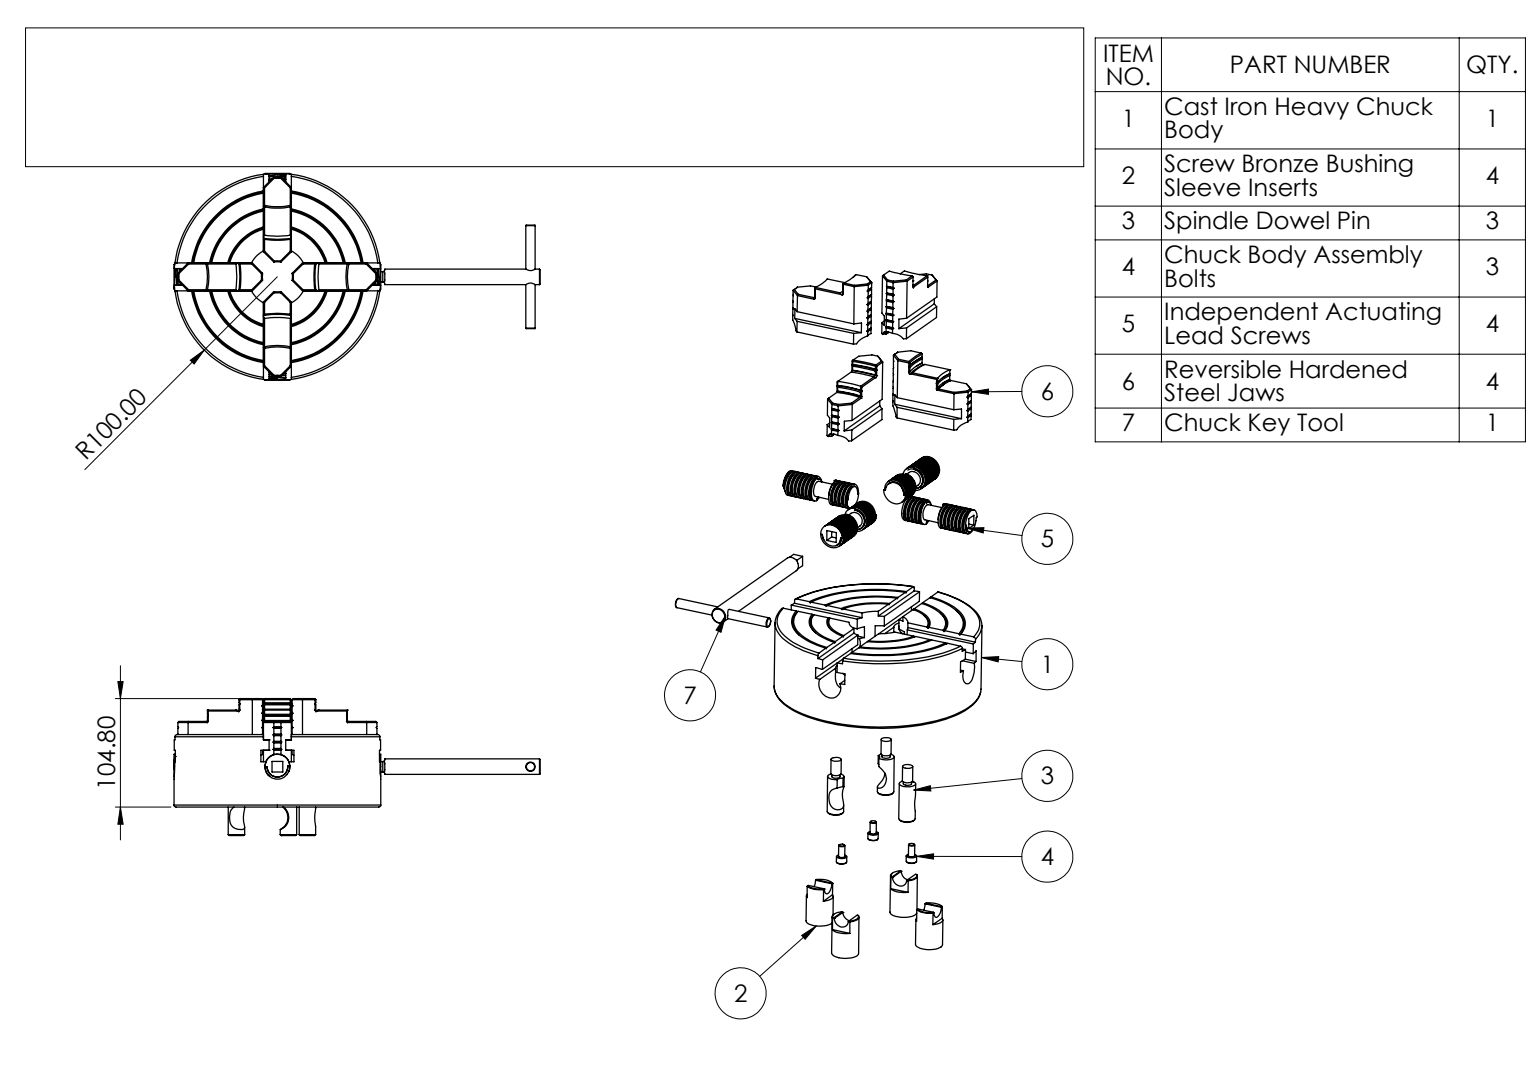
ISO-10303-21;
HEADER;
FILE_DESCRIPTION (('STEP AP214'),
    '1' );
FILE_NAME ('MAS-416',
    '2026-10-09T08:48:44',
    ( '' ),
    ( '' ),
    'SwSTEP 2.0',
    'SolidWorks 2026',
    '' );
FILE_SCHEMA (( 'AUTOMOTIVE_DESIGN' ));
ENDSEC;

DATA;
#1 =( BOUNDED_CURVE ( )  B_SPLINE_CURVE ( 2, ( #10533, #60209, #55118, #80827, #73261, #48394, #10118, #21906, #55527, #48810, #23141, #53876, #74509 ),
 .UNSPECIFIED., .F., .F. ) 
 B_SPLINE_CURVE_WITH_KNOTS ( ( 3, 2, 2, 2, 2, 2, 3 ),
 ( 0.7124999999999999112, 0.7166666666666665630, 0.7208333333333332149, 0.7249999999999998668, 0.7291666666666665186, 0.7333333333333331705, 0.7374999999999999334 ),
 .UNSPECIFIED. ) 
 CURVE ( )  GEOMETRIC_REPRESENTATION_ITEM ( )  RATIONAL_B_SPLINE_CURVE ( ( 1.000000000000000888, 0.9659258262890674240, 1.000000000000000000, 0.9659258262890683122, 1.000000000000000000, 0.9659258262890683122, 1.000000000000000000, 0.9659258262890683122, 1.000000000000000000, 0.9659258262890683122, 1.000000000000000000, 0.9659258262890692004, 0.9999999999999991118 ) ) 
 REPRESENTATION_ITEM ( '' )  );
#2 = CARTESIAN_POINT ( 'NONE',  ( 0.3392501089628018329, 0.1958661417322835607, -1.790682414698162805 ) ) ;
#3 = CARTESIAN_POINT ( 'NONE',  ( -1.404199475065615932, -0.3690944881889765550, -0.3153832671262227771 ) ) ;
#4 = CARTESIAN_POINT ( 'NONE',  ( 1.318897637795276356, 0.1660481256975883668, -0.3530559997133364547 ) ) ;
#5 = CARTESIAN_POINT ( 'NONE',  ( 1.194225721784777594, 0.05413385826771666132, 0.4176697321401328100 ) ) ;
#6 = CARTESIAN_POINT ( 'NONE',  ( 0.3018372703412079971, -0.004921259842519870586, -0.3153832671262229437 ) ) ;
#7 = CARTESIAN_POINT ( 'NONE',  ( 1.003937007874016185, 0.1660481256975883668, -0.3530559997133364547 ) ) ;
#8 = CARTESIAN_POINT ( 'NONE',  ( 0.4091458600556403535, 0.2362204724409449896, -1.625328083989501460 ) ) ;
#9 = CARTESIAN_POINT ( 'NONE',  ( 0.1377952755905518800, 0.07958543189024071263, -0.2665933059059888421 ) ) ;
#10 = CARTESIAN_POINT ( 'NONE',  ( 0.3149606299212603933, -0.1870078740157479769, 0.4822834645669291653 ) ) ;
#11 = CARTESIAN_POINT ( 'NONE',  ( 0.3949938075777409408, -0.1058382717557499186, -1.133202099737532720 ) ) ;
#12 = CARTESIAN_POINT ( 'NONE',  ( -1.043307086614172707, 0.1660481256975883668, -0.3530559997133364547 ) ) ;
#13 = CARTESIAN_POINT ( 'NONE',  ( 0.4330708661417329575, -0.5511811023622047445, 6.969142054262312111E-17 ) ) ;
#14 = PLANE ( 'NONE',  #11131 ) ;
#15 = CARTESIAN_POINT ( 'NONE',  ( -0.1902887139107604098, -0.6692913385826771977, 0.1292274648535927661 ) ) ;
#16 = CARTESIAN_POINT ( 'NONE',  ( -0.1574803149606292529, -0.1870078740157480601, -0.3641732283464567677 ) ) ;
#17 = CARTESIAN_POINT ( 'NONE',  ( 3.210901138312283187, 2.729659904327170317, 0.5314960629921260393 ) ) ;
#18 = CARTESIAN_POINT ( 'NONE',  ( -0.2493438320209966919, 0.05413385826771626580, -0.4176697321401330321 ) ) ;
#19 = CARTESIAN_POINT ( 'NONE',  ( 0.4002624671916016896, -0.2845877964562161244, -0.3641732283464567121 ) ) ;
#20 = CARTESIAN_POINT ( 'NONE',  ( 0.1070741851644053388, 0.3996062992125986035, -1.959973753280839892 ) ) ;
#21 = CARTESIAN_POINT ( 'NONE',  ( -0.03280839895013062252, 0.2952755905511810774, -0.1292274648535930714 ) ) ;
#22 = EDGE_CURVE ( 'NONE', #75161, #32355, #82357, .T. ) ;
#23 = CARTESIAN_POINT ( 'NONE',  ( -0.1958661417322834497, -0.3392501089628018884, -1.562972810202412521 ) ) ;
#24 = CARTESIAN_POINT ( 'NONE',  ( 1.135170603674541256, -0.5511811023622048555, -0.09757992244046775898 ) ) ;
#25 = CARTESIAN_POINT ( 'NONE',  ( 2.372150492836604986E-17, 0.000000000000000000, 0.1937007874015747588 ) ) ;
#26 = CARTESIAN_POINT ( 'NONE',  ( -0.8530183727034112984, -0.3690944881889765550, -0.3153832671262227771 ) ) ;
#27 = CARTESIAN_POINT ( 'NONE',  ( -0.8792650918635160906, -0.004921259842519870586, -0.3153832671262229437 ) ) ;
#28 = CARTESIAN_POINT ( 'NONE',  ( -0.8530183727034112984, 0.05413385826771666132, 0.4176697321401328100 ) ) ;
#29 = CARTESIAN_POINT ( 'NONE',  ( -0.3018372703412066094, 0.05413385826771666132, 0.4176697321401328100 ) ) ;
#30 = CARTESIAN_POINT ( 'NONE',  ( 0.5905511811023629321, 0.1771653543307087630, 0.000000000000000000 ) ) ;
#31 = CARTESIAN_POINT ( 'NONE',  ( -0.2597599741900292747, 0.1405915162213216552, 5.593567858643829993 ) ) ;
#32 = CARTESIAN_POINT ( 'NONE',  ( 1.351706036745407458, -0.3690944881889765550, -0.3153832671262227771 ) ) ;
#33 = CARTESIAN_POINT ( 'NONE',  ( 0.6758530183727039509, -0.6692913385826771977, 0.1292274648535927661 ) ) ;
#34 = CARTESIAN_POINT ( 'NONE',  ( 0.3996062992125986035, -0.1070741851644052972, -0.03083989501312336262 ) ) ;
#35 = CARTESIAN_POINT ( 'NONE',  ( -0.09186351706036689768, 0.05413385826771626580, -0.4176697321401330321 ) ) ;
#36 = CARTESIAN_POINT ( 'NONE',  ( 0.1958661417322836440, -0.3392501089628017219, -0.9639107611548557442 ) ) ;
#37 = CARTESIAN_POINT ( 'NONE',  ( 1.476377952755906220, 0.07958543189024071263, -0.2665933059059888421 ) ) ;
#38 = CARTESIAN_POINT ( 'NONE',  ( 0.7874015748031503170, -0.1870078740157480879, -0.4822834645669291653 ) ) ;
#39 = CARTESIAN_POINT ( 'NONE',  ( 8.195543980992789655E-16, -0.1870078740157480879, -0.4822834645669291653 ) ) ;
#40 = DIRECTION ( 'NONE',  ( 0.000000000000000000, 0.000000000000000000, 1.000000000000000000 ) ) ;
#41 = CARTESIAN_POINT ( 'NONE',  ( 0.1706036745406830368, -0.3690944881889765550, -0.3153832671262227771 ) ) ;
#42 = CARTESIAN_POINT ( 'NONE',  ( 1.141732283464567788, -0.6692913385826771977, 8.415575281601705876E-17 ) ) ;
#43 = CARTESIAN_POINT ( 'NONE',  ( -0.2952755905511804668, 0.07958543189024085140, 0.2665933059059887866 ) ) ;
#44 = CARTESIAN_POINT ( 'NONE',  ( -0.7152230971128602510, -0.3162353388693405765, 0.4822834645669290543 ) ) ;
#45 = CARTESIAN_POINT ( 'NONE',  ( 0.4091458600556404646, -0.2362204724409448231, -2.624671916010498762 ) ) ;
#46 = CARTESIAN_POINT ( 'NONE',  ( 0.3346456692913390985, 0.1660481256975885056, 0.3530559997133364547 ) ) ;
#47 = CARTESIAN_POINT ( 'NONE',  ( -0.6758530183727028406, 0.2952755905511811885, 0.1292274648535926551 ) ) ;
#48 = CARTESIAN_POINT ( 'NONE',  ( -0.7086614173228339419, -0.1870078740157480601, -0.3641732283464567677 ) ) ;
#49 = CARTESIAN_POINT ( 'NONE',  ( 0.1837270341207354329, 0.2306618581243848609, 0.2411417322834645549 ) ) ;
#50 = CARTESIAN_POINT ( 'NONE',  ( -1.135170603674539924, -0.6692913385826771977, 0.1292274648535927661 ) ) ;
#51 = CARTESIAN_POINT ( 'NONE',  ( -0.3412073490813641308, 0.2306618581243847221, -0.2411417322834647770 ) ) ;
#52 = CARTESIAN_POINT ( 'NONE',  ( 0.4724409448818898682, 2.892866454678787531E-17, -2.322834645669291209 ) ) ;
#54 = CARTESIAN_POINT ( 'NONE',  ( 1.161417322834646271, 0.1660481256975883668, -0.3530559997133364547 ) ) ;
#53 = CYLINDRICAL_SURFACE ( 'NONE', #64776, 0.3937007874015748254 ) ;
#55 = CARTESIAN_POINT ( 'NONE',  ( 1.135170603674541256, -0.6692913385826773087, -0.1292274648535924053 ) ) ;
#56 = CARTESIAN_POINT ( 'NONE',  ( 0.2867679344610366554, -0.2867679344610365444, -2.610236220472440749 ) ) ;
#57 = CARTESIAN_POINT ( 'NONE',  ( -1.489501312335957062, -0.05778040916215522460, 0.4822834645669289988 ) ) ;
#58 = CARTESIAN_POINT ( 'NONE',  ( -0.7217847769028863381, 0.05413385826771626580, -0.4176697321401330321 ) ) ;
#59 = CARTESIAN_POINT ( 'NONE',  ( 5.785732909357575061E-17, -0.4724409448818898682, -0.3937007874015748254 ) ) ;
#60 = CARTESIAN_POINT ( 'NONE',  ( -0.1070741851644051862, -0.3996062992125987146, -0.07217847769028871985 ) ) ;
#61 = ORIENTED_EDGE ( 'NONE', *, *, #30614, .T. ) ;
#62 = CARTESIAN_POINT ( 'NONE',  ( -0.08530183727034056085, -0.2845877964562159024, 0.3641732283464567677 ) ) ;
#63 = CARTESIAN_POINT ( 'NONE',  ( -0.1049643490035302024, -0.3917322834645671215, -1.796587926509185973 ) ) ;
#64 = EDGE_LOOP ( 'NONE', ( #43919, #18024, #48228, #40467 ) ) ;
#65 = CARTESIAN_POINT ( 'NONE',  ( 0.1837270341207354329, 0.2306618581243848609, 0.2411417322834645549 ) ) ;
#66 = CARTESIAN_POINT ( 'NONE',  ( -0.4724409448818898682, -8.678599364036362592E-17, -2.716535433070865757 ) ) ;
#67 = CYLINDRICAL_SURFACE ( 'NONE', #60105, 0.3937007874015748254 ) ;
#68 = CARTESIAN_POINT ( 'NONE',  ( -0.4265091863517051496, -0.5511811023622046335, 0.09757992244046803654 ) ) ;
#69 = CARTESIAN_POINT ( 'NONE',  ( 0.3346456692913390985, 0.1660481256975885056, 0.3530559997133364547 ) ) ;
#70 = CARTESIAN_POINT ( 'NONE',  ( 1.220472440944882608, 0.2952755905511811885, 0.000000000000000000 ) ) ;
#71 = CARTESIAN_POINT ( 'NONE',  ( 0.7283464566929140904, -0.4536011799217368745, -0.2665933059059886201 ) ) ;
#72 = AXIS2_PLACEMENT_3D ( 'NONE', #38595, #24309, #82401 ) ;
#73 = CARTESIAN_POINT ( 'NONE',  ( -0.04593175853018302557, 0.2952755905511811885, 0.1292274648535926551 ) ) ;
#74 = CARTESIAN_POINT ( 'NONE',  ( 4.797336870675655290E-17, -0.3917322834645669549, -0.9461749099399457963 ) ) ;
#75 = CARTESIAN_POINT ( 'NONE',  ( -0.7414698162729651543, -0.6692913385826771977, 0.1292274648535927661 ) ) ;
#76 = CARTESIAN_POINT ( 'NONE',  ( -1.351706036745406347, -0.004921259842519870586, -0.3153832671262229437 ) ) ;
#77 = CARTESIAN_POINT ( 'NONE',  ( -0.5839895013123351797, 0.2952755905511810774, -0.1292274648535930714 ) ) ;
#78 = FACE_OUTER_BOUND ( 'NONE', #30932, .T. ) ;
#79 = CARTESIAN_POINT ( 'NONE',  ( 1.515748031496063408, 0.07958543189024085140, 0.2665933059059887866 ) ) ;
#80 = VERTEX_POINT ( 'NONE', #70589 ) ;
#81 = CARTESIAN_POINT ( 'NONE',  ( 0.1049643490035304799, -0.3917322834645670104, -2.444245037566615597 ) ) ;
#82 = CARTESIAN_POINT ( 'NONE',  ( 0.2362204724409456558, -0.1870078740157479769, 0.4822834645669291653 ) ) ;
#83 = ORIENTED_EDGE ( 'NONE', *, *, #43269, .T. ) ;
#84 = CARTESIAN_POINT ( 'NONE',  ( -0.6561679790026240244, -0.6046776061558807314, 0.2411417322834647770 ) ) ;
#85 = CARTESIAN_POINT ( 'NONE',  ( 1.332020997375328974, -0.05778040916215560624, -0.4822834645669293319 ) ) ;
#86 = CARTESIAN_POINT ( 'NONE',  ( 1.213910761154856299, -0.6692913385826773087, -0.1292274648535924053 ) ) ;
#87 = CARTESIAN_POINT ( 'NONE',  ( 0.4724409448818904789, -0.1870078740157479769, 0.4822834645669291653 ) ) ;
#88 = CARTESIAN_POINT ( 'NONE',  ( 0.1574803149606306130, -0.1870078740157480879, -0.4822834645669291653 ) ) ;
#89 = CARTESIAN_POINT ( 'NONE',  ( -0.1049643490035302024, -0.3917322834645671215, -1.416666666666666519 ) ) ;
#90 = CARTESIAN_POINT ( 'NONE',  ( -0.9120734908136475250, 0.2952755905511811885, 0.1292274648535926551 ) ) ;
#91 = CARTESIAN_POINT ( 'NONE',  ( -0.1968503937007867743, 0.2952755905511811885, 0.000000000000000000 ) ) ;
#92 = CARTESIAN_POINT ( 'NONE',  ( -0.006561679790025524116, -0.08942795157528024563, -0.3641732283464568787 ) ) ;
#93 = CARTESIAN_POINT ( 'NONE',  ( -0.2945219335573386332, -0.02405856270293451477, 5.877884953661866696 ) ) ;
#94 = CARTESIAN_POINT ( 'NONE',  ( 0.07217847769028949700, -0.05778040916215560624, -0.4822834645669293319 ) ) ;
#95 = CARTESIAN_POINT ( 'NONE',  ( 2.362204724409448620, 1.724409448818897461, 8.247593713802677664E-15 ) ) ;
#96 = CARTESIAN_POINT ( 'NONE',  ( 1.253280839895013710, -0.3162353388693405765, 0.4822834645669290543 ) ) ;
#97 = CARTESIAN_POINT ( 'NONE',  ( 3.935554666754304876, 1.075197191891656523, -0.1080298857917176142 ) ) ;
#98 = EDGE_LOOP ( 'NONE', ( #67193, #53701, #56792, #76408 ) ) ;
#99 = ORIENTED_EDGE ( 'NONE', *, *, #69485, .F. ) ;
#100 = CARTESIAN_POINT ( 'NONE',  ( 0.3215223097112867578, -0.3162353388693409650, -0.4822834645669289433 ) ) ;
#101 = CARTESIAN_POINT ( 'NONE',  ( -0.3543307086614165824, -0.5511811023622047445, 6.969142054262312111E-17 ) ) ;
#103 = CARTESIAN_POINT ( 'NONE',  ( -0.06764250034433647030, -3.915482057279200494E-15, 0.3954985857520088577 ) ) ;
#102 = CARTESIAN_POINT ( 'NONE',  ( 1.377952755905512472, 0.1771653543307087630, 0.000000000000000000 ) ) ;
#104 = CARTESIAN_POINT ( 'NONE',  ( -0.3392501089628019995, 0.1958661417322832277, -1.213254593175852936 ) ) ;
#105 = CARTESIAN_POINT ( 'NONE',  ( -0.4091458600556405756, 0.2362204724409446288, -0.1030183727034120617 ) ) ;
#106 = CARTESIAN_POINT ( 'NONE',  ( 1.410761154855643795, -0.08942795157528024563, -0.3641732283464568787 ) ) ;
#107 = CARTESIAN_POINT ( 'NONE',  ( -1.423884514435694859, -0.05778040916215560624, -0.4822834645669293319 ) ) ;
#108 = CARTESIAN_POINT ( 'NONE',  ( 0.2891555358219910499, 0.2891555358219910499, 0.1003937007874015630 ) ) ;
#109 = CARTESIAN_POINT ( 'NONE',  ( -0.1377952755905504645, 0.1660481256975885056, 0.3530559997133364547 ) ) ;
#110 = CARTESIAN_POINT ( 'NONE',  ( -1.056430446194224881, -0.6692913385826771977, 0.1292274648535927661 ) ) ;
#111 = CARTESIAN_POINT ( 'NONE',  ( -0.9645669291338575535, -0.5400638737290844871, 0.3530559997133364547 ) ) ;
#112 = CARTESIAN_POINT ( 'NONE',  ( 0.1902887139107617975, 0.2952755905511811885, 0.1292274648535926551 ) ) ;
#113 = CARTESIAN_POINT ( 'NONE',  ( -0.3949938075777409963, -7.255918531996591613E-17, 0.04133858267716533641 ) ) ;
#114 = CARTESIAN_POINT ( 'NONE',  ( -1.653543307086613234, -0.1870078740157479769, 0.3641732283464567677 ) ) ;
#115 = CARTESIAN_POINT ( 'NONE',  ( 1.108923884514436242, -0.05778040916215522460, 0.4822834645669289988 ) ) ;
#116 = CARTESIAN_POINT ( 'NONE',  ( 0.7545931758530189937, 0.1771653543307087075, -0.09757992244046823083 ) ) ;
#117 = CARTESIAN_POINT ( 'NONE',  ( 0.3074112942705509166, 1.261823755618582510, 0.05913325304464405602 ) ) ;
#118 = CARTESIAN_POINT ( 'NONE',  ( 0.9055118110236227702, 0.1771653543307087630, 0.000000000000000000 ) ) ;
#119 = CARTESIAN_POINT ( 'NONE',  ( -1.200787401574802349, -0.5400638737290844871, 0.3530559997133364547 ) ) ;
#120 = CARTESIAN_POINT ( 'NONE',  ( -9.787531504996566615E-17, 0.3996062992125985480, -0.7066929133858268486 ) ) ;
#121 = CARTESIAN_POINT ( 'NONE',  ( 1.358267716535433323, 0.1660481256975885056, 0.3530559997133364547 ) ) ;
#122 = CARTESIAN_POINT ( 'NONE',  ( -0.3392501089628017219, -0.1958661417322836718, -0.6745406824146981117 ) ) ;
#124 = DIRECTION ( 'NONE',  ( 1.000000000000000000, 0.000000000000000000, -0.000000000000000000 ) ) ;
#123 = CARTESIAN_POINT ( 'NONE',  ( 0.6036745406824154392, 0.2306618581243847221, -0.2411417322834647770 ) ) ;
#125 = CARTESIAN_POINT ( 'NONE',  ( -1.653543307086613234, -0.1870078740157480601, -0.3641732283464567677 ) ) ;
#126 = CARTESIAN_POINT ( 'NONE',  ( 0.01968503937007957949, -0.5400638737290845981, -0.3530559997133363437 ) ) ;
#127 = CARTESIAN_POINT ( 'NONE',  ( 0.6102362204724416372, -0.4536011799217367080, 0.2665933059059888421 ) ) ;
#128 = CARTESIAN_POINT ( 'NONE',  ( 0.9776902887139113929, -0.6692913385826773087, -0.1292274648535924053 ) ) ;
#129 = CARTESIAN_POINT ( 'NONE',  ( 1.640419947506562393, -0.3690944881889763329, 0.3153832671262228327 ) ) ;
#130 = CARTESIAN_POINT ( 'NONE',  ( -0.6824146981627291497, -0.5023911411419708095, -0.1820866141732282451 ) ) ;
#131 = CARTESIAN_POINT ( 'NONE',  ( -0.6430446194225716283, -0.4281496062992124485, 0.4176697321401328655 ) ) ;
#132 = CARTESIAN_POINT ( 'NONE',  ( 1.574803149606299746, -0.1870078740157480879, -0.4822834645669291653 ) ) ;
#133 = CARTESIAN_POINT ( 'NONE',  ( -1.246719160104986512, 0.05413385826771666132, 0.4176697321401328100 ) ) ;
#134 = CONICAL_SURFACE ( 'NONE', #57903, 2.401574803149606918, 0.7125723459225955514 ) ;
#135 = CARTESIAN_POINT ( 'NONE',  ( 0.8923884514435703741, 0.2306618581243848609, 0.2411417322834645549 ) ) ;
#136 = CARTESIAN_POINT ( 'NONE',  ( -1.345144356955379816, -0.2845877964562159024, 0.3641732283464567677 ) ) ;
#137 = CARTESIAN_POINT ( 'NONE',  ( 1.067341128551216878, 1.212753000281105331, 0.3462674622822208836 ) ) ;
#138 = CARTESIAN_POINT ( 'NONE',  ( 0.8070866141732288002, 0.1660481256975885056, 0.3530559997133364547 ) ) ;
#139 = CARTESIAN_POINT ( 'NONE',  ( -0.2362204724409447953, -0.4091458600556404646, -2.347112860892388575 ) ) ;
#140 = CARTESIAN_POINT ( 'NONE',  ( -1.561679790026246017, 0.05413385826771666132, 0.4176697321401328100 ) ) ;
#141 = CARTESIAN_POINT ( 'NONE',  ( -1.555118110236219930, -0.4536011799217368745, -0.2665933059059886201 ) ) ;
#142 = CARTESIAN_POINT ( 'NONE',  ( -0.8792650918635160906, -0.004921259842519870586, -0.3153832671262229437 ) ) ;
#143 = B_SPLINE_CURVE_WITH_KNOTS ( 'NONE', 3,
 ( #64397, #13065, #45854, #433 ),
 .UNSPECIFIED., .F., .F.,
 ( 4, 4 ),
 ( 3.878959614448864246E-18, 0.001357026659661165861 ),
 .UNSPECIFIED. ) ;
#144 = CARTESIAN_POINT ( 'NONE',  ( 1.496062992125985147, -0.1870078740157479769, 0.3641732283464567677 ) ) ;
#145 = CARTESIAN_POINT ( 'NONE',  ( -0.3280839895013117347, 0.05413385826771626580, -0.4176697321401330321 ) ) ;
#146 = CARTESIAN_POINT ( 'NONE',  ( -0.2230971128608915943, -0.004921259842519576551, 0.3153832671262227771 ) ) ;
#147 = CARTESIAN_POINT ( 'NONE',  ( -1.660104986876639543, -0.08942795157528024563, -0.3641732283464568787 ) ) ;
#148 = CARTESIAN_POINT ( 'NONE',  ( 0.9711286089238851948, 0.1283753931104748280, 0.1820866141732283561 ) ) ;
#149 = CARTESIAN_POINT ( 'NONE',  ( 0.6299212598425204535, -0.1870078740157480879, -0.4822834645669291653 ) ) ;
#150 = CARTESIAN_POINT ( 'NONE',  ( 1.489501312335958172, -0.05778040916215560624, -0.4822834645669293319 ) ) ;
#151 = CARTESIAN_POINT ( 'NONE',  ( 0.4986876640419954376, -0.6046776061558809534, -0.2411417322834644161 ) ) ;
#152 = CIRCLE ( 'NONE', #29714, 0.3149606299212598381 ) ;
#153 = EDGE_CURVE ( 'NONE', #58154, #38787, #62911, .T. ) ;
#154 = CARTESIAN_POINT ( 'NONE',  ( 0.6889763779527563470, 0.07958543189024071263, -0.2665933059059888421 ) ) ;
#155 = CARTESIAN_POINT ( 'NONE',  ( -1.443569553805773564, 0.2306618581243847221, -0.2411417322834647770 ) ) ;
#156 = ADVANCED_FACE ( 'NONE', ( #41522 ), #80675, .F. ) ;
#157 = CARTESIAN_POINT ( 'NONE',  ( -1.351706036745406347, -0.4281496062992124485, 0.4176697321401328655 ) ) ;
#158 = CARTESIAN_POINT ( 'NONE',  ( -0.4724409448818890911, -0.1870078740157479769, 0.4822834645669291653 ) ) ;
#159 = CARTESIAN_POINT ( 'NONE',  ( 0.1070741851644053666, 0.3996062992125986035, -0.4658792650918635037 ) ) ;
#160 = CARTESIAN_POINT ( 'NONE',  ( -0.1070741851644051862, -0.3996062992125986590, -2.668635170603674833 ) ) ;
#161 = CARTESIAN_POINT ( 'NONE',  ( -0.04593175853018302557, -0.6692913385826773087, -0.1292274648535924053 ) ) ;
#162 = CARTESIAN_POINT ( 'NONE',  ( 1.187664041994751285, -0.2845877964562161244, -0.3641732283464567121 ) ) ;
#163 = CARTESIAN_POINT ( 'NONE',  ( -0.3608923884514428360, 0.2952755905511811885, 0.1292274648535926551 ) ) ;
#164 = CARTESIAN_POINT ( 'NONE',  ( 0.2952755905511816326, -0.5400638737290844871, 0.3530559997133364547 ) ) ;
#165 = CARTESIAN_POINT ( 'NONE',  ( 0.2925321140481932369, 0.2925321140481932369, -2.342519685039369914 ) ) ;
#166 = CARTESIAN_POINT ( 'NONE',  ( 0.3420746716998660508, -0.1974969037888703871, -1.994750656167979086 ) ) ;
#167 = CARTESIAN_POINT ( 'NONE',  ( -0.3917322834645671215, 0.1049643490035301469, -0.4973753280839895430 ) ) ;
#168 = CARTESIAN_POINT ( 'NONE',  ( -1.157146581871515012E-16, 0.4724409448818898682, -2.519685039370078705 ) ) ;
#169 = CARTESIAN_POINT ( 'NONE',  ( 0.1049643490035304799, -0.3917322834645669549, -0.8648293963254591876 ) ) ;
#170 = CARTESIAN_POINT ( 'NONE',  ( -0.8464566929133852113, -0.4536011799217368745, -0.2665933059059886201 ) ) ;
#171 = CARTESIAN_POINT ( 'NONE',  ( -1.272965879265091305, -0.4281496062992124485, 0.4176697321401328655 ) ) ;
#172 = CARTESIAN_POINT ( 'NONE',  ( -0.3420746716998662729, 0.1974969037888702206, -2.780183727034121866 ) ) ;
#173 = CARTESIAN_POINT ( 'NONE',  ( 0.3280839895013130669, -0.4281496062992127816, -0.4176697321401328100 ) ) ;
#174 = EDGE_CURVE ( 'NONE', #2979, #51820, #28890, .T. ) ;
#175 = CARTESIAN_POINT ( 'NONE',  ( 1.233595800524935227, -0.6046776061558807314, 0.2411417322834647770 ) ) ;
#176 = CARTESIAN_POINT ( 'NONE',  ( 0.8202099737532813073, 0.2952755905511811885, 0.1292274648535926551 ) ) ;
#177 = CARTESIAN_POINT ( 'NONE',  ( 0.2362204724409451007, -0.4091458600556402980, -2.769028871391076230 ) ) ;
#178 = CARTESIAN_POINT ( 'NONE',  ( 0.2925321140481932369, 0.2925321140481932369, -2.185039370078739829 ) ) ;
#179 = CARTESIAN_POINT ( 'NONE',  ( -0.3392501089628017219, -0.1958661417322836995, -0.8366334890101857491 ) ) ;
#180 = CARTESIAN_POINT ( 'NONE',  ( 1.541994750656168645, 0.2952755905511810774, -0.1292274648535930714 ) ) ;
#181 = CARTESIAN_POINT ( 'NONE',  ( 0.4330708661417329575, -0.6692913385826771977, 8.415575281601705876E-17 ) ) ;
#182 = CARTESIAN_POINT ( 'NONE',  ( 0.07217847769028949700, -0.05778040916215560624, -0.4822834645669293319 ) ) ;
#183 = CARTESIAN_POINT ( 'NONE',  ( 0.7480314960629927956, -0.5511811023622047445, 6.969142054262312111E-17 ) ) ;
#184 = CARTESIAN_POINT ( 'NONE',  ( 1.371391076115485941, 0.2952755905511811885, 0.1292274648535926551 ) ) ;
#185 = CARTESIAN_POINT ( 'NONE',  ( -0.2867679344610364334, -0.2867679344610367109, -0.1437007874015748810 ) ) ;
#186 = CARTESIAN_POINT ( 'NONE',  ( 0.5643044619422579178, -0.4281496062992127816, -0.4176697321401328100 ) ) ;
#187 = CARTESIAN_POINT ( 'NONE',  ( 0.9514435695538062676, -0.3162353388693409650, -0.4822834645669289433 ) ) ;
#188 = CARTESIAN_POINT ( 'NONE',  ( 0.2690288713910767848, 0.2952755905511811885, 0.1292274648535926551 ) ) ;
#189 = CARTESIAN_POINT ( 'NONE',  ( 1.233595800524935227, 0.1283753931104746893, -0.1820866141732285504 ) ) ;
#190 = CARTESIAN_POINT ( 'NONE',  ( -0.9448818897637790704, -0.1870078740157479769, 0.4822834645669291653 ) ) ;
#191 = CARTESIAN_POINT ( 'NONE',  ( -1.102362204724408601, -0.1870078740157479769, 0.4822834645669291653 ) ) ;
#192 = CIRCLE ( 'NONE', #6913, 0.3149606299212597826 ) ;
#193 = CARTESIAN_POINT ( 'NONE',  ( 1.089238845144357537, -0.4281496062992124485, 0.4176697321401328655 ) ) ;
#194 = CARTESIAN_POINT ( 'NONE',  ( -0.3917322834645670104, -7.196005306013484475E-17, -0.7539370078740157410 ) ) ;
#195 = CARTESIAN_POINT ( 'NONE',  ( 0.3917322834645669549, 0.1049643490035304660, -1.691601049868766360 ) ) ;
#196 = CARTESIAN_POINT ( 'NONE',  ( -0.3917322834645671215, 0.1049643490035301469, -2.859580052493438274 ) ) ;
#197 = ORIENTED_EDGE ( 'NONE', *, *, #73267, .T. ) ;
#198 = CARTESIAN_POINT ( 'NONE',  ( -0.2925321140481930704, -0.2925321140481933480, -0.2165354330708662012 ) ) ;
#199 = VERTEX_POINT ( 'NONE', #53305 ) ;
#200 = CARTESIAN_POINT ( 'NONE',  ( 1.509186351706037543, 0.05413385826771666132, 0.4176697321401328100 ) ) ;
#201 = CARTESIAN_POINT ( 'NONE',  ( 0.9317585301837276734, -0.3690944881889763329, 0.3153832671262228327 ) ) ;
#202 = CARTESIAN_POINT ( 'NONE',  ( -0.3996062992125986035, -0.1070741851644056997, -1.620734908136482799 ) ) ;
#203 = CARTESIAN_POINT ( 'NONE',  ( 1.213910761154856299, 0.1771653543307087630, 0.09757992244046791164 ) ) ;
#204 = CARTESIAN_POINT ( 'NONE',  ( -0.4724409448818899238, 0.1265901696524986964, -2.471784776902886893 ) ) ;
#205 = DIRECTION ( 'NONE',  ( 1.000000000000000000, 0.000000000000000000, -1.692413147294446216E-16 ) ) ;
#206 = CARTESIAN_POINT ( 'NONE',  ( -0.6175017169405814244, 0.000000000000000000, 0.3464511005275205946 ) ) ;
#207 = CARTESIAN_POINT ( 'NONE',  ( 0.3392501089628018884, -0.1958661417322834220, -0.6620734908136483021 ) ) ;
#208 = CARTESIAN_POINT ( 'NONE',  ( -0.9776902887139098386, 0.1771653543307087075, -0.09757992244046823083 ) ) ;
#209 = CARTESIAN_POINT ( 'NONE',  ( -1.640419947506561060, -0.3690944881889765550, -0.3153832671262227771 ) ) ;
#210 = CARTESIAN_POINT ( 'NONE',  ( -1.423884514435694859, -0.05778040916215560624, -0.4822834645669293319 ) ) ;
#211 = CARTESIAN_POINT ( 'NONE',  ( 5.463695987328526437E-16, -0.1870078740157479769, 0.4822834645669291653 ) ) ;
#212 = CARTESIAN_POINT ( 'NONE',  ( 1.312335958005249825, 0.2306618581243847221, -0.2411417322834647770 ) ) ;
#213 = ORIENTED_EDGE ( 'NONE', *, *, #72282, .F. ) ;
#214 = CARTESIAN_POINT ( 'NONE',  ( -1.122047244094487306, 0.1012011053420775880, -0.2882089793578256898 ) ) ;
#215 =( CONVERSION_BASED_UNIT ( 'INCH', #44794 ) LENGTH_UNIT ( ) NAMED_UNIT ( #76065 ) );
#216 = CARTESIAN_POINT ( 'NONE',  ( -0.2362204724409447953, -0.4091458600556404646, -2.112860892388451539 ) ) ;
#217 = DIRECTION ( 'NONE',  ( 1.000000000000000000, -0.000000000000000000, -0.000000000000000000 ) ) ;
#218 = LINE ( 'NONE', #70923, #26406 ) ;
#219 = CARTESIAN_POINT ( 'NONE',  ( -0.8727034120734901146, -0.2845877964562159024, 0.3641732283464567677 ) ) ;
#220 = CARTESIAN_POINT ( 'NONE',  ( -1.161417322834644716, 0.1660481256975885056, 0.3530559997133364547 ) ) ;
#221 = CARTESIAN_POINT ( 'NONE',  ( 0.7283464566929143125, 0.1660481256975885056, 0.3530559997133364547 ) ) ;
#222 = ORIENTED_EDGE ( 'NONE', *, *, #16494, .T. ) ;
#223 = ADVANCED_FACE ( 'NONE', ( #9541 ), #47687, .T. ) ;
#225 = DIRECTION ( 'NONE',  ( -0.000000000000000000, -1.000000000000000000, -0.000000000000000000 ) ) ;
#224 = CARTESIAN_POINT ( 'NONE',  ( 0.3458507752293908943, -0.3458507752293908943, -2.537401574803149984 ) ) ;
#226 = CARTESIAN_POINT ( 'NONE',  ( 1.161417322834646493, -0.5400638737290844871, 0.3530559997133364547 ) ) ;
#227 = CARTESIAN_POINT ( 'NONE',  ( -1.240157480314959759, 0.1660481256975885056, 0.3530559997133364547 ) ) ;
#228 = CARTESIAN_POINT ( 'NONE',  ( -0.3917322834645669549, -7.196005306013483243E-17, -0.7493245162391581893 ) ) ;
#229 = CARTESIAN_POINT ( 'NONE',  ( -0.5380577427821514602, -0.3690944881889765550, -0.3153832671262227771 ) ) ;
#230 = CARTESIAN_POINT ( 'NONE',  ( -1.253280839895012377, -0.2845877964562161244, -0.3641732283464567121 ) ) ;
#231 = CARTESIAN_POINT ( 'NONE',  ( 0.1958661417322836440, -0.3392501089628017219, -0.9639107611548557442 ) ) ;
#232 = CARTESIAN_POINT ( 'NONE',  ( -0.4855643044619415427, -0.004921259842519870586, -0.3153832671262229437 ) ) ;
#233 = CARTESIAN_POINT ( 'NONE',  ( -0.07217847769028813698, -0.2845877964562161244, -0.3641732283464567121 ) ) ;
#234 = CARTESIAN_POINT ( 'NONE',  ( 0.3215223097112867578, -0.05778040916215522460, 0.4822834645669289988 ) ) ;
#235 = CARTESIAN_POINT ( 'NONE',  ( -1.076115485564303809, -0.5023911411419708095, -0.1820866141732282451 ) ) ;
#236 = CARTESIAN_POINT ( 'NONE',  ( -0.3392501089628017219, -0.1958661417322836718, -2.879265091863516979 ) ) ;
#237 = CARTESIAN_POINT ( 'NONE',  ( 1.167979002624672580, 0.05413385826771626580, -0.4176697321401330321 ) ) ;
#238 = EDGE_CURVE ( 'NONE', #62570, #82725, #55742, .T. ) ;
#239 = CARTESIAN_POINT ( 'NONE',  ( -1.345144356955379816, -0.3162353388693405765, 0.4822834645669290543 ) ) ;
#240 = CARTESIAN_POINT ( 'NONE',  ( -1.157146581871515012E-16, 0.4724409448818898682, -1.021653543307086576 ) ) ;
#241 = CARTESIAN_POINT ( 'NONE',  ( -0.2952755905511804668, 0.1660481256975885056, 0.3530559997133364547 ) ) ;
#242 = CARTESIAN_POINT ( 'NONE',  ( -0.8923884514435688198, -0.6046776061558807314, 0.2411417322834647770 ) ) ;
#243 = CARTESIAN_POINT ( 'NONE',  ( 0.9251968503937015864, 0.07958543189024071263, -0.2665933059059888421 ) ) ;
#244 = CARTESIAN_POINT ( 'NONE',  ( -0.4986876640419942164, -0.5023911411419708095, 0.1820866141732285504 ) ) ;
#245 = CARTESIAN_POINT ( 'NONE',  ( -0.5052493438320203589, -0.6692913385826771977, 0.1292274648535927661 ) ) ;
#246 = CARTESIAN_POINT ( 'NONE',  ( -1.364829396325458521, -0.6046776061558807314, 0.2411417322834647770 ) ) ;
#247 = CARTESIAN_POINT ( 'NONE',  ( 0.000000000000000000, 0.000000000000000000, -0.01968503937007903132 ) ) ;
#248 = CARTESIAN_POINT ( 'NONE',  ( 1.089238845144357759, -0.004921259842519870586, -0.3153832671262229437 ) ) ;
#249 = CARTESIAN_POINT ( 'NONE',  ( -0.4330708661417315697, -0.6692913385826771977, 8.415575281601705876E-17 ) ) ;
#250 = CARTESIAN_POINT ( 'NONE',  ( -1.561679790026246017, 0.05413385826771666132, 0.4176697321401328100 ) ) ;
#251 = AXIS2_PLACEMENT_3D ( 'NONE', #31198, #57691, #45055 ) ;
#252 = ORIENTED_EDGE ( 'NONE', *, *, #19019, .F. ) ;
#253 = CARTESIAN_POINT ( 'NONE',  ( -0.3996062992125984925, -0.1070741851644056858, -2.484908136482939955 ) ) ;
#254 = CARTESIAN_POINT ( 'NONE',  ( -0.9776902887139098386, 0.1771653543307087075, -0.09757992244046823083 ) ) ;
#255 = CARTESIAN_POINT ( 'NONE',  ( 0.7349081364829402885, -0.6046776061558809534, -0.2411417322834644161 ) ) ;
#256 = CARTESIAN_POINT ( 'NONE',  ( -1.135170603674539924, -0.5511811023622046335, 0.09757992244046803654 ) ) ;
#257 = CARTESIAN_POINT ( 'NONE',  ( 0.1070741851644053388, 0.3996062992125986035, -1.330052493438320438 ) ) ;
#258 = CARTESIAN_POINT ( 'NONE',  ( -1.017060367454067249, -0.3162353388693409650, -0.4822834645669289433 ) ) ;
#259 = CARTESIAN_POINT ( 'NONE',  ( 0.7020997375328090762, -0.3162353388693405765, 0.4822834645669290543 ) ) ;
#260 = CARTESIAN_POINT ( 'NONE',  ( 0.6955380577427828781, -0.4281496062992124485, 0.4176697321401328655 ) ) ;
#261 = CARTESIAN_POINT ( 'NONE',  ( 1.463254593175853824, 0.2952755905511810774, -0.1292274648535930714 ) ) ;
#262 = CARTESIAN_POINT ( 'NONE',  ( -1.377952755905511140, 0.1771653543307087630, 0.000000000000000000 ) ) ;
#263 = CARTESIAN_POINT ( 'NONE',  ( -0.2925321140481930149, -0.2925321140481933480, -0.7657480314960628531 ) ) ;
#264 = CARTESIAN_POINT ( 'NONE',  ( 0.1998031496062994405, -0.3460692066303958092, -0.8792650918635170898 ) ) ;
#265 = CARTESIAN_POINT ( 'NONE',  ( 0.3420746716998659953, 0.1974969037888705536, -0.2887139107611549349 ) ) ;
#266 = LINE ( 'NONE', #58323, #72192 ) ;
#267 = CARTESIAN_POINT ( 'NONE',  ( 1.043307086614173818, 0.07958543189024085140, 0.2665933059059887866 ) ) ;
#268 = CARTESIAN_POINT ( 'NONE',  ( 0.3871391076115492380, -0.08942795157528024563, -0.3641732283464568787 ) ) ;
#269 = CARTESIAN_POINT ( 'NONE',  ( 0.1377952755905518800, -0.5400638737290844871, 0.3530559997133364547 ) ) ;
#270 = CARTESIAN_POINT ( 'NONE',  ( 1.161417322834646271, 0.1660481256975883668, -0.3530559997133364547 ) ) ;
#271 = CARTESIAN_POINT ( 'NONE',  ( -0.1974969037888704149, -0.3420746716998661063, -1.244750656167979086 ) ) ;
#272 = CARTESIAN_POINT ( 'NONE',  ( 0.2887139107611556010, 0.1283753931104746893, -0.1820866141732285504 ) ) ;
#273 = CARTESIAN_POINT ( 'NONE',  ( -0.6036745406824141069, -0.6046776061558809534, -0.2411417322834644161 ) ) ;
#274 = CARTESIAN_POINT ( 'NONE',  ( -1.246719160104985846, -0.4281496062992127816, -0.4176697321401328100 ) ) ;
#275 = CARTESIAN_POINT ( 'NONE',  ( 0.6627296587926517768, -0.6692913385826773087, -0.1292274648535924053 ) ) ;
#276 = CARTESIAN_POINT ( 'NONE',  ( -0.3458507752293906723, -0.3458507752293910609, -1.633858267716534973 ) ) ;
#277 = CARTESIAN_POINT ( 'NONE',  ( 4.893765752498283924E-17, -0.3996062992125986035, -2.598425196850393970 ) ) ;
#278 = EDGE_LOOP ( 'NONE', ( #70982, #45636, #76392, #46329 ) ) ;
#279 = ORIENTED_EDGE ( 'NONE', *, *, #37675, .F. ) ;
#280 = CARTESIAN_POINT ( 'NONE',  ( -1.391076115485563758, 0.2306618581243848609, 0.2411417322834645549 ) ) ;
#281 = CARTESIAN_POINT ( 'NONE',  ( -0.7742782152230962556, -0.4281496062992127816, -0.4176697321401328100 ) ) ;
#283 = CARTESIAN_POINT ( 'NONE',  ( -0.5971128608923877978, -0.6692913385826773087, -0.1292274648535924053 ) ) ;
#282 = CARTESIAN_POINT ( 'NONE',  ( -0.7020997375328074108, -0.08942795157527998196, 0.3641732283464567121 ) ) ;
#284 = CARTESIAN_POINT ( 'NONE',  ( -9.594673741351310580E-17, 0.3917322834645669549, -1.969796957184039909 ) ) ;
#285 = CARTESIAN_POINT ( 'NONE',  ( -9.787531504996566615E-17, 0.3996062992125985480, -2.753937007874015741 ) ) ;
#286 = CARTESIAN_POINT ( 'NONE',  ( -1.607611548556429737, 0.1771653543307087075, -0.09757992244046823083 ) ) ;
#287 = CARTESIAN_POINT ( 'NONE',  ( -1.069553805774277722, 0.2952755905511811885, 0.1292274648535926551 ) ) ;
#288 = CARTESIAN_POINT ( 'NONE',  ( 0.2952755905511816326, -0.5400638737290844871, 0.3530559997133364547 ) ) ;
#289 = CARTESIAN_POINT ( 'NONE',  ( -0.7349081364829387342, -0.6046776061558807314, 0.2411417322834647770 ) ) ;
#290 = CARTESIAN_POINT ( 'NONE',  ( -0.1958661417322834220, -0.3392501089628018884, -1.317585301837270295 ) ) ;
#291 = CARTESIAN_POINT ( 'NONE',  ( -0.8595800524934373854, -0.08942795157527998196, 0.3641732283464567121 ) ) ;
#292 = ORIENTED_EDGE ( 'NONE', *, *, #19718, .F. ) ;
#293 = CARTESIAN_POINT ( 'NONE',  ( 0.1974969037888704704, 0.3420746716998660508, -2.034120734908136718 ) ) ;
#294 = ORIENTED_EDGE ( 'NONE', *, *, #5614, .T. ) ;
#295 = CARTESIAN_POINT ( 'NONE',  ( -1.535433070866141225, 0.1771653543307087630, 0.000000000000000000 ) ) ;
#296 = CARTESIAN_POINT ( 'NONE',  ( -1.240157480314959759, 0.1660481256975885056, 0.3530559997133364547 ) ) ;
#297 = CARTESIAN_POINT ( 'NONE',  ( -0.7414698162729651543, -0.6692913385826771977, 0.1292274648535927661 ) ) ;
#298 = CARTESIAN_POINT ( 'NONE',  ( -0.1998031496062994683, 0.3460692066303958092, -0.3280839895013123453 ) ) ;
#299 = CARTESIAN_POINT ( 'NONE',  ( -0.9645669291338575535, -0.5400638737290844871, 0.3530559997133364547 ) ) ;
#300 = CARTESIAN_POINT ( 'NONE',  ( -1.410761154855642463, -0.05778040916215522460, 0.4822834645669289988 ) ) ;
#301 = CARTESIAN_POINT ( 'NONE',  ( 0.000000000000000000, 2.185039370078740273, -0.2736220472440938911 ) ) ;
#302 = EDGE_CURVE ( 'NONE', #13567, #50475, #28771, .T. ) ;
#303 = LINE ( 'NONE', #76901, #13349 ) ;
#304 = CARTESIAN_POINT ( 'NONE',  ( 0.5971128608923891301, 0.1771653543307087075, -0.09757992244046823083 ) ) ;
#305 = DIRECTION ( 'NONE',  ( -3.096699300667737957E-16, 1.000000000000000000, -0.000000000000000000 ) ) ;
#306 = CARTESIAN_POINT ( 'NONE',  ( 0.1049643490035303689, 0.3917322834645670104, -0.5505249343832020470 ) ) ;
#307 = CARTESIAN_POINT ( 'NONE',  ( -0.2034120734908131112, -0.5511811023622048555, -0.09757992244046775898 ) ) ;
#308 = CARTESIAN_POINT ( 'NONE',  ( -0.6036745406824141069, -0.6046776061558809534, -0.2411417322834644161 ) ) ;
#309 = ADVANCED_FACE ( 'NONE', ( #49336 ), #12419, .F. ) ;
#310 = CARTESIAN_POINT ( 'NONE',  ( 1.555118110236221041, -0.5400638737290844871, 0.3530559997133364547 ) ) ;
#311 = CARTESIAN_POINT ( 'NONE',  ( -0.6233595800524928121, -0.3162353388693409650, -0.4822834645669289433 ) ) ;
#312 = VERTEX_POINT ( 'NONE', #80938 ) ;
#313 = ORIENTED_EDGE ( 'NONE', *, *, #50172, .F. ) ;
#314 = CARTESIAN_POINT ( 'NONE',  ( 0.2925321140481932369, -0.2925321140481931814, -2.064960629921259283 ) ) ;
#316 = TOROIDAL_SURFACE ( 'NONE', #58028, 1.178877988035069047, 0.01968503937007873988 ) ;
#315 = CARTESIAN_POINT ( 'NONE',  ( -1.095800524934382292, -0.3162353388693409650, -0.4822834645669289433 ) ) ;
#317 = CARTESIAN_POINT ( 'NONE',  ( 1.404199475065617264, -0.4281496062992124485, 0.4176697321401328655 ) ) ;
#318 = CARTESIAN_POINT ( 'NONE',  ( -1.043307086614172707, 0.07958543189024071263, -0.2665933059059888421 ) ) ;
#319 = CARTESIAN_POINT ( 'NONE',  ( -1.443569553805773564, -0.6046776061558807314, 0.2411417322834647770 ) ) ;
#320 = CARTESIAN_POINT ( 'NONE',  ( -0.3458507752293906723, -0.3458507752293910609, -0.8464566929133857665 ) ) ;
#321 = CARTESIAN_POINT ( 'NONE',  ( 2.165589143934496530, 1.494558157769224405, 0.4725443725032424380 ) ) ;
#322 = CARTESIAN_POINT ( 'NONE',  ( -0.1049643490035302024, -0.3917322834645671215, -0.2217847769028870319 ) ) ;
#323 = CARTESIAN_POINT ( 'NONE',  ( 0.3808816823641231752, -0.09156050430092187165, -1.929133858267716661 ) ) ;
#324 = CARTESIAN_POINT ( 'NONE',  ( 0.01312335958005323398, -0.4281496062992127816, -0.4176697321401328100 ) ) ;
#325 = CARTESIAN_POINT ( 'NONE',  ( -1.135170603674539924, 0.1771653543307087075, -0.09757992244046823083 ) ) ;
#326 = CARTESIAN_POINT ( 'NONE',  ( -0.6299212598425188991, -0.1870078740157479769, 0.4822834645669291653 ) ) ;
#327 = CARTESIAN_POINT ( 'NONE',  ( 0.2362204724409451007, -0.4091458600556402980, -2.845800524934383624 ) ) ;
#328 = CARTESIAN_POINT ( 'NONE',  ( -1.384514435695537005, 0.2952755905511811885, 0.1292274648535926551 ) ) ;
#329 = CARTESIAN_POINT ( 'NONE',  ( -1.095800524934382292, -0.05778040916215522460, 0.4822834645669289988 ) ) ;
#330 = CARTESIAN_POINT ( 'NONE',  ( 0.2362204724409456558, -0.1870078740157480879, -0.4822834645669291653 ) ) ;
#331 = CARTESIAN_POINT ( 'NONE',  ( -0.1058382717557497660, -0.3949938075777411073, -2.668635170603674833 ) ) ;
#332 = CARTESIAN_POINT ( 'NONE',  ( 0.7349081364829402885, -0.5023911411419708095, -0.1820866141732282451 ) ) ;
#333 = CARTESIAN_POINT ( 'NONE',  ( -0.7742782152230965886, -0.004921259842519576551, 0.3153832671262227771 ) ) ;
#334 = CARTESIAN_POINT ( 'NONE',  ( -0.09693039542137318887, 1.072949718929360641, -1.590986883761158932 ) ) ;
#335 = CARTESIAN_POINT ( 'NONE',  ( 0.8267716535433078384, -0.5511811023622047445, 6.969142054262312111E-17 ) ) ;
#336 = CARTESIAN_POINT ( 'NONE',  ( 1.496062992125984703, -0.1870078740157480601, -0.3641732283464567677 ) ) ;
#337 = CARTESIAN_POINT ( 'NONE',  ( 1.299212598425197429, 0.2952755905511811885, 0.000000000000000000 ) ) ;
#338 = CARTESIAN_POINT ( 'NONE',  ( -0.05905511811023545637, 0.07958543189024085140, 0.2665933059059887866 ) ) ;
#339 = CARTESIAN_POINT ( 'NONE',  ( 0.2867679344610365999, -0.2867679344610365444, -1.350393700787401619 ) ) ;
#340 = CARTESIAN_POINT ( 'NONE',  ( -1.023622047244093558, -0.1870078740157479769, 0.4822834645669291653 ) ) ;
#341 = CARTESIAN_POINT ( 'NONE',  ( 1.049868766404200127, -0.6046776061558809534, -0.2411417322834644161 ) ) ;
#342 = CARTESIAN_POINT ( 'NONE',  ( -0.1265901696524993347, 0.4724409448818895907, 0.2316272965879264956 ) ) ;
#343 = CARTESIAN_POINT ( 'NONE',  ( -0.3215223097112853146, -0.08942795157528024563, -0.3641732283464568787 ) ) ;
#344 = CLOSED_SHELL ( 'NONE', ( #79052, #33768, #52211, #21587, #26399, #17656, #70205, #46060, #62381, #39288, #25788, #19324, #81414, #28723, #19290, #156, #10629, #6095, #46496, #61602, #656, #8490, #16295, #73331, #72597, #52522, #44952 ) ) ;
#345 = CARTESIAN_POINT ( 'NONE',  ( 0.3937007874015754361, -0.1870078740157479769, 0.4822834645669291653 ) ) ;
#346 = CARTESIAN_POINT ( 'NONE',  ( -1.024276469446319116, 1.664626768191372896, -0.4581463608586889835 ) ) ;
#347 = CARTESIAN_POINT ( 'NONE',  ( 0.8398950131233602345, 0.1283753931104746893, -0.1820866141732285504 ) ) ;
#348 = CARTESIAN_POINT ( 'NONE',  ( 0.02624671916010564918, 0.1283753931104748280, 0.1820866141732283561 ) ) ;
#349 = CARTESIAN_POINT ( 'NONE',  ( 0.1181102362204730916, 0.2952755905511811885, 0.000000000000000000 ) ) ;
#350 = CARTESIAN_POINT ( 'NONE',  ( -1.207349081364828880, 0.2306618581243847221, -0.2411417322834647770 ) ) ;
#351 = CARTESIAN_POINT ( 'NONE',  ( -0.4986876640419939388, 0.1283753931104746893, -0.1820866141732285504 ) ) ;
#352 = DIRECTION ( 'NONE',  ( 0.000000000000000000, 1.000000000000000000, 0.000000000000000000 ) ) ;
#353 = CARTESIAN_POINT ( 'NONE',  ( -0.9580052493438311334, 0.05413385826771626580, -0.4176697321401330321 ) ) ;
#354 = CARTESIAN_POINT ( 'NONE',  ( 0.3996062992125985480, 2.446882876249141654E-17, -0.9822834645669291653 ) ) ;
#355 = CARTESIAN_POINT ( 'NONE',  ( 0.1049643490035303689, 0.3917322834645670104, -2.597769028871390606 ) ) ;
#356 = CARTESIAN_POINT ( 'NONE',  ( 0.3608923884514443348, 0.1771653543307087075, -0.09757992244046823083 ) ) ;
#357 = CARTESIAN_POINT ( 'NONE',  ( -0.6692913385826764205, 0.2952755905511811885, 0.000000000000000000 ) ) ;
#358 = CARTESIAN_POINT ( 'NONE',  ( -1.227034120734907141, -0.6692913385826773087, -0.1292274648535924053 ) ) ;
#359 = CARTESIAN_POINT ( 'NONE',  ( -1.023622047244093558, -0.1870078740157479769, 0.3641732283464567677 ) ) ;
#360 = CARTESIAN_POINT ( 'NONE',  ( 1.548556430446194954, 0.2306618581243847221, -0.2411417322834647770 ) ) ;
#361 =( BOUNDED_SURFACE ( )  B_SPLINE_SURFACE ( 1, 2, ( 
 ( #63527, #18507, #32782, #810, #5858, #57610, #388, #44971, #24798, #82892, #31534, #44150, #60014, #57190, #26473, #37849, #12602, #7111, #44556, #25212, #19741, #21303, #64772, #58024, #6692, #14998, #13435, #70667, #78982, #53273, #58450, #50878, #46956, #26045, #64355, #32362, #76578, #6273, #18906, #63937, #31949, #50466, #72648, #38677, #83301, #25623, #40655, #51704, #51286, #76989, #77406, #19319, #66339, #69842, #8678, #34348, #76170, #12192, #71092, #13023, #39091, #16663, #53684, #36007, #28856, #73906, #54518, #67177, #42303, #79392, #49035, #68001, #22549, #15842, #17080, #21711, #47375, #73065, #16247, #54100, #10346, #68413, #9098, #9506, #10753, #22132, #35179, #29273, #60840, #74732, #22955, #34771, #41076, #47790, #15415, #3607, #66765, #41490, #60430, #2781, #28441, #61677, #4018, #29682, #42717, #73494, #54937, #55344, #79815, #3192, #81051, #23365, #80643, #48211, #2369, #48622, #41894, #80233, #67588, #9918, #36413, #61253, #28025, #35590, #74317, #24189, #49858, #11989, #70043, #37643, #82687, #38054, #12397, #63730, #6070, #51083, #75558, #5658, #31744, #4837, #62918, #57406, #83097, #63320, #82283, #62086, #31325, #18307, #55757, #30093, #68820, #76780, #56989, #44761, #81463, #75146, #17898, #43534, #25006, #25418, #50678, #76377, #19112, #43122, #11582, #18711, #24601, #4427, #36824, #17491, #23781, #12815, #11165, #70457, #62499, #69233, #44352, #81877, #30512, #49452, #56174, #37241, #5251, #43949, #30915, #56582, #50270, #75967, #69645, #65422, #70888, #7756, #1029, #7325, #32994, #45185, #603, #51494, #13238, #38887, #40148, #33422, #64990, #26259, #64566, #27095, #26682, #51920, #45609, #52337, #71302, #20790, #32159, #78465, #72139, #52757, #46446, #46025, #6903, #77625, #14074, #6489, #59083, #19958, #39303, #13650, #58664, #39727, #64156, #14495, #1438, #78044, #32574, #38472, #25835, #182, #77197, #20373, #58236, #57815, #19528, #71719, #55293, #42669, #10291, #35538, #10706, #61200, #28804, #11113, #54047, #81002, #16610, #15785, #47737, #48159, #3141, #23316, #54468, #48985, #55704, #73435, #3557, #29222, #81412, #75094, #80181, #22496, #62037, #54889, #35958, #74684, #23729, #17442, #35122, #17030, #49400, #68368, #68769, #36362, #36770, #62446, #43072, #4782, #60788, #48569, #61627, #41437, #67120, #9451, #4374, #73854, #30042, #79761, #80594, #74267, #16195, #3969, #22078, #41841, #67531, #9869, #22902, #42253, #67948, #29632, #69994, #11939, #70409, #37594, #5202, #70840, #30458, #57351, #76329, #75509, #24138, #24553, #62865, #31692, #30866, #12765, #56531, #82234, #83047, #64517, #37186, #38422, #49808, #12349, #19483, #25370, #63683, #77151, #6021, #13189, #38838, #63267, #5608, #24951, #44303, #51033, #56122, #64104, #131, #38005, #76732, #81828, #17848, #43482, #50219, #31276, #45136, #11529, #75915, #18254, #43896, #69593, #56941, #82638, #44712, #19064, #6439, #32111, #50624, #18659, #57769, #25786, #51447, #69178, #13601, #32948, #52291, #53123, #46397, #52707, #58614, #66197, #71672, #59039, #7708, #33786, #14024, #1802, #45559, #981, #59865, #8534, #27884, #39255, #7277, #14856, #33375, #72090, #27465, #34202, #53544, #71255, #78834, #2218, #21160, #21567, #46816, #47229, #15270, #79252, #72919, #64937, #1393, #14449, #26209, #51871, #77577, #40517, #26637, #59450, #72507, #65373, #27047, #77996, #40100, #40931, #6854, #19909, #20324, #556, #45977, #8121, #32524, #65788, #39681, #58186, #78418, #20747, #23629, #66611, #10195, #29126, #28294, #60287, #60696, #15690, #67857, #67029, #23218, #9361, #41348, #35864, #17347, #73342, #74589, #2637, #22813, #55604, #61529, #16518, #29940, #42162, #49300, #75001, #73764, #41744, #61109, #80497, #3875, #8947, #48888, #36267, #48470, #29534, #34623, #53955, #79668, #35032, #67438, #81316, #47647, #3046, #28711, #54375, #80085, #22405, #48062, #80904, #74171, #55197, #16933, #16099, #9772, #42573, #54794, #68275, #10610, #35443, #3461, #61936, #4279, #21985, #5511, #69080, #18964, #24450, #11845, #43790, #69897, #50118, #37907, #81731, #11431, #12661, #44207 ),
 ( #17751, #37086, #62772, #75405, #49710, #43380, #57247, #24856, #12251, #31592, #5106, #30773, #25269, #31174, #5918, #63584, #56434, #82136, #75815, #82951, #82538, #56840, #18158, #44612, #69496, #37498, #63173, #50935, #50524, #76633, #24040, #76230, #38322, #70308, #63996, #36669, #18564, #6337, #32010, #57670, #32, #25685, #51345, #77049, #42975, #68671, #11010, #62344, #4683, #30354, #56023, #8022, #34099, #65693, #59762, #27783, #21058, #72410, #451, #13922, #58938, #38739, #64416, #6751, #53020, #45456, #71993, #46298, #77893, #39578, #26106, #1296, #78735, #53446, #32423, #58085, #13086, #51768, #20645, #33685, #26946, #877, #59347, #26536, #77470, #2117, #19381, #14346, #65268, #19807, #71154, #13495, #39151, #40006, #64836, #1704, #7174, #32845, #27361, #45033, #58514, #46718, #52189, #52607, #8431, #14759, #78314, #66095, #40414, #70732, #20224, #45873, #71571, #7604, #33278, #16416, #4180, #35757, #34937, #15169, #34520, #72819, #3773, #55096, #29437, #68169, #41246, #22713, #80804, #21882, #79986, #48789, #23121, #80400, #16005, #79154, #48371, #35347, #40825, #47129, #2538, #10512, #54689, #61839, #66510, #8844, #66933, #9266, #29023, #74486, #74070, #42063, #16833, #60186, #28614, #67758, #41652, #21471, #53854, #28196, #79567, #29843, #47546, #42469, #73236, #60599, #61423, #15587, #2949, #10092, #36165, #54271, #22299, #61009, #47960, #73664, #67343, #9676, #3358, #64624, #55921, #37810, #31078, #11751, #37407, #30257, #36990, #36571, #81634, #23945, #7383, #6961, #69399, #62669, #75307, #51977, #56746, #5009, #24353, #5417, #50022, #45663, #74901, #20012, #13706, #77682, #71359, #18471, #49612, #30679, #69806, #23530, #32632, #82039, #43694, #75721, #56340, #12154, #49200, #39361, #58295, #18061, #68982, #65046, #17249, #42878, #68571, #63079, #17651, #660, #10913, #62249, #26316, #55507, #43283, #82444, #24761, #50429, #81215, #76129, #4586, #11330, #44114, #1085, #34308, #26737, #7811, #14553, #14131, #59139, #33477, #67132, #66720, #46917, #40205, #52813, #28399, #8637, #65888, #1908, #66298, #27569, #22088, #52391, #79772, #73447, #54057, #47748, #79353, #1497, #8223, #47333, #78100, #9056, #59553, #21262, #53228, #33887, #73023, #20431, #15797, #15373, #78944, #46500, #41447, #46084, #71777, #39784, #72610, #27149, #41034, #65479, #78523, #34729, #33051, #20847, #14958, #59969, #40615, #58722, #53645, #72200, #2329, #27985, #21672, #60389, #2739, #48580, #28815, #48169, #3151, #17453, #68780, #43083, #81839, #16621, #61211, #75520, #43494, #24150, #4385, #42680, #56134, #68378, #49820, #17859, #42263, #67960, #3979, #23326, #30054, #9461, #49413, #62458, #48996, #10717, #35135, #60797, #54479, #67544, #10302, #80191, #73864, #9879, #35548, #3566, #41852, #16205, #29233, #23740, #74695, #36374, #81425, #54897, #80603, #75106, #55304, #55715, #62048, #22912, #74277, #35968, #11124, #17040, #81013, #61638, #36781, #29643, #4793, #30470, #22508, #50635, #64116, #12360, #57363, #38018, #76340, #25798, #37197, #32534, #142, #6033, #82649, #566, #62878, #5213, #30877, #83059, #37606, #77161, #56544, #75926, #19493, #51882, #5621, #18670, #12776, #44315, #58198, #6451, #18266, #24564, #31287, #82245, #70421, #50230, #24964, #43907, #69605, #11951, #45147, #70850, #13201, #26219, #77587, #38848, #64528, #31705, #70005, #6865, #19921, #38433, #25381, #69190, #32121, #51044, #63280, #56952, #63694, #11541, #44723, #76745, #19075, #57779, #51458, #7717, #78843, #53553, #21169, #66206, #21576, #26646, #78428, #46825, #65797, #45570, #20334, #991, #64947, #79676, #78006, #47238, #58624, #33385, #27893, #65382, #52300, #40527, #40940, #2228, #72517, #27474, #34631, #34211, #8131, #15279, #72928, #79261, #45986, #66619, #14865, #1812, #53132, #71682, #27058, #14034, #39690, #59048, #71264, #8957, #59461, #52717, #1402, #60295, #8545, #20756, #14458, #59874, #40110, #2645, #7287, #28302, #53964, #13611, #39265, #32957, #46406, #72100, #33796, #73350, #55612, #23225, #15698, #61116, #41355, #60704, #67036, #29948, #81323, #23637, #11020 ) ),
 .UNSPECIFIED., .F., .F., .F. ) 
 B_SPLINE_SURFACE_WITH_KNOTS ( ( 2, 2 ),
 ( 3, 2, 2, 2, 2, 2, 2, 2, 2, 2, 2, 2, 2, 2, 2, 2, 2, 2, 2, 2, 2, 2, 2, 2, 2, 2, 2, 2, 2, 2, 2, 2, 2, 2, 2, 2, 2, 2, 2, 2, 2, 2, 2, 2, 2, 2, 2, 2, 2, 2, 2, 2, 2, 2, 2, 2, 2, 2, 2, 2, 2, 2, 2, 2, 2, 2, 2, 2, 2, 2, 2, 2, 2, 2, 2, 2, 2, 2, 2, 2, 2, 2, 2, 2, 2, 2, 2, 2, 2, 2, 2, 2, 2, 2, 2, 2, 2, 2, 2, 2, 2, 2, 2, 2, 2, 2, 2, 2, 2, 2, 2, 2, 2, 2, 2, 2, 2, 2, 2, 2, 2, 2, 2, 2, 2, 2, 2, 2, 2, 2, 2, 2, 2, 2, 2, 2, 2, 2, 2, 2, 2, 2, 2, 2, 2, 2, 2, 2, 2, 2, 2, 2, 2, 2, 2, 2, 2, 2, 2, 2, 2, 2, 2, 2, 2, 2, 2, 2, 2, 2, 2, 2, 2, 2, 2, 2, 2, 2, 2, 2, 2, 2, 2, 2, 2, 2, 2, 2, 2, 2, 2, 2, 2, 2, 2, 2, 2, 2, 2, 2, 2, 2, 2, 2, 2, 2, 2, 2, 2, 2, 2, 2, 2, 2, 2, 2, 2, 2, 2, 2, 2, 2, 2, 2, 2, 2, 2, 2, 2, 2, 2, 2, 2, 2, 2, 2, 2, 2, 2, 2, 2, 2, 2, 2, 2, 2, 2, 2, 2, 2, 2, 2, 2, 2, 2, 3 ),
 ( 0.000000000000000000, 1.000000000000000000 ),
 ( 0.000000000000000000, 0.003787878787878787984, 0.007575757575757575968, 0.01136363636363636395, 0.01515151515151515194, 0.01893939393939393992, 0.02272727272727272790, 0.02651515151515151589, 0.03030303030303030387, 0.03409090909090908839, 0.03787878787878787984, 0.04166666666666666435, 0.04545454545454545581, 0.04924242424242424032, 0.05303030303030303177, 0.05681818181818181629, 0.06060606060606060774, 0.06439393939393939226, 0.06818181818181817677, 0.07196969696969697516, 0.07575757575757575968, 0.07954545454545454419, 0.08333333333333332871, 0.08712121212121212710, 0.09090909090909091161, 0.09469696969696969613, 0.09848484848484848064, 0.1022727272727272790, 0.1060606060606060635, 0.1098484848484848481, 0.1136363636363636326, 0.1174242424242424310, 0.1212121212121212155, 0.1250000000000000000, 0.1287878787878787845, 0.1325757575757575690, 0.1363636363636363535, 0.1401515151515151381, 0.1439393939393939503, 0.1477272727272727348, 0.1515151515151515194, 0.1553030303030303039, 0.1590909090909090884, 0.1628787878787878729, 0.1666666666666666574, 0.1704545454545454419, 0.1742424242424242542, 0.1780303030303030387, 0.1818181818181818232, 0.1856060606060606077, 0.1893939393939393923, 0.1931818181818181768, 0.1969696969696969613, 0.2007575757575757458, 0.2045454545454545581, 0.2083333333333333426, 0.2121212121212121271, 0.2159090909090909116, 0.2196969696969696961, 0.2234848484848484806, 0.2272727272727272652, 0.2310606060606060497, 0.2348484848484848619, 0.2386363636363636465, 0.2424242424242424310, 0.2462121212121212155, 0.2500000000000000000, 0.2537878787878787845, 0.2575757575757575690, 0.2613636363636363535, 0.2651515151515151381, 0.2689393939393939226, 0.2727272727272727071, 0.2765151515151514916, 0.2803030303030302761, 0.2840909090909091161, 0.2878787878787879007, 0.2916666666666666852, 0.2954545454545454697, 0.2992424242424242542, 0.3030303030303030387, 0.3068181818181818232, 0.3106060606060606077, 0.3143939393939393923, 0.3181818181818181768, 0.3219696969696969613, 0.3257575757575757458, 0.3295454545454545303, 0.3333333333333333148, 0.3371212121212120993, 0.3409090909090908839, 0.3446969696969697239, 0.3484848484848485084, 0.3522727272727272929, 0.3560606060606060774, 0.3598484848484848619, 0.3636363636363636465, 0.3674242424242424310, 0.3712121212121212155, 0.3750000000000000000, 0.3787878787878787845, 0.3825757575757575690, 0.3863636363636363535, 0.3901515151515151381, 0.3939393939393939226, 0.3977272727272727071, 0.4015151515151514916, 0.4053030303030302761, 0.4090909090909091161, 0.4128787878787879007, 0.4166666666666666852, 0.4204545454545454697, 0.4242424242424242542, 0.4280303030303030387, 0.4318181818181818232, 0.4356060606060606077, 0.4393939393939393923, 0.4431818181818181768, 0.4469696969696969613, 0.4507575757575757458, 0.4545454545454545303, 0.4583333333333333148, 0.4621212121212120993, 0.4659090909090908839, 0.4696969696969697239, 0.4734848484848485084, 0.4772727272727272929, 0.4810606060606060774, 0.4848484848484848619, 0.4886363636363636465, 0.4924242424242424310, 0.4962121212121212155, 0.5000000000000000000, 0.5037878787878787845, 0.5075757575757575690, 0.5113636363636363535, 0.5151515151515151381, 0.5189393939393939226, 0.5227272727272727071, 0.5265151515151514916, 0.5303030303030302761, 0.5340909090909090606, 0.5378787878787878451, 0.5416666666666666297, 0.5454545454545454142, 0.5492424242424241987, 0.5530303030303029832, 0.5568181818181817677, 0.5606060606060605522, 0.5643939393939394478, 0.5681818181818182323, 0.5719696969696970168, 0.5757575757575758013, 0.5795454545454545858, 0.5833333333333333703, 0.5871212121212121549, 0.5909090909090909394, 0.5946969696969697239, 0.5984848484848485084, 0.6022727272727272929, 0.6060606060606060774, 0.6098484848484848619, 0.6136363636363636465, 0.6174242424242424310, 0.6212121212121212155, 0.6250000000000000000, 0.6287878787878787845, 0.6325757575757575690, 0.6363636363636363535, 0.6401515151515151381, 0.6439393939393939226, 0.6477272727272727071, 0.6515151515151514916, 0.6553030303030302761, 0.6590909090909090606, 0.6628787878787878451, 0.6666666666666666297, 0.6704545454545454142, 0.6742424242424241987, 0.6780303030303029832, 0.6818181818181817677, 0.6856060606060605522, 0.6893939393939394478, 0.6931818181818182323, 0.6969696969696970168, 0.7007575757575758013, 0.7045454545454545858, 0.7083333333333333703, 0.7121212121212121549, 0.7159090909090909394, 0.7196969696969697239, 0.7234848484848485084, 0.7272727272727272929, 0.7310606060606060774, 0.7348484848484848619, 0.7386363636363636465, 0.7424242424242424310, 0.7462121212121212155, 0.7500000000000000000, 0.7537878787878787845, 0.7575757575757575690, 0.7613636363636363535, 0.7651515151515151381, 0.7689393939393939226, 0.7727272727272727071, 0.7765151515151514916, 0.7803030303030302761, 0.7840909090909090606, 0.7878787878787878451, 0.7916666666666666297, 0.7954545454545454142, 0.7992424242424241987, 0.8030303030303029832, 0.8068181818181817677, 0.8106060606060605522, 0.8143939393939394478, 0.8181818181818182323, 0.8219696969696970168, 0.8257575757575758013, 0.8295454545454545858, 0.8333333333333333703, 0.8371212121212121549, 0.8409090909090909394, 0.8446969696969697239, 0.8484848484848485084, 0.8522727272727272929, 0.8560606060606060774, 0.8598484848484848619, 0.8636363636363636465, 0.8674242424242424310, 0.8712121212121212155, 0.8750000000000000000, 0.8787878787878787845, 0.8825757575757575690, 0.8863636363636363535, 0.8901515151515151381, 0.8939393939393939226, 0.8977272727272727071, 0.9015151515151514916, 0.9053030303030302761, 0.9090909090909090606, 0.9128787878787878451, 0.9166666666666666297, 0.9204545454545454142, 0.9242424242424241987, 0.9280303030303029832, 0.9318181818181817677, 0.9356060606060605522, 0.9393939393939394478, 0.9431818181818182323, 0.9469696969696970168, 0.9507575757575758013, 0.9545454545454545858, 0.9583333333333333703, 0.9621212121212121549, 0.9659090909090909394 ),
 .UNSPECIFIED. ) 
 GEOMETRIC_REPRESENTATION_ITEM ( )  RATIONAL_B_SPLINE_SURFACE ( (
 ( 1.000000000000000000, 0.9659258262890683122, 1.000000000000000000, 0.9659258262890683122, 1.000000000000000000, 0.9659258262890683122, 1.000000000000000000, 0.9659258262890683122, 1.000000000000000000, 0.9659258262890683122, 1.000000000000000000, 0.9659258262890683122, 1.000000000000000000, 0.9659258262890683122, 1.000000000000000000, 0.9659258262890683122, 1.000000000000000000, 0.9659258262890683122, 1.000000000000000000, 0.9659258262890683122, 1.000000000000000000, 0.9659258262890683122, 1.000000000000000000, 0.9659258262890683122, 1.000000000000000000, 0.9659258262890683122, 1.000000000000000000, 0.9659258262890683122, 1.000000000000000000, 0.9659258262890683122, 1.000000000000000000, 0.9659258262890683122, 1.000000000000000000, 0.9659258262890683122, 1.000000000000000000, 0.9659258262890683122, 1.000000000000000000, 0.9659258262890683122, 1.000000000000000000, 0.9659258262890683122, 1.000000000000000000, 0.9659258262890683122, 1.000000000000000000, 0.9659258262890683122, 1.000000000000000000, 0.9659258262890683122, 1.000000000000000000, 0.9659258262890683122, 1.000000000000000000, 0.9659258262890683122, 1.000000000000000000, 0.9659258262890683122, 1.000000000000000000, 0.9659258262890683122, 1.000000000000000000, 0.9659258262890683122, 1.000000000000000000, 0.9659258262890683122, 1.000000000000000000, 0.9659258262890683122, 1.000000000000000000, 0.9659258262890683122, 1.000000000000000000, 0.9659258262890683122, 1.000000000000000000, 0.9659258262890683122, 1.000000000000000000, 0.9659258262890683122, 1.000000000000000000, 0.9659258262890683122, 1.000000000000000000, 0.9659258262890683122, 1.000000000000000000, 0.9659258262890683122, 1.000000000000000000, 0.9659258262890683122, 1.000000000000000000, 0.9659258262890683122, 1.000000000000000000, 0.9659258262890683122, 1.000000000000000000, 0.9659258262890683122, 1.000000000000000000, 0.9659258262890683122, 1.000000000000000000, 0.9659258262890683122, 1.000000000000000000, 0.9659258262890683122, 1.000000000000000000, 0.9659258262890683122, 1.000000000000000000, 0.9659258262890683122, 1.000000000000000000, 0.9659258262890683122, 1.000000000000000000, 0.9659258262890683122, 1.000000000000000000, 0.9659258262890683122, 1.000000000000000000, 0.9659258262890683122, 1.000000000000000000, 0.9659258262890683122, 1.000000000000000000, 0.9659258262890683122, 1.000000000000000000, 0.9659258262890683122, 1.000000000000000000, 0.9659258262890683122, 1.000000000000000000, 0.9659258262890683122, 1.000000000000000000, 0.9659258262890683122, 1.000000000000000000, 0.9659258262890683122, 1.000000000000000000, 0.9659258262890683122, 1.000000000000000000, 0.9659258262890683122, 1.000000000000000000, 0.9659258262890683122, 1.000000000000000000, 0.9659258262890683122, 1.000000000000000000, 0.9659258262890683122, 1.000000000000000000, 0.9659258262890683122, 1.000000000000000000, 0.9659258262890683122, 1.000000000000000000, 0.9659258262890683122, 1.000000000000000000, 0.9659258262890683122, 1.000000000000000000, 0.9659258262890683122, 1.000000000000000000, 0.9659258262890683122, 1.000000000000000000, 0.9659258262890683122, 1.000000000000000000, 0.9659258262890683122, 1.000000000000000000, 0.9659258262890683122, 1.000000000000000000, 0.9659258262890683122, 1.000000000000000000, 0.9659258262890683122, 1.000000000000000000, 0.9659258262890683122, 1.000000000000000000, 0.9659258262890683122, 1.000000000000000000, 0.9659258262890683122, 1.000000000000000000, 0.9659258262890683122, 1.000000000000000000, 0.9659258262890683122, 1.000000000000000000, 0.9659258262890683122, 1.000000000000000000, 0.9659258262890683122, 1.000000000000000000, 0.9659258262890683122, 1.000000000000000000, 0.9659258262890683122, 1.000000000000000000, 0.9659258262890683122, 1.000000000000000000, 0.9659258262890683122, 1.000000000000000000, 0.9659258262890683122, 1.000000000000000000, 0.9659258262890683122, 1.000000000000000000, 0.9659258262890683122, 1.000000000000000000, 0.9659258262890683122, 1.000000000000000000, 0.9659258262890683122, 1.000000000000000000, 0.9659258262890683122, 1.000000000000000000, 0.9659258262890683122, 1.000000000000000000, 0.9659258262890683122, 1.000000000000000000, 0.9659258262890683122, 1.000000000000000000, 0.9659258262890683122, 1.000000000000000000, 0.9659258262890683122, 1.000000000000000000, 0.9659258262890683122, 1.000000000000000000, 0.9659258262890683122, 1.000000000000000000, 0.9659258262890683122, 1.000000000000000000, 0.9659258262890683122, 1.000000000000000000, 0.9659258262890683122, 1.000000000000000000, 0.9659258262890683122, 1.000000000000000000, 0.9659258262890683122, 1.000000000000000000, 0.9659258262890683122, 1.000000000000000000, 0.9659258262890683122, 1.000000000000000000, 0.9659258262890683122, 1.000000000000000000, 0.9659258262890683122, 1.000000000000000000, 0.9659258262890683122, 1.000000000000000000, 0.9659258262890683122, 1.000000000000000000, 0.9659258262890683122, 1.000000000000000000, 0.9659258262890683122, 1.000000000000000000, 0.9659258262890683122, 1.000000000000000000, 0.9659258262890683122, 1.000000000000000000, 0.9659258262890683122, 1.000000000000000000, 0.9659258262890683122, 1.000000000000000000, 0.9659258262890683122, 1.000000000000000000, 0.9659258262890683122, 1.000000000000000000, 0.9659258262890683122, 1.000000000000000000, 0.9659258262890683122, 1.000000000000000000, 0.9659258262890683122, 1.000000000000000000, 0.9659258262890683122, 1.000000000000000000, 0.9659258262890683122, 1.000000000000000000, 0.9659258262890683122, 1.000000000000000000, 0.9659258262890683122, 1.000000000000000000, 0.9659258262890683122, 1.000000000000000000, 0.9659258262890683122, 1.000000000000000000, 0.9659258262890683122, 1.000000000000000000, 0.9659258262890683122, 1.000000000000000000, 0.9659258262890683122, 1.000000000000000000, 0.9659258262890683122, 1.000000000000000000, 0.9659258262890683122, 1.000000000000000000, 0.9659258262890683122, 1.000000000000000000, 0.9659258262890683122, 1.000000000000000000, 0.9659258262890683122, 1.000000000000000000, 0.9659258262890683122, 1.000000000000000000, 0.9659258262890683122, 1.000000000000000000, 0.9659258262890683122, 1.000000000000000000, 0.9659258262890683122, 1.000000000000000000, 0.9659258262890683122, 1.000000000000000000, 0.9659258262890683122, 1.000000000000000000, 0.9659258262890683122, 1.000000000000000000, 0.9659258262890683122, 1.000000000000000000, 0.9659258262890683122, 1.000000000000000000, 0.9659258262890683122, 1.000000000000000000, 0.9659258262890683122, 1.000000000000000000, 0.9659258262890683122, 1.000000000000000000, 0.9659258262890683122, 1.000000000000000000, 0.9659258262890683122, 1.000000000000000000, 0.9659258262890683122, 1.000000000000000000, 0.9659258262890683122, 1.000000000000000000, 0.9659258262890683122, 1.000000000000000000, 0.9659258262890683122, 1.000000000000000000, 0.9659258262890683122, 1.000000000000000000, 0.9659258262890683122, 1.000000000000000000, 0.9659258262890683122, 1.000000000000000000, 0.9659258262890683122, 1.000000000000000000, 0.9659258262890683122, 1.000000000000000000, 0.9659258262890683122, 1.000000000000000000, 0.9659258262890683122, 1.000000000000000000, 0.9659258262890683122, 1.000000000000000000, 0.9659258262890683122, 1.000000000000000000, 0.9659258262890683122, 1.000000000000000000, 0.9659258262890683122, 1.000000000000000000, 0.9659258262890683122, 1.000000000000000000, 0.9659258262890683122, 1.000000000000000000, 0.9659258262890683122, 1.000000000000000000, 0.9659258262890683122, 1.000000000000000000, 0.9659258262890683122, 1.000000000000000000, 0.9659258262890683122, 1.000000000000000000, 0.9659258262890683122, 1.000000000000000000, 0.9659258262890683122, 1.000000000000000000, 0.9659258262890683122, 1.000000000000000000, 0.9659258262890683122, 1.000000000000000000, 0.9659258262890683122, 1.000000000000000000, 0.9659258262890683122, 1.000000000000000000, 0.9659258262890683122, 1.000000000000000000, 0.9659258262890683122, 1.000000000000000000, 0.9659258262890683122, 1.000000000000000000, 0.9659258262890683122, 1.000000000000000000, 0.9659258262890683122, 1.000000000000000000, 0.9659258262890683122, 1.000000000000000000, 0.9659258262890683122, 1.000000000000000000, 0.9659258262890683122, 1.000000000000000000, 0.9659258262890683122, 1.000000000000000000, 0.9659258262890683122, 1.000000000000000000, 0.9659258262890683122, 1.000000000000000000, 0.9659258262890683122, 1.000000000000000000, 0.9659258262890683122, 1.000000000000000000, 0.9659258262890683122, 1.000000000000000000, 0.9659258262890683122, 1.000000000000000000, 0.9659258262890683122, 1.000000000000000000, 0.9659258262890683122, 1.000000000000000000, 0.9659258262890683122, 1.000000000000000000, 0.9659258262890683122, 1.000000000000000000, 0.9659258262890683122, 1.000000000000000000, 0.9659258262890683122, 1.000000000000000000, 0.9659258262890683122, 1.000000000000000000, 0.9659258262890683122, 1.000000000000000000, 0.9659258262890683122, 1.000000000000000000, 0.9659258262890683122, 1.000000000000000000, 0.9659258262890683122, 1.000000000000000000, 0.9659258262890683122, 1.000000000000000000, 0.9659258262890683122, 1.000000000000000000, 0.9659258262890683122, 1.000000000000000000, 0.9659258262890683122, 1.000000000000000000, 0.9659258262890683122, 1.000000000000000000, 0.9659258262890683122, 1.000000000000000000, 0.9659258262890683122, 1.000000000000000000, 0.9659258262890683122, 1.000000000000000000, 0.9659258262890683122, 1.000000000000000000, 0.9659258262890683122, 1.000000000000000000, 0.9659258262890683122, 1.000000000000000000, 0.9659258262890683122, 1.000000000000000000, 0.9659258262890683122, 1.000000000000000000, 0.9659258262890683122, 1.000000000000000000, 0.9659258262890683122, 1.000000000000000000, 0.9659258262890683122, 1.000000000000000000, 0.9659258262890683122, 1.000000000000000000, 0.9659258262890683122, 1.000000000000000000, 0.9659258262890683122, 1.000000000000000000, 0.9659258262890683122, 1.000000000000000000, 0.9659258262890683122, 1.000000000000000000, 0.9659258262890683122, 1.000000000000000000, 0.9659258262890683122, 1.000000000000000000, 0.9659258262890683122, 1.000000000000000000, 0.9659258262890683122, 1.000000000000000000, 0.9659258262890683122, 1.000000000000000000, 0.9659258262890683122, 1.000000000000000000, 0.9659258262890683122, 1.000000000000000000, 0.9659258262890683122, 1.000000000000000000, 0.9659258262890683122, 1.000000000000000000, 0.9659258262890683122, 1.000000000000000000, 0.9659258262890683122, 1.000000000000000000, 0.9659258262890683122, 1.000000000000000000, 0.9659258262890683122, 1.000000000000000000, 0.9659258262890683122, 1.000000000000000000, 0.9659258262890683122, 1.000000000000000000, 0.9659258262890683122, 1.000000000000000000, 0.9659258262890683122, 1.000000000000000000, 0.9659258262890683122, 1.000000000000000000, 0.9659258262890683122, 1.000000000000000000, 0.9659258262890683122, 1.000000000000000000, 0.9659258262890683122, 1.000000000000000000, 0.9659258262890683122, 1.000000000000000000, 0.9659258262890683122, 1.000000000000000000, 0.9659258262890683122, 1.000000000000000000, 0.9659258262890683122, 1.000000000000000000, 0.9659258262890683122, 1.000000000000000000, 0.9659258262890683122, 1.000000000000000000, 0.9659258262890683122, 1.000000000000000000, 0.9659258262890683122, 1.000000000000000000, 0.9659258262890683122, 1.000000000000000000, 0.9659258262890683122, 1.000000000000000000, 0.9659258262890683122, 1.000000000000000000, 0.9659258262890683122, 1.000000000000000000, 0.9659258262890683122, 1.000000000000000000),
 ( 1.000000000000000000, 0.9659258262890683122, 1.000000000000000000, 0.9659258262890683122, 1.000000000000000000, 0.9659258262890683122, 1.000000000000000000, 0.9659258262890683122, 1.000000000000000000, 0.9659258262890683122, 1.000000000000000000, 0.9659258262890683122, 1.000000000000000000, 0.9659258262890683122, 1.000000000000000000, 0.9659258262890683122, 1.000000000000000000, 0.9659258262890683122, 1.000000000000000000, 0.9659258262890683122, 1.000000000000000000, 0.9659258262890683122, 1.000000000000000000, 0.9659258262890683122, 1.000000000000000000, 0.9659258262890683122, 1.000000000000000000, 0.9659258262890683122, 1.000000000000000000, 0.9659258262890683122, 1.000000000000000000, 0.9659258262890683122, 1.000000000000000000, 0.9659258262890683122, 1.000000000000000000, 0.9659258262890683122, 1.000000000000000000, 0.9659258262890683122, 1.000000000000000000, 0.9659258262890683122, 1.000000000000000000, 0.9659258262890683122, 1.000000000000000000, 0.9659258262890683122, 1.000000000000000000, 0.9659258262890683122, 1.000000000000000000, 0.9659258262890683122, 1.000000000000000000, 0.9659258262890683122, 1.000000000000000000, 0.9659258262890683122, 1.000000000000000000, 0.9659258262890683122, 1.000000000000000000, 0.9659258262890683122, 1.000000000000000000, 0.9659258262890683122, 1.000000000000000000, 0.9659258262890683122, 1.000000000000000000, 0.9659258262890683122, 1.000000000000000000, 0.9659258262890683122, 1.000000000000000000, 0.9659258262890683122, 1.000000000000000000, 0.9659258262890683122, 1.000000000000000000, 0.9659258262890683122, 1.000000000000000000, 0.9659258262890683122, 1.000000000000000000, 0.9659258262890683122, 1.000000000000000000, 0.9659258262890683122, 1.000000000000000000, 0.9659258262890683122, 1.000000000000000000, 0.9659258262890683122, 1.000000000000000000, 0.9659258262890683122, 1.000000000000000000, 0.9659258262890683122, 1.000000000000000000, 0.9659258262890683122, 1.000000000000000000, 0.9659258262890683122, 1.000000000000000000, 0.9659258262890683122, 1.000000000000000000, 0.9659258262890683122, 1.000000000000000000, 0.9659258262890683122, 1.000000000000000000, 0.9659258262890683122, 1.000000000000000000, 0.9659258262890683122, 1.000000000000000000, 0.9659258262890683122, 1.000000000000000000, 0.9659258262890683122, 1.000000000000000000, 0.9659258262890683122, 1.000000000000000000, 0.9659258262890683122, 1.000000000000000000, 0.9659258262890683122, 1.000000000000000000, 0.9659258262890683122, 1.000000000000000000, 0.9659258262890683122, 1.000000000000000000, 0.9659258262890683122, 1.000000000000000000, 0.9659258262890683122, 1.000000000000000000, 0.9659258262890683122, 1.000000000000000000, 0.9659258262890683122, 1.000000000000000000, 0.9659258262890683122, 1.000000000000000000, 0.9659258262890683122, 1.000000000000000000, 0.9659258262890683122, 1.000000000000000000, 0.9659258262890683122, 1.000000000000000000, 0.9659258262890683122, 1.000000000000000000, 0.9659258262890683122, 1.000000000000000000, 0.9659258262890683122, 1.000000000000000000, 0.9659258262890683122, 1.000000000000000000, 0.9659258262890683122, 1.000000000000000000, 0.9659258262890683122, 1.000000000000000000, 0.9659258262890683122, 1.000000000000000000, 0.9659258262890683122, 1.000000000000000000, 0.9659258262890683122, 1.000000000000000000, 0.9659258262890683122, 1.000000000000000000, 0.9659258262890683122, 1.000000000000000000, 0.9659258262890683122, 1.000000000000000000, 0.9659258262890683122, 1.000000000000000000, 0.9659258262890683122, 1.000000000000000000, 0.9659258262890683122, 1.000000000000000000, 0.9659258262890683122, 1.000000000000000000, 0.9659258262890683122, 1.000000000000000000, 0.9659258262890683122, 1.000000000000000000, 0.9659258262890683122, 1.000000000000000000, 0.9659258262890683122, 1.000000000000000000, 0.9659258262890683122, 1.000000000000000000, 0.9659258262890683122, 1.000000000000000000, 0.9659258262890683122, 1.000000000000000000, 0.9659258262890683122, 1.000000000000000000, 0.9659258262890683122, 1.000000000000000000, 0.9659258262890683122, 1.000000000000000000, 0.9659258262890683122, 1.000000000000000000, 0.9659258262890683122, 1.000000000000000000, 0.9659258262890683122, 1.000000000000000000, 0.9659258262890683122, 1.000000000000000000, 0.9659258262890683122, 1.000000000000000000, 0.9659258262890683122, 1.000000000000000000, 0.9659258262890683122, 1.000000000000000000, 0.9659258262890683122, 1.000000000000000000, 0.9659258262890683122, 1.000000000000000000, 0.9659258262890683122, 1.000000000000000000, 0.9659258262890683122, 1.000000000000000000, 0.9659258262890683122, 1.000000000000000000, 0.9659258262890683122, 1.000000000000000000, 0.9659258262890683122, 1.000000000000000000, 0.9659258262890683122, 1.000000000000000000, 0.9659258262890683122, 1.000000000000000000, 0.9659258262890683122, 1.000000000000000000, 0.9659258262890683122, 1.000000000000000000, 0.9659258262890683122, 1.000000000000000000, 0.9659258262890683122, 1.000000000000000000, 0.9659258262890683122, 1.000000000000000000, 0.9659258262890683122, 1.000000000000000000, 0.9659258262890683122, 1.000000000000000000, 0.9659258262890683122, 1.000000000000000000, 0.9659258262890683122, 1.000000000000000000, 0.9659258262890683122, 1.000000000000000000, 0.9659258262890683122, 1.000000000000000000, 0.9659258262890683122, 1.000000000000000000, 0.9659258262890683122, 1.000000000000000000, 0.9659258262890683122, 1.000000000000000000, 0.9659258262890683122, 1.000000000000000000, 0.9659258262890683122, 1.000000000000000000, 0.9659258262890683122, 1.000000000000000000, 0.9659258262890683122, 1.000000000000000000, 0.9659258262890683122, 1.000000000000000000, 0.9659258262890683122, 1.000000000000000000, 0.9659258262890683122, 1.000000000000000000, 0.9659258262890683122, 1.000000000000000000, 0.9659258262890683122, 1.000000000000000000, 0.9659258262890683122, 1.000000000000000000, 0.9659258262890683122, 1.000000000000000000, 0.9659258262890683122, 1.000000000000000000, 0.9659258262890683122, 1.000000000000000000, 0.9659258262890683122, 1.000000000000000000, 0.9659258262890683122, 1.000000000000000000, 0.9659258262890683122, 1.000000000000000000, 0.9659258262890683122, 1.000000000000000000, 0.9659258262890683122, 1.000000000000000000, 0.9659258262890683122, 1.000000000000000000, 0.9659258262890683122, 1.000000000000000000, 0.9659258262890683122, 1.000000000000000000, 0.9659258262890683122, 1.000000000000000000, 0.9659258262890683122, 1.000000000000000000, 0.9659258262890683122, 1.000000000000000000, 0.9659258262890683122, 1.000000000000000000, 0.9659258262890683122, 1.000000000000000000, 0.9659258262890683122, 1.000000000000000000, 0.9659258262890683122, 1.000000000000000000, 0.9659258262890683122, 1.000000000000000000, 0.9659258262890683122, 1.000000000000000000, 0.9659258262890683122, 1.000000000000000000, 0.9659258262890683122, 1.000000000000000000, 0.9659258262890683122, 1.000000000000000000, 0.9659258262890683122, 1.000000000000000000, 0.9659258262890683122, 1.000000000000000000, 0.9659258262890683122, 1.000000000000000000, 0.9659258262890683122, 1.000000000000000000, 0.9659258262890683122, 1.000000000000000000, 0.9659258262890683122, 1.000000000000000000, 0.9659258262890683122, 1.000000000000000000, 0.9659258262890683122, 1.000000000000000000, 0.9659258262890683122, 1.000000000000000000, 0.9659258262890683122, 1.000000000000000000, 0.9659258262890683122, 1.000000000000000000, 0.9659258262890683122, 1.000000000000000000, 0.9659258262890683122, 1.000000000000000000, 0.9659258262890683122, 1.000000000000000000, 0.9659258262890683122, 1.000000000000000000, 0.9659258262890683122, 1.000000000000000000, 0.9659258262890683122, 1.000000000000000000, 0.9659258262890683122, 1.000000000000000000, 0.9659258262890683122, 1.000000000000000000, 0.9659258262890683122, 1.000000000000000000, 0.9659258262890683122, 1.000000000000000000, 0.9659258262890683122, 1.000000000000000000, 0.9659258262890683122, 1.000000000000000000, 0.9659258262890683122, 1.000000000000000000, 0.9659258262890683122, 1.000000000000000000, 0.9659258262890683122, 1.000000000000000000, 0.9659258262890683122, 1.000000000000000000, 0.9659258262890683122, 1.000000000000000000, 0.9659258262890683122, 1.000000000000000000, 0.9659258262890683122, 1.000000000000000000, 0.9659258262890683122, 1.000000000000000000, 0.9659258262890683122, 1.000000000000000000, 0.9659258262890683122, 1.000000000000000000, 0.9659258262890683122, 1.000000000000000000, 0.9659258262890683122, 1.000000000000000000, 0.9659258262890683122, 1.000000000000000000, 0.9659258262890683122, 1.000000000000000000, 0.9659258262890683122, 1.000000000000000000, 0.9659258262890683122, 1.000000000000000000, 0.9659258262890683122, 1.000000000000000000, 0.9659258262890683122, 1.000000000000000000, 0.9659258262890683122, 1.000000000000000000, 0.9659258262890683122, 1.000000000000000000, 0.9659258262890683122, 1.000000000000000000, 0.9659258262890683122, 1.000000000000000000, 0.9659258262890683122, 1.000000000000000000, 0.9659258262890683122, 1.000000000000000000, 0.9659258262890683122, 1.000000000000000000, 0.9659258262890683122, 1.000000000000000000, 0.9659258262890683122, 1.000000000000000000, 0.9659258262890683122, 1.000000000000000000, 0.9659258262890683122, 1.000000000000000000, 0.9659258262890683122, 1.000000000000000000, 0.9659258262890683122, 1.000000000000000000, 0.9659258262890683122, 1.000000000000000000, 0.9659258262890683122, 1.000000000000000000, 0.9659258262890683122, 1.000000000000000000, 0.9659258262890683122, 1.000000000000000000, 0.9659258262890683122, 1.000000000000000000, 0.9659258262890683122, 1.000000000000000000, 0.9659258262890683122, 1.000000000000000000, 0.9659258262890683122, 1.000000000000000000, 0.9659258262890683122, 1.000000000000000000, 0.9659258262890683122, 1.000000000000000000, 0.9659258262890683122, 1.000000000000000000, 0.9659258262890683122, 1.000000000000000000, 0.9659258262890683122, 1.000000000000000000, 0.9659258262890683122, 1.000000000000000000, 0.9659258262890683122, 1.000000000000000000, 0.9659258262890683122, 1.000000000000000000, 0.9659258262890683122, 1.000000000000000000, 0.9659258262890683122, 1.000000000000000000, 0.9659258262890683122, 1.000000000000000000, 0.9659258262890683122, 1.000000000000000000, 0.9659258262890683122, 1.000000000000000000, 0.9659258262890683122, 1.000000000000000000, 0.9659258262890683122, 1.000000000000000000, 0.9659258262890683122, 1.000000000000000000, 0.9659258262890683122, 1.000000000000000000, 0.9659258262890683122, 1.000000000000000000, 0.9659258262890683122, 1.000000000000000000, 0.9659258262890683122, 1.000000000000000000, 0.9659258262890683122, 1.000000000000000000, 0.9659258262890683122, 1.000000000000000000, 0.9659258262890683122, 1.000000000000000000, 0.9659258262890683122, 1.000000000000000000, 0.9659258262890683122, 1.000000000000000000, 0.9659258262890683122, 1.000000000000000000, 0.9659258262890683122, 1.000000000000000000, 0.9659258262890683122, 1.000000000000000000, 0.9659258262890683122, 1.000000000000000000, 0.9659258262890683122, 1.000000000000000000, 0.9659258262890683122, 1.000000000000000000, 0.9659258262890683122, 1.000000000000000000, 0.9659258262890683122, 1.000000000000000000, 0.9659258262890683122, 1.000000000000000000, 0.9659258262890683122, 1.000000000000000000, 0.9659258262890683122, 1.000000000000000000, 0.9659258262890683122, 1.000000000000000000, 0.9659258262890683122, 1.000000000000000000, 0.9659258262890683122, 1.000000000000000000, 0.9659258262890683122, 1.000000000000000000) ) ) 
 REPRESENTATION_ITEM ( '' )  SURFACE ( )  );
#362 = CARTESIAN_POINT ( 'NONE',  ( -0.9580052493438311334, -0.004921259842519870586, -0.3153832671262229437 ) ) ;
#363 = CARTESIAN_POINT ( 'NONE',  ( -1.377952755905511140, 0.1771653543307087630, 0.000000000000000000 ) ) ;
#364 = CARTESIAN_POINT ( 'NONE',  ( 1.450131233595801428, 0.2952755905511811885, 0.1292274648535926551 ) ) ;
#365 = CARTESIAN_POINT ( 'NONE',  ( -0.3996062992125987146, 0.1070741851644051862, 0.1246719160104986790 ) ) ;
#366 = CIRCLE ( 'NONE', #79699, 0.2755905511811031494 ) ;
#367 = CARTESIAN_POINT ( 'NONE',  ( -0.3917322834645670659, -7.196005306013484475E-17, -1.925872334154542509 ) ) ;
#368 = ORIENTED_EDGE ( 'NONE', *, *, #43225, .F. ) ;
#369 = CARTESIAN_POINT ( 'NONE',  ( 0.3149606299212637239, 2.165354330708661568, -1.076935383196056417 ) ) ;
#370 = CARTESIAN_POINT ( 'NONE',  ( 1.410761154855643795, -0.2845877964562159024, 0.3641732283464567677 ) ) ;
#371 = CARTESIAN_POINT ( 'NONE',  ( -1.351706036745406347, 0.05413385826771626580, -0.4176697321401330321 ) ) ;
#372 = CARTESIAN_POINT ( 'NONE',  ( -1.594488188976377119, 0.1660481256975883668, -0.3530559997133364547 ) ) ;
#373 = CARTESIAN_POINT ( 'NONE',  ( 0.1049643490035303689, 0.3917322834645670104, -1.810367454068241511 ) ) ;
#374 = DIRECTION ( 'NONE',  ( 0.000000000000000000, -0.000000000000000000, 1.000000000000000000 ) ) ;
#375 = CARTESIAN_POINT ( 'NONE',  ( 0.5971128608923891301, 0.2952755905511810774, -0.1292274648535930714 ) ) ;
#376 = CARTESIAN_POINT ( 'NONE',  ( 0.1181102362204730916, 0.2952755905511811885, 0.000000000000000000 ) ) ;
#377 = CARTESIAN_POINT ( 'NONE',  ( 0.06179655389848991154, 1.065998012190817246, -3.936642156184892105 ) ) ;
#378 = CARTESIAN_POINT ( 'NONE',  ( -0.6430446194225712953, 0.05413385826771626580, -0.4176697321401330321 ) ) ;
#379 = CARTESIAN_POINT ( 'NONE',  ( 0.6758530183727039509, 0.1771653543307087075, -0.09757992244046823083 ) ) ;
#380 = CARTESIAN_POINT ( 'NONE',  ( 0.1998031496062992740, 0.3460692066303959757, -1.404199475065616820 ) ) ;
#381 = ORIENTED_EDGE ( 'NONE', *, *, #63426, .T. ) ;
#382 = CARTESIAN_POINT ( 'NONE',  ( 4.797336870675656522E-17, -0.3917322834645670659, 0.08200168159348891761 ) ) ;
#383 = EDGE_LOOP ( 'NONE', ( #46578, #71434, #76162, #29656 ) ) ;
#384 = CARTESIAN_POINT ( 'NONE',  ( -0.07874015748031421014, -0.1870078740157480879, -0.4822834645669291653 ) ) ;
#385 = CARTESIAN_POINT ( 'NONE',  ( -1.332020997375327642, -0.05778040916215522460, 0.4822834645669289988 ) ) ;
#386 = CARTESIAN_POINT ( 'NONE',  ( 0.5708661417322842269, 0.1660481256975885056, 0.3530559997133364547 ) ) ;
#387 = CARTESIAN_POINT ( 'NONE',  ( 1.030183727034121421, -0.05778040916215522460, 0.4822834645669289988 ) ) ;
#388 = CARTESIAN_POINT ( 'NONE',  ( 1.574803149606299746, -0.1870078740157479769, 0.4822834645669291653 ) ) ;
#389 = CARTESIAN_POINT ( 'NONE',  ( -0.3543307086614165824, 0.2952755905511811885, 0.000000000000000000 ) ) ;
#390 = CARTESIAN_POINT ( 'NONE',  ( -0.1640419947506555343, -0.3162353388693405765, 0.4822834645669290543 ) ) ;
#391 = CARTESIAN_POINT ( 'NONE',  ( 1.482939632545932307, 0.05413385826771626580, -0.4176697321401330321 ) ) ;
#392 = CARTESIAN_POINT ( 'NONE',  ( 1.443569553805774897, 0.2306618581243848609, 0.2411417322834645549 ) ) ;
#393 = CARTESIAN_POINT ( 'NONE',  ( 1.345144356955381593, -0.05778040916215522460, 0.4822834645669289988 ) ) ;
#394 = CARTESIAN_POINT ( 'NONE',  ( -0.3083989501312330295, -0.05778040916215522460, 0.4822834645669289988 ) ) ;
#395 = CARTESIAN_POINT ( 'NONE',  ( 0.2867679344610365999, -0.2867679344610365444, -0.2480314960629920740 ) ) ;
#396 = CARTESIAN_POINT ( 'NONE',  ( 0.2755905511811031494, 0.1771653543307087630, 0.000000000000000000 ) ) ;
#397 = ORIENTED_EDGE ( 'NONE', *, *, #78869, .T. ) ;
#398 = CARTESIAN_POINT ( 'NONE',  ( -0.3420746716998661618, 0.1974969037888702206, -0.6561679790026245795 ) ) ;
#399 = B_SPLINE_CURVE_WITH_KNOTS ( 'NONE', 3,
 ( #14331, #45441, #8006, #13068 ),
 .UNSPECIFIED., .F., .F.,
 ( 4, 4 ),
 ( 0.05904796282231847965, 0.06105363127456257810 ),
 .UNSPECIFIED. ) ;
#400 = VERTEX_POINT ( 'NONE', #34658 ) ;
#401 = CARTESIAN_POINT ( 'NONE',  ( -0.4593175853018366950, -0.004921259842519576551, 0.3153832671262227771 ) ) ;
#402 = CARTESIAN_POINT ( 'NONE',  ( 1.614173228346456712, 2.401574803149606474, 0.5309055118110233007 ) ) ;
#403 = CARTESIAN_POINT ( 'NONE',  ( 0.1706036745406830368, 0.05413385826771666132, 0.4176697321401328100 ) ) ;
#404 = CARTESIAN_POINT ( 'NONE',  ( -0.1771653543307080136, -0.5400638737290844871, 0.3530559997133364547 ) ) ;
#405 = EDGE_CURVE ( 'NONE', #79849, #33739, #16525, .T. ) ;
#406 = CARTESIAN_POINT ( 'NONE',  ( -0.9120734908136475250, 0.2952755905511811885, 0.1292274648535926551 ) ) ;
#407 = CARTESIAN_POINT ( 'NONE',  ( 0.3392501089628018884, -0.1958661417322833942, -1.519048187172915343 ) ) ;
#408 = CARTESIAN_POINT ( 'NONE',  ( -1.338582677165353729, -0.1870078740157479769, 0.4822834645669291653 ) ) ;
#409 = CARTESIAN_POINT ( 'NONE',  ( 0.01224130022169934474, 1.075705580628688152, 0.2362204724409448231 ) ) ;
#410 = CARTESIAN_POINT ( 'NONE',  ( 1.056430446194226436, -0.5511811023622048555, -0.09757992244046775898 ) ) ;
#411 = AXIS2_PLACEMENT_3D ( 'NONE', #247, #37306, #45669 ) ;
#412 = CARTESIAN_POINT ( 'NONE',  ( 0.4068241469816281097, 0.05413385826771666132, 0.4176697321401328100 ) ) ;
#413 = CARTESIAN_POINT ( 'NONE',  ( 0.8858267716535438430, 0.1660481256975885056, 0.3530559997133364547 ) ) ;
#414 = CARTESIAN_POINT ( 'NONE',  ( -0.1070741851644056997, 0.3996062992125986035, -1.266404199475065440 ) ) ;
#415 = CARTESIAN_POINT ( 'NONE',  ( -1.568241469816272105, -0.05778040916215522460, 0.4822834645669289988 ) ) ;
#416 = CARTESIAN_POINT ( 'NONE',  ( 0.1998031496062994128, -0.3460692066303957537, -0.6410761154855643129 ) ) ;
#417 = CARTESIAN_POINT ( 'NONE',  ( -0.3460692066303957537, -0.1998031496062994405, -0.2867454068241469534 ) ) ;
#418 = CARTESIAN_POINT ( 'NONE',  ( -0.01312335958005186876, -0.4281496062992124485, 0.4176697321401328655 ) ) ;
#419 = CARTESIAN_POINT ( 'NONE',  ( -0.3460692066303960868, 0.1998031496062990242, -2.860892388451443669 ) ) ;
#420 = CARTESIAN_POINT ( 'NONE',  ( 0.2867679344610365999, 0.2867679344610365999, -2.269685039370078705 ) ) ;
#421 = CARTESIAN_POINT ( 'NONE',  ( -1.371391076115484609, -0.5511811023622046335, 0.09757992244046803654 ) ) ;
#422 = CARTESIAN_POINT ( 'NONE',  ( 1.246719160104987623, -0.4281496062992124485, 0.4176697321401328655 ) ) ;
#423 = CARTESIAN_POINT ( 'NONE',  ( 1.174540682414699111, -0.3162353388693405765, 0.4822834645669290543 ) ) ;
#424 = CARTESIAN_POINT ( 'NONE',  ( 0.1049868766404206816, 0.1283753931104748280, 0.1820866141732283561 ) ) ;
#425 = CARTESIAN_POINT ( 'NONE',  ( 0.5708661417322841158, -0.5400638737290845981, -0.3530559997133363437 ) ) ;
#426 = CARTESIAN_POINT ( 'NONE',  ( -0.4724409448818898682, -8.678599364036362592E-17, -1.375984251968503713 ) ) ;
#427 = CARTESIAN_POINT ( 'NONE',  ( 0.5314960629921267055, -0.4536011799217367080, 0.2665933059059888421 ) ) ;
#428 = CARTESIAN_POINT ( 'NONE',  ( -0.1246719160104980823, 0.2952755905511811885, 0.1292274648535926551 ) ) ;
#429 = VECTOR ( 'NONE', #73458, 39.37007874015748143 ) ;
#430 = CARTESIAN_POINT ( 'NONE',  ( 0.1058382717557500852, -0.3949938075777408852, -1.264435695538058013 ) ) ;
#431 = CARTESIAN_POINT ( 'NONE',  ( -1.122047244094487306, -0.5400638737290844871, 0.3530559997133364547 ) ) ;
#432 = CARTESIAN_POINT ( 'NONE',  ( 0.5971128608923890191, -0.5511811023622046335, 0.09757992244046803654 ) ) ;
#433 = CARTESIAN_POINT ( 'NONE',  ( 0.4606732211678742361, 1.778019097314512686, 0.5309055118110234117 ) ) ;
#434 = CARTESIAN_POINT ( 'NONE',  ( -0.6299212598425188991, -0.1870078740157479769, 0.4822834645669291653 ) ) ;
#435 = CARTESIAN_POINT ( 'NONE',  ( -0.1640419947506553400, -0.08942795157528024563, -0.3641732283464568787 ) ) ;
#436 = DIRECTION ( 'NONE',  ( 0.000000000000000000, 1.000000000000000000, 0.000000000000000000 ) ) ;
#437 = CARTESIAN_POINT ( 'NONE',  ( -0.2952755905511804668, 0.1660481256975885056, 0.3530559997133364547 ) ) ;
#438 = CARTESIAN_POINT ( 'NONE',  ( -0.4002624671916004129, -0.3162353388693405765, 0.4822834645669290543 ) ) ;
#439 = CARTESIAN_POINT ( 'NONE',  ( 0.4593175853018379162, -0.3690944881889763329, 0.3153832671262228327 ) ) ;
#440 = CARTESIAN_POINT ( 'NONE',  ( 0.1070741851644053388, 0.3996062992125986035, -2.274934383202099397 ) ) ;
#441 = CARTESIAN_POINT ( 'NONE',  ( -0.1312335958005241554, -0.6046776061558809534, -0.2411417322834644161 ) ) ;
#442 = CARTESIAN_POINT ( 'NONE',  ( 0.2867679344610365999, 0.2867679344610365999, -1.477670972932071614 ) ) ;
#443 = CARTESIAN_POINT ( 'NONE',  ( 0.8661417322834653598, -0.1870078740157479769, 0.3641732283464567677 ) ) ;
#444 = CARTESIAN_POINT ( 'NONE',  ( 1.266404199475066328, -0.05778040916215522460, 0.4822834645669289988 ) ) ;
#445 = CARTESIAN_POINT ( 'NONE',  ( -0.9842519685039365918, -0.5511811023622047445, 6.969142054262312111E-17 ) ) ;
#446 = CARTESIAN_POINT ( 'NONE',  ( -0.7283464566929126471, 0.07958543189024071263, -0.2665933059059888421 ) ) ;
#447 = CARTESIAN_POINT ( 'NONE',  ( -0.8727034120734901146, -0.3162353388693405765, 0.4822834645669290543 ) ) ;
#448 = CARTESIAN_POINT ( 'NONE',  ( -0.2362204724409442680, -0.1870078740157480879, -0.4822834645669291653 ) ) ;
#449 = CARTESIAN_POINT ( 'NONE',  ( 0.3871391076115493490, -0.2845877964562159024, 0.3641732283464567677 ) ) ;
#450 = CARTESIAN_POINT ( 'NONE',  ( 0.1265901696524989184, 0.4724409448818898127, -2.355643044619422533 ) ) ;
#451 = CARTESIAN_POINT ( 'NONE',  ( 1.233595800524935227, -0.5023911411419708095, 0.1820866141732285504 ) ) ;
#452 = CARTESIAN_POINT ( 'NONE',  ( 0.5971128608923891301, 0.2952755905511810774, -0.1292274648535930714 ) ) ;
#453 = CARTESIAN_POINT ( 'NONE',  ( 0.2925321140481932369, -0.2925321140481931814, -0.01771653543307087630 ) ) ;
#454 = CARTESIAN_POINT ( 'NONE',  ( -0.2362204724409442680, -0.1870078740157480879, -0.4822834645669291653 ) ) ;
#455 = CARTESIAN_POINT ( 'NONE',  ( 0.1049643490035304938, -0.3917322834645669549, -1.272309711286089273 ) ) ;
#456 = CARTESIAN_POINT ( 'NONE',  ( 1.364829396325459854, -0.5023911411419708095, -0.1820866141732282451 ) ) ;
#457 = CARTESIAN_POINT ( 'NONE',  ( 0.4986876640419954376, -0.6046776061558809534, -0.2411417322834644161 ) ) ;
#458 = CARTESIAN_POINT ( 'NONE',  ( 0.1181102362204730916, 0.2952755905511811885, 0.000000000000000000 ) ) ;
#459 = CARTESIAN_POINT ( 'NONE',  ( 0.4359958488159310086, 1.724409448818897461, 3.912791665790203766 ) ) ;
#460 = CARTESIAN_POINT ( 'NONE',  ( 0.4986876640419954376, -0.5023911411419708095, -0.1820866141732282451 ) ) ;
#461 = CARTESIAN_POINT ( 'NONE',  ( 0.8858267716535438430, 0.1660481256975885056, 0.3530559997133364547 ) ) ;
#462 = CARTESIAN_POINT ( 'NONE',  ( -0.2427821522309703550, -0.08942795157528024563, -0.3641732283464568787 ) ) ;
#463 = CARTESIAN_POINT ( 'NONE',  ( -0.7217847769028863381, -0.4281496062992124485, 0.4176697321401328655 ) ) ;
#464 = CARTESIAN_POINT ( 'NONE',  ( -0.4724409448818898682, 5.785732909357575061E-17, -2.755905511811024056 ) ) ;
#465 = CARTESIAN_POINT ( 'NONE',  ( -0.2887139107611542133, 0.2306618581243848609, 0.2411417322834645549 ) ) ;
#466 = CARTESIAN_POINT ( 'NONE',  ( -1.200787401574802349, -0.5400638737290844871, 0.3530559997133364547 ) ) ;
#467 = CIRCLE ( 'NONE', #4492, 0.1181102362204724116 ) ;
#468 = CARTESIAN_POINT ( 'NONE',  ( -0.5052493438320203589, -0.5511811023622046335, 0.09757992244046803654 ) ) ;
#469 = CARTESIAN_POINT ( 'NONE',  ( 0.5643044619422579178, -0.4281496062992127816, -0.4176697321401328100 ) ) ;
#470 = CARTESIAN_POINT ( 'NONE',  ( -1.364829396325458521, 0.2306618581243847221, -0.2411417322834647770 ) ) ;
#471 = CARTESIAN_POINT ( 'NONE',  ( -0.5183727034120726440, 0.2952755905511811885, 0.1292274648535926551 ) ) ;
#472 = CARTESIAN_POINT ( 'NONE',  ( -0.6299212598425164567, 2.165354330708661568, -0.9285414500055735321 ) ) ;
#474 = CARTESIAN_POINT ( 'NONE',  ( 1.561679790026247350, -0.4281496062992124485, 0.4176697321401328655 ) ) ;
#473 = FACE_OUTER_BOUND ( 'NONE', #49663, .T. ) ;
#475 = CARTESIAN_POINT ( 'NONE',  ( 1.259842519685040019, -0.1870078740157480879, -0.4822834645669291653 ) ) ;
#476 = CARTESIAN_POINT ( 'NONE',  ( 0.1049643490035303689, 0.3917322834645670104, -2.505249343832020692 ) ) ;
#477 = CARTESIAN_POINT ( 'NONE',  ( -1.587926509186350810, 0.05413385826771626580, -0.4176697321401330321 ) ) ;
#478 = CARTESIAN_POINT ( 'NONE',  ( -1.351706036745406347, 0.05413385826771626580, -0.4176697321401330321 ) ) ;
#479 = CARTESIAN_POINT ( 'NONE',  ( -0.3458507752293909498, 0.3458507752293907833, -0.8070866141732284671 ) ) ;
#480 = CARTESIAN_POINT ( 'NONE',  ( -0.2925321140481930704, -0.2925321140481933480, 0.09842519685039367860 ) ) ;
#481 = ORIENTED_EDGE ( 'NONE', *, *, #70225, .T. ) ;
#482 = CARTESIAN_POINT ( 'NONE',  ( 0.1181102362204730916, 0.1771653543307087630, 0.000000000000000000 ) ) ;
#484 = CARTESIAN_POINT ( 'NONE',  ( -0.3917322834645671215, 0.1049643490035301469, -1.757217847769028340 ) ) ;
#483 = CIRCLE ( 'NONE', #78489, 0.3149606299212597271 ) ;
#485 = ORIENTED_EDGE ( 'NONE', *, *, #53883, .T. ) ;
#486 = CARTESIAN_POINT ( 'NONE',  ( 0.3674540682414705883, 0.2306618581243847221, -0.2411417322834647770 ) ) ;
#487 = CARTESIAN_POINT ( 'NONE',  ( 0.5577427821522314977, -0.3162353388693409650, -0.4822834645669289433 ) ) ;
#488 = CARTESIAN_POINT ( 'NONE',  ( -0.1265901696524986964, -0.4724409448818899238, -2.906824146981627610 ) ) ;
#489 = CARTESIAN_POINT ( 'NONE',  ( -1.595398199321657717, 0.4829664696085547715, 0.1559797534342468595 ) ) ;
#490 = CARTESIAN_POINT ( 'NONE',  ( -0.3215223097112853146, -0.08942795157528024563, -0.3641732283464568787 ) ) ;
#491 = DIRECTION ( 'NONE',  ( 0.000000000000000000, 0.000000000000000000, -1.000000000000000000 ) ) ;
#492 = CARTESIAN_POINT ( 'NONE',  ( 0.8333333333333340365, -0.6692913385826771977, 0.1292274648535927661 ) ) ;
#493 = CARTESIAN_POINT ( 'NONE',  ( 0.8858267716535438430, -0.4536011799217368745, -0.2665933059059886201 ) ) ;
#494 = CARTESIAN_POINT ( 'NONE',  ( -0.4002624671916004129, -0.3162353388693405765, 0.4822834645669290543 ) ) ;
#495 = CARTESIAN_POINT ( 'NONE',  ( -0.1958661417322834497, -0.3392501089628018884, -1.248012180281152794 ) ) ;
#496 = CARTESIAN_POINT ( 'NONE',  ( -0.9186351706036736120, -0.6046776061558809534, -0.2411417322834644161 ) ) ;
#497 = CARTESIAN_POINT ( 'NONE',  ( -1.135170603674539924, -0.5511811023622046335, 0.09757992244046803654 ) ) ;
#498 = ADVANCED_FACE ( 'NONE', ( #29570 ), #56283, .F. ) ;
#499 = CARTESIAN_POINT ( 'NONE',  ( -0.9055118110236215490, 0.2952755905511811885, 0.000000000000000000 ) ) ;
#500 =( BOUNDED_CURVE ( )  B_SPLINE_CURVE ( 3, ( #56843, #36672, #56026, #75410 ),
 .UNSPECIFIED., .F., .F. ) 
 B_SPLINE_CURVE_WITH_KNOTS ( ( 4, 4 ),
 ( 0.000000000000000000, 0.6251940424154354137 ),
 .UNSPECIFIED. ) 
 CURVE ( )  GEOMETRIC_REPRESENTATION_ITEM ( )  RATIONAL_B_SPLINE_CURVE ( ( 1.000000000000000000, 0.9676920770090842172, 0.9676920770090842172, 1.000000000000000000 ) ) 
 REPRESENTATION_ITEM ( '' )  );
#501 = CARTESIAN_POINT ( 'NONE',  ( 1.476377952755906442, -0.5400638737290844871, 0.3530559997133364547 ) ) ;
#502 = CARTESIAN_POINT ( 'NONE',  ( -0.4477342634306575864, 1.379855024864608204, -2.114057166015708589 ) ) ;
#503 = ORIENTED_EDGE ( 'NONE', *, *, #38239, .F. ) ;
#504 = CARTESIAN_POINT ( 'NONE',  ( 0.1958661417322834775, 0.3392501089628018884, -2.503300155676852157 ) ) ;
#505 = CARTESIAN_POINT ( 'NONE',  ( 0.03937007874015833325, -0.6692913385826771977, 8.415575281601705876E-17 ) ) ;
#506 = ORIENTED_EDGE ( 'NONE', *, *, #19297, .F. ) ;
#507 = CARTESIAN_POINT ( 'NONE',  ( -0.8136482939632537770, -0.6046776061558807314, 0.2411417322834647770 ) ) ;
#508 = CARTESIAN_POINT ( 'NONE',  ( 1.404199475065617264, -0.4281496062992124485, 0.4176697321401328655 ) ) ;
#509 = CARTESIAN_POINT ( 'NONE',  ( 1.069553805774278610, -0.6692913385826771977, 0.1292274648535927661 ) ) ;
#510 = CARTESIAN_POINT ( 'NONE',  ( 0.05905511811023681640, 0.1660481256975883668, -0.3530559997133364547 ) ) ;
#511 = EDGE_CURVE ( 'NONE', #3191, #62716, #18015, .T. ) ;
#512 = CARTESIAN_POINT ( 'NONE',  ( 0.05249343832021075018, -0.6046776061558807314, 0.2411417322834647770 ) ) ;
#513 = CARTESIAN_POINT ( 'NONE',  ( -0.1958661417322834220, -0.3392501089628018884, -1.725065616797900381 ) ) ;
#514 = CARTESIAN_POINT ( 'NONE',  ( -1.259842519685038686, -0.1870078740157479769, 0.4822834645669291653 ) ) ;
#515 = CARTESIAN_POINT ( 'NONE',  ( -0.1115485564304453947, -0.6692913385826771977, 0.1292274648535927661 ) ) ;
#516 = CARTESIAN_POINT ( 'NONE',  ( -0.2559055118110227234, -0.4536011799217367080, 0.2665933059059888421 ) ) ;
#517 = CARTESIAN_POINT ( 'NONE',  ( 1.660104986876641320, -0.05778040916215522460, 0.4822834645669289988 ) ) ;
#518 = CARTESIAN_POINT ( 'NONE',  ( 1.450131233595801428, -0.6692913385826773087, -0.1292274648535924053 ) ) ;
#519 = CARTESIAN_POINT ( 'NONE',  ( -0.6036745406824141069, 0.2306618581243848609, 0.2411417322834645549 ) ) ;
#520 = CARTESIAN_POINT ( 'NONE',  ( 0.2755905511811031494, 0.2066929133858268208, 0.000000000000000000 ) ) ;
#521 = CARTESIAN_POINT ( 'NONE',  ( 1.259842519685040019, -0.1870078740157479769, 0.4822834645669291653 ) ) ;
#522 = CARTESIAN_POINT ( 'NONE',  ( 0.5387615594602674918, 2.409604939980833412E-17, -0.3464511005275205946 ) ) ;
#523 = ORIENTED_EDGE ( 'NONE', *, *, #53975, .F. ) ;
#524 = ORIENTED_EDGE ( 'NONE', *, *, #54320, .F. ) ;
#525 = CARTESIAN_POINT ( 'NONE',  ( 0.1115485564304470323, 0.2952755905511811885, 0.1292274648535926551 ) ) ;
#526 = CARTESIAN_POINT ( 'NONE',  ( -0.3937007874015740483, -0.1870078740157480601, -0.3641732283464567677 ) ) ;
#528 = CARTESIAN_POINT ( 'NONE',  ( 0.000000000000000000, 0.000000000000000000, -0.3937007874015748254 ) ) ;
#527 = CARTESIAN_POINT ( 'NONE',  ( 1.417322834645670104, -0.1870078740157480601, -0.3641732283464567677 ) ) ;
#529 = CARTESIAN_POINT ( 'NONE',  ( 0.3458507752293908943, -0.3458507752293908943, -0.1751968503937007537 ) ) ;
#530 = CARTESIAN_POINT ( 'NONE',  ( 1.614173228346457378, -0.5511811023622047445, 6.969142054262312111E-17 ) ) ;
#531 = CARTESIAN_POINT ( 'NONE',  ( -1.443569553805773564, 0.2306618581243847221, -0.2411417322834647770 ) ) ;
#532 = CARTESIAN_POINT ( 'NONE',  ( 4.837279021331061486E-17, -0.3949938075777409963, -0.3129921259842520231 ) ) ;
#533 = CARTESIAN_POINT ( 'NONE',  ( -0.1181102362204717315, 0.2952755905511811885, 0.000000000000000000 ) ) ;
#534 = CARTESIAN_POINT ( 'NONE',  ( -1.555118110236219930, -0.5400638737290845981, -0.3530559997133363437 ) ) ;
#535 = AXIS2_PLACEMENT_3D ( 'NONE', #45483, #71180, #13522 ) ;
#536 = CARTESIAN_POINT ( 'NONE',  ( -1.371391076115484831, 0.2952755905511810774, -0.1292274648535930714 ) ) ;
#537 = CARTESIAN_POINT ( 'NONE',  ( 0.1837270341207354329, 0.2306618581243848609, 0.2411417322834645549 ) ) ;
#538 = CARTESIAN_POINT ( 'NONE',  ( 0.1058382717557500852, -0.3949938075777408852, -0.004593175853018378711 ) ) ;
#539 = CARTESIAN_POINT ( 'NONE',  ( -1.646981627296586703, -0.08942795157527998196, 0.3641732283464567121 ) ) ;
#540 = CARTESIAN_POINT ( 'NONE',  ( 0.3543307086614179147, 0.2952755905511811885, 0.000000000000000000 ) ) ;
#541 = CARTESIAN_POINT ( 'NONE',  ( 0.8923884514435703741, 0.1283753931104748280, 0.1820866141732283561 ) ) ;
#542 = CARTESIAN_POINT ( 'NONE',  ( -0.06561679790026180015, 0.05413385826771666132, 0.4176697321401328100 ) ) ;
#543 = CARTESIAN_POINT ( 'NONE',  ( 0.6889763779527566800, -0.4536011799217367080, 0.2665933059059888421 ) ) ;
#544 = CARTESIAN_POINT ( 'NONE',  ( -1.463254593175852492, 0.2952755905511811885, 0.1292274648535926551 ) ) ;
#545 = CARTESIAN_POINT ( 'NONE',  ( 4.893765752498283308E-17, -0.3996062992125985480, -0.7854330708661416693 ) ) ;
#546 = CARTESIAN_POINT ( 'NONE',  ( 1.194225721784777594, 0.05413385826771666132, 0.4176697321401328100 ) ) ;
#547 = CARTESIAN_POINT ( 'NONE',  ( -0.2867679344610365999, 0.2867679344610364889, -0.7992125984251968740 ) ) ;
#549 = CARTESIAN_POINT ( 'NONE',  ( 1.614173228346457378, 0.7794589730112001513, -0.1372047244094476148 ) ) ;
#548 = CARTESIAN_POINT ( 'NONE',  ( 0.9055118110236227702, 0.2952755905511811885, 0.000000000000000000 ) ) ;
#550 = LINE ( 'NONE', #1797, #42889 ) ;
#551 = CARTESIAN_POINT ( 'NONE',  ( 0.4002624671916016896, -0.2845877964562161244, -0.3641732283464567121 ) ) ;
#552 = AXIS2_PLACEMENT_3D ( 'NONE', #45585, #8559, #7302 ) ;
#553 = CARTESIAN_POINT ( 'NONE',  ( 0.5643044619422579178, 0.05413385826771666132, 0.4176697321401328100 ) ) ;
#554 = CARTESIAN_POINT ( 'NONE',  ( 0.7349081364829403995, 0.1539470093639523085, 0.1968503937007873850 ) ) ;
#555 = CARTESIAN_POINT ( 'NONE',  ( -0.9842519685039365918, -0.5511811023622047445, 6.969142054262312111E-17 ) ) ;
#556 = CARTESIAN_POINT ( 'NONE',  ( -1.174540682414697335, -0.3162353388693409650, -0.4822834645669289433 ) ) ;
#557 = CARTESIAN_POINT ( 'NONE',  ( 1.548556430446194954, 0.2306618581243847221, -0.2411417322834647770 ) ) ;
#558 = CARTESIAN_POINT ( 'NONE',  ( -1.220472440944881054, 0.2952755905511811885, 0.000000000000000000 ) ) ;
#559 = CARTESIAN_POINT ( 'NONE',  ( 0.7545931758530189937, 0.2952755905511810774, -0.1292274648535930714 ) ) ;
#560 = CARTESIAN_POINT ( 'NONE',  ( -1.305774278215222184, 0.1771653543307087630, 0.09757992244046791164 ) ) ;
#561 = LINE ( 'NONE', #45565, #71983 ) ;
#562 = CARTESIAN_POINT ( 'NONE',  ( 0.9317585301837276734, -0.4281496062992124485, 0.4176697321401328655 ) ) ;
#563 = CARTESIAN_POINT ( 'NONE',  ( 0.1265901696524989462, 0.4724409448818897572, -2.274934383202099397 ) ) ;
#564 = CARTESIAN_POINT ( 'NONE',  ( -0.08874907683609993547, 8.471767977567108961E-16, -0.4445507791589058955 ) ) ;
#565 = CARTESIAN_POINT ( 'NONE',  ( 1.207349081364829990, 0.2306618581243848609, 0.2411417322834645549 ) ) ;
#566 = CARTESIAN_POINT ( 'NONE',  ( -0.8989501312335946848, 0.1771653543307087075, -0.09757992244046823083 ) ) ;
#567 = CARTESIAN_POINT ( 'NONE',  ( 1.509186351706037543, -0.004921259842519576551, 0.3153832671262227771 ) ) ;
#568 = CARTESIAN_POINT ( 'NONE',  ( -1.430446194225720724, -0.004921259842519870586, -0.3153832671262229437 ) ) ;
#569 = CARTESIAN_POINT ( 'NONE',  ( -0.5118110236220466680, 0.1771653543307087630, 0.000000000000000000 ) ) ;
#570 = CARTESIAN_POINT ( 'NONE',  ( -1.601049868766403650, -0.5023911411419708095, 0.1820866141732285504 ) ) ;
#571 = CARTESIAN_POINT ( 'NONE',  ( 0.7611548556430451917, -0.5023911411419708095, 0.1820866141732285504 ) ) ;
#572 = CARTESIAN_POINT ( 'NONE',  ( 0.6955380577427828781, -0.4281496062992124485, 0.4176697321401328655 ) ) ;
#573 = CARTESIAN_POINT ( 'NONE',  ( 1.456692913385827515, 0.2952755905511811885, 0.000000000000000000 ) ) ;
#574 = CARTESIAN_POINT ( 'NONE',  ( 0.03280839895013198948, -0.6692913385826773087, -0.1292274648535924053 ) ) ;
#575 = CARTESIAN_POINT ( 'NONE',  ( 0.5971128608923890191, -0.5511811023622046335, 0.09757992244046803654 ) ) ;
#576 = CARTESIAN_POINT ( 'NONE',  ( 1.601049868766404982, 0.2306618581243848609, 0.2411417322834645549 ) ) ;
#577 = CARTESIAN_POINT ( 'NONE',  ( -1.364829396325458521, -0.6046776061558807314, 0.2411417322834647770 ) ) ;
#578 = CARTESIAN_POINT ( 'NONE',  ( -0.5971128608923877978, 0.2952755905511811885, 0.1292274648535926551 ) ) ;
#579 = CARTESIAN_POINT ( 'NONE',  ( 4.893765752498283924E-17, -0.3996062992125986035, -0.2362204724409449341 ) ) ;
#580 = CARTESIAN_POINT ( 'NONE',  ( -0.4724409448818898682, -8.678599364036362592E-17, -1.218503937007874072 ) ) ;
#581 = CARTESIAN_POINT ( 'NONE',  ( 0.1115485564304467270, -0.6692913385826773087, -0.1292274648535924053 ) ) ;
#582 = CARTESIAN_POINT ( 'NONE',  ( -0.2755905511811015396, -0.6692913385826771977, 8.415575281601705876E-17 ) ) ;
#583 = CARTESIAN_POINT ( 'NONE',  ( 0.1771653543307093182, 0.1660481256975885056, 0.3530559997133364547 ) ) ;
#584 = CARTESIAN_POINT ( 'NONE',  ( -0.1070741851644056997, 0.3996062992125986035, -2.526246719160104792 ) ) ;
#585 = CARTESIAN_POINT ( 'NONE',  ( -0.3949938075777409963, -7.255918531996591613E-17, -2.086614173228346303 ) ) ;
#586 = CARTESIAN_POINT ( 'NONE',  ( -9.594673741351313045E-17, 0.3917322834645670104, -0.6220472440944880832 ) ) ;
#587 = CARTESIAN_POINT ( 'NONE',  ( 0.2950900605411925781, -0.01202116872835604609, 5.525111687089955481 ) ) ;
#588 = VECTOR ( 'NONE', #6530, 39.37007874015748143 ) ;
#589 = CARTESIAN_POINT ( 'NONE',  ( -0.1958661417322834220, -0.3392501089628018884, -1.160104986876640210 ) ) ;
#590 = CARTESIAN_POINT ( 'NONE',  ( -0.8267716535433065062, -0.5511811023622047445, 6.969142054262312111E-17 ) ) ;
#591 = CARTESIAN_POINT ( 'NONE',  ( -0.1049643490035307020, 0.3917322834645669549, -1.258530183727033958 ) ) ;
#592 = CARTESIAN_POINT ( 'NONE',  ( -1.305774278215222184, -0.6692913385826773087, -0.1292274648535924053 ) ) ;
#593 = CARTESIAN_POINT ( 'NONE',  ( -0.3917322834645668994, -0.1049643490035306742, 0.03151537877396508314 ) ) ;
#594 = CARTESIAN_POINT ( 'NONE',  ( 0.5708661417322842269, 0.1660481256975885056, 0.3530559997133364547 ) ) ;
#595 = CARTESIAN_POINT ( 'NONE',  ( 0.03937007874015806264, 0.1771653543307087630, 0.000000000000000000 ) ) ;
#596 = CARTESIAN_POINT ( 'NONE',  ( 1.174540682414699111, -0.05778040916215560624, -0.4822834645669293319 ) ) ;
#597 = CARTESIAN_POINT ( 'NONE',  ( 0.5511811023622054106, -0.1870078740157480879, -0.4822834645669291653 ) ) ;
#598 = CARTESIAN_POINT ( 'NONE',  ( -0.4091458600556405756, 0.2362204724409446288, -2.860892388451443669 ) ) ;
#599 = CARTESIAN_POINT ( 'NONE',  ( 0.3460692066303959757, -0.1998031496062991907, -2.624671916010498762 ) ) ;
#600 = CARTESIAN_POINT ( 'NONE',  ( -0.3392501089628017219, -0.1958661417322836995, -1.151594118931445365 ) ) ;
#601 = CARTESIAN_POINT ( 'NONE',  ( 1.141732283464567788, -0.6692913385826771977, 8.415575281601705876E-17 ) ) ;
#602 = CARTESIAN_POINT ( 'NONE',  ( 0.5183727034120741983, 0.2952755905511810774, -0.1292274648535930714 ) ) ;
#603 = CARTESIAN_POINT ( 'NONE',  ( 0.3280839895013130669, 0.05413385826771666132, 0.4176697321401328100 ) ) ;
#604 = CARTESIAN_POINT ( 'NONE',  ( 0.9711286089238851948, 0.1283753931104748280, 0.1820866141732283561 ) ) ;
#605 = CARTESIAN_POINT ( 'NONE',  ( 1.115485564304462551, -0.4281496062992127816, -0.4176697321401328100 ) ) ;
#606 = CARTESIAN_POINT ( 'NONE',  ( 0.1049643490035303689, 0.3917322834645670104, -0.07808398950131241467 ) ) ;
#607 = CARTESIAN_POINT ( 'NONE',  ( 0.2296587926509192634, -0.05778040916215560624, -0.4822834645669293319 ) ) ;
#608 = CARTESIAN_POINT ( 'NONE',  ( 1.062992125984252745, 0.2952755905511811885, 0.000000000000000000 ) ) ;
#609 = CARTESIAN_POINT ( 'NONE',  ( 0.5446194225721792126, -0.3162353388693405765, 0.4822834645669290543 ) ) ;
#610 = CARTESIAN_POINT ( 'NONE',  ( 1.030183727034121421, -0.08942795157527998196, 0.3641732283464567121 ) ) ;
#611 = CARTESIAN_POINT ( 'NONE',  ( -1.017060367454067249, -0.3162353388693409650, -0.4822834645669289433 ) ) ;
#612 = CARTESIAN_POINT ( 'NONE',  ( -1.476377952755905110, -0.5400638737290845981, -0.3530559997133363437 ) ) ;
#613 = CARTESIAN_POINT ( 'NONE',  ( 1.082677165354331228, -0.5400638737290844871, 0.3530559997133364547 ) ) ;
#614 = CARTESIAN_POINT ( 'NONE',  ( -0.05870088567476314939, -0.3874523867754370854, -1.929133858267717549 ) ) ;
#615 = CARTESIAN_POINT ( 'NONE',  ( -0.1958661417322834220, -0.3392501089628018884, -1.790026246719160330 ) ) ;
#616 = CARTESIAN_POINT ( 'NONE',  ( 0.3392501089628018329, 0.1958661417322835607, -2.800524934383201714 ) ) ;
#617 = ORIENTED_EDGE ( 'NONE', *, *, #783, .T. ) ;
#618 = CARTESIAN_POINT ( 'NONE',  ( -0.3996062992125986035, -0.1070741851644056997, -0.2034120734908136385 ) ) ;
#619 = EDGE_LOOP ( 'NONE', ( #4517, #46542, #69561, #51297 ) ) ;
#620 = CARTESIAN_POINT ( 'NONE',  ( 1.404199475065617708, 0.05413385826771626580, -0.4176697321401330321 ) ) ;
#621 = CARTESIAN_POINT ( 'NONE',  ( 0.8333333333333340365, 0.1771653543307087075, -0.09757992244046823083 ) ) ;
#622 = CARTESIAN_POINT ( 'NONE',  ( 0.1265901696524989184, 0.4724409448818898127, -2.432414698162729483 ) ) ;
#623 = DIRECTION ( 'NONE',  ( 0.000000000000000000, 1.000000000000000000, 0.000000000000000000 ) ) ;
#624 = DIRECTION ( 'NONE',  ( -1.000000000000000000, -3.050063254464715781E-16, 0.000000000000000000 ) ) ;
#625 = CARTESIAN_POINT ( 'NONE',  ( 0.3392501089628018884, -0.1958661417322834220, -0.8195538057742782767 ) ) ;
#626 = CARTESIAN_POINT ( 'NONE',  ( -1.056430446194224881, -0.5511811023622046335, 0.09757992244046803654 ) ) ;
#627 = CARTESIAN_POINT ( 'NONE',  ( -1.686351706036744558, 0.1771653543307087075, -0.09757992244046823083 ) ) ;
#628 = CARTESIAN_POINT ( 'NONE',  ( -1.607611548556429737, 0.2952755905511810774, -0.1292274648535930714 ) ) ;
#629 = CARTESIAN_POINT ( 'NONE',  ( -0.1377952755905504645, 0.1660481256975885056, 0.3530559997133364547 ) ) ;
#630 = CARTESIAN_POINT ( 'NONE',  ( 1.496062992125984703, -0.1870078740157480879, -0.4822834645669291653 ) ) ;
#631 = ORIENTED_EDGE ( 'NONE', *, *, #1460, .F. ) ;
#632 = EDGE_CURVE ( 'NONE', #39221, #82812, #83215, .T. ) ;
#633 = DIRECTION ( 'NONE',  ( -1.000000000000000000, 1.445602896647338917E-16, -0.000000000000000000 ) ) ;
#634 =( LENGTH_UNIT ( ) NAMED_UNIT ( * ) SI_UNIT ( $, .METRE. ) );
#635 = CARTESIAN_POINT ( 'NONE',  ( 0.1273213304869930951, 0.1377952755905511861, -1.680969278250197707 ) ) ;
#636 = CARTESIAN_POINT ( 'NONE',  ( -0.3503937007874015630, -0.5120078740157480990, 0.000000000000000000 ) ) ;
#637 = CARTESIAN_POINT ( 'NONE',  ( -1.049868766404198794, -0.5023911411419708095, 0.1820866141732285504 ) ) ;
#638 = CARTESIAN_POINT ( 'NONE',  ( -1.443569553805773564, 0.2306618581243847221, -0.2411417322834647770 ) ) ;
#639 = CARTESIAN_POINT ( 'NONE',  ( 0.4724409448818904789, -0.1870078740157480879, -0.4822834645669291653 ) ) ;
#640 = ORIENTED_EDGE ( 'NONE', *, *, #71767, .F. ) ;
#642 = FACE_OUTER_BOUND ( 'NONE', #22838, .T. ) ;
#641 = CARTESIAN_POINT ( 'NONE',  ( 0.000000000000000000, 2.677165354330708791, 0.000000000000000000 ) ) ;
#643 = CARTESIAN_POINT ( 'NONE',  ( 1.305774278215223960, -0.6692913385826771977, 0.1292274648535927661 ) ) ;
#644 = CARTESIAN_POINT ( 'NONE',  ( -1.620734908136482577, -0.6692913385826773087, -0.1292274648535924053 ) ) ;
#645 = CARTESIAN_POINT ( 'NONE',  ( 0.1958661417322836162, -0.3392501089628018329, -0.8018179545593683288 ) ) ;
#646 = CARTESIAN_POINT ( 'NONE',  ( -0.4330708661417315697, 0.1771653543307087630, 0.000000000000000000 ) ) ;
#647 = CARTESIAN_POINT ( 'NONE',  ( -1.463254593175852492, 0.1771653543307087630, 0.09757992244046791164 ) ) ;
#648 = CARTESIAN_POINT ( 'NONE',  ( 0.4091458600556403535, 0.2362204724409449896, -0.7611548556430446366 ) ) ;
#649 =( GEOMETRIC_REPRESENTATION_CONTEXT ( 3 ) GLOBAL_UNCERTAINTY_ASSIGNED_CONTEXT ( ( #13385 ) ) GLOBAL_UNIT_ASSIGNED_CONTEXT ( ( #28477, #67211, #3642 ) ) REPRESENTATION_CONTEXT ( 'NONE', 'WORKASPACE' ) );
#650 = CARTESIAN_POINT ( 'NONE',  ( -0.3674540682414689785, 0.1283753931104748280, 0.1820866141732283561 ) ) ;
#651 = CARTESIAN_POINT ( 'NONE',  ( 0.1574803149606306130, -0.1870078740157479769, 0.3641732283464567677 ) ) ;
#652 = CARTESIAN_POINT ( 'NONE',  ( 0.2493438320209980519, -0.4281496062992127816, -0.4176697321401328100 ) ) ;
#653 = CARTESIAN_POINT ( 'NONE',  ( -1.194225721784776262, -0.3690944881889763329, 0.3153832671262228327 ) ) ;
#654 = CARTESIAN_POINT ( 'NONE',  ( 0.1049643490035303689, 0.3917322834645670104, -2.662729658792650778 ) ) ;
#655 = CARTESIAN_POINT ( 'NONE',  ( 0.6824146981627303710, 0.2306618581243847221, -0.2411417322834647770 ) ) ;
#656 = ADVANCED_FACE ( 'NONE', ( #5775 ), #70162, .T. ) ;
#657 = CARTESIAN_POINT ( 'NONE',  ( -1.286089238845143479, 0.2306618581243847221, -0.2411417322834647770 ) ) ;
#658 = CARTESIAN_POINT ( 'NONE',  ( -0.2362204724409447953, -0.4091458600556404646, -1.087270341207349000 ) ) ;
#659 = CARTESIAN_POINT ( 'NONE',  ( -0.3280839895013117347, -0.4281496062992124485, 0.4176697321401328655 ) ) ;
#660 = CARTESIAN_POINT ( 'NONE',  ( 0.1115485564304467270, -0.5511811023622048555, -0.09757992244046775898 ) ) ;
#661 = CARTESIAN_POINT ( 'NONE',  ( -0.9711286089238838626, 0.2306618581243847221, -0.2411417322834647770 ) ) ;
#662 = CARTESIAN_POINT ( 'NONE',  ( 0.8136482939632553313, -0.5023911411419708095, -0.1820866141732282451 ) ) ;
#663 = AXIS2_PLACEMENT_3D ( 'NONE', #18331, #57428, #5275 ) ;
#664 = CARTESIAN_POINT ( 'NONE',  ( -0.3412073490813641308, -0.5023911411419708095, 0.1820866141732285504 ) ) ;
#665 = CARTESIAN_POINT ( 'NONE',  ( -0.4790026246719154557, -0.3162353388693405765, 0.4822834645669290543 ) ) ;
#666 = CARTESIAN_POINT ( 'NONE',  ( -1.384514435695537005, -0.6692913385826773087, -0.1292274648535924053 ) ) ;
#667 = CARTESIAN_POINT ( 'NONE',  ( -0.4043999638110875594, 5.961526036605507449E-15, -0.4118484887281962381 ) ) ;
#668 = CARTESIAN_POINT ( 'NONE',  ( 1.305774278215223960, -0.5511811023622046335, 0.09757992244046803654 ) ) ;
#669 = CARTESIAN_POINT ( 'NONE',  ( -1.594488188976377119, 0.1660481256975883668, -0.3530559997133364547 ) ) ;
#670 = CARTESIAN_POINT ( 'NONE',  ( -1.417322834645668772, -0.1870078740157479769, 0.4822834645669291653 ) ) ;
#671 = ORIENTED_EDGE ( 'NONE', *, *, #74772, .T. ) ;
#672 = EDGE_CURVE ( 'NONE', #11621, #29401, #37361, .T. ) ;
#673 = CARTESIAN_POINT ( 'NONE',  ( -0.1998031496062991630, -0.3460692066303959202, -2.504593175853018661 ) ) ;
#674 = CARTESIAN_POINT ( 'NONE',  ( -0.7874015748031489847, -0.1870078740157480601, -0.3641732283464567677 ) ) ;
#675 = CARTESIAN_POINT ( 'NONE',  ( 0.6036745406824153282, -0.6046776061558807314, 0.2411417322834647770 ) ) ;
#676 = CARTESIAN_POINT ( 'NONE',  ( -0.9317585301837263412, -0.004921259842519576551, 0.3153832671262227771 ) ) ;
#677 = CARTESIAN_POINT ( 'NONE',  ( 0.3996062992125985480, 2.446882876249141654E-17, -1.769685039370078927 ) ) ;
#678 = CARTESIAN_POINT ( 'NONE',  ( -0.8530183727034112984, -0.4281496062992127816, -0.4176697321401328100 ) ) ;
#679 = CARTESIAN_POINT ( 'NONE',  ( 0.9842519685039378130, -0.6692913385826771977, 8.415575281601705876E-17 ) ) ;
#680 = CARTESIAN_POINT ( 'NONE',  ( 0.3937007874015754361, -0.1870078740157479769, 0.4822834645669291653 ) ) ;
#681 = CARTESIAN_POINT ( 'NONE',  ( -1.351706036745406347, -0.004921259842519870586, -0.3153832671262229437 ) ) ;
#682 = CARTESIAN_POINT ( 'NONE',  ( 0.3996062992125984925, 0.1070741851644054499, -1.146325459317585116 ) ) ;
#683 = CARTESIAN_POINT ( 'NONE',  ( -0.3460692066303958092, -0.1998031496062994683, -1.469816272965879245 ) ) ;
#684 = CARTESIAN_POINT ( 'NONE',  ( 0.3420746716998659953, 0.1974969037888705536, -0.6036745406824147731 ) ) ;
#685 = CARTESIAN_POINT ( 'NONE',  ( 0.4602852883866460076, 1.653403552777538366, 2.586150256253575197 ) ) ;
#686 = CARTESIAN_POINT ( 'NONE',  ( 0.8398950131233602345, -0.5023911411419708095, 0.1820866141732285504 ) ) ;
#687 = CARTESIAN_POINT ( 'NONE',  ( 0.4133858267716541968, -0.4536011799217368745, -0.2665933059059886201 ) ) ;
#688 = CARTESIAN_POINT ( 'NONE',  ( -0.04593175853018302557, -0.6692913385826773087, -0.1292274648535924053 ) ) ;
#689 = CARTESIAN_POINT ( 'NONE',  ( 1.482939632545932307, 0.05413385826771626580, -0.4176697321401330321 ) ) ;
#690 = CARTESIAN_POINT ( 'NONE',  ( -0.3949938075777411073, 0.1058382717557497660, -1.841863517060367661 ) ) ;
#691 = CARTESIAN_POINT ( 'NONE',  ( 0.5446194225721792126, -0.2845877964562159024, 0.3641732283464567677 ) ) ;
#692 = CARTESIAN_POINT ( 'NONE',  ( -0.9055118110236215490, -0.6692913385826771977, 8.415575281601705876E-17 ) ) ;
#693 = CARTESIAN_POINT ( 'NONE',  ( -1.043307086614172041, -0.5400638737290844871, 0.3530559997133364547 ) ) ;
#694 = CARTESIAN_POINT ( 'NONE',  ( 0.9908136482939640111, -0.6692913385826771977, 0.1292274648535927661 ) ) ;
#695 = CARTESIAN_POINT ( 'NONE',  ( 0.1265901696524989462, 0.4724409448818897572, -1.410761154855643129 ) ) ;
#696 = CARTESIAN_POINT ( 'NONE',  ( -0.7742782152230965886, 0.05413385826771666132, 0.4176697321401328100 ) ) ;
#697 = ORIENTED_EDGE ( 'NONE', *, *, #58155, .F. ) ;
#698 = ORIENTED_EDGE ( 'NONE', *, *, #49898, .F. ) ;
#699 = CARTESIAN_POINT ( 'NONE',  ( -1.095800524934382292, -0.05778040916215522460, 0.4822834645669289988 ) ) ;
#700 = CARTESIAN_POINT ( 'NONE',  ( -0.6692913385826764205, 0.2952755905511811885, 0.000000000000000000 ) ) ;
#702 = CARTESIAN_POINT ( 'NONE',  ( -0.9448818897637790704, -0.1870078740157480879, -0.4822834645669291653 ) ) ;
#701 = CARTESIAN_POINT ( 'NONE',  ( -0.8792650918635160906, -0.3690944881889763329, 0.3153832671262228327 ) ) ;
#703 = CARTESIAN_POINT ( 'NONE',  ( 0.2867679344610365999, -0.2867679344610365999, -2.068222154034434546 ) ) ;
#704 = CARTESIAN_POINT ( 'NONE',  ( 0.1323808228461570424, -0.2647380121165202049, 0.1574803149606299746 ) ) ;
#705 = CARTESIAN_POINT ( 'NONE',  ( 1.568241469816273659, -0.05778040916215560624, -0.4822834645669293319 ) ) ;
#706 = CARTESIAN_POINT ( 'NONE',  ( -1.128608923884513837, -0.6046776061558807314, 0.2411417322834647770 ) ) ;
#707 = CARTESIAN_POINT ( 'NONE',  ( 0.3412073490813655186, 0.2306618581243848609, 0.2411417322834645549 ) ) ;
#708 = CARTESIAN_POINT ( 'NONE',  ( -0.8398950131233585692, 0.2306618581243848609, 0.2411417322834645549 ) ) ;
#709 = CARTESIAN_POINT ( 'NONE',  ( 0.7939632545931766261, -0.05778040916215522460, 0.4822834645669289988 ) ) ;
#710 = CARTESIAN_POINT ( 'NONE',  ( 0.1958661417322836440, -0.3392501089628017219, -1.501312335958005173 ) ) ;
#711 = CARTESIAN_POINT ( 'NONE',  ( -0.8530183727034112984, -0.004921259842519576551, 0.3153832671262227771 ) ) ;
#712 = VERTEX_POINT ( 'NONE', #12515 ) ;
#713 = CARTESIAN_POINT ( 'NONE',  ( -0.3420746716998661618, 0.1974969037888702206, -1.758530183727034180 ) ) ;
#714 = ORIENTED_EDGE ( 'NONE', *, *, #48541, .F. ) ;
#715 = CARTESIAN_POINT ( 'NONE',  ( -1.640419947506561060, -0.3690944881889765550, -0.3153832671262227771 ) ) ;
#716 = CONICAL_SURFACE ( 'NONE', #24907, 0.1771653543307085410, 1.029744258676653645 ) ;
#717 = CARTESIAN_POINT ( 'NONE',  ( -1.036745406824146176, 0.05413385826771626580, -0.4176697321401330321 ) ) ;
#718 = CARTESIAN_POINT ( 'NONE',  ( -1.122047244094487306, 0.1660481256975883668, -0.3530559997133364547 ) ) ;
#719 = CARTESIAN_POINT ( 'NONE',  ( -0.3996062992125986035, -0.1070741851644056997, -0.3608923884514435576 ) ) ;
#720 = CARTESIAN_POINT ( 'NONE',  ( -1.286089238845143479, -0.6046776061558807314, 0.2411417322834647770 ) ) ;
#721 = CARTESIAN_POINT ( 'NONE',  ( -1.279527559055116948, -0.5400638737290844871, 0.3530559997133364547 ) ) ;
#722 = CARTESIAN_POINT ( 'NONE',  ( -1.594488188976377119, 0.1660481256975883668, -0.3530559997133364547 ) ) ;
#723 = CARTESIAN_POINT ( 'NONE',  ( 3.224202737261815166, 2.716535433070866645, 0.5314960629921260393 ) ) ;
#724 = CARTESIAN_POINT ( 'NONE',  ( -0.7426113562972000981, 2.362204724409448620, -0.5309055118110235227 ) ) ;
#725 = AXIS2_PLACEMENT_3D ( 'NONE', #34776, #73071, #41496 ) ;
#726 = CARTESIAN_POINT ( 'NONE',  ( 0.2952755905511819101, 0.07958543189024071263, -0.2665933059059888421 ) ) ;
#727 = CARTESIAN_POINT ( 'NONE',  ( -0.1938976377952756625, -0.1938976377952756625, 0.07874015748031495954 ) ) ;
#728 = CARTESIAN_POINT ( 'NONE',  ( -0.2867679344610364334, -0.2867679344610367109, -0.4586614173228347746 ) ) ;
#729 = CARTESIAN_POINT ( 'NONE',  ( -0.1574803149606292529, -0.1870078740157479769, 0.3641732283464567677 ) ) ;
#730 = CARTESIAN_POINT ( 'NONE',  ( -0.9776902887139098386, 0.2952755905511810774, -0.1292274648535930714 ) ) ;
#731 = CARTESIAN_POINT ( 'NONE',  ( 1.220472440944882386, -0.6692913385826771977, 8.415575281601705876E-17 ) ) ;
#732 = CARTESIAN_POINT ( 'NONE',  ( -0.3215223097112853146, -0.05778040916215560624, -0.4822834645669293319 ) ) ;
#733 = EDGE_CURVE ( 'NONE', #7205, #57884, #50385, .T. ) ;
#734 = EDGE_LOOP ( 'NONE', ( #77385, #67273, #78260, #71101 ) ) ;
#735 = EDGE_LOOP ( 'NONE', ( #48750, #68189, #51593, #70339 ) ) ;
#736 = CARTESIAN_POINT ( 'NONE',  ( -0.1070741851644051862, -0.3996062992125986590, -2.038713910761154491 ) ) ;
#737 = CARTESIAN_POINT ( 'NONE',  ( -0.7874015748031489847, -0.1870078740157480879, -0.4822834645669291653 ) ) ;
#738 = CARTESIAN_POINT ( 'NONE',  ( 1.246719160104987623, -0.4281496062992124485, 0.4176697321401328655 ) ) ;
#739 = FACE_BOUND ( 'NONE', #72764, .T. ) ;
#740 = CARTESIAN_POINT ( 'NONE',  ( -0.1265901696524993347, 0.4724409448818895907, -0.7939632545931758489 ) ) ;
#741 = CARTESIAN_POINT ( 'NONE',  ( -2.152447471807442891, 1.622068519643041551, 0.4668652553835654917 ) ) ;
#742 = CARTESIAN_POINT ( 'NONE',  ( -0.3392501089628019995, 0.1958661417322832277, -0.3333333333333333148 ) ) ;
#743 = DIRECTION ( 'NONE',  ( 0.000000000000000000, 0.000000000000000000, 1.000000000000000000 ) ) ;
#744 = CARTESIAN_POINT ( 'NONE',  ( -0.4461942257217840213, -0.6046776061558809534, -0.2411417322834644161 ) ) ;
#745 = CARTESIAN_POINT ( 'NONE',  ( -1.338582677165353729, -0.1870078740157479769, 0.3641732283464567677 ) ) ;
#746 = CARTESIAN_POINT ( 'NONE',  ( -0.7677165354330699465, 0.1660481256975885056, 0.3530559997133364547 ) ) ;
#747 = CARTESIAN_POINT ( 'NONE',  ( -0.1998031496062994405, 0.3460692066303957537, 0.2250656167979002420 ) ) ;
#749 = CARTESIAN_POINT ( 'NONE',  ( -0.3458507752293906723, -0.3458507752293910609, -1.080708661417322691 ) ) ;
#748 = CARTESIAN_POINT ( 'NONE',  ( -1.148293963254592542, -0.6692913385826773087, -0.1292274648535924053 ) ) ;
#750 = CARTESIAN_POINT ( 'NONE',  ( -1.049868766404198794, 0.2306618581243847221, -0.2411417322834647770 ) ) ;
#751 = CARTESIAN_POINT ( 'NONE',  ( -0.1968503937007867743, -0.6692913385826771977, 8.415575281601705876E-17 ) ) ;
#752 = CARTESIAN_POINT ( 'NONE',  ( -0.2891555358219909388, -0.2891555358219912164, -2.498031496062992574 ) ) ;
#753 = CARTESIAN_POINT ( 'NONE',  ( 0.9317585301837276734, -0.3690944881889763329, 0.3153832671262228327 ) ) ;
#754 = CARTESIAN_POINT ( 'NONE',  ( 1.141392835773559211, 1.299212598425196985, 0.9642274814428540841 ) ) ;
#755 = CARTESIAN_POINT ( 'NONE',  ( 0.6430446194225729606, -0.3690944881889765550, -0.3153832671262227771 ) ) ;
#756 = CARTESIAN_POINT ( 'NONE',  ( 1.397637795275591177, -0.4536011799217367080, 0.2665933059059888421 ) ) ;
#757 = CARTESIAN_POINT ( 'NONE',  ( 1.469816272965879911, 0.2306618581243847221, -0.2411417322834647770 ) ) ;
#758 = CARTESIAN_POINT ( 'NONE',  ( 0.2296587926509192634, -0.2845877964562159024, 0.3641732283464567677 ) ) ;
#759 = CARTESIAN_POINT ( 'NONE',  ( -0.2867679344610365999, 0.2867679344610364889, -1.586614173228346747 ) ) ;
#760 = CARTESIAN_POINT ( 'NONE',  ( -0.9908136482939626788, 0.2952755905511811885, 0.1292274648535926551 ) ) ;
#761 = CARTESIAN_POINT ( 'NONE',  ( 1.391076115485564868, -0.6046776061558807314, 0.2411417322834647770 ) ) ;
#762 = CARTESIAN_POINT ( 'NONE',  ( -0.4091458600556405756, 0.2362204724409446288, 0.2119422572178477626 ) ) ;
#763 = CARTESIAN_POINT ( 'NONE',  ( -0.5577427821522301654, -0.2845877964562159024, 0.3641732283464567677 ) ) ;
#764 = CARTESIAN_POINT ( 'NONE',  ( 1.614173228346456712, 2.401574803149606474, -0.1372047244094476703 ) ) ;
#765 = CARTESIAN_POINT ( 'NONE',  ( 0.4461942257217856311, 0.2306618581243847221, -0.2411417322834647770 ) ) ;
#766 = PLANE ( 'NONE',  #65364 ) ;
#767 = CARTESIAN_POINT ( 'NONE',  ( 1.082677165354331228, -0.4536011799217367080, 0.2665933059059888421 ) ) ;
#768 = CARTESIAN_POINT ( 'NONE',  ( -0.02624671916010428221, -0.5023911411419708095, 0.1820866141732285504 ) ) ;
#769 = CARTESIAN_POINT ( 'NONE',  ( -0.4461942257217840213, -0.6046776061558809534, -0.2411417322834644161 ) ) ;
#770 = CARTESIAN_POINT ( 'NONE',  ( -1.272965879265091305, -0.4281496062992124485, 0.4176697321401328655 ) ) ;
#771 = CARTESIAN_POINT ( 'NONE',  ( -0.7939632545931750718, -0.08942795157528024563, -0.3641732283464568787 ) ) ;
#772 = DIRECTION ( 'NONE',  ( 0.000000000000000000, 0.000000000000000000, 1.000000000000000000 ) ) ;
#773 = CARTESIAN_POINT ( 'NONE',  ( 0.7414698162729663755, 0.2952755905511811885, 0.1292274648535926551 ) ) ;
#774 = CARTESIAN_POINT ( 'NONE',  ( -0.7939632545931750718, -0.05778040916215560624, -0.4822834645669293319 ) ) ;
#775 = CARTESIAN_POINT ( 'NONE',  ( -0.1998031496062994405, 0.3460692066303957537, -1.034776902887139194 ) ) ;
#776 = CARTESIAN_POINT ( 'NONE',  ( 0.3917322834645670104, 2.398668435337828261E-17, -2.722440944881889369 ) ) ;
#777 = CARTESIAN_POINT ( 'NONE',  ( 0.3346456692913390985, 0.07958543189024085140, 0.2665933059059887866 ) ) ;
#778 = CARTESIAN_POINT ( 'NONE',  ( -0.8661417322834640276, -0.1870078740157479769, 0.4822834645669291653 ) ) ;
#779 = VECTOR ( 'NONE', #35095, 39.37007874015748143 ) ;
#780 = CARTESIAN_POINT ( 'NONE',  ( -1.272965879265091305, 0.05413385826771626580, -0.4176697321401330321 ) ) ;
#781 = CARTESIAN_POINT ( 'NONE',  ( -1.108923884514435132, -0.08942795157528024563, -0.3641732283464568787 ) ) ;
#782 = CARTESIAN_POINT ( 'NONE',  ( 1.646981627296588035, -0.3162353388693405765, 0.4822834645669290543 ) ) ;
#783 = EDGE_CURVE ( 'NONE', #80, #29401, #36528, .T. ) ;
#784 = CARTESIAN_POINT ( 'NONE',  ( -1.089238845144356427, -0.3690944881889765550, -0.3153832671262227771 ) ) ;
#785 = CARTESIAN_POINT ( 'NONE',  ( -1.541994750656167090, 0.1771653543307087630, 0.09757992244046791164 ) ) ;
#786 = CARTESIAN_POINT ( 'NONE',  ( 1.095800524934383846, -0.3162353388693405765, 0.4822834645669290543 ) ) ;
#787 = CARTESIAN_POINT ( 'NONE',  ( 0.01193304242178773455, 1.795490347638496118E-16, 0.3627985898453511826 ) ) ;
#788 = CARTESIAN_POINT ( 'NONE',  ( -0.1958661417322836995, 0.3392501089628017219, -2.372066559876327307 ) ) ;
#789 = ORIENTED_EDGE ( 'NONE', *, *, #46286, .F. ) ;
#790 = ADVANCED_FACE ( 'NONE', ( #76083 ), #69761, .F. ) ;
#791 = DIRECTION ( 'NONE',  ( 0.000000000000000000, 0.000000000000000000, -1.000000000000000000 ) ) ;
#792 = CARTESIAN_POINT ( 'NONE',  ( -1.620734908136482577, -0.6692913385826773087, -0.1292274648535924053 ) ) ;
#793 = CARTESIAN_POINT ( 'NONE',  ( -1.181102362204723644, -0.1870078740157480879, -0.4822834645669291653 ) ) ;
#794 = CARTESIAN_POINT ( 'NONE',  ( 1.181102362204724976, -0.1870078740157480879, -0.4822834645669291653 ) ) ;
#795 = CARTESIAN_POINT ( 'NONE',  ( -0.3392501089628019995, 0.1958661417322832277, -1.843175853018372834 ) ) ;
#796 = CARTESIAN_POINT ( 'NONE',  ( 1.692913385826772421, 0.1771653543307087630, 0.000000000000000000 ) ) ;
#797 = CARTESIAN_POINT ( 'NONE',  ( 0.4461942257217856311, 0.2306618581243847221, -0.2411417322834647770 ) ) ;
#798 = CARTESIAN_POINT ( 'NONE',  ( -0.04593175853018302557, 0.2952755905511811885, 0.1292274648535926551 ) ) ;
#799 = DIRECTION ( 'NONE',  ( -0.000000000000000000, -1.000000000000000000, -0.000000000000000000 ) ) ;
#800 = CARTESIAN_POINT ( 'NONE',  ( -0.3996062992125985480, -7.340648628747423112E-17, -2.635826771653543066 ) ) ;
#801 = CARTESIAN_POINT ( 'NONE',  ( 0.7874015748031503170, -0.1870078740157479769, 0.3641732283464567677 ) ) ;
#802 = CARTESIAN_POINT ( 'NONE',  ( -0.1070741851644056997, 0.3996062992125986035, -1.423884514435695525 ) ) ;
#803 = ORIENTED_EDGE ( 'NONE', *, *, #65634, .F. ) ;
#804 = CARTESIAN_POINT ( 'NONE',  ( 0.3917322834645670104, -0.1049643490035303411, -2.938320209973753538 ) ) ;
#805 = ORIENTED_EDGE ( 'NONE', *, *, #65450, .T. ) ;
#806 = CARTESIAN_POINT ( 'NONE',  ( 0.07217847769028949700, -0.05778040916215560624, -0.4822834645669293319 ) ) ;
#807 = CARTESIAN_POINT ( 'NONE',  ( 1.148293963254593653, 0.2952755905511810774, -0.1292274648535930714 ) ) ;
#808 = CARTESIAN_POINT ( 'NONE',  ( 0.6889763779527566800, -0.5400638737290844871, 0.3530559997133364547 ) ) ;
#809 = CARTESIAN_POINT ( 'NONE',  ( 1.082677165354331228, 0.1660481256975883668, -0.3530559997133364547 ) ) ;
#810 = CARTESIAN_POINT ( 'NONE',  ( 1.594488188976378673, 0.1660481256975885056, 0.3530559997133364547 ) ) ;
#811 = CARTESIAN_POINT ( 'NONE',  ( -0.6758530183727028406, 0.2952755905511811885, 0.1292274648535926551 ) ) ;
#812 = CARTESIAN_POINT ( 'NONE',  ( 0.08530183727034192087, -0.3162353388693409650, -0.4822834645669289433 ) ) ;
#813 = CARTESIAN_POINT ( 'NONE',  ( 1.574803149606299746, -0.1870078740157479769, 0.4822834645669291653 ) ) ;
#814 = CARTESIAN_POINT ( 'NONE',  ( 1.227034120734908917, -0.6692913385826771977, 0.1292274648535927661 ) ) ;
#815 = EDGE_CURVE ( 'NONE', #64851, #29791, #21395, .T. ) ;
#816 = CARTESIAN_POINT ( 'NONE',  ( 1.122047244094488860, -0.5400638737290845981, -0.3530559997133363437 ) ) ;
#817 = CARTESIAN_POINT ( 'NONE',  ( -0.1968503937007867743, -0.6692913385826771977, 8.415575281601705876E-17 ) ) ;
#818 = CARTESIAN_POINT ( 'NONE',  ( 0.1958661417322834775, 0.3392501089628018884, -0.2939632545931757934 ) ) ;
#819 = CARTESIAN_POINT ( 'NONE',  ( 0.6364829396325465405, -0.2845877964562161244, -0.3641732283464567121 ) ) ;
#820 = VERTEX_POINT ( 'NONE', #82802 ) ;
#821 = CARTESIAN_POINT ( 'NONE',  ( 0.2891555358219910499, 0.2891555358219910499, -0.7677165354330709457 ) ) ;
#822 = AXIS2_PLACEMENT_3D ( 'NONE', #34394, #67220, #78191 ) ;
#823 = ORIENTED_EDGE ( 'NONE', *, *, #81853, .F. ) ;
#824 = CARTESIAN_POINT ( 'NONE',  ( -0.4396325459317579898, 0.1771653543307087630, 0.09757992244046791164 ) ) ;
#825 = AXIS2_PLACEMENT_3D ( 'NONE', #7918, #52916, #78631 ) ;
#826 = VECTOR ( 'NONE', #11111, 39.37007874015748143 ) ;
#827 = CARTESIAN_POINT ( 'NONE',  ( 0.02624671916010564918, -0.6046776061558809534, -0.2411417322834644161 ) ) ;
#828 = CARTESIAN_POINT ( 'NONE',  ( 2.750540364621160361, 1.199841186584418518, -0.3336616047370271065 ) ) ;
#829 = CARTESIAN_POINT ( 'NONE',  ( -0.01968503937007793844, -0.5400638737290844871, 0.3530559997133364547 ) ) ;
#830 = CARTESIAN_POINT ( 'NONE',  ( -0.1181102362204717315, 0.2952755905511811885, 0.000000000000000000 ) ) ;
#831 = CARTESIAN_POINT ( 'NONE',  ( -0.8989501312335946848, 0.2952755905511810774, -0.1292274648535930714 ) ) ;
#832 = ADVANCED_FACE ( 'NONE', ( #63850 ), #17200, .F. ) ;
#833 = CARTESIAN_POINT ( 'NONE',  ( 1.194225721784777594, -0.004921259842519576551, 0.3153832671262227771 ) ) ;
#834 = CARTESIAN_POINT ( 'NONE',  ( -1.463254593175852492, 0.2952755905511811885, 0.1292274648535926551 ) ) ;
#835 = CARTESIAN_POINT ( 'NONE',  ( 1.948818897637795367, 0.000000000000000000, 5.701968306260621233 ) ) ;
#836 = CARTESIAN_POINT ( 'NONE',  ( 0.8858267716535438430, -0.4536011799217368745, -0.2665933059059886201 ) ) ;
#837 = CARTESIAN_POINT ( 'NONE',  ( 0.4921259842519691285, -0.5400638737290845981, -0.3530559997133363437 ) ) ;
#838 = CARTESIAN_POINT ( 'NONE',  ( 0.9317585301837276734, 0.05413385826771626580, -0.4176697321401330321 ) ) ;
#839 = CARTESIAN_POINT ( 'NONE',  ( 0.1998031496062994405, -0.3460692066303958092, -1.351706036745406792 ) ) ;
#840 = CARTESIAN_POINT ( 'NONE',  ( -1.587926509186350810, -0.4281496062992124485, 0.4176697321401328655 ) ) ;
#841 = CARTESIAN_POINT ( 'NONE',  ( 0.3996062992125986035, -0.1070741851644052972, -0.8182414698162727706 ) ) ;
#842 = CARTESIAN_POINT ( 'NONE',  ( -0.2925321140481930149, -0.2925321140481933480, 0.02165354330708658959 ) ) ;
#843 = CARTESIAN_POINT ( 'NONE',  ( 0.03280839895013198948, 0.2952755905511811885, 0.1292274648535926551 ) ) ;
#844 = CARTESIAN_POINT ( 'NONE',  ( 0.2925321140481932369, 0.2925321140481932369, -2.814960629921259727 ) ) ;
#845 = EDGE_CURVE ( 'NONE', #15186, #5577, #75262, .T. ) ;
#846 = CARTESIAN_POINT ( 'NONE',  ( -0.1958661417322836718, 0.3392501089628017219, -1.987532808398950079 ) ) ;
#847 = CARTESIAN_POINT ( 'NONE',  ( -1.122047244094487306, 0.07958543189024071263, -0.2665933059059888421 ) ) ;
#848 = CARTESIAN_POINT ( 'NONE',  ( 1.128608923884514947, 0.2306618581243848609, 0.2411417322834645549 ) ) ;
#849 = CARTESIAN_POINT ( 'NONE',  ( 1.240157480314961314, 0.1660481256975883668, -0.3530559997133364547 ) ) ;
#850 = CARTESIAN_POINT ( 'NONE',  ( -0.4265091863517051496, -0.5511811023622046335, 0.09757992244046803654 ) ) ;
#851 = CARTESIAN_POINT ( 'NONE',  ( 0.5905511811023629321, -0.6692913385826771977, 8.415575281601705876E-17 ) ) ;
#852 = CARTESIAN_POINT ( 'NONE',  ( 0.4724409448818898682, 2.892866454678787531E-17, -1.612204724409448842 ) ) ;
#853 = CARTESIAN_POINT ( 'NONE',  ( 0.2559055118110243332, 0.07958543189024085140, 0.2665933059059887866 ) ) ;
#854 = CARTESIAN_POINT ( 'NONE',  ( -0.1509186351706028884, -0.05778040916215522460, 0.4822834645669289988 ) ) ;
#855 = CARTESIAN_POINT ( 'NONE',  ( -0.2891555358219911054, 0.2891555358219909388, -1.513779527559055094 ) ) ;
#856 = CARTESIAN_POINT ( 'NONE',  ( -1.017060367454067249, -0.3162353388693409650, -0.4822834645669289433 ) ) ;
#857 = CARTESIAN_POINT ( 'NONE',  ( 0.5183727034120741983, 0.1771653543307087075, -0.09757992244046823083 ) ) ;
#858 = CARTESIAN_POINT ( 'NONE',  ( -0.5314960629921122726, 2.755905511811024056, -3.937007874015763687 ) ) ;
#859 = CARTESIAN_POINT ( 'NONE',  ( -0.8136482939632537770, -0.6046776061558807314, 0.2411417322834647770 ) ) ;
#860 = CARTESIAN_POINT ( 'NONE',  ( -0.3608923884514428360, 0.1771653543307087630, 0.09757992244046791164 ) ) ;
#861 = CARTESIAN_POINT ( 'NONE',  ( -1.363814626685861287, 0.1354692512615926214, 0.3875633260700430682 ) ) ;
#862 = CARTESIAN_POINT ( 'NONE',  ( -0.5774278215223089816, 0.2306618581243847221, -0.2411417322834647770 ) ) ;
#863 = CARTESIAN_POINT ( 'NONE',  ( -0.3149606299212590610, -0.1870078740157480879, -0.4822834645669291653 ) ) ;
#864 = CARTESIAN_POINT ( 'NONE',  ( 0.3674540682414705883, 0.1283753931104746893, -0.1820866141732285504 ) ) ;
#865 = CARTESIAN_POINT ( 'NONE',  ( 0.2925321140481932369, 0.2925321140481932369, -2.104330708661417582 ) ) ;
#866 = CARTESIAN_POINT ( 'NONE',  ( 0.08530183727034192087, -0.05778040916215522460, 0.4822834645669289988 ) ) ;
#867 = CARTESIAN_POINT ( 'NONE',  ( 0.1049643490035303689, 0.3917322834645668994, -1.963235277394014267 ) ) ;
#868 = CARTESIAN_POINT ( 'NONE',  ( -1.594488188976377563, -0.4536011799217367080, 0.2665933059059888421 ) ) ;
#869 = CARTESIAN_POINT ( 'NONE',  ( 0.6299212598425204535, -0.1870078740157480601, -0.3641732283464567677 ) ) ;
#870 = CARTESIAN_POINT ( 'NONE',  ( 1.568241469816273437, -0.3162353388693405765, 0.4822834645669290543 ) ) ;
#871 = CARTESIAN_POINT ( 'NONE',  ( -0.6233595800524928121, -0.08942795157527998196, 0.3641732283464567121 ) ) ;
#872 = CARTESIAN_POINT ( 'NONE',  ( -1.108923884514435132, -0.2845877964562159024, 0.3641732283464567677 ) ) ;
#873 = CARTESIAN_POINT ( 'NONE',  ( -0.5511811023622038563, -0.1870078740157479769, 0.4822834645669291653 ) ) ;
#874 = CARTESIAN_POINT ( 'NONE',  ( -0.2624671916010490880, 0.2306618581243847221, -0.2411417322834647770 ) ) ;
#875 = CARTESIAN_POINT ( 'NONE',  ( 0.5314960629921267055, -0.4536011799217367080, 0.2665933059059888421 ) ) ;
#876 = DIRECTION ( 'NONE',  ( -0.000000000000000000, -1.000000000000000000, 0.000000000000000000 ) ) ;
#877 = CARTESIAN_POINT ( 'NONE',  ( 1.082677165354331228, -0.4536011799217367080, 0.2665933059059888421 ) ) ;
#878 = CARTESIAN_POINT ( 'NONE',  ( 0.1246719160104994284, 0.2952755905511810774, -0.1292274648535930714 ) ) ;
#879 = CARTESIAN_POINT ( 'NONE',  ( 0.3460692066303959202, -0.1998031496062991630, -0.02427821522309711946 ) ) ;
#880 = CARTESIAN_POINT ( 'NONE',  ( -0.3805774278215216522, -0.4281496062992127816, -0.4176697321401328100 ) ) ;
#881 = AXIS2_PLACEMENT_3D ( 'NONE', #25875, #225, #37687 ) ;
#882 = CARTESIAN_POINT ( 'NONE',  ( -0.3392501089628017219, -0.1958661417322836718, -1.554461942257217899 ) ) ;
#883 = CARTESIAN_POINT ( 'NONE',  ( 1.358267716535433323, -0.4536011799217368745, -0.2665933059059886201 ) ) ;
#885 = CARTESIAN_POINT ( 'NONE',  ( 0.6299212598425204535, -0.1870078740157480879, -0.4822834645669291653 ) ) ;
#884 = AXIS2_PLACEMENT_3D ( 'NONE', #26992, #71617, #52655 ) ;
#886 = AXIS2_PLACEMENT_3D ( 'NONE', #7786, #38921, #40179 ) ;
#887 = CARTESIAN_POINT ( 'NONE',  ( 0.1640419947506569498, -0.3162353388693409650, -0.4822834645669289433 ) ) ;
#888 = CARTESIAN_POINT ( 'NONE',  ( 0.1377952755905518800, 0.07958543189024071263, -0.2665933059059888421 ) ) ;
#889 = CARTESIAN_POINT ( 'NONE',  ( 0.7086614173228353852, -0.1870078740157479769, 0.4822834645669291653 ) ) ;
#890 = EDGE_CURVE ( 'NONE', #78998, #7122, #78646, .T. ) ;
#891 = CARTESIAN_POINT ( 'NONE',  ( -0.4790026246719154557, -0.2845877964562159024, 0.3641732283464567677 ) ) ;
#892 = CARTESIAN_POINT ( 'NONE',  ( -0.6955380577427815458, 0.05413385826771666132, 0.4176697321401328100 ) ) ;
#893 = CARTESIAN_POINT ( 'NONE',  ( -0.4724409448818896462, -0.1265901696524993070, -2.565616797900262647 ) ) ;
#894 = CARTESIAN_POINT ( 'NONE',  ( -0.2099737532808391705, -0.6046776061558809534, -0.2411417322834644161 ) ) ;
#895 = VERTEX_POINT ( 'NONE', #75675 ) ;
#896 = CARTESIAN_POINT ( 'NONE',  ( -1.003937007874014853, 0.1660481256975885056, 0.3530559997133364547 ) ) ;
#897 = CARTESIAN_POINT ( 'NONE',  ( -0.5118110236220466680, -0.5511811023622047445, 6.969142054262312111E-17 ) ) ;
#898 = CARTESIAN_POINT ( 'NONE',  ( 0.09186351706036799403, -0.4281496062992127816, -0.4176697321401328100 ) ) ;
#899 = CARTESIAN_POINT ( 'NONE',  ( -1.102362204724408601, -0.1870078740157479769, 0.4822834645669291653 ) ) ;
#900 = CARTESIAN_POINT ( 'NONE',  ( -0.8267716535433065062, 0.2952755905511811885, 0.000000000000000000 ) ) ;
#901 = CARTESIAN_POINT ( 'NONE',  ( 0.4359958488159797474, 1.724409448818897905, -2.094141031014984833 ) ) ;
#903 = CARTESIAN_POINT ( 'NONE',  ( 1.056430446194226436, -0.6692913385826773087, -0.1292274648535924053 ) ) ;
#902 = CARTESIAN_POINT ( 'NONE',  ( 1.089238845144357759, 0.05413385826771626580, -0.4176697321401330321 ) ) ;
#904 = CARTESIAN_POINT ( 'NONE',  ( 1.325459317585302665, -0.4281496062992124485, 0.4176697321401328655 ) ) ;
#905 = CARTESIAN_POINT ( 'NONE',  ( 0.1049643490035303689, 0.3917322834645670104, -2.662729658792650778 ) ) ;
#907 = VECTOR ( 'NONE', #66466, 39.37007874015748143 ) ;
#906 = CARTESIAN_POINT ( 'NONE',  ( -1.555118110236219930, -0.5400638737290845981, -0.3530559997133363437 ) ) ;
#908 = CARTESIAN_POINT ( 'NONE',  ( -1.240157480314959759, 0.1660481256975885056, 0.3530559997133364547 ) ) ;
#909 = CARTESIAN_POINT ( 'NONE',  ( 0.3458507752293908943, -0.3458507752293908943, -0.5708661417322833387 ) ) ;
#910 = CARTESIAN_POINT ( 'NONE',  ( -0.1998031496062991907, -0.3460692066303959757, -0.06561679790026248016 ) ) ;
#911 = ORIENTED_EDGE ( 'NONE', *, *, #49585, .T. ) ;
#912 = CARTESIAN_POINT ( 'NONE',  ( 0.08530183727034192087, -0.08942795157527998196, 0.3641732283464567121 ) ) ;
#913 = CARTESIAN_POINT ( 'NONE',  ( -0.2867679344610364334, -0.2867679344610367109, -1.625984251968503491 ) ) ;
#914 = ORIENTED_EDGE ( 'NONE', *, *, #4017, .T. ) ;
#915 = CARTESIAN_POINT ( 'NONE',  ( 0.2427821522309716595, -0.3162353388693409650, -0.4822834645669289433 ) ) ;
#916 = CARTESIAN_POINT ( 'NONE',  ( 0.2755905511811031494, -0.6692913385826771977, 8.415575281601705876E-17 ) ) ;
#917 = CARTESIAN_POINT ( 'NONE',  ( -0.2362204724409447953, -0.4091458600556404646, -2.900262467191600635 ) ) ;
#918 = CARTESIAN_POINT ( 'NONE',  ( -0.5400834452262261998, -4.992347309556208597E-15, 0.3954985857520076920 ) ) ;
#919 = CARTESIAN_POINT ( 'NONE',  ( -0.9645669291338575535, 0.07958543189024071263, -0.2665933059059888421 ) ) ;
#920 = FACE_OUTER_BOUND ( 'NONE', #64636, .T. ) ;
#921 = CARTESIAN_POINT ( 'NONE',  ( 0.6561679790026253567, -0.6046776061558809534, -0.2411417322834644161 ) ) ;
#922 = CARTESIAN_POINT ( 'NONE',  ( 0.9645669291338588858, 0.07958543189024085140, 0.2665933059059887866 ) ) ;
#923 = CARTESIAN_POINT ( 'NONE',  ( -0.4068241469816264999, -0.4281496062992124485, 0.4176697321401328655 ) ) ;
#924 = CARTESIAN_POINT ( 'NONE',  ( 0.1049643490035303689, 0.3917322834645668994, -1.333314017551494368 ) ) ;
#925 = CARTESIAN_POINT ( 'NONE',  ( -0.9120734908136475250, -0.6692913385826773087, -0.1292274648535924053 ) ) ;
#926 = CARTESIAN_POINT ( 'NONE',  ( 1.968503937007874072, 0.000000000000000000, 5.701968306260621233 ) ) ;
#927 = CARTESIAN_POINT ( 'NONE',  ( 1.299212598425197429, -0.6692913385826771977, 8.415575281601705876E-17 ) ) ;
#928 = CARTESIAN_POINT ( 'NONE',  ( 1.594488188976378673, -0.4536011799217368745, -0.2665933059059886201 ) ) ;
#929 = ORIENTED_EDGE ( 'NONE', *, *, #10585, .T. ) ;
#930 = CARTESIAN_POINT ( 'NONE',  ( 0.1958661417322834775, 0.3392501089628018884, -2.345819840716222515 ) ) ;
#931 = CARTESIAN_POINT ( 'NONE',  ( 0.03280839895013198948, -0.6692913385826773087, -0.1292274648535924053 ) ) ;
#932 = EDGE_LOOP ( 'NONE', ( #23051, #15115, #31365, #8595 ) ) ;
#933 = CARTESIAN_POINT ( 'NONE',  ( -0.6955380577427815458, -0.4281496062992127816, -0.4176697321401328100 ) ) ;
#934 = CARTESIAN_POINT ( 'NONE',  ( 1.496062992125984703, -0.1870078740157480879, -0.4822834645669291653 ) ) ;
#935 = CARTESIAN_POINT ( 'NONE',  ( 1.423884514435696191, -0.05778040916215522460, 0.4822834645669289988 ) ) ;
#936 = CARTESIAN_POINT ( 'NONE',  ( 0.2755905511811031494, -0.6692913385826771977, 8.415575281601705876E-17 ) ) ;
#937 = CARTESIAN_POINT ( 'NONE',  ( -0.5774278215223089816, -0.6046776061558807314, 0.2411417322834647770 ) ) ;
#938 = CARTESIAN_POINT ( 'NONE',  ( 0.3917322834645670104, 2.398668435337828261E-17, -1.777559055118110409 ) ) ;
#939 = CARTESIAN_POINT ( 'NONE',  ( -1.062992125984250968, 0.2952755905511811885, 0.000000000000000000 ) ) ;
#940 = CARTESIAN_POINT ( 'NONE',  ( -0.1377952755905504645, -0.5400638737290845981, -0.3530559997133363437 ) ) ;
#941 = CARTESIAN_POINT ( 'NONE',  ( -0.2821522309711278487, -0.5511811023622048555, -0.09757992244046775898 ) ) ;
#942 = CARTESIAN_POINT ( 'NONE',  ( 1.568241469816273659, -0.05778040916215560624, -0.4822834645669293319 ) ) ;
#943 = CARTESIAN_POINT ( 'NONE',  ( 1.292650918635171564, -0.6692913385826773087, -0.1292274648535924053 ) ) ;
#944 = CARTESIAN_POINT ( 'NONE',  ( -0.4986876640419942164, -0.6046776061558807314, 0.2411417322834647770 ) ) ;
#945 = CARTESIAN_POINT ( 'NONE',  ( -0.5314960629921398061, 2.687614851728676424, 3.900966923095589234 ) ) ;
#946 = CONICAL_SURFACE ( 'NONE', #61424, 1.250000000000000000, 0.1221730476396033355 ) ;
#947 = CARTESIAN_POINT ( 'NONE',  ( 1.056430446194226436, -0.6692913385826773087, -0.1292274648535924053 ) ) ;
#948 = DIRECTION ( 'NONE',  ( -0.000000000000000000, -1.000000000000000000, -0.000000000000000000 ) ) ;
#949 = VERTEX_POINT ( 'NONE', #43649 ) ;
#950 = AXIS2_PLACEMENT_3D ( 'NONE', #7471, #12953, #25977 ) ;
#951 = CARTESIAN_POINT ( 'NONE',  ( 0.4855643044619430415, -0.4281496062992127816, -0.4176697321401328100 ) ) ;
#952 = CARTESIAN_POINT ( 'NONE',  ( -0.3346456692913377662, -0.4536011799217367080, 0.2665933059059888421 ) ) ;
#953 = VECTOR ( 'NONE', #10670, 39.37007874015748143 ) ;
#955 = CARTESIAN_POINT ( 'NONE',  ( -1.614173228346457378, 0.7794589730111965986, 0.1372047244094476981 ) ) ;
#954 = CARTESIAN_POINT ( 'NONE',  ( 1.338582677165355062, -0.1870078740157479769, 0.3641732283464567677 ) ) ;
#956 = CARTESIAN_POINT ( 'NONE',  ( -0.1265901696524986964, -0.4724409448818899238, -0.1489501312335958227 ) ) ;
#957 = CARTESIAN_POINT ( 'NONE',  ( 1.522309711286089939, 0.1283753931104748280, 0.1820866141732283561 ) ) ;
#958 = CARTESIAN_POINT ( 'NONE',  ( 1.108923884514436242, -0.05778040916215522460, 0.4822834645669289988 ) ) ;
#959 = CARTESIAN_POINT ( 'NONE',  ( -0.1058382717557497660, -0.3949938075777411073, 0.008530183727034110208 ) ) ;
#960 = PRODUCT_DEFINITION_SHAPE ( 'NONE', 'NONE',  #83329 ) ;
#961 = CARTESIAN_POINT ( 'NONE',  ( 0.1443569553805781891, -0.4281496062992124485, 0.4176697321401328655 ) ) ;
#962 = DIRECTION ( 'NONE',  ( 0.000000000000000000, 0.000000000000000000, -1.000000000000000000 ) ) ;
#963 = CARTESIAN_POINT ( 'NONE',  ( -1.502624671916009680, -0.05778040916215560624, -0.4822834645669293319 ) ) ;
#964 = CARTESIAN_POINT ( 'NONE',  ( -0.1640419947506555343, -0.3162353388693405765, 0.4822834645669290543 ) ) ;
#965 = CARTESIAN_POINT ( 'NONE',  ( 0.3420746716998660508, 0.1974969037888705814, -0.05052493438320211638 ) ) ;
#966 = CARTESIAN_POINT ( 'NONE',  ( -1.450131233595799651, 0.1771653543307087075, -0.09757992244046823083 ) ) ;
#967 = CARTESIAN_POINT ( 'NONE',  ( 0.6955380577427828781, 0.05413385826771626580, -0.4176697321401330321 ) ) ;
#968 = CARTESIAN_POINT ( 'NONE',  ( 0.8989501312335964611, 0.1771653543307087630, 0.09757992244046791164 ) ) ;
#969 = CARTESIAN_POINT ( 'NONE',  ( 0.1341536278048623965, 1.050682278017460725, 0.2827841492639507348 ) ) ;
#970 = CARTESIAN_POINT ( 'NONE',  ( 0.8727034120734913358, -0.08942795157527998196, 0.3641732283464567121 ) ) ;
#971 = CARTESIAN_POINT ( 'NONE',  ( -1.391076115485563314, -0.6046776061558809534, -0.2411417322834644161 ) ) ;
#972 = CARTESIAN_POINT ( 'NONE',  ( -0.3996062992125985480, -7.340648628747423112E-17, -1.061023622047243986 ) ) ;
#973 = CARTESIAN_POINT ( 'NONE',  ( 1.187664041994751285, -0.05778040916215522460, 0.4822834645669289988 ) ) ;
#974 = CARTESIAN_POINT ( 'NONE',  ( 0.1049643490035304938, -0.3917322834645669549, -0.7073490813648293241 ) ) ;
#976 = CARTESIAN_POINT ( 'NONE',  ( 0.8858267716535438430, 0.1660481256975885056, 0.3530559997133364547 ) ) ;
#975 = CARTESIAN_POINT ( 'NONE',  ( 0.7349081364829403995, 0.2306618581243848609, 0.2411417322834645549 ) ) ;
#977 = CARTESIAN_POINT ( 'NONE',  ( -0.3809280630633181675, 0.004960608223778821026, 0.3437734562760189072 ) ) ;
#978 = CARTESIAN_POINT ( 'NONE',  ( 0.4330708661417329575, -0.5511811023622047445, 6.969142054262312111E-17 ) ) ;
#979 = CARTESIAN_POINT ( 'NONE',  ( 0.4330708661417329575, 0.2952755905511811885, 0.000000000000000000 ) ) ;
#980 = CARTESIAN_POINT ( 'NONE',  ( -0.7939632545931754048, -0.2845877964562159024, 0.3641732283464567677 ) ) ;
#981 = CARTESIAN_POINT ( 'NONE',  ( -0.9120734908136475250, 0.2952755905511811885, 0.1292274648535926551 ) ) ;
#982 = CARTESIAN_POINT ( 'NONE',  ( -1.706036745406823485, 0.2306618581243848609, 0.2411417322834645549 ) ) ;
#983 = CARTESIAN_POINT ( 'NONE',  ( 0.8661417322834653598, -0.1870078740157479769, 0.4822834645669291653 ) ) ;
#984 = B_SPLINE_CURVE_WITH_KNOTS ( 'NONE', 3,
 ( #68449, #81500, #10385, #37680, #36449, #62954, #50304, #24225, #61714, #57026, #56618, #36863 ),
 .UNSPECIFIED., .F., .F.,
 ( 4, 2, 2, 2, 2, 4 ),
 ( 0.007992874908875213444, 0.009303755029337302043, 0.01061463514979939064, 0.01192551527026147924, 0.01258095533049252354, 0.01323639539072356784 ),
 .UNSPECIFIED. ) ;
#985 = CARTESIAN_POINT ( 'NONE',  ( -1.653543307086613234, -0.1870078740157479769, 0.3641732283464567677 ) ) ;
#986 = CARTESIAN_POINT ( 'NONE',  ( 1.019692277575655615, 1.459399361446979126, -0.4682193611689622892 ) ) ;
#987 = CARTESIAN_POINT ( 'NONE',  ( 1.108923884514436242, -0.05778040916215522460, 0.4822834645669289988 ) ) ;
#988 = CARTESIAN_POINT ( 'NONE',  ( -1.157146581871515012E-16, 0.4724409448818898682, -2.281496062992125928 ) ) ;
#989 = CARTESIAN_POINT ( 'NONE',  ( 0.4116877677584974138, 1.299622705822838453, 3.915462153828698888 ) ) ;
#990 = CARTESIAN_POINT ( 'NONE',  ( 1.502624671916010790, -0.05778040916215522460, 0.4822834645669289988 ) ) ;
#991 = CARTESIAN_POINT ( 'NONE',  ( -1.318897637795274802, -0.4536011799217368745, -0.2665933059059886201 ) ) ;
#992 = CARTESIAN_POINT ( 'NONE',  ( 1.122047244094488860, -0.4536011799217368745, -0.2665933059059886201 ) ) ;
#993 = CARTESIAN_POINT ( 'NONE',  ( -1.476377952755905110, 0.07958543189024085140, 0.2665933059059887866 ) ) ;
#994 = CARTESIAN_POINT ( 'NONE',  ( -0.5905511811023613777, -0.5511811023622047445, 6.969142054262312111E-17 ) ) ;
#995 = ADVANCED_FACE ( 'NONE', ( #71847 ), #78589, .F. ) ;
#996 = CARTESIAN_POINT ( 'NONE',  ( -1.686351706036744558, 0.1771653543307087075, -0.09757992244046823083 ) ) ;
#997 = CARTESIAN_POINT ( 'NONE',  ( 0.8595800524934390507, -0.08942795157528024563, -0.3641732283464568787 ) ) ;
#998 = CARTESIAN_POINT ( 'NONE',  ( 0.5118110236220480003, -0.6692913385826771977, 8.415575281601705876E-17 ) ) ;
#999 = CARTESIAN_POINT ( 'NONE',  ( 0.9973753280839902091, 0.2306618581243847221, -0.2411417322834647770 ) ) ;
#1000 = CARTESIAN_POINT ( 'NONE',  ( -0.07217847769028787330, -0.05778040916215522460, 0.4822834645669289988 ) ) ;
#1001 = CARTESIAN_POINT ( 'NONE',  ( 0.5052493438320215802, 0.1771653543307087630, 0.09757992244046791164 ) ) ;
#1002 = CARTESIAN_POINT ( 'NONE',  ( 1.076115485564305141, -0.6046776061558807314, 0.2411417322834647770 ) ) ;
#1003 = CARTESIAN_POINT ( 'NONE',  ( 0.4724409448818898682, 2.892866454678787531E-17, -0.4330708661417322913 ) ) ;
#1004 = CARTESIAN_POINT ( 'NONE',  ( -0.7152230971128602510, -0.05778040916215560624, -0.4822834645669293319 ) ) ;
#1005 = CIRCLE ( 'NONE', #37280, 0.2952755905511810774 ) ;
#1006 = CARTESIAN_POINT ( 'NONE',  ( 0.3996062992125986035, 2.446882876249141962E-17, -0.4330708661417322913 ) ) ;
#1007 = CARTESIAN_POINT ( 'NONE',  ( -0.2937696495028822574, 1.187747051217076910, 0.1083477314895111149 ) ) ;
#1008 = CARTESIAN_POINT ( 'NONE',  ( 0.2427821522309716595, -0.3162353388693409650, -0.4822834645669289433 ) ) ;
#1009 = CARTESIAN_POINT ( 'NONE',  ( -0.5380577427821514602, 0.05413385826771666132, 0.4176697321401328100 ) ) ;
#1010 = CARTESIAN_POINT ( 'NONE',  ( 0.09842519685039434474, -0.5400638737290845981, -0.3530559997133363437 ) ) ;
#1011 = CARTESIAN_POINT ( 'NONE',  ( -0.1070741851644051862, -0.3996062992125987146, -2.749343832020996636 ) ) ;
#1012 = CARTESIAN_POINT ( 'NONE',  ( -0.3420746716998659953, -0.1974969037888706647, -2.099737532808398921 ) ) ;
#1013 = CARTESIAN_POINT ( 'NONE',  ( -0.3392501089628017219, -0.1958661417322836718, -0.6745406824146981117 ) ) ;
#1014 = CARTESIAN_POINT ( 'NONE',  ( 0.2952755905511810774, 3.179810529374183920E-17, 5.879133660591329580 ) ) ;
#1015 = CARTESIAN_POINT ( 'NONE',  ( -0.1958661417322836718, 0.3392501089628017219, -0.9501312335958004285 ) ) ;
#1016 = CARTESIAN_POINT ( 'NONE',  ( -0.7939632545931754048, -0.2845877964562159024, 0.3641732283464567677 ) ) ;
#1017 = CARTESIAN_POINT ( 'NONE',  ( -0.1049643490035307020, 0.3917322834645669549, -1.101049868766403872 ) ) ;
#1018 = CARTESIAN_POINT ( 'NONE',  ( -1.351706036745406347, 0.05413385826771626580, -0.4176697321401330321 ) ) ;
#1019 = CARTESIAN_POINT ( 'NONE',  ( 4.797336870675655290E-17, -0.3917322834645669549, -0.001293020176166160412 ) ) ;
#1020 = CARTESIAN_POINT ( 'NONE',  ( 0.3018372703412079971, 0.05413385826771626580, -0.4176697321401330321 ) ) ;
#1021 = CARTESIAN_POINT ( 'NONE',  ( -0.4724409448818890911, -0.1870078740157479769, 0.3641732283464567677 ) ) ;
#1022 = CARTESIAN_POINT ( 'NONE',  ( 1.181102362204724976, -0.1870078740157480879, -0.4822834645669291653 ) ) ;
#1023 = CARTESIAN_POINT ( 'NONE',  ( 0.2165354330708668673, 0.1660481256975883668, -0.3530559997133364547 ) ) ;
#1024 = CARTESIAN_POINT ( 'NONE',  ( 4.821444151489972621E-16, 1.062992125984252745, 3.937007874015748143 ) ) ;
#1025 = CARTESIAN_POINT ( 'NONE',  ( -0.3996062992125986035, -0.1070741851644056997, -2.723097112860892288 ) ) ;
#1026 = CARTESIAN_POINT ( 'NONE',  ( 0.1958661417322834775, 0.3392501089628018884, -1.085977321031183163 ) ) ;
#1027 = CARTESIAN_POINT ( 'NONE',  ( 1.056430446194226658, 0.2952755905511811885, 0.1292274648535926551 ) ) ;
#1028 = CARTESIAN_POINT ( 'NONE',  ( 0.2952755905511816326, -0.5400638737290844871, 0.3530559997133364547 ) ) ;
#1029 = CARTESIAN_POINT ( 'NONE',  ( 0.3543307086614179147, 0.2952755905511811885, 0.000000000000000000 ) ) ;
#1030 = CARTESIAN_POINT ( 'NONE',  ( 1.351706036745407680, 0.05413385826771666132, 0.4176697321401328100 ) ) ;
#1031 = CARTESIAN_POINT ( 'NONE',  ( 0.3917322834645670104, -0.1049643490035303411, -0.5111548556430445256 ) ) ;
#1032 = CARTESIAN_POINT ( 'NONE',  ( -0.03937007874015669567, -0.6692913385826771977, 8.415575281601705876E-17 ) ) ;
#1033 = CARTESIAN_POINT ( 'NONE',  ( 1.102362204724410155, -0.1870078740157480879, -0.4822834645669291653 ) ) ;
#1034 = CARTESIAN_POINT ( 'NONE',  ( 0.2099737532808405305, -0.6046776061558807314, 0.2411417322834647770 ) ) ;
#1035 = CARTESIAN_POINT ( 'NONE',  ( 0.9776902887139113929, -0.5511811023622048555, -0.09757992244046775898 ) ) ;
#1036 = CARTESIAN_POINT ( 'NONE',  ( -1.102362204724408601, -0.1870078740157479769, 0.4822834645669291653 ) ) ;
#1037 = CARTESIAN_POINT ( 'NONE',  ( -1.443569553805773564, -0.6046776061558807314, 0.2411417322834647770 ) ) ;
#1038 = CARTESIAN_POINT ( 'NONE',  ( 0.7020997375328090762, -0.05778040916215560624, -0.4822834645669293319 ) ) ;
#1039 = CARTESIAN_POINT ( 'NONE',  ( -0.7402641841139964152, 2.388450810264987734, -0.4916013665244729491 ) ) ;
#1040 = CARTESIAN_POINT ( 'NONE',  ( -0.3917322834645669549, -0.1049643490035306603, -1.927821522309711044 ) ) ;
#1041 = ORIENTED_EDGE ( 'NONE', *, *, #25445, .F. ) ;
#1042 = CARTESIAN_POINT ( 'NONE',  ( 0.2925321140481932369, -0.2925321140481932369, -0.09842519685039373412 ) ) ;
#1043 = ORIENTED_EDGE ( 'NONE', *, *, #78852, .T. ) ;
#1044 = CARTESIAN_POINT ( 'NONE',  ( 1.384514435695538559, 0.2952755905511810774, -0.1292274648535930714 ) ) ;
#1045 = CARTESIAN_POINT ( 'NONE',  ( 1.128608923884514947, 0.1283753931104748280, 0.1820866141732283561 ) ) ;
#1046 = DIRECTION ( 'NONE',  ( 0.000000000000000000, -0.000000000000000000, 1.000000000000000000 ) ) ;
#1047 = DIRECTION ( 'NONE',  ( 1.492469013153037857E-17, -0.9925461516413219831, 0.1218693434051477398 ) ) ;
#1048 = FACE_OUTER_BOUND ( 'NONE', #12186, .T. ) ;
#1049 = CARTESIAN_POINT ( 'NONE',  ( 0.3917322834645670104, -0.1049643490035303411, -0.6686351706036747222 ) ) ;
#1050 = CARTESIAN_POINT ( 'NONE',  ( -1.312335958005248715, 0.1283753931104748280, 0.1820866141732283561 ) ) ;
#1051 = CARTESIAN_POINT ( 'NONE',  ( 1.561679790026247350, -0.4281496062992124485, 0.4176697321401328655 ) ) ;
#1052 = CARTESIAN_POINT ( 'NONE',  ( 0.4711392887345147162, 1.601500657493326152, -3.908721069869979026 ) ) ;
#1053 = CARTESIAN_POINT ( 'NONE',  ( -0.3674540682414692561, -0.6046776061558809534, -0.2411417322834644161 ) ) ;
#1054 = CARTESIAN_POINT ( 'NONE',  ( 1.056430446194226436, -0.6692913385826773087, -0.1292274648535924053 ) ) ;
#1055 = VERTEX_POINT ( 'NONE', #7876 ) ;
#1056 = CARTESIAN_POINT ( 'NONE',  ( -1.522309711286088607, 0.2306618581243847221, -0.2411417322834647770 ) ) ;
#1057 = CARTESIAN_POINT ( 'NONE',  ( -0.7190005367825885729, -1.283732188437465593E-15, -0.4281993546915544013 ) ) ;
#1058 = CARTESIAN_POINT ( 'NONE',  ( 3.523619145740909619, 3.916330350904249524, 9.906383945723261419 ) ) ;
#1059 = CARTESIAN_POINT ( 'NONE',  ( -0.3458507752293909498, 0.3458507752293908388, -2.696850393700787052 ) ) ;
#1060 = CYLINDRICAL_SURFACE ( 'NONE', #55948, 0.4724409448818898682 ) ;
#1061 = CARTESIAN_POINT ( 'NONE',  ( -0.8202099737532799750, 0.1771653543307087075, -0.09757992244046823083 ) ) ;
#1062 = CARTESIAN_POINT ( 'NONE',  ( -1.581364829396324945, -0.05778040916215560624, -0.4822834645669293319 ) ) ;
#1063 = CARTESIAN_POINT ( 'NONE',  ( 0.4133858267716541968, 0.1660481256975885056, 0.3530559997133364547 ) ) ;
#1064 = AXIS2_PLACEMENT_3D ( 'NONE', #67446, #9780, #68282 ) ;
#1065 = VERTEX_POINT ( 'NONE', #20078 ) ;
#1067 = CARTESIAN_POINT ( 'NONE',  ( -2.787279214012418738, 2.401574803149606474, 0.000000000000000000 ) ) ;
#1066 = CARTESIAN_POINT ( 'NONE',  ( -0.7461015469960392554, 2.206450217141186609, 0.5309055118110236338 ) ) ;
#1068 = CARTESIAN_POINT ( 'NONE',  ( 1.312335958005250269, -0.6046776061558807314, 0.2411417322834647770 ) ) ;
#1069 = CARTESIAN_POINT ( 'NONE',  ( -1.699475065616797398, 0.2952755905511811885, 0.1292274648535926551 ) ) ;
#1070 = CARTESIAN_POINT ( 'NONE',  ( 0.2867679344610365999, -0.2867679344610365999, -0.8083796343493945269 ) ) ;
#1071 = CARTESIAN_POINT ( 'NONE',  ( -0.9645669291338575535, -0.4536011799217367080, 0.2665933059059888421 ) ) ;
#1072 = CARTESIAN_POINT ( 'NONE',  ( -1.489501312335957062, -0.08942795157527998196, 0.3641732283464567121 ) ) ;
#1073 = CARTESIAN_POINT ( 'NONE',  ( -0.3676198365746922714, 0.1467283321115996353, -1.216801570222568740 ) ) ;
#1074 = CARTESIAN_POINT ( 'NONE',  ( 0.6036745406824153282, -0.6046776061558807314, 0.2411417322834647770 ) ) ;
#1075 = CARTESIAN_POINT ( 'NONE',  ( -0.8727034120734901146, -0.2845877964562159024, 0.3641732283464567677 ) ) ;
#1076 = CARTESIAN_POINT ( 'NONE',  ( 0.1115485564304467270, -0.5511811023622048555, -0.09757992244046775898 ) ) ;
#1077 = CARTESIAN_POINT ( 'NONE',  ( 0.2624671916010504757, -0.6046776061558809534, -0.2411417322834644161 ) ) ;
#1078 = CARTESIAN_POINT ( 'NONE',  ( -1.272965879265091305, -0.004921259842519870586, -0.3153832671262229437 ) ) ;
#1079 = CARTESIAN_POINT ( 'NONE',  ( -9.594673741351313045E-17, 0.3917322834645670659, -0.1542187908474559610 ) ) ;
#1080 = CARTESIAN_POINT ( 'NONE',  ( 0.7217847769028878924, -0.4281496062992127816, -0.4176697321401328100 ) ) ;
#1081 = ADVANCED_FACE ( 'NONE', ( #25538 ), #52041, .F. ) ;
#1082 = CARTESIAN_POINT ( 'NONE',  ( -1.456692913385826182, 0.2952755905511811885, 0.000000000000000000 ) ) ;
#1083 = CARTESIAN_POINT ( 'NONE',  ( 0.1265901696524989462, 0.4724409448818897572, -1.330052493438320216 ) ) ;
#1084 = CARTESIAN_POINT ( 'NONE',  ( -0.6167979002624665030, 0.05413385826771666132, 0.4176697321401328100 ) ) ;
#1085 = CARTESIAN_POINT ( 'NONE',  ( 0.01968503937007930540, 0.07958543189024085140, 0.2665933059059887866 ) ) ;
#1086 = CARTESIAN_POINT ( 'NONE',  ( -1.108923884514435132, -0.05778040916215560624, -0.4822834645669293319 ) ) ;
#1087 = CARTESIAN_POINT ( 'NONE',  ( 0.9055118110236227702, 0.1771653543307087630, 0.000000000000000000 ) ) ;
#1088 = CARTESIAN_POINT ( 'NONE',  ( -0.1771653543307080136, -0.4536011799217367080, 0.2665933059059888421 ) ) ;
#1089 = CARTESIAN_POINT ( 'NONE',  ( -0.6889763779527552368, -0.5400638737290845981, -0.3530559997133363437 ) ) ;
#1090 = CARTESIAN_POINT ( 'NONE',  ( -1.017060367454067249, -0.3162353388693409650, -0.4822834645669289433 ) ) ;
#1091 = CARTESIAN_POINT ( 'NONE',  ( 1.666666666666667185, 0.05413385826771666132, 0.4176697321401328100 ) ) ;
#1092 = FACE_OUTER_BOUND ( 'NONE', #21318, .T. ) ;
#1093 = CARTESIAN_POINT ( 'NONE',  ( 1.325459317585302665, -0.3690944881889763329, 0.3153832671262228327 ) ) ;
#1094 = CARTESIAN_POINT ( 'NONE',  ( 0.2427821522309719648, -0.05778040916215522460, 0.4822834645669289988 ) ) ;
#1095 = CARTESIAN_POINT ( 'NONE',  ( 0.000000000000000000, 2.755905511811024056, 0.000000000000000000 ) ) ;
#1096 = CARTESIAN_POINT ( 'NONE',  ( -1.673228346456691717, 0.1660481256975883668, -0.3530559997133364547 ) ) ;
#1097 = ORIENTED_EDGE ( 'NONE', *, *, #67975, .T. ) ;
#1098 = CARTESIAN_POINT ( 'NONE',  ( -0.3460692066303957537, -0.1998031496062994405, -2.333989501312335957 ) ) ;
#1099 = CARTESIAN_POINT ( 'NONE',  ( -0.9908136482939626788, 0.1771653543307087630, 0.09757992244046791164 ) ) ;
#1100 = CARTESIAN_POINT ( 'NONE',  ( 0.9055118110236227702, -0.6692913385826771977, 8.415575281601705876E-17 ) ) ;
#1101 = CARTESIAN_POINT ( 'NONE',  ( -1.154855643044618851, -0.5023911411419708095, -0.1820866141732282451 ) ) ;
#1102 = CARTESIAN_POINT ( 'NONE',  ( 0.2925321140481932369, 0.2925321140481932369, -1.631889763779527325 ) ) ;
#1103 = CARTESIAN_POINT ( 'NONE',  ( -0.9973753280839886548, -0.6046776061558809534, -0.2411417322834644161 ) ) ;
#1104 = CARTESIAN_POINT ( 'NONE',  ( 1.036745406824147731, 0.05413385826771666132, 0.4176697321401328100 ) ) ;
#1105 = CARTESIAN_POINT ( 'NONE',  ( 0.6167979002624679463, 0.05413385826771626580, -0.4176697321401330321 ) ) ;
#1106 = CARTESIAN_POINT ( 'NONE',  ( 1.240157480314961314, -0.5400638737290844871, 0.3530559997133364547 ) ) ;
#1107 = CARTESIAN_POINT ( 'NONE',  ( -1.496062992125983815, -0.1870078740157480601, -0.3641732283464567677 ) ) ;
#1108 = CARTESIAN_POINT ( 'NONE',  ( 0.3996062992125985480, 2.446882876249141654E-17, -1.139763779527559029 ) ) ;
#1109 = CARTESIAN_POINT ( 'NONE',  ( -0.3460692066303960868, 0.1998031496062990242, -1.443569553805774230 ) ) ;
#1110 = CARTESIAN_POINT ( 'NONE',  ( 0.1974969037888706369, -0.3420746716998659953, -0.7217847769028871152 ) ) ;
#1111 = DIRECTION ( 'NONE',  ( -1.000000000000000000, 1.445602896647338917E-16, -0.000000000000000000 ) ) ;
#1112 = CARTESIAN_POINT ( 'NONE',  ( 0.7939632545931766261, -0.2845877964562161244, -0.3641732283464567121 ) ) ;
#1113 = CARTESIAN_POINT ( 'NONE',  ( 0.3805774278215230400, -0.004921259842519870586, -0.3153832671262229437 ) ) ;
#1114 = CARTESIAN_POINT ( 'NONE',  ( 0.05905511811023681640, 0.1660481256975883668, -0.3530559997133364547 ) ) ;
#1115 = CARTESIAN_POINT ( 'NONE',  ( 1.108923884514436242, -0.05778040916215522460, 0.4822834645669289988 ) ) ;
#1116 = CARTESIAN_POINT ( 'NONE',  ( 0.3949938075777408852, 0.1058382717557500435, -1.933727034120735100 ) ) ;
#1117 = CARTESIAN_POINT ( 'NONE',  ( 0.2165354330708668673, -0.4536011799217367080, 0.2665933059059888421 ) ) ;
#1118 = CARTESIAN_POINT ( 'NONE',  ( -0.7742782152230962556, -0.4281496062992127816, -0.4176697321401328100 ) ) ;
#1119 = CARTESIAN_POINT ( 'NONE',  ( 1.443569553805774897, 0.2306618581243848609, 0.2411417322834645549 ) ) ;
#1120 = CARTESIAN_POINT ( 'NONE',  ( 1.010498687664042716, -0.4281496062992124485, 0.4176697321401328655 ) ) ;
#1121 = CARTESIAN_POINT ( 'NONE',  ( -0.4724409448818898682, -8.678599364036362592E-17, -1.929133858267716439 ) ) ;
#1122 = VECTOR ( 'NONE', #79900, 39.37007874015748143 ) ;
#1123 = CARTESIAN_POINT ( 'NONE',  ( 1.167979002624672580, 0.05413385826771626580, -0.4176697321401330321 ) ) ;
#1124 = ORIENTED_EDGE ( 'NONE', *, *, #39342, .F. ) ;
#1125 = EDGE_LOOP ( 'NONE', ( #30642, #47090, #57720, #8607 ) ) ;
#1126 = CARTESIAN_POINT ( 'NONE',  ( -1.456692913385826182, -0.6692913385826771977, 8.415575281601705876E-17 ) ) ;
#1128 = CARTESIAN_POINT ( 'NONE',  ( -0.6561679790026240244, 0.2306618581243847221, -0.2411417322834647770 ) ) ;
#1127 = CARTESIAN_POINT ( 'NONE',  ( -0.8267716535433065062, 0.1771653543307087630, 0.000000000000000000 ) ) ;
#1129 = CARTESIAN_POINT ( 'NONE',  ( 0.3917322834645669549, 2.398668435337827645E-17, -2.245387508365142892 ) ) ;
#1130 = DIRECTION ( 'NONE',  ( 0.000000000000000000, -0.6427876096865366984, -0.7660444431189802339 ) ) ;
#1131 = CARTESIAN_POINT ( 'NONE',  ( 1.509186351706037543, 0.05413385826771666132, 0.4176697321401328100 ) ) ;
#1132 = CARTESIAN_POINT ( 'NONE',  ( -1.167979002624671470, -0.4281496062992127816, -0.4176697321401328100 ) ) ;
#1133 = CARTESIAN_POINT ( 'NONE',  ( 0.3280839895013130669, 0.05413385826771666132, 0.4176697321401328100 ) ) ;
#1134 = CARTESIAN_POINT ( 'NONE',  ( -1.227034120734907141, -0.6692913385826773087, -0.1292274648535924053 ) ) ;
#1135 = CARTESIAN_POINT ( 'NONE',  ( 0.3917322834645670104, -0.1049643490035303411, 0.1187664041994749703 ) ) ;
#1136 = CARTESIAN_POINT ( 'NONE',  ( 0.7742782152230978099, -0.4281496062992124485, 0.4176697321401328655 ) ) ;
#1137 = CARTESIAN_POINT ( 'NONE',  ( -0.1049643490035307020, 0.3917322834645669549, -2.045931758530183497 ) ) ;
#1138 = CARTESIAN_POINT ( 'NONE',  ( -0.8464566929133852113, 0.07958543189024085140, 0.2665933059059887866 ) ) ;
#1139 = ORIENTED_EDGE ( 'NONE', *, *, #22849, .T. ) ;
#1140 = CARTESIAN_POINT ( 'NONE',  ( -0.1974969037888706647, 0.3420746716998658843, -1.902887139107611869 ) ) ;
#1141 = ORIENTED_EDGE ( 'NONE', *, *, #845, .F. ) ;
#1142 = CARTESIAN_POINT ( 'NONE',  ( -0.7426113562971995430, 2.793565526369265584, 0.5309055118110235227 ) ) ;
#1143 = CARTESIAN_POINT ( 'NONE',  ( -1.207349081364828880, 0.2306618581243847221, -0.2411417322834647770 ) ) ;
#1144 = CARTESIAN_POINT ( 'NONE',  ( -1.456692913385826182, 0.2952755905511811885, 0.000000000000000000 ) ) ;
#1145 = CARTESIAN_POINT ( 'NONE',  ( -9.787531504996567848E-17, 0.3996062992125986035, -0.6299212598425196763 ) ) ;
#1146 = CARTESIAN_POINT ( 'NONE',  ( -1.706036745406823485, 0.2306618581243848609, 0.2411417322834645549 ) ) ;
#1147 = CARTESIAN_POINT ( 'NONE',  ( -1.141732283464566011, -0.6692913385826771977, 8.415575281601705876E-17 ) ) ;
#1148 = CARTESIAN_POINT ( 'NONE',  ( -1.312335958005248715, 0.2306618581243848609, 0.2411417322834645549 ) ) ;
#1149 = CARTESIAN_POINT ( 'NONE',  ( -0.3836918680457887532, -2.191421614605370878E-15, 0.4445507791589071167 ) ) ;
#1150 = CARTESIAN_POINT ( 'NONE',  ( -0.8136482939632537770, 0.2306618581243847221, -0.2411417322834647770 ) ) ;
#1151 = CARTESIAN_POINT ( 'NONE',  ( 0.1312335958005257930, 0.1283753931104746893, -0.1820866141732285504 ) ) ;
#1152 = CARTESIAN_POINT ( 'NONE',  ( 3.591975847892823865E-17, 2.185039370078740273, 0.2736220472440938911 ) ) ;
#1153 = CARTESIAN_POINT ( 'NONE',  ( 0.2867679344610365999, -0.2867679344610365444, -0.3405511811023621549 ) ) ;
#1154 = CARTESIAN_POINT ( 'NONE',  ( -0.4855643044619415427, -0.3690944881889763329, 0.3153832671262228327 ) ) ;
#1155 = CARTESIAN_POINT ( 'NONE',  ( -0.6364829396325453192, -0.05778040916215560624, -0.4822834645669293319 ) ) ;
#1156 = CARTESIAN_POINT ( 'NONE',  ( 0.8727034120734912248, -0.3162353388693409650, -0.4822834645669289433 ) ) ;
#1157 = CARTESIAN_POINT ( 'NONE',  ( -0.3871391076115476282, -0.05778040916215522460, 0.4822834645669289988 ) ) ;
#1158 = ORIENTED_EDGE ( 'NONE', *, *, #12089, .T. ) ;
#1159 = ORIENTED_EDGE ( 'NONE', *, *, #69637, .F. ) ;
#1160 = CARTESIAN_POINT ( 'NONE',  ( 4.893765752498283308E-17, -0.3996062992125985480, -2.202755905511811108 ) ) ;
#1161 = CARTESIAN_POINT ( 'NONE',  ( -1.030183727034119867, -0.3162353388693405765, 0.4822834645669290543 ) ) ;
#1162 = CARTESIAN_POINT ( 'NONE',  ( 1.082677165354331228, -0.5400638737290844871, 0.3530559997133364547 ) ) ;
#1163 = CARTESIAN_POINT ( 'NONE',  ( -1.732283464566928277, -0.1870078740157479769, 0.3641732283464567677 ) ) ;
#1164 =( CONVERSION_BASED_UNIT ( 'INCH', #77760 ) LENGTH_UNIT ( ) NAMED_UNIT ( #11550 ) );
#1165 = CARTESIAN_POINT ( 'NONE',  ( -0.4724409448818898682, -8.678599364036362592E-17, -1.141732283464566899 ) ) ;
#1166 = LINE ( 'NONE', #52475, #66762 ) ;
#1167 = CARTESIAN_POINT ( 'NONE',  ( 0.3392501089628018329, 0.1958661417322835607, -0.1233595800524933811 ) ) ;
#1168 = CARTESIAN_POINT ( 'NONE',  ( -0.2867679344610366554, 0.2867679344610365444, -2.624015748031495843 ) ) ;
#1169 = CARTESIAN_POINT ( 'NONE',  ( -0.2624671916010490880, -0.6046776061558807314, 0.2411417322834647770 ) ) ;
#1170 = CARTESIAN_POINT ( 'NONE',  ( -1.469816272965878357, 0.1283753931104748280, 0.1820866141732283561 ) ) ;
#1171 = CARTESIAN_POINT ( 'NONE',  ( -0.8136482939632537770, -0.6046776061558807314, 0.2411417322834647770 ) ) ;
#1172 = CARTESIAN_POINT ( 'NONE',  ( -0.1070741851644051862, -0.3996062992125986590, -0.1489501312335958227 ) ) ;
#1174 = DIRECTION ( 'NONE',  ( -0.000000000000000000, 1.734723475976808327E-16, 1.000000000000000000 ) ) ;
#1173 = CARTESIAN_POINT ( 'NONE',  ( -1.259842519685038686, -0.1870078740157479769, 0.4822834645669291653 ) ) ;
#1175 = CARTESIAN_POINT ( 'NONE',  ( -0.8464566929133852113, -0.5400638737290845981, -0.3530559997133363437 ) ) ;
#1176 = CARTESIAN_POINT ( 'NONE',  ( -0.3543307086614165824, -0.6692913385826771977, 8.415575281601705876E-17 ) ) ;
#1177 = CARTESIAN_POINT ( 'NONE',  ( -0.2891555358219909388, -0.2891555358219912164, -2.812992125984251857 ) ) ;
#1178 = CARTESIAN_POINT ( 'NONE',  ( 0.7939632545931766261, -0.08942795157527998196, 0.3641732283464567121 ) ) ;
#1179 = CARTESIAN_POINT ( 'NONE',  ( 0.3917322834645670104, 2.398668435337828261E-17, -0.2027559055118111353 ) ) ;
#1180 = CARTESIAN_POINT ( 'NONE',  ( 0.1246719160104994284, 0.1771653543307087075, -0.09757992244046823083 ) ) ;
#1181 = CARTESIAN_POINT ( 'NONE',  ( 1.535433070866142335, -0.5511811023622047445, 6.969142054262312111E-17 ) ) ;
#1182 = CARTESIAN_POINT ( 'NONE',  ( 1.548556430446194954, -0.6046776061558807314, 0.2411417322834647770 ) ) ;
#1183 = CARTESIAN_POINT ( 'NONE',  ( 0.1574803149606306130, -0.1870078740157480601, -0.3641732283464567677 ) ) ;
#1184 = CARTESIAN_POINT ( 'NONE',  ( 0.3917322834645669549, 0.1049643490035304660, -1.849081364829396223 ) ) ;
#1185 = CARTESIAN_POINT ( 'NONE',  ( -1.345144356955379816, -0.3162353388693405765, 0.4822834645669290543 ) ) ;
#1186 = CARTESIAN_POINT ( 'NONE',  ( 1.213910761154856299, -0.6692913385826773087, -0.1292274648535924053 ) ) ;
#1187 = B_SPLINE_CURVE_WITH_KNOTS ( 'NONE', 3,
 ( #54995, #8742, #74380, #67239 ),
 .UNSPECIFIED., .F., .F.,
 ( 4, 4 ),
 ( 0.1688788475280605661, 0.1702663099542993941 ),
 .UNSPECIFIED. ) ;
#1188 = CARTESIAN_POINT ( 'NONE',  ( 0.2362204724409451007, -0.4091458600556402980, 0.1463254593175852825 ) ) ;
#1189 = CARTESIAN_POINT ( 'NONE',  ( -0.7020997375328074108, -0.08942795157527998196, 0.3641732283464567121 ) ) ;
#1190 = CARTESIAN_POINT ( 'NONE',  ( -0.4593175853018366950, 0.05413385826771666132, 0.4176697321401328100 ) ) ;
#1191 = CARTESIAN_POINT ( 'NONE',  ( 0.2887139107611556010, 0.2306618581243847221, -0.2411417322834647770 ) ) ;
#1192 = CARTESIAN_POINT ( 'NONE',  ( 0.4091458600556403535, 0.2362204724409449896, -0.6804461942257218343 ) ) ;
#1193 = CARTESIAN_POINT ( 'NONE',  ( 1.122047244094488860, 0.07958543189024085140, 0.2665933059059887866 ) ) ;
#1194 = CARTESIAN_POINT ( 'NONE',  ( 0.3477690288713918276, 0.1771653543307087630, 0.09757992244046791164 ) ) ;
#1195 = CARTESIAN_POINT ( 'NONE',  ( -0.1837270341207340729, 0.2306618581243847221, -0.2411417322834647770 ) ) ;
#1196 = CARTESIAN_POINT ( 'NONE',  ( 3.937007874015748143, 2.559055118110236560, 0.5314960629921260393 ) ) ;
#1197 = CARTESIAN_POINT ( 'NONE',  ( -0.8661417322834640276, -0.1870078740157479769, 0.3641732283464567677 ) ) ;
#1198 = CARTESIAN_POINT ( 'NONE',  ( 0.4606732211678799538, 2.793565526369266028, -0.5309055118110236338 ) ) ;
#1199 = CARTESIAN_POINT ( 'NONE',  ( 0.6496062992125991586, -0.5400638737290845981, -0.3530559997133363437 ) ) ;
#1200 = CARTESIAN_POINT ( 'NONE',  ( -1.062992125984250968, -0.6692913385826771977, 8.415575281601705876E-17 ) ) ;
#1201 = CARTESIAN_POINT ( 'NONE',  ( 0.3996062992125984925, 0.1070741851644054637, -0.9888451443569553634 ) ) ;
#1202 = CARTESIAN_POINT ( 'NONE',  ( -0.2867679344610365999, 0.2867679344610364889, -2.781496062992125040 ) ) ;
#1203 = CARTESIAN_POINT ( 'NONE',  ( 0.1115485564304467270, -0.5511811023622048555, -0.09757992244046775898 ) ) ;
#1204 = CARTESIAN_POINT ( 'NONE',  ( -0.8267716535433065062, 0.2952755905511811885, 0.000000000000000000 ) ) ;
#1205 = CARTESIAN_POINT ( 'NONE',  ( -1.207349081364828436, -0.6046776061558807314, 0.2411417322834647770 ) ) ;
#1206 = CARTESIAN_POINT ( 'NONE',  ( -1.148293963254592542, 0.1771653543307087630, 0.09757992244046791164 ) ) ;
#1207 = CARTESIAN_POINT ( 'NONE',  ( -3.937007874015748143, 1.537401574803149984, -2.901595197523589142E-16 ) ) ;
#1208 = CARTESIAN_POINT ( 'NONE',  ( -0.8398950131233585692, 0.1283753931104748280, 0.1820866141732283561 ) ) ;
#1209 = CARTESIAN_POINT ( 'NONE',  ( -1.595398199321655497, 1.860919225514068076, 0.1559797534342490799 ) ) ;
#1210 = CARTESIAN_POINT ( 'NONE',  ( 1.128608923884514947, 0.2306618581243848609, 0.2411417322834645549 ) ) ;
#1211 = CARTESIAN_POINT ( 'NONE',  ( -0.1998031496062994683, 0.3460692066303958092, -0.1706036745406823985 ) ) ;
#1212 = CARTESIAN_POINT ( 'NONE',  ( 0.3917322834645670104, 0.1049643490035304660, -2.483615116306773452 ) ) ;
#1213 = ORIENTED_EDGE ( 'NONE', *, *, #76419, .T. ) ;
#1214 = FACE_BOUND ( 'NONE', #26809, .T. ) ;
#1215 = EDGE_CURVE ( 'NONE', #15840, #72947, #65515, .T. ) ;
#1216 = CARTESIAN_POINT ( 'NONE',  ( -1.699475065616797398, 0.2952755905511811885, 0.1292274648535926551 ) ) ;
#1217 = CARTESIAN_POINT ( 'NONE',  ( -1.417322834645668772, -0.1870078740157479769, 0.4822834645669291653 ) ) ;
#1218 = CARTESIAN_POINT ( 'NONE',  ( 1.397637795275591177, -0.5400638737290844871, 0.3530559997133364547 ) ) ;
#1219 = CARTESIAN_POINT ( 'NONE',  ( 0.2867679344610365999, 0.2867679344610365999, -2.269685039370078705 ) ) ;
#1220 = FACE_OUTER_BOUND ( 'NONE', #57084, .T. ) ;
#1221 = EDGE_CURVE ( 'NONE', #16864, #33327, #33540, .T. ) ;
#1222 = CARTESIAN_POINT ( 'NONE',  ( 0.3543307086614181922, -0.6692913385826771977, 8.415575281601705876E-17 ) ) ;
#1223 = CARTESIAN_POINT ( 'NONE',  ( -0.4199475065616791736, -0.6046776061558807314, 0.2411417322834647770 ) ) ;
#1224 = CARTESIAN_POINT ( 'NONE',  ( 0.4622706148242299307, 1.429654486764701193, -3.909775711958814348 ) ) ;
#1225 = DIRECTION ( 'NONE',  ( -0.000000000000000000, -1.000000000000000000, -0.000000000000000000 ) ) ;
#1226 = CARTESIAN_POINT ( 'NONE',  ( 0.7217847769028878924, -0.3690944881889765550, -0.3153832671262227771 ) ) ;
#1227 = CARTESIAN_POINT ( 'NONE',  ( -0.3460692066303958092, -0.1998031496062994683, -1.469816272965879245 ) ) ;
#1228 = ORIENTED_EDGE ( 'NONE', *, *, #71870, .F. ) ;
#1229 = CARTESIAN_POINT ( 'NONE',  ( 0.1049643490035303967, 0.3917322834645670659, -0.1476571110574297074 ) ) ;
#1230 = VERTEX_POINT ( 'NONE', #26801 ) ;
#1231 = CARTESIAN_POINT ( 'NONE',  ( -0.1049868766404193215, 0.2306618581243847221, -0.2411417322834647770 ) ) ;
#1232 = CARTESIAN_POINT ( 'NONE',  ( 1.456692913385827515, 0.2952755905511811885, 0.000000000000000000 ) ) ;
#1233 = CARTESIAN_POINT ( 'NONE',  ( 0.4199475065616805614, 0.2306618581243848609, 0.2411417322834645549 ) ) ;
#1234 = CARTESIAN_POINT ( 'NONE',  ( 1.404199475065617708, 0.05413385826771626580, -0.4176697321401330321 ) ) ;
#1235 = CARTESIAN_POINT ( 'NONE',  ( -0.6364829396325453192, -0.05778040916215560624, -0.4822834645669293319 ) ) ;
#1236 = CARTESIAN_POINT ( 'NONE',  ( 5.463695987328526437E-16, -0.1870078740157479769, 0.4822834645669291653 ) ) ;
#1237 = CARTESIAN_POINT ( 'NONE',  ( 1.456692913385827515, 0.2952755905511811885, 0.000000000000000000 ) ) ;
#1238 = CARTESIAN_POINT ( 'NONE',  ( 1.233595800524935227, -0.6046776061558807314, 0.2411417322834647770 ) ) ;
#1239 = CARTESIAN_POINT ( 'NONE',  ( 1.351706036745407680, 0.05413385826771666132, 0.4176697321401328100 ) ) ;
#1240 = EDGE_CURVE ( 'NONE', #12200, #44534, #303, .T. ) ;
#1241 = CARTESIAN_POINT ( 'NONE',  ( 4.797336870675656522E-17, -0.3917322834645670104, -0.2283464566929133410 ) ) ;
#1242 = CARTESIAN_POINT ( 'NONE',  ( 0.2296587926509192634, -0.2845877964562159024, 0.3641732283464567677 ) ) ;
#1243 = VERTEX_POINT ( 'NONE', #14615 ) ;
#1244 = CARTESIAN_POINT ( 'NONE',  ( 0.3420746716998659953, 0.1974969037888705536, -0.6036745406824147731 ) ) ;
#1245 = ORIENTED_EDGE ( 'NONE', *, *, #82772, .T. ) ;
#1246 = CARTESIAN_POINT ( 'NONE',  ( -0.5314960629921254842, -0.4536011799217368745, -0.2665933059059886201 ) ) ;
#1247 = CARTESIAN_POINT ( 'NONE',  ( 0.09186351706036827158, 0.05413385826771666132, 0.4176697321401328100 ) ) ;
#1248 = CARTESIAN_POINT ( 'NONE',  ( 2.759994995438110443, 1.188885443925058238, 0.3231744412229853869 ) ) ;
#1249 = CARTESIAN_POINT ( 'NONE',  ( 0.2559055118110243332, -0.5400638737290845981, -0.3530559997133363437 ) ) ;
#1250 = CARTESIAN_POINT ( 'NONE',  ( 0.1771653543307093182, 0.1660481256975885056, 0.3530559997133364547 ) ) ;
#1251 = EDGE_CURVE ( 'NONE', #57928, #4124, #72516, .T. ) ;
#1252 = CARTESIAN_POINT ( 'NONE',  ( -0.7020997375328074108, -0.05778040916215522460, 0.4822834645669289988 ) ) ;
#1253 = CARTESIAN_POINT ( 'NONE',  ( -0.8005249343832013809, -0.4281496062992124485, 0.4176697321401328655 ) ) ;
#1254 = CARTESIAN_POINT ( 'NONE',  ( 1.200787401574803681, 0.07958543189024085140, 0.2665933059059887866 ) ) ;
#1255 = CARTESIAN_POINT ( 'NONE',  ( 1.604771003085129433, 0.4514378173630680946, 0.1466069496707752551 ) ) ;
#1256 = DIRECTION ( 'NONE',  ( 1.000000000000000000, 0.000000000000000000, 0.000000000000000000 ) ) ;
#1257 = CARTESIAN_POINT ( 'NONE',  ( 1.030183727034121421, -0.2845877964562161244, -0.3641732283464567121 ) ) ;
#1258 = CARTESIAN_POINT ( 'NONE',  ( 0.5905511811023629321, 0.2952755905511811885, 0.000000000000000000 ) ) ;
#1259 = CARTESIAN_POINT ( 'NONE',  ( 0.9251968503937015864, 0.1660481256975883668, -0.3530559997133364547 ) ) ;
#1260 = CARTESIAN_POINT ( 'NONE',  ( 0.1070741851644053527, 0.3996062992125986590, -1.410761154855643129 ) ) ;
#1261 = CARTESIAN_POINT ( 'NONE',  ( -1.594488188976377563, -0.5400638737290844871, 0.3530559997133364547 ) ) ;
#1262 = CARTESIAN_POINT ( 'NONE',  ( -0.1070741851644056997, 0.3996062992125984925, -0.7132545931758530466 ) ) ;
#1263 = CARTESIAN_POINT ( 'NONE',  ( -0.3460692066303960313, 0.1998031496062989965, -0.1030183727034120894 ) ) ;
#1264 = CARTESIAN_POINT ( 'NONE',  ( -0.4790026246719154557, -0.3162353388693405765, 0.4822834645669290543 ) ) ;
#1265 = CARTESIAN_POINT ( 'NONE',  ( 0.3460692066303959202, 0.1998031496062993295, -2.650918635170603554 ) ) ;
#1266 = CARTESIAN_POINT ( 'NONE',  ( 0.3392501089628018329, 0.1958661417322835607, -1.948162729658792891 ) ) ;
#1267 = CARTESIAN_POINT ( 'NONE',  ( -1.246719160104985846, -0.3690944881889765550, -0.3153832671262227771 ) ) ;
#1268 = CARTESIAN_POINT ( 'NONE',  ( 1.213910761154856299, -0.6692913385826773087, -0.1292274648535924053 ) ) ;
#1269 = CARTESIAN_POINT ( 'NONE',  ( 1.115485564304462551, -0.4281496062992127816, -0.4176697321401328100 ) ) ;
#1270 = CARTESIAN_POINT ( 'NONE',  ( -0.3018372703412066094, -0.3690944881889765550, -0.3153832671262227771 ) ) ;
#1271 = CARTESIAN_POINT ( 'NONE',  ( 0.2821522309711292364, -0.6692913385826771977, 0.1292274648535927661 ) ) ;
#1272 = CARTESIAN_POINT ( 'NONE',  ( 0.1265901696524989462, 0.4724409448818897572, -1.330052493438320216 ) ) ;
#1273 = CARTESIAN_POINT ( 'NONE',  ( 0.3674540682414705883, -0.5023911411419708095, 0.1820866141732285504 ) ) ;
#1274 = CARTESIAN_POINT ( 'NONE',  ( -0.09842519685039295696, 0.1660481256975883668, -0.3530559997133364547 ) ) ;
#1275 = CARTESIAN_POINT ( 'NONE',  ( 0.3420746716998660508, -0.1974969037888704149, -1.284120734908136718 ) ) ;
#1276 = CARTESIAN_POINT ( 'NONE',  ( -1.259842519685038686, -0.1870078740157479769, 0.4822834645669291653 ) ) ;
#1277 = CARTESIAN_POINT ( 'NONE',  ( 0.6430446194225728496, -0.004921259842519576551, 0.3153832671262227771 ) ) ;
#1278 = CARTESIAN_POINT ( 'NONE',  ( 0.3805774278215230400, 0.009842519685039144428, -0.3409548833797004797 ) ) ;
#1279 = CARTESIAN_POINT ( 'NONE',  ( -0.8923884514435688198, 0.2306618581243847221, -0.2411417322834647770 ) ) ;
#1280 = CARTESIAN_POINT ( 'NONE',  ( -0.1443569553805765515, -0.3690944881889765550, -0.3153832671262227771 ) ) ;
#1281 = FACE_OUTER_BOUND ( 'NONE', #60724, .T. ) ;
#1282 = CARTESIAN_POINT ( 'NONE',  ( -0.8267716535433065062, -0.6692913385826771977, 8.415575281601705876E-17 ) ) ;
#1283 = CARTESIAN_POINT ( 'NONE',  ( -0.7020997375328074108, -0.05778040916215522460, 0.4822834645669289988 ) ) ;
#1284 = CARTESIAN_POINT ( 'NONE',  ( 0.1049868766404206816, 0.2306618581243848609, 0.2411417322834645549 ) ) ;
#1285 = CARTESIAN_POINT ( 'NONE',  ( -0.1070741851644051862, -0.3996062992125986590, -2.353674540682414662 ) ) ;
#1286 = CARTESIAN_POINT ( 'NONE',  ( 0.2867679344610365999, -0.2867679344610365999, -1.910741839073804016 ) ) ;
#1287 = DIRECTION ( 'NONE',  ( -1.000000000000000000, -0.000000000000000000, -0.000000000000000000 ) ) ;
#1288 = CARTESIAN_POINT ( 'NONE',  ( 0.8923884514435703741, 0.1283753931104748280, 0.1820866141732283561 ) ) ;
#1289 = CARTESIAN_POINT ( 'NONE',  ( 1.450131233595801428, 0.2952755905511811885, 0.1292274648535926551 ) ) ;
#1290 = CARTESIAN_POINT ( 'NONE',  ( -0.9055118110236215490, 0.1771653543307087630, 0.000000000000000000 ) ) ;
#1291 = CARTESIAN_POINT ( 'NONE',  ( -1.003937007874015297, -0.4536011799217368745, -0.2665933059059886201 ) ) ;
#1292 = CARTESIAN_POINT ( 'NONE',  ( -0.7086614173228339419, -0.1870078740157479769, 0.4822834645669291653 ) ) ;
#1293 = CARTESIAN_POINT ( 'NONE',  ( -0.2493438320209966919, 0.05413385826771626580, -0.4176697321401330321 ) ) ;
#1294 = CARTESIAN_POINT ( 'NONE',  ( 0.7086614173228353852, -0.1870078740157479769, 0.3641732283464567677 ) ) ;
#1295 = CARTESIAN_POINT ( 'NONE',  ( -0.2635443281053753695, 0.1334515064332122414, 5.819037890265706281 ) ) ;
#1296 = CARTESIAN_POINT ( 'NONE',  ( 1.148293963254593653, 0.1771653543307087075, -0.09757992244046823083 ) ) ;
#1297 = ADVANCED_FACE ( 'NONE', ( #26383 ), #52458, .F. ) ;
#1298 = CARTESIAN_POINT ( 'NONE',  ( 0.3083989501312343062, -0.05778040916215560624, -0.4822834645669293319 ) ) ;
#1299 = CARTESIAN_POINT ( 'NONE',  ( -0.3996062992125985480, -7.340648628747423112E-17, 0.04133858267716534335 ) ) ;
#1300 = CARTESIAN_POINT ( 'NONE',  ( -0.5511811023622041894, -0.1870078740157480879, -0.4822834645669291653 ) ) ;
#1301 = CARTESIAN_POINT ( 'NONE',  ( 0.1049643490035304938, -0.3917322834645669549, -1.587270341207349222 ) ) ;
#1302 = CARTESIAN_POINT ( 'NONE',  ( 1.266404199475066328, -0.08942795157527998196, 0.3641732283464567121 ) ) ;
#1303 = CARTESIAN_POINT ( 'NONE',  ( 0.3083989501312343062, -0.05778040916215560624, -0.4822834645669293319 ) ) ;
#1304 = CARTESIAN_POINT ( 'NONE',  ( 0.01312335958005323398, -0.4281496062992127816, -0.4176697321401328100 ) ) ;
#1305 = CARTESIAN_POINT ( 'NONE',  ( 0.1706036745406830368, -0.3690944881889765550, -0.3153832671262227771 ) ) ;
#1306 = DIRECTION ( 'NONE',  ( 0.000000000000000000, 0.000000000000000000, -1.000000000000000000 ) ) ;
#1307 = CARTESIAN_POINT ( 'NONE',  ( -0.03280839895013062252, 0.1771653543307087075, -0.09757992244046823083 ) ) ;
#1308 = CARTESIAN_POINT ( 'NONE',  ( 0.8595800524934390507, -0.3162353388693405765, 0.4822834645669290543 ) ) ;
#1309 = CARTESIAN_POINT ( 'NONE',  ( -0.7611548556430438595, 0.1283753931104748280, 0.1820866141732283561 ) ) ;
#1310 = CARTESIAN_POINT ( 'NONE',  ( -0.6692913385826764205, 0.2952755905511811885, 0.000000000000000000 ) ) ;
#1311 = CARTESIAN_POINT ( 'NONE',  ( -0.8537221893815262197, -2.294479370626195693E-15, 0.3464511005275217603 ) ) ;
#1312 = EDGE_LOOP ( 'NONE', ( #54492, #20805, #16795, #50693 ) ) ;
#1313 = CARTESIAN_POINT ( 'NONE',  ( -1.279527559055116948, 0.1660481256975883668, -0.3530559997133364547 ) ) ;
#1314 = CARTESIAN_POINT ( 'NONE',  ( -1.299212598425196097, -0.5511811023622047445, 6.969142054262312111E-17 ) ) ;
#1315 = CARTESIAN_POINT ( 'NONE',  ( -0.03937007874015669567, -0.6692913385826771977, 8.415575281601705876E-17 ) ) ;
#1316 = CARTESIAN_POINT ( 'NONE',  ( -1.489501312335957062, -0.3162353388693409650, -0.4822834645669289433 ) ) ;
#1317 = CARTESIAN_POINT ( 'NONE',  ( -0.9317585301837263412, -0.4281496062992127816, -0.4176697321401328100 ) ) ;
#1318 = CARTESIAN_POINT ( 'NONE',  ( 0.5314960629921156032, 0.000000000000000000, 0.9881811337016697117 ) ) ;
#1320 = CARTESIAN_POINT ( 'NONE',  ( 1.069553805774278610, -0.6692913385826771977, 0.1292274648535927661 ) ) ;
#1319 = CARTESIAN_POINT ( 'NONE',  ( 1.069553805774278832, 0.2952755905511810219, -0.1292274648535930437 ) ) ;
#1321 = CARTESIAN_POINT ( 'NONE',  ( 1.410761154855643795, -0.05778040916215560624, -0.4822834645669293319 ) ) ;
#1322 = CARTESIAN_POINT ( 'NONE',  ( 0.2867679344610366554, 0.2867679344610366554, -2.334645669291338432 ) ) ;
#1323 = CARTESIAN_POINT ( 'NONE',  ( 1.348312163386739426, 1.062992125984252079, 0.7386866130305692613 ) ) ;
#1324 = CARTESIAN_POINT ( 'NONE',  ( -1.187664041994750175, -0.05778040916215560624, -0.4822834645669293319 ) ) ;
#1325 = CARTESIAN_POINT ( 'NONE',  ( 0.4724409448818897572, -0.1265901696524988906, -0.7414698162729659314 ) ) ;
#1326 = CARTESIAN_POINT ( 'NONE',  ( 0.1070741851644053527, 0.3996062992125986590, 0.006561679790026227546 ) ) ;
#1327 = ORIENTED_EDGE ( 'NONE', *, *, #22709, .T. ) ;
#1328 = CARTESIAN_POINT ( 'NONE',  ( -0.2624671916010490880, -0.5023911411419708095, 0.1820866141732285504 ) ) ;
#1329 = CARTESIAN_POINT ( 'NONE',  ( 4.797336870675656522E-17, -0.3917322834645670104, -1.803149606299212726 ) ) ;
#1330 = ORIENTED_EDGE ( 'NONE', *, *, #56817, .F. ) ;
#1331 = CARTESIAN_POINT ( 'NONE',  ( 0.1246719160104994284, -0.6692913385826771977, 0.1292274648535927661 ) ) ;
#1332 = CARTESIAN_POINT ( 'NONE',  ( 0.1181102362204730916, -0.6692913385826771977, 8.415575281601705876E-17 ) ) ;
#1333 = CARTESIAN_POINT ( 'NONE',  ( -0.6561679790026240244, 0.2306618581243847221, -0.2411417322834647770 ) ) ;
#1334 = DIRECTION ( 'NONE',  ( 0.5773502691896310601, -0.5773502691896310601, -0.5773502691896149619 ) ) ;
#1335 = CARTESIAN_POINT ( 'NONE',  ( -0.9514435695538050464, -0.08942795157528024563, -0.3641732283464568787 ) ) ;
#1336 = CARTESIAN_POINT ( 'NONE',  ( 0.8070866141732289112, -0.5400638737290845981, -0.3530559997133363437 ) ) ;
#1337 = CARTESIAN_POINT ( 'NONE',  ( 0.7152230971128614723, -0.2845877964562161244, -0.3641732283464567121 ) ) ;
#1338 = CARTESIAN_POINT ( 'NONE',  ( -0.3346456692913377662, 0.1660481256975883668, -0.3530559997133364547 ) ) ;
#1339 = CARTESIAN_POINT ( 'NONE',  ( 4.797336870675655290E-17, -0.3917322834645669549, -1.103655224900575993 ) ) ;
#1340 = CARTESIAN_POINT ( 'NONE',  ( -0.6561679790026240244, 0.2306618581243847221, -0.2411417322834647770 ) ) ;
#1341 = CARTESIAN_POINT ( 'NONE',  ( -1.627296587926508442, -0.5023911411419708095, -0.1820866141732282451 ) ) ;
#1342 = EDGE_CURVE ( 'NONE', #17299, #25966, #65115, .T. ) ;
#1343 = CARTESIAN_POINT ( 'NONE',  ( 1.141732283464567788, -0.6692913385826771977, 8.415575281601705876E-17 ) ) ;
#1344 = CARTESIAN_POINT ( 'NONE',  ( 1.509186351706037543, -0.004921259842519576551, 0.3153832671262227771 ) ) ;
#1345 = EDGE_LOOP ( 'NONE', ( #66456, #45202, #47720, #72344 ) ) ;
#1346 = CARTESIAN_POINT ( 'NONE',  ( 0.2867679344610366554, 0.2867679344610366554, -2.654218790847456155 ) ) ;
#1347 = CARTESIAN_POINT ( 'NONE',  ( -0.1771653543307080136, 0.1660481256975883668, -0.3530559997133364547 ) ) ;
#1348 = ORIENTED_EDGE ( 'NONE', *, *, #13593, .T. ) ;
#1349 = CARTESIAN_POINT ( 'NONE',  ( -0.8923884514435688198, 0.2306618581243847221, -0.2411417322834647770 ) ) ;
#1350 = CARTESIAN_POINT ( 'NONE',  ( 1.299212598425197429, 0.2952755905511811885, 0.000000000000000000 ) ) ;
#1351 = CARTESIAN_POINT ( 'NONE',  ( 1.469816272965879911, 0.2306618581243847221, -0.2411417322834647770 ) ) ;
#1352 = CARTESIAN_POINT ( 'NONE',  ( 0.08530183727034192087, -0.3162353388693409650, -0.4822834645669289433 ) ) ;
#1353 = CARTESIAN_POINT ( 'NONE',  ( -0.2034120734908128059, 0.2952755905511811885, 0.1292274648535926551 ) ) ;
#1354 = CARTESIAN_POINT ( 'NONE',  ( 0.1049643490035303689, 0.3917322834645670104, -1.810367454068241511 ) ) ;
#1355 = CARTESIAN_POINT ( 'NONE',  ( -1.049868766404198794, 0.2306618581243847221, -0.2411417322834647770 ) ) ;
#1356 = CARTESIAN_POINT ( 'NONE',  ( -0.4199475065616791736, -0.6046776061558807314, 0.2411417322834647770 ) ) ;
#1357 = CARTESIAN_POINT ( 'NONE',  ( -0.1246719160104980823, -0.5511811023622048555, -0.09757992244046775898 ) ) ;
#1358 = CARTESIAN_POINT ( 'NONE',  ( 1.535433070866142558, 0.2952755905511811885, 0.000000000000000000 ) ) ;
#1359 = CARTESIAN_POINT ( 'NONE',  ( -0.6627296587926503335, -0.6692913385826771977, 0.1292274648535927661 ) ) ;
#1360 = CARTESIAN_POINT ( 'NONE',  ( -1.213910761154854967, 0.2952755905511810219, -0.1292274648535930437 ) ) ;
#1361 = CARTESIAN_POINT ( 'NONE',  ( 0.8005249343832027131, 0.05413385826771666132, 0.4176697321401328100 ) ) ;
#1362 = CARTESIAN_POINT ( 'NONE',  ( 3.915483736577200613, 1.300266479744685899, -0.4111838468780947276 ) ) ;
#1363 = ORIENTED_EDGE ( 'NONE', *, *, #54694, .F. ) ;
#1364 = CARTESIAN_POINT ( 'NONE',  ( -0.03937007874015669567, 0.2952755905511811885, 0.000000000000000000 ) ) ;
#1365 = CARTESIAN_POINT ( 'NONE',  ( -0.2296587926509179312, -0.2845877964562161244, -0.3641732283464567121 ) ) ;
#1367 = CARTESIAN_POINT ( 'NONE',  ( 0.6299212598425235621, 0.000000000000000000, -0.9285414500055687581 ) ) ;
#1366 = CARTESIAN_POINT ( 'NONE',  ( 1.220472440944882608, 0.1771653543307087630, 0.000000000000000000 ) ) ;
#1368 = CARTESIAN_POINT ( 'NONE',  ( -0.3458507752293906723, -0.3458507752293910609, -0.4507874015748031815 ) ) ;
#1369 = CARTESIAN_POINT ( 'NONE',  ( 1.646981627296588035, -0.2845877964562159024, 0.3641732283464567677 ) ) ;
#1370 = EDGE_CURVE ( 'NONE', #22431, #62933, #19231, .T. ) ;
#1371 = CARTESIAN_POINT ( 'NONE',  ( 1.167979002624672580, 0.05413385826771626580, -0.4176697321401330321 ) ) ;
#1372 = CARTESIAN_POINT ( 'NONE',  ( -0.3420746716998660508, -0.1974969037888706924, -0.1292650918635170898 ) ) ;
#1373 = CARTESIAN_POINT ( 'NONE',  ( 0.2230971128608929543, 0.05413385826771626580, -0.4176697321401330321 ) ) ;
#1374 = CARTESIAN_POINT ( 'NONE',  ( -1.489501312335957062, -0.3162353388693409650, -0.4822834645669289433 ) ) ;
#1375 = CARTESIAN_POINT ( 'NONE',  ( -0.2690288713910754526, 0.2952755905511810774, -0.1292274648535930714 ) ) ;
#1376 = EDGE_CURVE ( 'NONE', #53683, #11079, #1562, .T. ) ;
#1377 = CARTESIAN_POINT ( 'NONE',  ( 0.2891555358219910499, -0.2891555358219909944, 0.1397637795275590844 ) ) ;
#1378 = CARTESIAN_POINT ( 'NONE',  ( -1.633858267716534529, 0.07958543189024085140, 0.2665933059059887866 ) ) ;
#1379 = CARTESIAN_POINT ( 'NONE',  ( 0.5249343832021003964, 0.2306618581243847221, -0.2411417322834647770 ) ) ;
#1380 = CARTESIAN_POINT ( 'NONE',  ( 0.8858267716535438430, 0.07958543189024085140, 0.2665933059059887866 ) ) ;
#1381 = CARTESIAN_POINT ( 'NONE',  ( 0.2099737532808405305, -0.5023911411419708095, 0.1820866141732285504 ) ) ;
#1382 = CARTESIAN_POINT ( 'NONE',  ( -1.318897637795274802, 0.1660481256975885056, 0.3530559997133364547 ) ) ;
#1383 = CARTESIAN_POINT ( 'NONE',  ( -0.1998031496062994405, 0.3460692066303957537, -0.8772965879265091083 ) ) ;
#1384 = CARTESIAN_POINT ( 'NONE',  ( 1.286089238845145033, -0.6046776061558809534, -0.2411417322834644161 ) ) ;
#1385 = CARTESIAN_POINT ( 'NONE',  ( 0.1049643490035304938, -0.3917322834645669549, -0.8648293963254591876 ) ) ;
#1387 = CARTESIAN_POINT ( 'NONE',  ( 0.8792650918635177559, 0.05413385826771666132, 0.4176697321401328100 ) ) ;
#1386 = CARTESIAN_POINT ( 'NONE',  ( 0.8070866141732289112, -0.5400638737290845981, -0.3530559997133363437 ) ) ;
#1388 = CARTESIAN_POINT ( 'NONE',  ( 0.5314960629921070545, 2.755905511811024056, 1.813482582612299110 ) ) ;
#1389 = CARTESIAN_POINT ( 'NONE',  ( 0.4265091863517067039, -0.5511811023622048555, -0.09757992244046775898 ) ) ;
#1390 = CARTESIAN_POINT ( 'NONE',  ( 0.5577427821522316087, -0.05778040916215522460, 0.4822834645669289988 ) ) ;
#1391 = CARTESIAN_POINT ( 'NONE',  ( 1.627296587926509996, -0.5023911411419708095, 0.1820866141732285504 ) ) ;
#1392 = CARTESIAN_POINT ( 'NONE',  ( -0.8595800524934373854, -0.2845877964562161244, -0.3641732283464567121 ) ) ;
#1393 = CARTESIAN_POINT ( 'NONE',  ( -1.062992125984250968, 0.2952755905511811885, 0.000000000000000000 ) ) ;
#1394 = CARTESIAN_POINT ( 'NONE',  ( -1.528871391076114250, 0.2952755905511810774, -0.1292274648535930714 ) ) ;
#1395 = CARTESIAN_POINT ( 'NONE',  ( 0.8464566929133866546, -0.5400638737290844871, 0.3530559997133364547 ) ) ;
#1396 = CARTESIAN_POINT ( 'NONE',  ( -1.561679790026246017, -0.3690944881889765550, -0.3153832671262227771 ) ) ;
#1397 = CARTESIAN_POINT ( 'NONE',  ( -0.3951562584566667424, -0.01150853369506067876, -1.220472440945443493 ) ) ;
#1398 = CARTESIAN_POINT ( 'NONE',  ( 0.6561679790026253567, 0.2306618581243848609, 0.2411417322834645549 ) ) ;
#1399 = CARTESIAN_POINT ( 'NONE',  ( 0.4091458600556404646, -0.2362204724409448231, -2.858923884514435798 ) ) ;
#1400 = DIRECTION ( 'NONE',  ( 1.000000000000000000, -0.000000000000000000, -0.000000000000000000 ) ) ;
#1401 = CARTESIAN_POINT ( 'NONE',  ( 1.476377952755906442, -0.5400638737290844871, 0.3530559997133364547 ) ) ;
#1402 = CARTESIAN_POINT ( 'NONE',  ( -1.548556430446193399, 0.1283753931104748280, 0.1820866141732283561 ) ) ;
#1403 = CARTESIAN_POINT ( 'NONE',  ( 1.351706036745407680, -0.004921259842519576551, 0.3153832671262227771 ) ) ;
#1404 = CARTESIAN_POINT ( 'NONE',  ( -1.154855643044618851, 0.1283753931104748280, 0.1820866141732283561 ) ) ;
#1405 = CARTESIAN_POINT ( 'NONE',  ( -0.5380577427821514602, -0.004921259842519576551, 0.3153832671262227771 ) ) ;
#1406 = CARTESIAN_POINT ( 'NONE',  ( 0.1265901696524989184, 0.4724409448818898127, -2.040682414698162361 ) ) ;
#1407 = CARTESIAN_POINT ( 'NONE',  ( 0.9580052493438326877, -0.004921259842519576551, 0.3153832671262227771 ) ) ;
#1408 = CARTESIAN_POINT ( 'NONE',  ( 0.4396325459317593221, 0.2952755905511810774, -0.1292274648535930714 ) ) ;
#1409 = CARTESIAN_POINT ( 'NONE',  ( 1.181102362204724976, -0.1870078740157480879, -0.4822834645669291653 ) ) ;
#1410 = CIRCLE ( 'NONE', #37669, 0.1574803149606300579 ) ;
#1411 = CARTESIAN_POINT ( 'NONE',  ( 0.2034120734908144990, -0.6692913385826771977, 0.1292274648535927661 ) ) ;
#1412 = CARTESIAN_POINT ( 'NONE',  ( 0.4133858267716541968, -0.4536011799217368745, -0.2665933059059886201 ) ) ;
#1413 = CARTESIAN_POINT ( 'NONE',  ( 1.115485564304462551, 0.05413385826771666132, 0.4176697321401328100 ) ) ;
#1414 = PLANE ( 'NONE',  #32563 ) ;
#1415 = CARTESIAN_POINT ( 'NONE',  ( -0.5183727034120726440, -0.6692913385826773087, -0.1292274648535924053 ) ) ;
#1416 = CARTESIAN_POINT ( 'NONE',  ( -0.1070741851644057135, 0.3996062992125985480, -0.9514435695538056015 ) ) ;
#1417 = CARTESIAN_POINT ( 'NONE',  ( -0.3126853129631109174, 1.368901411070787777, 0.01600703956764241986 ) ) ;
#1418 = CARTESIAN_POINT ( 'NONE',  ( -0.01312335958005186876, -0.4281496062992124485, 0.4176697321401328655 ) ) ;
#1419 = CARTESIAN_POINT ( 'NONE',  ( -0.6299212598425188991, -0.1870078740157480879, -0.4822834645669291653 ) ) ;
#1420 = CARTESIAN_POINT ( 'NONE',  ( -0.2296587926509179312, -0.3162353388693409650, -0.4822834645669289433 ) ) ;
#1421 = CARTESIAN_POINT ( 'NONE',  ( 0.1998031496062994405, -0.3460692066303958092, -2.611548556430446144 ) ) ;
#1422 = CARTESIAN_POINT ( 'NONE',  ( 0.1974969037888706369, -0.3420746716998659953, -1.824146981627296382 ) ) ;
#1423 = CARTESIAN_POINT ( 'NONE',  ( 0.1049643490035304938, -0.3917322834645669549, -0.7073490813648293241 ) ) ;
#1424 = CARTESIAN_POINT ( 'NONE',  ( 0.3917322834645669549, 0.1049643490035304660, -1.061679790026246684 ) ) ;
#1425 = CARTESIAN_POINT ( 'NONE',  ( -0.9580052493438311334, -0.3690944881889763329, 0.3153832671262228327 ) ) ;
#1426 = CARTESIAN_POINT ( 'NONE',  ( -0.3917322834645671215, 0.1049643490035301469, -1.284776902887139194 ) ) ;
#1427 = CARTESIAN_POINT ( 'NONE',  ( -1.049868766404198794, 0.2306618581243847221, -0.2411417322834647770 ) ) ;
#1428 = CARTESIAN_POINT ( 'NONE',  ( 0.2867679344610365999, -0.2867679344610365999, 0.1365022554143850153 ) ) ;
#1429 = CARTESIAN_POINT ( 'NONE',  ( 0.4133858267716541968, 0.1660481256975885056, 0.3530559997133364547 ) ) ;
#1430 = CARTESIAN_POINT ( 'NONE',  ( -0.4199475065616791736, 0.1283753931104746893, -0.1820866141732285504 ) ) ;
#1431 = CARTESIAN_POINT ( 'NONE',  ( 1.437007874015748810, 0.1660481256975885056, 0.3530559997133364547 ) ) ;
#1432 = CARTESIAN_POINT ( 'NONE',  ( 0.1968503937007881344, 0.2952755905511811885, 0.000000000000000000 ) ) ;
#1433 = CARTESIAN_POINT ( 'NONE',  ( -0.4724922890202599146, 1.580837543196282446, -2.165463280039293892 ) ) ;
#1434 = CARTESIAN_POINT ( 'NONE',  ( 0.1070741851644054915, -0.3996062992125986035, -2.762467191601049255 ) ) ;
#1435 = CARTESIAN_POINT ( 'NONE',  ( 0.3917322834645670659, 2.398668435337828261E-17, -1.059730601871078148 ) ) ;
#1436 = CARTESIAN_POINT ( 'NONE',  ( 1.213910761154856299, 0.2952755905511811885, 0.1292274648535926551 ) ) ;
#1437 = CARTESIAN_POINT ( 'NONE',  ( 0.6430446194225728496, 0.05413385826771666132, 0.4176697321401328100 ) ) ;
#1438 = CARTESIAN_POINT ( 'NONE',  ( 0.1049868766404206816, -0.6046776061558809534, -0.2411417322834644161 ) ) ;
#1439 = CARTESIAN_POINT ( 'NONE',  ( 1.607611548556431069, 0.2952755905511811885, 0.1292274648535926551 ) ) ;
#1440 = CARTESIAN_POINT ( 'NONE',  ( 0.9251968503937015864, 0.1660481256975883668, -0.3530559997133364547 ) ) ;
#1441 = CARTESIAN_POINT ( 'NONE',  ( -0.1958661417322834220, -0.3392501089628018884, -0.6227034120734910028 ) ) ;
#1442 = CARTESIAN_POINT ( 'NONE',  ( 0.09186351706036799403, -0.4281496062992127816, -0.4176697321401328100 ) ) ;
#1443 = CARTESIAN_POINT ( 'NONE',  ( 1.108923884514436686, -0.3162353388693409650, -0.4822834645669289433 ) ) ;
#1444 = CARTESIAN_POINT ( 'NONE',  ( 0.3280839895013130669, -0.4281496062992127816, -0.4176697321401328100 ) ) ;
#1445 = CARTESIAN_POINT ( 'NONE',  ( 1.240157480314961314, 0.07958543189024071263, -0.2665933059059888421 ) ) ;
#1446 = CARTESIAN_POINT ( 'NONE',  ( -1.489501312335957062, -0.3162353388693409650, -0.4822834645669289433 ) ) ;
#1447 = CARTESIAN_POINT ( 'NONE',  ( -1.246719160104986512, 0.05413385826771666132, 0.4176697321401328100 ) ) ;
#1448 = CARTESIAN_POINT ( 'NONE',  ( 0.5774278215223103139, -0.6046776061558809534, -0.2411417322834644161 ) ) ;
#1449 = CARTESIAN_POINT ( 'NONE',  ( 0.4724409448818892576, 0.1265901696524997788, -0.5164041994750656617 ) ) ;
#1450 = CARTESIAN_POINT ( 'NONE',  ( -0.1049643490035302024, -0.3917322834645671215, -1.796587926509185973 ) ) ;
#1451 = EDGE_LOOP ( 'NONE', ( #12170, #38807, #56909, #39319 ) ) ;
#1452 = CARTESIAN_POINT ( 'NONE',  ( 0.3460692066303959202, 0.1998031496062993295, -0.2887139107611548794 ) ) ;
#1453 = VERTEX_POINT ( 'NONE', #31866 ) ;
#1454 = CARTESIAN_POINT ( 'NONE',  ( 1.627296587926509996, -0.6046776061558807314, 0.2411417322834647770 ) ) ;
#1455 = CARTESIAN_POINT ( 'NONE',  ( 1.003937007874016185, 0.07958543189024071263, -0.2665933059059888421 ) ) ;
#1456 = DIRECTION ( 'NONE',  ( -1.687538997430237941E-14, 0.000000000000000000, -1.000000000000000000 ) ) ;
#1457 = CARTESIAN_POINT ( 'NONE',  ( -0.008542603271839102619, 1.062992125984252301, 2.874015748031496731 ) ) ;
#1458 = DIRECTION ( 'NONE',  ( -3.096699300667737957E-16, 1.000000000000000000, -0.000000000000000000 ) ) ;
#1459 = CARTESIAN_POINT ( 'NONE',  ( 0.3392501089628018329, 0.1958661417322835607, -1.003280839895013266 ) ) ;
#1460 = EDGE_CURVE ( 'NONE', #74234, #57436, #76219, .T. ) ;
#1461 = CARTESIAN_POINT ( 'NONE',  ( 1.364829396325459854, -0.6046776061558809534, -0.2411417322834644161 ) ) ;
#1462 = CARTESIAN_POINT ( 'NONE',  ( -0.3726288332202236653, -0.1208384647423932784, -1.929133858267952473 ) ) ;
#1463 = CARTESIAN_POINT ( 'NONE',  ( -0.4855643044619415427, -0.4281496062992124485, 0.4176697321401328655 ) ) ;
#1464 = CARTESIAN_POINT ( 'NONE',  ( 1.076115485564305141, -0.6046776061558807314, 0.2411417322834647770 ) ) ;
#1465 = ORIENTED_EDGE ( 'NONE', *, *, #46764, .T. ) ;
#1466 = VECTOR ( 'NONE', #20081, 39.37007874015748143 ) ;
#1467 = CARTESIAN_POINT ( 'NONE',  ( -1.502624671916009680, -0.05778040916215560624, -0.4822834645669293319 ) ) ;
#1468 = CARTESIAN_POINT ( 'NONE',  ( -1.074107865122115868, 1.191152302059476087, -0.3246720348184669591 ) ) ;
#1469 = CARTESIAN_POINT ( 'NONE',  ( 3.523619145740964242, 3.916330350904249524, 2.040242213439797059 ) ) ;
#1470 = B_SPLINE_CURVE_WITH_KNOTS ( 'NONE', 3,
 ( #22018, #9392, #8152, #74203 ),
 .UNSPECIFIED., .F., .F.,
 ( 4, 4 ),
 ( 0.03364299943132197795, 0.03394594375427735511 ),
 .UNSPECIFIED. ) ;
#1471 = CARTESIAN_POINT ( 'NONE',  ( 1.679790026246720025, 0.1283753931104748280, 0.1820866141732283561 ) ) ;
#1472 = DIRECTION ( 'NONE',  ( -3.096699300667737957E-16, 1.000000000000000000, -0.000000000000000000 ) ) ;
#1473 = CARTESIAN_POINT ( 'NONE',  ( -0.8530183727034112984, -0.004921259842519576551, 0.3153832671262227771 ) ) ;
#1474 = CARTESIAN_POINT ( 'NONE',  ( 0.8858267716535437319, 0.1012011053420777407, 0.2882089793578256898 ) ) ;
#1475 = CARTESIAN_POINT ( 'NONE',  ( 0.7874015748031503170, -0.1870078740157480879, -0.4822834645669291653 ) ) ;
#1476 = ORIENTED_EDGE ( 'NONE', *, *, #70755, .T. ) ;
#1478 = DIRECTION ( 'NONE',  ( -0.000000000000000000, 1.000000000000000000, -0.000000000000000000 ) ) ;
#1477 = CARTESIAN_POINT ( 'NONE',  ( -0.5314960629921193780, 2.755905511811024056, -1.895394334970793793 ) ) ;
#1479 = CARTESIAN_POINT ( 'NONE',  ( 0.8727034120734913358, -0.05778040916215522460, 0.4822834645669289988 ) ) ;
#1480 = CARTESIAN_POINT ( 'NONE',  ( 1.502624671916010790, -0.2845877964562161244, -0.3641732283464567121 ) ) ;
#1481 = CARTESIAN_POINT ( 'NONE',  ( 0.3917322834645668994, -0.1049643490035303134, -0.9789833088900768976 ) ) ;
#1482 = CARTESIAN_POINT ( 'NONE',  ( -0.5971128608923877978, 0.1771653543307087630, 0.09757992244046791164 ) ) ;
#1483 = CARTESIAN_POINT ( 'NONE',  ( 1.646981627296588035, -0.3162353388693405765, 0.4822834645669290543 ) ) ;
#1484 = CARTESIAN_POINT ( 'NONE',  ( -0.1049643490035307020, 0.3917322834645669549, -1.193569553805774230 ) ) ;
#1485 = CARTESIAN_POINT ( 'NONE',  ( 0.5118110236220478892, 0.2952755905511811885, 0.000000000000000000 ) ) ;
#1486 = CARTESIAN_POINT ( 'NONE',  ( -1.095800524934382292, -0.2845877964562161244, -0.3641732283464567121 ) ) ;
#1487 = CARTESIAN_POINT ( 'NONE',  ( 0.1312335958005255154, -0.5023911411419708095, 0.1820866141732285504 ) ) ;
#1488 = AXIS2_PLACEMENT_3D ( 'NONE', #72842, #78337, #8046 ) ;
#1489 = CARTESIAN_POINT ( 'NONE',  ( -0.4002624671916004129, -0.05778040916215560624, -0.4822834645669293319 ) ) ;
#1490 = CARTESIAN_POINT ( 'NONE',  ( -1.207349081364828436, -0.5023911411419708095, 0.1820866141732285504 ) ) ;
#1491 = CARTESIAN_POINT ( 'NONE',  ( 0.2867679344610366554, -0.2867679344610365999, -0.09516367273721974829 ) ) ;
#1492 = CARTESIAN_POINT ( 'NONE',  ( 0.9120734908136489683, -0.6692913385826771977, 0.1292274648535927661 ) ) ;
#1493 =( BOUNDED_CURVE ( )  B_SPLINE_CURVE ( 2, ( #10605, #74166, #55192, #80899, #29935, #73759, #2632, #61524, #42568, #35027, #41739, #68269, #28288 ),
 .UNSPECIFIED., .F., .F. ) 
 B_SPLINE_CURVE_WITH_KNOTS ( ( 3, 2, 2, 2, 2, 2, 3 ),
 ( 0.4460583673620736045, 0.4469696969696969613, 0.4507575757575757458, 0.4545454545454545303, 0.4583333333333333148, 0.4621212121212120993, 0.4630325417288355672 ),
 .UNSPECIFIED. ) 
 CURVE ( )  GEOMETRIC_REPRESENTATION_ITEM ( )  RATIONAL_B_SPLINE_CURVE ( ( 0.9875488213027530104, 0.9918020599134685922, 1.000000000000000000, 0.9659258262890683122, 1.000000000000000000, 0.9659258262890683122, 1.000000000000000000, 0.9659258262890683122, 1.000000000000000000, 0.9659258262890683122, 1.000000000000000000, 0.9918020599134675930, 0.9875488213027519002 ) ) 
 REPRESENTATION_ITEM ( '' )  );
#1494 = FACE_OUTER_BOUND ( 'NONE', #73999, .T. ) ;
#1495 = CARTESIAN_POINT ( 'NONE',  ( 0.4724409448818897572, -0.1265901696524988906, -1.448162729658792669 ) ) ;
#1496 = CARTESIAN_POINT ( 'NONE',  ( -0.7808398950131225646, -0.05778040916215522460, 0.4822834645669289988 ) ) ;
#1497 = CARTESIAN_POINT ( 'NONE',  ( -0.1509186351706028884, -0.08942795157527998196, 0.3641732283464567121 ) ) ;
#1498 = CARTESIAN_POINT ( 'NONE',  ( -1.246719160104985846, -0.4281496062992127816, -0.4176697321401328100 ) ) ;
#1499 = CARTESIAN_POINT ( 'NONE',  ( 0.8595800524934390507, -0.2845877964562159024, 0.3641732283464567677 ) ) ;
#1500 = CARTESIAN_POINT ( 'NONE',  ( -0.7480314960629914633, 0.1771653543307087630, 0.000000000000000000 ) ) ;
#1501 = CARTESIAN_POINT ( 'NONE',  ( -1.056430446194224881, 0.2952755905511810774, -0.1292274648535930714 ) ) ;
#1502 = CARTESIAN_POINT ( 'NONE',  ( -0.9776902887139098386, -0.6692913385826771977, 0.1292274648535927661 ) ) ;
#1503 = CARTESIAN_POINT ( 'NONE',  ( -1.620734908136482577, 0.2952755905511811885, 0.1292274648535926551 ) ) ;
#1504 = CARTESIAN_POINT ( 'NONE',  ( 0.1265901696524989184, 0.4724409448818898127, -2.117454068241469756 ) ) ;
#1505 = CARTESIAN_POINT ( 'NONE',  ( 0.8989501312335964611, 0.1771653543307087630, 0.09757992244046791164 ) ) ;
#1506 = CARTESIAN_POINT ( 'NONE',  ( 0.3477690288713918276, -0.6692913385826773087, -0.1292274648535924053 ) ) ;
#1507 = CARTESIAN_POINT ( 'NONE',  ( -1.482939632545930975, 0.05413385826771666132, 0.4176697321401328100 ) ) ;
#1508 = CARTESIAN_POINT ( 'NONE',  ( -1.666666666666665853, 0.05413385826771626580, -0.4176697321401330321 ) ) ;
#1509 = ORIENTED_EDGE ( 'NONE', *, *, #33244, .T. ) ;
#1510 = CARTESIAN_POINT ( 'NONE',  ( 0.1070741851644054776, -0.3996062992125984925, -2.681758530183727895 ) ) ;
#1511 = CARTESIAN_POINT ( 'NONE',  ( -1.437007874015747477, 0.07958543189024071263, -0.2665933059059888421 ) ) ;
#1512 = CARTESIAN_POINT ( 'NONE',  ( -0.4330708661417315697, -0.6692913385826771977, 8.415575281601705876E-17 ) ) ;
#1513 = CARTESIAN_POINT ( 'NONE',  ( 0.7742782152230978099, -0.4281496062992124485, 0.4176697321401328655 ) ) ;
#1514 = CARTESIAN_POINT ( 'NONE',  ( -1.443569553805773564, -0.5023911411419708095, 0.1820866141732285504 ) ) ;
#1515 = CARTESIAN_POINT ( 'NONE',  ( -0.2925321140481932369, 0.2925321140481931259, -1.986220472440945128 ) ) ;
#1516 = CARTESIAN_POINT ( 'NONE',  ( -1.299212598425196097, -0.6692913385826771977, 8.415575281601705876E-17 ) ) ;
#1517 = CARTESIAN_POINT ( 'NONE',  ( 1.010498687664042716, -0.4281496062992124485, 0.4176697321401328655 ) ) ;
#1518 = CARTESIAN_POINT ( 'NONE',  ( 0.6299212598425204535, -0.1870078740157480879, -0.4822834645669291653 ) ) ;
#1519 = CARTESIAN_POINT ( 'NONE',  ( 1.076115485564305141, -0.6046776061558807314, 0.2411417322834647770 ) ) ;
#1520 = CARTESIAN_POINT ( 'NONE',  ( 0.3460692066303959202, -0.1998031496062991630, -0.9691601049868766582 ) ) ;
#1521 = CARTESIAN_POINT ( 'NONE',  ( -9.787531504996567848E-17, 0.3996062992125986035, -1.417322834645669216 ) ) ;
#1522 = CARTESIAN_POINT ( 'NONE',  ( 0.1058382717557499880, 0.3949938075777411073, -0.4658792650918635592 ) ) ;
#1523 = CARTESIAN_POINT ( 'NONE',  ( 0.2491324880211018833, 1.133662664435919787, -1.613879522126778543 ) ) ;
#1524 = CARTESIAN_POINT ( 'NONE',  ( 0.4265091863517067039, -0.5511811023622048555, -0.09757992244046775898 ) ) ;
#1525 = CARTESIAN_POINT ( 'NONE',  ( 0.1968503937007881344, 0.2952755905511811885, 0.000000000000000000 ) ) ;
#1526 = CARTESIAN_POINT ( 'NONE',  ( 1.299212598425197429, 0.2952755905511811885, 0.000000000000000000 ) ) ;
#1527 = CARTESIAN_POINT ( 'NONE',  ( -9.674558042662122972E-17, 0.3949938075777409963, -1.809055118110236560 ) ) ;
#1528 = CARTESIAN_POINT ( 'NONE',  ( 0.1771653543307093182, -0.4536011799217368745, -0.2665933059059886201 ) ) ;
#1529 = CARTESIAN_POINT ( 'NONE',  ( -0.7874015748031489847, -0.1870078740157480879, -0.4822834645669291653 ) ) ;
#1530 = CARTESIAN_POINT ( 'NONE',  ( 1.568241469816273437, -0.3162353388693405765, 0.4822834645669290543 ) ) ;
#1531 = CARTESIAN_POINT ( 'NONE',  ( 0.3477690288713918276, -0.6692913385826773087, -0.1292274648535924053 ) ) ;
#1532 = CARTESIAN_POINT ( 'NONE',  ( 0.1265901696524990294, -0.4724409448818896462, -1.975065616797900381 ) ) ;
#1533 = CARTESIAN_POINT ( 'NONE',  ( -0.7137454485294953965, 2.244094488188976388, -0.4917280318828581298 ) ) ;
#1534 = EDGE_LOOP ( 'NONE', ( #3579, #29369, #48090, #58856 ) ) ;
#1535 = ORIENTED_EDGE ( 'NONE', *, *, #67469, .T. ) ;
#1536 = CARTESIAN_POINT ( 'NONE',  ( 1.555118110236221041, -0.4536011799217367080, 0.2665933059059888421 ) ) ;
#1538 = CARTESIAN_POINT ( 'NONE',  ( -1.167979002624671470, 0.05413385826771666132, 0.4176697321401328100 ) ) ;
#1537 = CARTESIAN_POINT ( 'NONE',  ( -1.154855643044618851, 0.1283753931104748280, 0.1820866141732283561 ) ) ;
#1539 = CARTESIAN_POINT ( 'NONE',  ( 0.3392501089628018329, 0.1958661417322835052, -2.573471497866454794 ) ) ;
#1540 = CARTESIAN_POINT ( 'NONE',  ( -0.3996062992125984925, -0.1070741851644056858, -2.799868766404198794 ) ) ;
#1541 = CARTESIAN_POINT ( 'NONE',  ( -1.541994750656167090, -0.5511811023622048555, -0.09757992244046775898 ) ) ;
#1542 = CIRCLE ( 'NONE', #5549, 0.2165354330708660069 ) ;
#1543 = CARTESIAN_POINT ( 'NONE',  ( -1.233595800524933894, 0.2306618581243848609, 0.2411417322834645549 ) ) ;
#1544 = CARTESIAN_POINT ( 'NONE',  ( 0.2624671916010504757, -0.6046776061558809534, -0.2411417322834644161 ) ) ;
#1545 = CARTESIAN_POINT ( 'NONE',  ( -1.469816272965878357, 0.2306618581243848609, 0.2411417322834645549 ) ) ;
#1546 = CARTESIAN_POINT ( 'NONE',  ( -0.2867679344610366554, 0.2867679344610365444, -2.776883571357268821 ) ) ;
#1547 = ADVANCED_FACE ( 'NONE', ( #6606 ), #64907, .T. ) ;
#1548 = CARTESIAN_POINT ( 'NONE',  ( 0.8070866141732288002, 0.1660481256975885056, 0.3530559997133364547 ) ) ;
#1549 = CARTESIAN_POINT ( 'NONE',  ( 0.3917322834645670104, 2.398668435337828261E-17, -2.000000000000000000 ) ) ;
#1550 = CARTESIAN_POINT ( 'NONE',  ( -1.371391076115484609, -0.5511811023622046335, 0.09757992244046803654 ) ) ;
#1551 = ORIENTED_EDGE ( 'NONE', *, *, #64100, .T. ) ;
#1552 = CARTESIAN_POINT ( 'NONE',  ( 0.3420746716998660508, -0.1974969037888703871, -2.309711286089239035 ) ) ;
#1553 = ORIENTED_EDGE ( 'NONE', *, *, #33853, .T. ) ;
#1554 = CARTESIAN_POINT ( 'NONE',  ( -1.587926509186350810, -0.3690944881889763329, 0.3153832671262228327 ) ) ;
#1555 = CARTESIAN_POINT ( 'NONE',  ( -1.089238845144356427, 0.05413385826771666132, 0.4176697321401328100 ) ) ;
#1556 = CARTESIAN_POINT ( 'NONE',  ( -1.384514435695537005, -0.6692913385826773087, -0.1292274648535924053 ) ) ;
#1557 = CARTESIAN_POINT ( 'NONE',  ( -0.3996062992125986035, -7.340648628747425578E-17, -0.5118110236220472231 ) ) ;
#1558 = CARTESIAN_POINT ( 'NONE',  ( -1.476377952755905110, -0.5400638737290845981, -0.3530559997133363437 ) ) ;
#1559 = CARTESIAN_POINT ( 'NONE',  ( 1.019861537960135234, 1.617630162216313172, -0.4678516549211681474 ) ) ;
#1560 = CARTESIAN_POINT ( 'NONE',  ( -1.423884514435694859, -0.05778040916215560624, -0.4822834645669293319 ) ) ;
#1561 = CARTESIAN_POINT ( 'NONE',  ( -0.5411721830064186722, -2.191421614605370878E-15, 0.4445507791589071167 ) ) ;
#1562 = LINE ( 'NONE', #70580, #68456 ) ;
#1563 = EDGE_CURVE ( 'NONE', #58566, #38771, #73019, .T. ) ;
#1564 = CARTESIAN_POINT ( 'NONE',  ( 0.2427821522309719648, -0.08942795157527998196, 0.3641732283464567121 ) ) ;
#1565 = CARTESIAN_POINT ( 'NONE',  ( 0.4706608522957150820, 1.597527518877488450, 2.161121219943100691 ) ) ;
#1566 = CARTESIAN_POINT ( 'NONE',  ( 0.3917322834645670104, -0.1049643490035303411, -0.5111548556430445256 ) ) ;
#1567 = CARTESIAN_POINT ( 'NONE',  ( -0.5314960629921254842, -0.4536011799217368745, -0.2665933059059886201 ) ) ;
#1568 = CARTESIAN_POINT ( 'NONE',  ( -0.6496062992125976043, 0.1660481256975883668, -0.3530559997133364547 ) ) ;
#1569 = CARTESIAN_POINT ( 'NONE',  ( 1.082677165354331228, -0.5400638737290844871, 0.3530559997133364547 ) ) ;
#1570 = CARTESIAN_POINT ( 'NONE',  ( -0.8989501312335946848, -0.6692913385826771977, 0.1292274648535927661 ) ) ;
#1571 = VERTEX_POINT ( 'NONE', #58153 ) ;
#1572 = ORIENTED_EDGE ( 'NONE', *, *, #19166, .F. ) ;
#1573 = CARTESIAN_POINT ( 'NONE',  ( -1.023622047244093558, -0.1870078740157479769, 0.4822834645669291653 ) ) ;
#1574 = CARTESIAN_POINT ( 'NONE',  ( 0.6889763779527563470, 0.1660481256975883668, -0.3530559997133364547 ) ) ;
#1575 = CARTESIAN_POINT ( 'NONE',  ( -1.581364829396324945, -0.2845877964562159024, 0.3641732283464567677 ) ) ;
#1576 = CARTESIAN_POINT ( 'NONE',  ( -1.607611548556429737, -0.6692913385826771977, 0.1292274648535927661 ) ) ;
#1577 = CARTESIAN_POINT ( 'NONE',  ( 0.4091458600556403535, 0.2362204724409449896, -1.076115485564304475 ) ) ;
#1578 = CARTESIAN_POINT ( 'NONE',  ( -2.094141031015012366, 1.724409448818897905, 0.4359958488159718093 ) ) ;
#1579 = CARTESIAN_POINT ( 'NONE',  ( 4.797336870675656522E-17, -0.3917322834645670104, -0.3858267716535432879 ) ) ;
#1580 = CARTESIAN_POINT ( 'NONE',  ( -0.1958661417322836718, 0.3392501089628017219, -2.459973753280839670 ) ) ;
#1581 = CARTESIAN_POINT ( 'NONE',  ( -0.3871391076115476282, -0.05778040916215522460, 0.4822834645669289988 ) ) ;
#1582 = CARTESIAN_POINT ( 'NONE',  ( -1.384514435695537005, -0.5511811023622048555, -0.09757992244046775898 ) ) ;
#1583 = CARTESIAN_POINT ( 'NONE',  ( 0.2925321140481932369, -0.2925321140481931814, 0.1397637795275590289 ) ) ;
#1585 = CARTESIAN_POINT ( 'NONE',  ( 1.141392835773559211, 1.299212598425196985, 1.318558190104271333 ) ) ;
#1584 = CARTESIAN_POINT ( 'NONE',  ( -1.489501312335957062, -0.3162353388693409650, -0.4822834645669289433 ) ) ;
#1586 = CARTESIAN_POINT ( 'NONE',  ( -1.594488188976377563, -0.5400638737290844871, 0.3530559997133364547 ) ) ;
#1587 = CARTESIAN_POINT ( 'NONE',  ( -0.5118110236220466680, -0.6692913385826771977, 8.415575281601705876E-17 ) ) ;
#1588 = CARTESIAN_POINT ( 'NONE',  ( 0.1058382717557499880, 0.3949938075777409408, -2.589895013123359124 ) ) ;
#1589 = CARTESIAN_POINT ( 'NONE',  ( 0.5380577427821529035, -0.004921259842519870586, -0.3153832671262229437 ) ) ;
#1590 = LINE ( 'NONE', #65978, #22329 ) ;
#1591 = CARTESIAN_POINT ( 'NONE',  ( 0.1640419947506569498, -0.2845877964562161244, -0.3641732283464567121 ) ) ;
#1592 = CARTESIAN_POINT ( 'NONE',  ( 1.161417322834646271, 0.07958543189024071263, -0.2665933059059888421 ) ) ;
#1593 = CARTESIAN_POINT ( 'NONE',  ( 0.8661417322834652488, -0.1870078740157480879, -0.4822834645669291653 ) ) ;
#1594 = CARTESIAN_POINT ( 'NONE',  ( 0.1443569553805781891, -0.004921259842519870586, -0.3153832671262229437 ) ) ;
#1595 = CARTESIAN_POINT ( 'NONE',  ( 0.1049643490035303689, 0.3917322834645670104, -1.875328083989501460 ) ) ;
#1596 = CARTESIAN_POINT ( 'NONE',  ( -1.279527559055116948, 0.1660481256975883668, -0.3530559997133364547 ) ) ;
#1597 = CARTESIAN_POINT ( 'NONE',  ( -0.2230971128608915943, -0.3690944881889765550, -0.3153832671262227771 ) ) ;
#1598 = CARTESIAN_POINT ( 'NONE',  ( -1.157146581871515012E-16, 0.4724409448818898682, -0.3917322834645669549 ) ) ;
#1599 = CARTESIAN_POINT ( 'NONE',  ( -0.3477690288713902178, 0.1771653543307087075, -0.09757992244046823083 ) ) ;
#1600 = CARTESIAN_POINT ( 'NONE',  ( 0.01968503937007957949, -0.5400638737290845981, -0.3530559997133363437 ) ) ;
#1601 = CARTESIAN_POINT ( 'NONE',  ( 0.000000000000000000, 0.03937007874015747977, 0.000000000000000000 ) ) ;
#1602 = CARTESIAN_POINT ( 'NONE',  ( 1.049868766404200127, -0.5023911411419708095, -0.1820866141732282451 ) ) ;
#1603 = CARTESIAN_POINT ( 'NONE',  ( -0.3083989501312330295, -0.08942795157527998196, 0.3641732283464567121 ) ) ;
#1604 = CARTESIAN_POINT ( 'NONE',  ( -0.1115485564304453947, -0.6692913385826771977, 0.1292274648535927661 ) ) ;
#1605 = FACE_OUTER_BOUND ( 'NONE', #33008, .T. ) ;
#1606 = CARTESIAN_POINT ( 'NONE',  ( -1.305774278215222184, 0.1771653543307087630, 0.09757992244046791164 ) ) ;
#1607 = DIRECTION ( 'NONE',  ( 0.000000000000000000, -1.000000000000000000, 0.000000000000000000 ) ) ;
#1608 = CARTESIAN_POINT ( 'NONE',  ( 0.6955380577427828781, -0.4281496062992124485, 0.4176697321401328655 ) ) ;
#1609 = CARTESIAN_POINT ( 'NONE',  ( -0.7808398950131222316, -0.3162353388693409650, -0.4822834645669289433 ) ) ;
#1610 = CARTESIAN_POINT ( 'NONE',  ( -0.2925321140481932369, 0.2925321140481931259, -1.198818897637795367 ) ) ;
#1611 = CARTESIAN_POINT ( 'NONE',  ( -0.1049643490035302024, -0.3917322834645671215, -2.519028871391075786 ) ) ;
#1612 = CARTESIAN_POINT ( 'NONE',  ( 0.3215223097112867578, -0.08942795157527998196, 0.3641732283464567121 ) ) ;
#1613 = CARTESIAN_POINT ( 'NONE',  ( -0.9908136482939626788, 0.2952755905511811885, 0.1292274648535926551 ) ) ;
#1614 = CARTESIAN_POINT ( 'NONE',  ( -1.161417322834644716, 0.1660481256975885056, 0.3530559997133364547 ) ) ;
#1615 = CARTESIAN_POINT ( 'NONE',  ( -1.135170603674539924, 0.1771653543307087075, -0.09757992244046823083 ) ) ;
#1616 = CARTESIAN_POINT ( 'NONE',  ( 1.594488188976378673, -0.5400638737290845981, -0.3530559997133363437 ) ) ;
#1617 = CARTESIAN_POINT ( 'NONE',  ( -0.8005249343832011588, -0.004921259842519870586, -0.3153832671262229437 ) ) ;
#1618 = CARTESIAN_POINT ( 'NONE',  ( 0.5314960629920926216, 2.755905511811024056, 3.184294706754636106 ) ) ;
#1619 = CARTESIAN_POINT ( 'NONE',  ( 0.6758530183727039509, 0.2952755905511810774, -0.1292274648535930714 ) ) ;
#1620 = CARTESIAN_POINT ( 'NONE',  ( 0.2925321140481932369, -0.2925321140481932369, -0.2559055118110235560 ) ) ;
#1621 = CARTESIAN_POINT ( 'NONE',  ( -0.2867679344610367109, 0.2867679344610365444, -2.693588869587613566 ) ) ;
#1622 = CARTESIAN_POINT ( 'NONE',  ( 0.2952755905511810774, 3.616083068348483797E-17, 6.062992125984251857 ) ) ;
#1623 = CARTESIAN_POINT ( 'NONE',  ( -1.594488188976377563, -0.5400638737290844871, 0.3530559997133364547 ) ) ;
#1624 = CARTESIAN_POINT ( 'NONE',  ( -1.286089238845143479, -0.6046776061558807314, 0.2411417322834647770 ) ) ;
#1625 = CARTESIAN_POINT ( 'NONE',  ( 1.043307086614173818, -0.5400638737290845981, -0.3530559997133363437 ) ) ;
#1626 = CARTESIAN_POINT ( 'NONE',  ( 4.797336870675656522E-17, -0.3917322834645670104, -2.525590551181102317 ) ) ;
#1627 = CARTESIAN_POINT ( 'NONE',  ( 0.1181102362204724532, 0.09842519685039372024, 0.000000000000000000 ) ) ;
#1628 = CARTESIAN_POINT ( 'NONE',  ( 0.4068241469816281097, 0.05413385826771666132, 0.4176697321401328100 ) ) ;
#1629 = CARTESIAN_POINT ( 'NONE',  ( -0.5446194225721777693, -0.05778040916215522460, 0.4822834645669289988 ) ) ;
#1630 = CARTESIAN_POINT ( 'NONE',  ( 0.3567317632078913503, 1.224270319509463301, -3.920825516433590785 ) ) ;
#1631 = CARTESIAN_POINT ( 'NONE',  ( 4.893765752498283924E-17, -0.3996062992125986035, -1.968503937007873850 ) ) ;
#1632 = CARTESIAN_POINT ( 'NONE',  ( 0.6036745406824153282, -0.5023911411419708095, 0.1820866141732285504 ) ) ;
#1633 = CARTESIAN_POINT ( 'NONE',  ( -0.3996062992125986035, -7.340648628747425578E-17, -1.771653543307086576 ) ) ;
#1634 = ORIENTED_EDGE ( 'NONE', *, *, #46015, .T. ) ;
#1635 = CARTESIAN_POINT ( 'NONE',  ( 0.1049643490035304799, -0.3917322834645670104, -0.5544812580390570123 ) ) ;
#1636 = ORIENTED_EDGE ( 'NONE', *, *, #46095, .T. ) ;
#1637 = CARTESIAN_POINT ( 'NONE',  ( -0.05249343832020938322, -0.6046776061558809534, -0.2411417322834644161 ) ) ;
#1638 = PRODUCT_DEFINITION_SHAPE ( 'NONE', 'NONE',  #83319 ) ;
#1639 = CARTESIAN_POINT ( 'NONE',  ( 1.286089238845145033, 0.2306618581243848609, 0.2411417322834645549 ) ) ;
#1640 = CARTESIAN_POINT ( 'NONE',  ( 0.3608923884514443348, -0.6692913385826771977, 0.1292274648535927661 ) ) ;
#1641 = CARTESIAN_POINT ( 'NONE',  ( -0.2427821522309703550, -0.2845877964562159024, 0.3641732283464567677 ) ) ;
#1642 = CARTESIAN_POINT ( 'NONE',  ( 1.128608923884515169, -0.6046776061558809534, -0.2411417322834644161 ) ) ;
#1643 = CARTESIAN_POINT ( 'NONE',  ( -0.4986876640419939388, 0.2306618581243847221, -0.2411417322834647770 ) ) ;
#1644 = CARTESIAN_POINT ( 'NONE',  ( -0.1443569553805768291, 0.05413385826771666132, 0.4176697321401328100 ) ) ;
#1645 = CARTESIAN_POINT ( 'NONE',  ( -1.646981627296586703, -0.05778040916215522460, 0.4822834645669289988 ) ) ;
#1646 = CONICAL_SURFACE ( 'NONE', #8374, 1.220472440944881942, 0.7853981633974621568 ) ;
#1647 = CARTESIAN_POINT ( 'NONE',  ( 0.7152230971128614723, -0.3162353388693409650, -0.4822834645669289433 ) ) ;
#1648 = CARTESIAN_POINT ( 'NONE',  ( 1.286089238845145033, -0.6046776061558809534, -0.2411417322834644161 ) ) ;
#1649 = CARTESIAN_POINT ( 'NONE',  ( -0.1958661417322836718, 0.3392501089628017219, -0.6351706036745405903 ) ) ;
#1650 = CARTESIAN_POINT ( 'NONE',  ( 0.4986876640419954376, -0.5023911411419708095, -0.1820866141732282451 ) ) ;
#1651 = VERTEX_POINT ( 'NONE', #1773 ) ;
#1652 = CARTESIAN_POINT ( 'NONE',  ( 0.3420746716998660508, -0.1974969037888703871, -0.4199475065616798952 ) ) ;
#1653 = ORIENTED_EDGE ( 'NONE', *, *, #51709, .F. ) ;
#1654 = CARTESIAN_POINT ( 'NONE',  ( -0.6233595800524928121, -0.08942795157527998196, 0.3641732283464567121 ) ) ;
#1655 = CARTESIAN_POINT ( 'NONE',  ( -0.2493438320209966919, -0.4281496062992124485, 0.4176697321401328655 ) ) ;
#1656 = FACE_OUTER_BOUND ( 'NONE', #7657, .T. ) ;
#1657 = CARTESIAN_POINT ( 'NONE',  ( -0.2887139107611542133, 0.2306618581243848609, 0.2411417322834645549 ) ) ;
#1658 = CARTESIAN_POINT ( 'NONE',  ( -0.07874015748031421014, -0.1870078740157480879, -0.4822834645669291653 ) ) ;
#1659 = CARTESIAN_POINT ( 'NONE',  ( -0.9711286089238838626, 0.2306618581243847221, -0.2411417322834647770 ) ) ;
#1660 = CARTESIAN_POINT ( 'NONE',  ( -1.108923884514435132, -0.3162353388693405765, 0.4822834645669290543 ) ) ;
#1661 = CARTESIAN_POINT ( 'NONE',  ( 1.286089238845145033, -0.5023911411419708095, -0.1820866141732282451 ) ) ;
#1662 = FACE_OUTER_BOUND ( 'NONE', #12098, .T. ) ;
#1663 = CARTESIAN_POINT ( 'NONE',  ( -0.1450607720586916394, 0.000000000000000000, 0.3464511005275205946 ) ) ;
#1664 = CARTESIAN_POINT ( 'NONE',  ( 0.8464566929133865436, 0.07958543189024071263, -0.2665933059059888421 ) ) ;
#1665 = CARTESIAN_POINT ( 'NONE',  ( 0.2952755905511819101, 0.1660481256975883668, -0.3530559997133364547 ) ) ;
#1666 = CARTESIAN_POINT ( 'NONE',  ( 0.2559055118110243332, 0.1660481256975885056, 0.3530559997133364547 ) ) ;
#1667 = CARTESIAN_POINT ( 'NONE',  ( -0.1070741851644051862, -0.3996062992125987146, -1.174540682414698001 ) ) ;
#1668 = CARTESIAN_POINT ( 'NONE',  ( 0.6492324815748310440, 2.230753248847788139, 0.2292861212309488528 ) ) ;
#1669 = CARTESIAN_POINT ( 'NONE',  ( -0.3460692066303960313, 0.1998031496062989965, -0.5754593175853018883 ) ) ;
#1670 = CARTESIAN_POINT ( 'NONE',  ( -0.2925321140481930149, -0.2925321140481933480, -0.6082677165354329896 ) ) ;
#1671 = CARTESIAN_POINT ( 'NONE',  ( -0.7283464566929126471, 0.1660481256975883668, -0.3530559997133364547 ) ) ;
#1672 = CARTESIAN_POINT ( 'NONE',  ( 0.3458507752293908943, -0.3458507752293908943, 0.05905511811023620578 ) ) ;
#1673 = CARTESIAN_POINT ( 'NONE',  ( 0.1049643490035304938, -0.3917322834645669549, -1.902230971128608727 ) ) ;
#1674 = CARTESIAN_POINT ( 'NONE',  ( -1.266404199475064773, -0.08942795157528024563, -0.3641732283464568787 ) ) ;
#1675 = CARTESIAN_POINT ( 'NONE',  ( 0.9580052493438326877, 0.05413385826771666132, 0.4176697321401328100 ) ) ;
#1676 = CARTESIAN_POINT ( 'NONE',  ( 0.9383202099737538715, -0.05778040916215560624, -0.4822834645669293319 ) ) ;
#1677 = CARTESIAN_POINT ( 'NONE',  ( -0.1443569553805765515, -0.3690944881889765550, -0.3153832671262227771 ) ) ;
#1678 = CARTESIAN_POINT ( 'NONE',  ( 0.3871391076115492380, -0.05778040916215560624, -0.4822834645669293319 ) ) ;
#1679 = CARTESIAN_POINT ( 'NONE',  ( -1.157146581871515012E-16, 0.4724409448818898682, -1.809055118110236560 ) ) ;
#1680 = CARTESIAN_POINT ( 'NONE',  ( -0.03280839895013062252, 0.1771653543307087075, -0.09757992244046823083 ) ) ;
#1681 = CARTESIAN_POINT ( 'NONE',  ( 0.1115485564304467270, -0.6692913385826773087, -0.1292274648535924053 ) ) ;
#1682 = CARTESIAN_POINT ( 'NONE',  ( 4.837279021331061486E-17, -0.3949938075777409963, -1.572834645669291875 ) ) ;
#1683 = CARTESIAN_POINT ( 'NONE',  ( -1.646981627296586703, -0.3162353388693409650, -0.4822834645669289433 ) ) ;
#1684 = CARTESIAN_POINT ( 'NONE',  ( 0.4002624671916016896, -0.2845877964562161244, -0.3641732283464567121 ) ) ;
#1685 = CARTESIAN_POINT ( 'NONE',  ( 1.535433070866142558, 0.1771653543307087630, 0.000000000000000000 ) ) ;
#1687 = EDGE_CURVE ( 'NONE', #58735, #20676, #8090, .T. ) ;
#1686 = CARTESIAN_POINT ( 'NONE',  ( -0.9055118110236215490, 0.2952755905511811885, 0.000000000000000000 ) ) ;
#1688 = CARTESIAN_POINT ( 'NONE',  ( -0.1706036745406816491, -0.004921259842519870586, -0.3153832671262229437 ) ) ;
#1689 = DIRECTION ( 'NONE',  ( -3.491481338843132961E-15, -0.000000000000000000, 1.000000000000000000 ) ) ;
#1690 = CARTESIAN_POINT ( 'NONE',  ( -0.6692913385826764205, -0.6692913385826771977, 8.415575281601705876E-17 ) ) ;
#1691 = CARTESIAN_POINT ( 'NONE',  ( -0.5314960629921250401, 0.1660481256975885056, 0.3530559997133364547 ) ) ;
#1692 = CARTESIAN_POINT ( 'NONE',  ( -0.04593175853018302557, 0.2952755905511811885, 0.1292274648535926551 ) ) ;
#1693 = CARTESIAN_POINT ( 'NONE',  ( 0.3996062992125986035, -0.1070741851644052972, -2.708005249343832688 ) ) ;
#1694 = CARTESIAN_POINT ( 'NONE',  ( -0.1049643490035301746, -0.3917322834645670659, -1.884495119913699002 ) ) ;
#1695 = CARTESIAN_POINT ( 'NONE',  ( -1.541994750656167090, 0.1771653543307087630, 0.09757992244046791164 ) ) ;
#1696 = CARTESIAN_POINT ( 'NONE',  ( 0.9120734908136490793, 0.1771653543307087075, -0.09757992244046823083 ) ) ;
#1697 = CARTESIAN_POINT ( 'NONE',  ( 1.338582677165355062, -0.1870078740157480879, -0.4822834645669291653 ) ) ;
#1698 = CARTESIAN_POINT ( 'NONE',  ( -0.6167979002624665030, -0.004921259842519576551, 0.3153832671262227771 ) ) ;
#1699 = CARTESIAN_POINT ( 'NONE',  ( -1.240157480314959759, 0.07958543189024085140, 0.2665933059059887866 ) ) ;
#1700 = CIRCLE ( 'NONE', #48719, 3.937007874015748143 ) ;
#1701 = CARTESIAN_POINT ( 'NONE',  ( -0.6824146981627291497, -0.6046776061558809534, -0.2411417322834644161 ) ) ;
#1702 = CARTESIAN_POINT ( 'NONE',  ( 0.4396325459317593221, 0.1771653543307087075, -0.09757992244046823083 ) ) ;
#1703 = CARTESIAN_POINT ( 'NONE',  ( -0.2407525580057141290, 0.1709688663325618363, 5.655154502652836257 ) ) ;
#1704 = CARTESIAN_POINT ( 'NONE',  ( 0.9908136482939640111, 0.1771653543307087075, -0.09757992244046823083 ) ) ;
#1705 = ADVANCED_FACE ( 'NONE', ( #45099, #71223 ), #51837, .T. ) ;
#1706 = CARTESIAN_POINT ( 'NONE',  ( 0.5314960629921267055, -0.5400638737290844871, 0.3530559997133364547 ) ) ;
#1707 = EDGE_CURVE ( 'NONE', #26586, #5038, #58582, .T. ) ;
#1708 = CARTESIAN_POINT ( 'NONE',  ( 0.1070741851644054776, -0.3996062992125984925, -0.004593175853018378711 ) ) ;
#1709 = CARTESIAN_POINT ( 'NONE',  ( -0.4790026246719154557, -0.3162353388693405765, 0.4822834645669290543 ) ) ;
#1710 = CARTESIAN_POINT ( 'NONE',  ( 0.3392501089628018329, 0.1958661417322835607, -1.475721784776902856 ) ) ;
#1711 = CARTESIAN_POINT ( 'NONE',  ( 1.345144356955381593, -0.2845877964562161244, -0.3641732283464567121 ) ) ;
#1712 = CARTESIAN_POINT ( 'NONE',  ( 0.6496062992125991586, -0.5400638737290845981, -0.3530559997133363437 ) ) ;
#1713 = CARTESIAN_POINT ( 'NONE',  ( 0.1837270341207357105, -0.6046776061558809534, -0.2411417322834644161 ) ) ;
#1714 = CARTESIAN_POINT ( 'NONE',  ( -0.05249343832020911260, 0.1283753931104748280, 0.1820866141732283561 ) ) ;
#1715 = CARTESIAN_POINT ( 'NONE',  ( 1.113858370737683456, -1.206088964116209378E-16, 0.3791475997938230647 ) ) ;
#1716 = CARTESIAN_POINT ( 'NONE',  ( -0.1968503937007867743, 0.1771653543307087630, 0.000000000000000000 ) ) ;
#1717 = CARTESIAN_POINT ( 'NONE',  ( 0.8136482939632553313, -0.6046776061558809534, -0.2411417322834644161 ) ) ;
#1718 = CARTESIAN_POINT ( 'NONE',  ( -0.7939632545931754048, -0.2845877964562159024, 0.3641732283464567677 ) ) ;
#1719 = CARTESIAN_POINT ( 'NONE',  ( -1.095800524934382292, -0.3162353388693409650, -0.4822834645669289433 ) ) ;
#1720 = FACE_OUTER_BOUND ( 'NONE', #59119, .T. ) ;
#1721 = ORIENTED_EDGE ( 'NONE', *, *, #46438, .T. ) ;
#1722 = CARTESIAN_POINT ( 'NONE',  ( -1.345144356955379816, -0.3162353388693405765, 0.4822834645669290543 ) ) ;
#1723 = CARTESIAN_POINT ( 'NONE',  ( -1.076115485564303809, 0.1283753931104748280, 0.1820866141732283561 ) ) ;
#1724 = CARTESIAN_POINT ( 'NONE',  ( -0.1377952755905504645, 0.1660481256975885056, 0.3530559997133364547 ) ) ;
#1725 = CARTESIAN_POINT ( 'NONE',  ( -1.732283464566928277, -0.1870078740157479769, 0.4822834645669291653 ) ) ;
#1726 = CARTESIAN_POINT ( 'NONE',  ( -0.7545931758530176614, -0.6692913385826773087, -0.1292274648535924053 ) ) ;
#1727 =( BOUNDED_CURVE ( )  B_SPLINE_CURVE ( 2, ( #36399, #4412, #2768, #79802, #48608, #22118, #42290, #3177, #61664, #67987, #10332, #4005, #73479 ),
 .UNSPECIFIED., .F., .F. ) 
 B_SPLINE_CURVE_WITH_KNOTS ( ( 3, 2, 2, 2, 2, 2, 3 ),
 ( 0.2375000000000000167, 0.2416666666666666963, 0.2458333333333333204, 0.2500000000000000000, 0.2541666666666666519, 0.2583333333333333037, 0.2624999999999999556 ),
 .UNSPECIFIED. ) 
 CURVE ( )  GEOMETRIC_REPRESENTATION_ITEM ( )  RATIONAL_B_SPLINE_CURVE ( ( 0.9999999999999997780, 0.9659258262890685343, 1.000000000000000000, 0.9659258262890683122, 1.000000000000000000, 0.9659258262890683122, 1.000000000000000000, 0.9659258262890683122, 1.000000000000000000, 0.9659258262890683122, 1.000000000000000000, 0.9659258262890687563, 0.9999999999999995559 ) ) 
 REPRESENTATION_ITEM ( '' )  );
#1728 = FACE_OUTER_BOUND ( 'NONE', #20258, .T. ) ;
#1730 = CARTESIAN_POINT ( 'NONE',  ( 0.9317585301837276734, -0.4281496062992124485, 0.4176697321401328655 ) ) ;
#1729 = CARTESIAN_POINT ( 'NONE',  ( 1.679790026246720025, 0.2306618581243848609, 0.2411417322834645549 ) ) ;
#1731 = CARTESIAN_POINT ( 'NONE',  ( 0.9842519685039378130, -0.6692913385826771977, 8.415575281601705876E-17 ) ) ;
#1732 = CARTESIAN_POINT ( 'NONE',  ( 0.1958661417322834775, 0.3392501089628018884, -2.341207349081364963 ) ) ;
#1733 = FACE_OUTER_BOUND ( 'NONE', #53462, .T. ) ;
#1734 = CARTESIAN_POINT ( 'NONE',  ( -1.364829396325458521, 0.2306618581243847221, -0.2411417322834647770 ) ) ;
#1735 = CARTESIAN_POINT ( 'NONE',  ( 0.1998031496062994405, -0.3460692066303958092, -0.09186351706036746667 ) ) ;
#1736 = ORIENTED_EDGE ( 'NONE', *, *, #32413, .F. ) ;
#1737 = CARTESIAN_POINT ( 'NONE',  ( -0.5380577427821514602, -0.004921259842519576551, 0.3153832671262227771 ) ) ;
#1738 = CARTESIAN_POINT ( 'NONE',  ( 0.2867679344610365999, 0.2867679344610365999, -1.862204724409449064 ) ) ;
#1739 = ORIENTED_EDGE ( 'NONE', *, *, #20141, .T. ) ;
#1740 = CARTESIAN_POINT ( 'NONE',  ( 0.4133858267716541968, -0.5400638737290845981, -0.3530559997133363437 ) ) ;
#1741 = CARTESIAN_POINT ( 'NONE',  ( -0.03937007874015669567, -0.6692913385826771977, 8.415575281601705876E-17 ) ) ;
#1742 = CARTESIAN_POINT ( 'NONE',  ( -0.7414698162729651543, -0.6692913385826771977, 0.1292274648535927661 ) ) ;
#1743 = CARTESIAN_POINT ( 'NONE',  ( 1.437007874015748810, -0.5400638737290845981, -0.3530559997133363437 ) ) ;
#1744 = CARTESIAN_POINT ( 'NONE',  ( -1.023622047244093558, -0.1870078740157479769, 0.3641732283464567677 ) ) ;
#1745 = CARTESIAN_POINT ( 'NONE',  ( -0.4562819726585397584, 1.668167360224330098, -2.594269413088675424 ) ) ;
#1746 = CARTESIAN_POINT ( 'NONE',  ( 0.8136482939632553313, -0.6046776061558809534, -0.2411417322834644161 ) ) ;
#1747 = CARTESIAN_POINT ( 'NONE',  ( 0.5314960629921264834, 0.07958543189024071263, -0.2665933059059888421 ) ) ;
#1748 = CARTESIAN_POINT ( 'NONE',  ( -0.3280839895013117347, 0.05413385826771626580, -0.4176697321401330321 ) ) ;
#1749 = CARTESIAN_POINT ( 'NONE',  ( -9.594673741351310580E-17, 0.3917322834645669549, -1.182395382380890592 ) ) ;
#1750 = CARTESIAN_POINT ( 'NONE',  ( -0.6364829396325453192, -0.05778040916215560624, -0.4822834645669293319 ) ) ;
#1751 = CARTESIAN_POINT ( 'NONE',  ( -1.640419947506561060, -0.3690944881889765550, -0.3153832671262227771 ) ) ;
#1752 = CARTESIAN_POINT ( 'NONE',  ( 1.555118110236221041, 0.1660481256975883668, -0.3530559997133364547 ) ) ;
#1753 = CYLINDRICAL_SURFACE ( 'NONE', #53035, 0.1771653543307088186 ) ;
#1754 = VERTEX_POINT ( 'NONE', #46787 ) ;
#1755 = CARTESIAN_POINT ( 'NONE',  ( 0.2867679344610366554, 0.2867679344610366554, -2.496738475886826070 ) ) ;
#1756 = CARTESIAN_POINT ( 'NONE',  ( 0.02624671916010564918, -0.6046776061558809534, -0.2411417322834644161 ) ) ;
#1757 = VERTEX_POINT ( 'NONE', #65338 ) ;
#1758 = CARTESIAN_POINT ( 'NONE',  ( -1.377952755905511140, 0.2952755905511811885, 0.000000000000000000 ) ) ;
#1759 = CARTESIAN_POINT ( 'NONE',  ( 1.030183727034121421, -0.3162353388693409650, -0.4822834645669289433 ) ) ;
#1760 = CARTESIAN_POINT ( 'NONE',  ( 1.463254593175853824, 0.2952755905511810774, -0.1292274648535930714 ) ) ;
#1761 = CARTESIAN_POINT ( 'NONE',  ( 0.3937007874015754361, -0.1870078740157480879, -0.4822834645669291653 ) ) ;
#1762 = CARTESIAN_POINT ( 'NONE',  ( -0.4724409448818890911, -0.1870078740157480879, -0.4822834645669291653 ) ) ;
#1763 = CARTESIAN_POINT ( 'NONE',  ( -0.2867679344610365999, 0.2867679344610364889, -1.994094488188976610 ) ) ;
#1764 = CARTESIAN_POINT ( 'NONE',  ( -1.233595800524933894, 0.2306618581243848609, 0.2411417322834645549 ) ) ;
#1765 = CARTESIAN_POINT ( 'NONE',  ( -0.4855643044619415427, 0.05413385826771626580, -0.4176697321401330321 ) ) ;
#1766 = CARTESIAN_POINT ( 'NONE',  ( -0.5183727034120726440, 0.1771653543307087630, 0.09757992244046791164 ) ) ;
#1767 = CYLINDRICAL_SURFACE ( 'NONE', #31510, 0.4724409448818898682 ) ;
#1768 = CARTESIAN_POINT ( 'NONE',  ( -0.6889763779527552368, -0.5400638737290845981, -0.3530559997133363437 ) ) ;
#1769 = CARTESIAN_POINT ( 'NONE',  ( -0.5314960629921394730, 2.739927440807262915, 3.869764100875847213 ) ) ;
#1770 = ADVANCED_FACE ( 'NONE', ( #38806 ), #5298, .F. ) ;
#1771 = CARTESIAN_POINT ( 'NONE',  ( 0.5774278215223103139, -0.6046776061558809534, -0.2411417322834644161 ) ) ;
#1772 = CARTESIAN_POINT ( 'NONE',  ( 0.3996062992125986590, -0.1070741851644053111, -2.001312335958005395 ) ) ;
#1773 = CARTESIAN_POINT ( 'NONE',  ( -0.8761506516392493227, -2.567464376874931580E-15, -0.4445507791589072832 ) ) ;
#1774 = CARTESIAN_POINT ( 'NONE',  ( 0.05905511811023709395, -0.5400638737290844871, 0.3530559997133364547 ) ) ;
#1776 = CARTESIAN_POINT ( 'NONE',  ( -2.362204724409448620, 1.724409448818897905, -2.474278114140802984E-14 ) ) ;
#1775 = CARTESIAN_POINT ( 'NONE',  ( 0.8398950131233602345, -0.5023911411419708095, 0.1820866141732285504 ) ) ;
#1777 = CARTESIAN_POINT ( 'NONE',  ( 0.4724409448818898682, 2.892866454678787531E-17, -0.6673228346456693272 ) ) ;
#1778 = CARTESIAN_POINT ( 'NONE',  ( 1.194225721784777594, -0.004921259842519576551, 0.3153832671262227771 ) ) ;
#1779 = CARTESIAN_POINT ( 'NONE',  ( 1.384514435695538337, -0.6692913385826771977, 0.1292274648535927661 ) ) ;
#1780 = CARTESIAN_POINT ( 'NONE',  ( 0.1974969037888706092, -0.3420746716998660508, -0.01115485564304462274 ) ) ;
#1781 = CARTESIAN_POINT ( 'NONE',  ( 0.1246719160104994284, -0.6692913385826771977, 0.1292274648535927661 ) ) ;
#1782 = DIRECTION ( 'NONE',  ( -0.000000000000000000, 1.000000000000000000, 0.000000000000000000 ) ) ;
#1783 = CARTESIAN_POINT ( 'NONE',  ( -1.377952755905511140, 0.2952755905511811885, 0.000000000000000000 ) ) ;
#1784 = CARTESIAN_POINT ( 'NONE',  ( -0.03280839895013062252, -0.6692913385826771977, 0.1292274648535927661 ) ) ;
#1785 = CARTESIAN_POINT ( 'NONE',  ( -0.1058382717557497660, -0.3949938075777411073, -0.4639107611548556331 ) ) ;
#1786 = CARTESIAN_POINT ( 'NONE',  ( 1.213910761154856299, 0.2952755905511811885, 0.1292274648535926551 ) ) ;
#1787 = CARTESIAN_POINT ( 'NONE',  ( 0.4068241469816279987, -0.4281496062992127816, -0.4176697321401328100 ) ) ;
#1788 = CARTESIAN_POINT ( 'NONE',  ( 0.9514435695538062676, -0.2845877964562161244, -0.3641732283464567121 ) ) ;
#1789 = FACE_OUTER_BOUND ( 'NONE', #58870, .T. ) ;
#1790 = CARTESIAN_POINT ( 'NONE',  ( 0.3215223097112867578, -0.2845877964562161244, -0.3641732283464567121 ) ) ;
#1791 = CARTESIAN_POINT ( 'NONE',  ( -1.437007874015747477, 0.1660481256975883668, -0.3530559997133364547 ) ) ;
#1792 = CARTESIAN_POINT ( 'NONE',  ( 0.2925321140481932369, -0.2925321140481931814, -0.9625984251968502381 ) ) ;
#1793 = CARTESIAN_POINT ( 'NONE',  ( 1.154855643044620184, -0.6046776061558807314, 0.2411417322834647770 ) ) ;
#1794 = CARTESIAN_POINT ( 'NONE',  ( -0.1958661417322834220, -0.3392501089628018884, -0.6876640419947506189 ) ) ;
#1796 = CARTESIAN_POINT ( 'NONE',  ( 0.9186351706036752773, 0.2306618581243847221, -0.2411417322834647770 ) ) ;
#1795 = CARTESIAN_POINT ( 'NONE',  ( 0.4986876640419954376, -0.6046776061558809534, -0.2411417322834644161 ) ) ;
#1797 = CARTESIAN_POINT ( 'NONE',  ( -0.5120078740157480990, 6.270288040516270789E-17, -1.512162153811850596 ) ) ;
#1798 = CARTESIAN_POINT ( 'NONE',  ( 0.3280839895013130669, -0.004921259842519576551, 0.3153832671262227771 ) ) ;
#1799 = CARTESIAN_POINT ( 'NONE',  ( 0.3871391076115493490, -0.3162353388693405765, 0.4822834645669290543 ) ) ;
#1800 = CARTESIAN_POINT ( 'NONE',  ( 0.7749820319012125092, 2.784432375088962958E-17, -0.3464511005275205946 ) ) ;
#1801 = CARTESIAN_POINT ( 'NONE',  ( -1.003937007874015297, -0.4536011799217368745, -0.2665933059059886201 ) ) ;
#1802 = CARTESIAN_POINT ( 'NONE',  ( -0.8989501312335946848, 0.2952755905511810774, -0.1292274648535930714 ) ) ;
#1803 = AXIS2_PLACEMENT_3D ( 'NONE', #45032, #46717, #40005 ) ;
#1804 = CARTESIAN_POINT ( 'NONE',  ( -1.391076115485563758, 0.2306618581243848609, 0.2411417322834645549 ) ) ;
#1805 = CARTESIAN_POINT ( 'NONE',  ( 0.4527559055118117182, 0.1660481256975883668, -0.3530559997133364547 ) ) ;
#1806 = CARTESIAN_POINT ( 'NONE',  ( 1.587926509186352586, -0.4281496062992127816, -0.4176697321401328100 ) ) ;
#1807 = CARTESIAN_POINT ( 'NONE',  ( 1.087314056648182925, 1.152187173028865974, -0.2773278579668389532 ) ) ;
#1808 = CARTESIAN_POINT ( 'NONE',  ( 0.6036745406824153282, -0.6046776061558807314, 0.2411417322834647770 ) ) ;
#1809 = CARTESIAN_POINT ( 'NONE',  ( 0.3996062992125985480, 2.446882876249141654E-17, 0.1200787401574802959 ) ) ;
#1810 = FACE_OUTER_BOUND ( 'NONE', #51817, .T. ) ;
#1811 = CARTESIAN_POINT ( 'NONE',  ( 1.555118110236221041, 0.1660481256975883668, -0.3530559997133364547 ) ) ;
#1812 = CARTESIAN_POINT ( 'NONE',  ( -1.476377952755905110, -0.4536011799217368745, -0.2665933059059886201 ) ) ;
#1813 = CARTESIAN_POINT ( 'NONE',  ( 1.010498687664042716, -0.3690944881889763329, 0.3153832671262228327 ) ) ;
#1814 = CARTESIAN_POINT ( 'NONE',  ( -1.305774278215222184, 0.1771653543307087630, 0.09757992244046791164 ) ) ;
#1815 = CARTESIAN_POINT ( 'NONE',  ( -0.6955380577427815458, -0.004921259842519576551, 0.3153832671262227771 ) ) ;
#1816 = CARTESIAN_POINT ( 'NONE',  ( -0.4724409448818898682, -8.678599364036362592E-17, -2.086614173228346303 ) ) ;
#1817 = CARTESIAN_POINT ( 'NONE',  ( 0.5249343832021003964, 0.1283753931104746893, -0.1820866141732285504 ) ) ;
#1818 = CIRCLE ( 'NONE', #70341, 0.3149606299212598381 ) ;
#1819 = CARTESIAN_POINT ( 'NONE',  ( 0.4068241469816281097, 0.05413385826771666132, 0.4176697321401328100 ) ) ;
#1820 = CARTESIAN_POINT ( 'NONE',  ( 1.220472440944882386, -0.6692913385826771977, 8.415575281601705876E-17 ) ) ;
#1821 = ADVANCED_FACE ( 'NONE', ( #64482 ), #46366, .F. ) ;
#1822 = CARTESIAN_POINT ( 'NONE',  ( 0.1377952755905518800, 0.1660481256975883668, -0.3530559997133364547 ) ) ;
#1823 = CARTESIAN_POINT ( 'NONE',  ( 0.03937007874015806264, 0.1771653543307087630, 0.000000000000000000 ) ) ;
#1824 = CARTESIAN_POINT ( 'NONE',  ( 1.272965879265092637, 0.05413385826771666132, 0.4176697321401328100 ) ) ;
#1825 = CARTESIAN_POINT ( 'NONE',  ( -0.1702530392988850783, 0.004960608223778509643, -0.3437734562760191848 ) ) ;
#1826 = CARTESIAN_POINT ( 'NONE',  ( -0.9251968503937002541, 0.1660481256975885056, 0.3530559997133364547 ) ) ;
#1827 = CARTESIAN_POINT ( 'NONE',  ( 0.1070741851644053666, 0.3996062992125986035, -0.6233595800524933672 ) ) ;
#1828 = CARTESIAN_POINT ( 'NONE',  ( 2.795275590551181466, 1.968503937007874960, 0.000000000000000000 ) ) ;
#1829 = CARTESIAN_POINT ( 'NONE',  ( -0.006561679790025524116, -0.3162353388693405765, 0.4822834645669290543 ) ) ;
#1830 = CARTESIAN_POINT ( 'NONE',  ( -0.9908136482939626788, 0.2952755905511811885, 0.1292274648535926551 ) ) ;
#1831 = CARTESIAN_POINT ( 'NONE',  ( 0.03937007874015806264, 0.2952755905511811885, 0.000000000000000000 ) ) ;
#1832 = EDGE_CURVE ( 'NONE', #2851, #40183, #25750, .T. ) ;
#1833 = CARTESIAN_POINT ( 'NONE',  ( -0.3460692066303958092, -0.1998031496062994683, -2.414698162729658648 ) ) ;
#1834 = CARTESIAN_POINT ( 'NONE',  ( -0.3420746716998661618, 0.1974969037888702206, -1.758530183727034180 ) ) ;
#1835 = CARTESIAN_POINT ( 'NONE',  ( 0.3917322834645669549, 0.1049643490035304660, -0.7467191601049868455 ) ) ;
#1836 = DIRECTION ( 'NONE',  ( -0.000000000000000000, -1.000000000000000000, -0.000000000000000000 ) ) ;
#1837 = ADVANCED_FACE ( 'NONE', ( #71639 ), #72478, .F. ) ;
#1838 = CARTESIAN_POINT ( 'NONE',  ( -1.377952755905511140, 0.1771653543307087630, 0.000000000000000000 ) ) ;
#1839 = CARTESIAN_POINT ( 'NONE',  ( 4.797336870675656522E-17, -0.3917322834645670104, -1.015748031496062964 ) ) ;
#1840 = CARTESIAN_POINT ( 'NONE',  ( -1.646981627296586703, -0.3162353388693409650, -0.4822834645669289433 ) ) ;
#1841 = CARTESIAN_POINT ( 'NONE',  ( 0.1049643490035303689, 0.3917322834645668994, -0.07347149786645487679 ) ) ;
#1842 = CARTESIAN_POINT ( 'NONE',  ( 0.4396325459317593221, 0.2952755905511810774, -0.1292274648535930714 ) ) ;
#1843 = CARTESIAN_POINT ( 'NONE',  ( -0.5643044619422565855, -0.004921259842519870586, -0.3153832671262229437 ) ) ;
#1844 = CARTESIAN_POINT ( 'NONE',  ( 0.8464566929133865436, 0.1660481256975883668, -0.3530559997133364547 ) ) ;
#1845 = CARTESIAN_POINT ( 'NONE',  ( 0.2230971128608929543, 0.05413385826771626580, -0.4176697321401330321 ) ) ;
#1846 = CARTESIAN_POINT ( 'NONE',  ( -0.4724409448818898682, -8.678599364036362592E-17, -0.1161417322834645827 ) ) ;
#1847 = CARTESIAN_POINT ( 'NONE',  ( 0.1998031496062994405, -0.3460692066303958092, -2.611548556430446144 ) ) ;
#1848 = CARTESIAN_POINT ( 'NONE',  ( -0.1958661417322833942, -0.3392501089628018884, -1.322197793472127625 ) ) ;
#1849 = CARTESIAN_POINT ( 'NONE',  ( 1.371391076115485941, 0.2952755905511811885, 0.1292274648535926551 ) ) ;
#1850 = CARTESIAN_POINT ( 'NONE',  ( -0.1246719160104980823, 0.2952755905511811885, 0.1292274648535926551 ) ) ;
#1851 = CARTESIAN_POINT ( 'NONE',  ( -1.555118110236219930, -0.5400638737290845981, -0.3530559997133363437 ) ) ;
#1852 = CARTESIAN_POINT ( 'NONE',  ( 0.8595800524934390507, -0.3162353388693405765, 0.4822834645669290543 ) ) ;
#1853 = CARTESIAN_POINT ( 'NONE',  ( -0.3917322834645670104, -7.196005306013484475E-17, -0.4389763779527560139 ) ) ;
#1854 = CARTESIAN_POINT ( 'NONE',  ( 0.2690288713910767848, -0.6692913385826773087, -0.1292274648535924053 ) ) ;
#1855 = CARTESIAN_POINT ( 'NONE',  ( 0.8464566929133866546, -0.5400638737290844871, 0.3530559997133364547 ) ) ;
#1856 = CARTESIAN_POINT ( 'NONE',  ( -0.2230971128608915943, 0.05413385826771666132, 0.4176697321401328100 ) ) ;
#1857 = CARTESIAN_POINT ( 'NONE',  ( 0.6627296587926517768, -0.5511811023622048555, -0.09757992244046775898 ) ) ;
#1858 = CARTESIAN_POINT ( 'NONE',  ( -1.167979002624671470, -0.4281496062992127816, -0.4176697321401328100 ) ) ;
#1859 = CARTESIAN_POINT ( 'NONE',  ( -1.279527559055116948, -0.5400638737290844871, 0.3530559997133364547 ) ) ;
#1860 = CARTESIAN_POINT ( 'NONE',  ( 0.7545931758530188826, -0.6692913385826771977, 0.1292274648535927661 ) ) ;
#1861 = LINE ( 'NONE', #14911, #80277 ) ;
#1862 = EDGE_CURVE ( 'NONE', #53393, #21631, #12276, .T. ) ;
#1863 = CARTESIAN_POINT ( 'NONE',  ( -0.1958661417322836718, 0.3392501089628017219, -1.895013123359580165 ) ) ;
#1864 = ORIENTED_EDGE ( 'NONE', *, *, #35126, .T. ) ;
#1865 = CARTESIAN_POINT ( 'NONE',  ( -0.1070741851644051862, -0.3996062992125987146, -0.3871391076115485719 ) ) ;
#1866 = ORIENTED_EDGE ( 'NONE', *, *, #27189, .T. ) ;
#1867 = CARTESIAN_POINT ( 'NONE',  ( 1.246719160104987623, 0.05413385826771626580, -0.4176697321401330321 ) ) ;
#1868 = CARTESIAN_POINT ( 'NONE',  ( 1.023622047244095112, -0.1870078740157480601, -0.3641732283464567677 ) ) ;
#1869 = LINE ( 'NONE', #27531, #11538 ) ;
#1870 = CARTESIAN_POINT ( 'NONE',  ( -0.03178304480585582292, 0.3983403474834776858, -2.755905511811024500 ) ) ;
#1871 = DIRECTION ( 'NONE',  ( -0.000000000000000000, -1.000000000000000000, -0.000000000000000000 ) ) ;
#1872 = CARTESIAN_POINT ( 'NONE',  ( -0.3917322834645670104, -7.196005306013484475E-17, -1.383858267716535417 ) ) ;
#1873 = EDGE_CURVE ( 'NONE', #60349, #22261, #70553, .T. ) ;
#1874 = VECTOR ( 'NONE', #6880, 39.37007874015748143 ) ;
#1875 = CARTESIAN_POINT ( 'NONE',  ( 1.502624671916010790, -0.3162353388693409650, -0.4822834645669289433 ) ) ;
#1876 = CARTESIAN_POINT ( 'NONE',  ( 0.4615285972131335512, 1.648351240186696431, -3.909863522152617232 ) ) ;
#1877 = CARTESIAN_POINT ( 'NONE',  ( -0.5183727034120726440, -0.6692913385826773087, -0.1292274648535924053 ) ) ;
#1878 = CARTESIAN_POINT ( 'NONE',  ( 0.9645669291338588858, 0.1660481256975885056, 0.3530559997133364547 ) ) ;
#1879 = VERTEX_POINT ( 'NONE', #17206 ) ;
#1880 = CARTESIAN_POINT ( 'NONE',  ( -1.535433070866141225, 0.2952755905511811885, 0.000000000000000000 ) ) ;
#1881 = CARTESIAN_POINT ( 'NONE',  ( 0.5027385518326215053, 1.496062992125283708, 0.5309055118110234117 ) ) ;
#1882 = DIRECTION ( 'NONE',  ( 1.047444401652940007E-14, 0.000000000000000000, -1.000000000000000000 ) ) ;
#1883 = CARTESIAN_POINT ( 'NONE',  ( 1.502624671916010790, -0.08942795157527998196, 0.3641732283464567121 ) ) ;
#1884 = CARTESIAN_POINT ( 'NONE',  ( -1.603475055217291612, 1.881749232079046097, -0.04573490813648262154 ) ) ;
#1885 = CARTESIAN_POINT ( 'NONE',  ( -0.7677165354330699465, -0.4536011799217368745, -0.2665933059059886201 ) ) ;
#1886 = CARTESIAN_POINT ( 'NONE',  ( -1.594488188976377119, 0.1660481256975883668, -0.3530559997133364547 ) ) ;
#1887 = CARTESIAN_POINT ( 'NONE',  ( 0.4396325459317593221, 0.2952755905511810774, -0.1292274648535930714 ) ) ;
#1888 = ORIENTED_EDGE ( 'NONE', *, *, #11147, .T. ) ;
#1890 = CARTESIAN_POINT ( 'NONE',  ( -1.854472803289052507, 2.716535433070866645, 0.5314960629921260393 ) ) ;
#1889 = CARTESIAN_POINT ( 'NONE',  ( 1.502624671916010790, -0.05778040916215522460, 0.4822834645669289988 ) ) ;
#1891 = CARTESIAN_POINT ( 'NONE',  ( -0.7677165354330699465, 0.07958543189024085140, 0.2665933059059887866 ) ) ;
#1892 = CARTESIAN_POINT ( 'NONE',  ( 0.9186351706036752773, 0.2306618581243847221, -0.2411417322834647770 ) ) ;
#1893 = CARTESIAN_POINT ( 'NONE',  ( -1.660104986876639543, -0.05778040916215560624, -0.4822834645669293319 ) ) ;
#1894 = CARTESIAN_POINT ( 'NONE',  ( 0.3392501089628018329, -0.1958661417322834497, -1.129901944060680563 ) ) ;
#1895 = CARTESIAN_POINT ( 'NONE',  ( -0.7677165354330699465, 0.07958543189024085140, 0.2665933059059887866 ) ) ;
#1896 = CARTESIAN_POINT ( 'NONE',  ( 1.640419947506562393, -0.4281496062992124485, 0.4176697321401328655 ) ) ;
#1897 = CARTESIAN_POINT ( 'NONE',  ( 0.1265901696524989184, 0.4724409448818898127, -0.7808398950131233418 ) ) ;
#1898 = CARTESIAN_POINT ( 'NONE',  ( 0.5380577427821529035, 0.05413385826771626580, -0.4176697321401330321 ) ) ;
#1899 = CARTESIAN_POINT ( 'NONE',  ( -0.9186351706036736120, -0.5023911411419708095, -0.1820866141732282451 ) ) ;
#1900 = CARTESIAN_POINT ( 'NONE',  ( -0.4921259842519677963, -0.4536011799217367080, 0.2665933059059888421 ) ) ;
#1901 = CARTESIAN_POINT ( 'NONE',  ( -0.2427821522309703550, -0.05778040916215560624, -0.4822834645669293319 ) ) ;
#1902 = CARTESIAN_POINT ( 'NONE',  ( -1.220472440944881054, -0.5511811023622047445, 6.969142054262312111E-17 ) ) ;
#1903 = CARTESIAN_POINT ( 'NONE',  ( -0.3917322834645671770, 0.1049643490035302024, -0.1870271897975872011 ) ) ;
#1904 = CARTESIAN_POINT ( 'NONE',  ( 0.6299212598425204535, -0.1870078740157479769, 0.4822834645669291653 ) ) ;
#1905 = CARTESIAN_POINT ( 'NONE',  ( 0.8772393894194432384, 4.512065407040659715E-16, 0.3954985857520057491 ) ) ;
#1906 = CARTESIAN_POINT ( 'NONE',  ( -0.1265901696524993347, 0.4724409448818895907, -1.815616797900262425 ) ) ;
#1907 = CARTESIAN_POINT ( 'NONE',  ( -0.8595800524934373854, -0.3162353388693409650, -0.4822834645669289433 ) ) ;
#1908 = CARTESIAN_POINT ( 'NONE',  ( -0.08530183727034056085, -0.08942795157528024563, -0.3641732283464568787 ) ) ;
#1909 = CARTESIAN_POINT ( 'NONE',  ( -1.364829396325458521, -0.6046776061558807314, 0.2411417322834647770 ) ) ;
#1910 = CARTESIAN_POINT ( 'NONE',  ( 1.030183727034121421, -0.08942795157527998196, 0.3641732283464567121 ) ) ;
#1911 = CARTESIAN_POINT ( 'NONE',  ( -0.6036745406824141069, 0.1283753931104748280, 0.1820866141732283561 ) ) ;
#1912 = CARTESIAN_POINT ( 'NONE',  ( -1.115485564304461219, -0.4281496062992124485, 0.4176697321401328655 ) ) ;
#1913 = CARTESIAN_POINT ( 'NONE',  ( -1.502624671916009680, -0.05778040916215560624, -0.4822834645669293319 ) ) ;
#1914 = CARTESIAN_POINT ( 'NONE',  ( -1.587926509186350810, 0.05413385826771626580, -0.4176697321401330321 ) ) ;
#1915 = FACE_OUTER_BOUND ( 'NONE', #60545, .T. ) ;
#1916 = CARTESIAN_POINT ( 'NONE',  ( 0.8923884514435703741, 0.1283753931104748280, 0.1820866141732283561 ) ) ;
#1917 = VECTOR ( 'NONE', #49053, 39.37007874015748854 ) ;
#1918 = CARTESIAN_POINT ( 'NONE',  ( 0.5643044619422579178, 0.05413385826771666132, 0.4176697321401328100 ) ) ;
#1919 = CARTESIAN_POINT ( 'NONE',  ( -1.568241469816272105, -0.3162353388693409650, -0.4822834645669289433 ) ) ;
#1920 = CARTESIAN_POINT ( 'NONE',  ( 1.299212598425197429, 0.1771653543307087630, 0.000000000000000000 ) ) ;
#1921 = ORIENTED_EDGE ( 'NONE', *, *, #43859, .F. ) ;
#1922 = CARTESIAN_POINT ( 'NONE',  ( -0.3949938075777409963, -7.255918531996591613E-17, 0.1988188976377952832 ) ) ;
#1923 = CARTESIAN_POINT ( 'NONE',  ( -1.318897637795274802, 0.07958543189024085140, 0.2665933059059887866 ) ) ;
#1924 = CARTESIAN_POINT ( 'NONE',  ( -0.5905511811023613777, -0.6692913385826771977, 8.415575281601705876E-17 ) ) ;
#1925 = CARTESIAN_POINT ( 'NONE',  ( 0.3805774278215230400, 0.05413385826771626580, -0.4176697321401330321 ) ) ;
#1926 = CARTESIAN_POINT ( 'NONE',  ( -1.555118110236219930, 0.07958543189024085140, 0.2665933059059887866 ) ) ;
#1927 = CARTESIAN_POINT ( 'NONE',  ( 0.3460692066303959202, -0.1998031496062991630, -1.914041994750656395 ) ) ;
#1928 = CARTESIAN_POINT ( 'NONE',  ( -1.364829396325458521, 0.2306618581243847221, -0.2411417322834647770 ) ) ;
#1929 = CARTESIAN_POINT ( 'NONE',  ( 0.4986876640419954376, -0.6046776061558809534, -0.2411417322834644161 ) ) ;
#1930 = CARTESIAN_POINT ( 'NONE',  ( -0.05905511811023545637, 0.1660481256975885056, 0.3530559997133364547 ) ) ;
#1931 = CARTESIAN_POINT ( 'NONE',  ( 1.292650918635171564, 0.2952755905511811885, 0.1292274648535926551 ) ) ;
#1933 = EDGE_CURVE ( 'NONE', #33346, #9070, #6605, .T. ) ;
#1932 = CARTESIAN_POINT ( 'NONE',  ( -0.3996062992125986035, 0.1070741851644051584, -1.211942257217847541 ) ) ;
#1934 = CARTESIAN_POINT ( 'NONE',  ( 0.3996062992125986035, 2.446882876249141962E-17, -1.535433070866141669 ) ) ;
#1935 = AXIS2_PLACEMENT_3D ( 'NONE', #68198, #57178, #10937 ) ;
#1936 = CARTESIAN_POINT ( 'NONE',  ( -0.1058382717557503211, 0.3949938075777409408, -0.7939632545931760710 ) ) ;
#1937 = CARTESIAN_POINT ( 'NONE',  ( 0.2565672512708053188, 1.138339430604204061, -1.632951123234252400 ) ) ;
#1938 = CARTESIAN_POINT ( 'NONE',  ( 0.4068241469816279987, -0.3690944881889765550, -0.3153832671262227771 ) ) ;
#1939 = CARTESIAN_POINT ( 'NONE',  ( -0.3215223097112853146, -0.3162353388693405765, 0.4822834645669290543 ) ) ;
#1940 = CARTESIAN_POINT ( 'NONE',  ( 1.305774278215223960, 0.2952755905511810774, -0.1292274648535930714 ) ) ;
#1941 = CARTESIAN_POINT ( 'NONE',  ( 0.1974969037888706092, -0.3420746716998660508, -1.900918635170603554 ) ) ;
#1942 = CARTESIAN_POINT ( 'NONE',  ( 0.07217847769028949700, -0.2845877964562159024, 0.3641732283464567677 ) ) ;
#1943 = CARTESIAN_POINT ( 'NONE',  ( -0.9711286089238838626, 0.2306618581243847221, -0.2411417322834647770 ) ) ;
#1944 = CARTESIAN_POINT ( 'NONE',  ( 1.509186351706037543, -0.4281496062992127816, -0.4176697321401328100 ) ) ;
#1945 = CARTESIAN_POINT ( 'NONE',  ( -0.1265901696524986964, -0.4724409448818899238, -2.119422572178477626 ) ) ;
#1946 = CARTESIAN_POINT ( 'NONE',  ( 0.3874523867751310524, -0.05870088567678984764, -2.755905511811023612 ) ) ;
#1947 = ORIENTED_EDGE ( 'NONE', *, *, #65602, .T. ) ;
#1948 = ORIENTED_EDGE ( 'NONE', *, *, #50451, .F. ) ;
#1949 = CARTESIAN_POINT ( 'NONE',  ( -1.601049868766403650, -0.6046776061558807314, 0.2411417322834647770 ) ) ;
#1951 = CARTESIAN_POINT ( 'NONE',  ( -1.332020997375327642, -0.05778040916215522460, 0.4822834645669289988 ) ) ;
#1950 = CARTESIAN_POINT ( 'NONE',  ( -1.128608923884513837, 0.1283753931104746893, -0.1820866141732285504 ) ) ;
#1952 = CARTESIAN_POINT ( 'NONE',  ( -0.1049643490035306742, 0.3917322834645668994, -2.448799581855955587 ) ) ;
#1953 = CARTESIAN_POINT ( 'NONE',  ( -1.614173228346457378, 1.267785121476993293, 0.1372047244094476981 ) ) ;
#1954 = CARTESIAN_POINT ( 'NONE',  ( 1.102362204724410155, -0.1870078740157480879, -0.4822834645669291653 ) ) ;
#1955 = CARTESIAN_POINT ( 'NONE',  ( -1.082677165354329896, 0.1660481256975885056, 0.3530559997133364547 ) ) ;
#1956 = CARTESIAN_POINT ( 'NONE',  ( -0.1246719160104980823, 0.2952755905511811885, 0.1292274648535926551 ) ) ;
#1957 = CARTESIAN_POINT ( 'NONE',  ( -1.213910761154854745, -0.6692913385826771977, 0.1292274648535927661 ) ) ;
#1958 = CARTESIAN_POINT ( 'NONE',  ( -0.1958661417322834497, -0.3392501089628018884, -2.665335014926823121 ) ) ;
#1959 = CARTESIAN_POINT ( 'NONE',  ( 0.4527559055118117182, -0.5400638737290844871, 0.3530559997133364547 ) ) ;
#1960 = CARTESIAN_POINT ( 'NONE',  ( -0.1958661417322836718, 0.3392501089628017219, -2.052493438320210029 ) ) ;
#1961 = CARTESIAN_POINT ( 'NONE',  ( -1.207349081364828436, -0.5023911411419708095, 0.1820866141732285504 ) ) ;
#1962 = ORIENTED_EDGE ( 'NONE', *, *, #9565, .T. ) ;
#1963 = CARTESIAN_POINT ( 'NONE',  ( 4.837279021331060870E-17, -0.3949938075777409963, -2.125984251968503713 ) ) ;
#1964 = ORIENTED_EDGE ( 'NONE', *, *, #33686, .F. ) ;
#1965 = CARTESIAN_POINT ( 'NONE',  ( 1.614173228346456712, 1.267785121476991517, 0.1372047244094478646 ) ) ;
#1966 = CARTESIAN_POINT ( 'NONE',  ( -1.076115485564303809, 0.2306618581243848609, 0.2411417322834645549 ) ) ;
#1967 = CARTESIAN_POINT ( 'NONE',  ( -1.305774278215222184, 0.2952755905511811885, 0.1292274648535926551 ) ) ;
#1968 = CARTESIAN_POINT ( 'NONE',  ( 0.1998031496062992740, 0.3460692066303959757, -0.7742782152230971437 ) ) ;
#1969 = CARTESIAN_POINT ( 'NONE',  ( -1.377952755905511140, 0.2952755905511811885, 0.000000000000000000 ) ) ;
#1970 = CARTESIAN_POINT ( 'NONE',  ( -1.601049868766403650, -0.6046776061558807314, 0.2411417322834647770 ) ) ;
#1971 = CARTESIAN_POINT ( 'NONE',  ( -1.397637795275589623, -0.5400638737290845981, -0.3530559997133363437 ) ) ;
#1972 = CARTESIAN_POINT ( 'NONE',  ( -0.3917322834645670104, -7.196005306013484475E-17, 0.03346456692913377107 ) ) ;
#1973 = CARTESIAN_POINT ( 'NONE',  ( 0.2099737532808405305, -0.5023911411419708095, 0.1820866141732285504 ) ) ;
#1974 = CARTESIAN_POINT ( 'NONE',  ( 0.1049643490035304938, -0.3917322834645669549, -0.6423884514435697080 ) ) ;
#1975 = CARTESIAN_POINT ( 'NONE',  ( -0.8267716535433065062, -0.5511811023622047445, 6.969142054262312111E-17 ) ) ;
#1976 = VECTOR ( 'NONE', #64196, 39.37007874015748143 ) ;
#1977 = CARTESIAN_POINT ( 'NONE',  ( -1.148293963254592542, 0.2952755905511811885, 0.1292274648535926551 ) ) ;
#1978 = CARTESIAN_POINT ( 'NONE',  ( 0.9120734908136489683, -0.6692913385826771977, 0.1292274648535927661 ) ) ;
#1979 = CARTESIAN_POINT ( 'NONE',  ( -0.7677165354330699465, -0.5400638737290845981, -0.3530559997133363437 ) ) ;
#1980 = CARTESIAN_POINT ( 'NONE',  ( 0.1049643490035303689, 0.3917322834645670104, 0.01443569553805778768 ) ) ;
#1981 = ORIENTED_EDGE ( 'NONE', *, *, #28395, .F. ) ;
#1982 = CARTESIAN_POINT ( 'NONE',  ( -0.7808398950131222316, -0.3162353388693409650, -0.4822834645669289433 ) ) ;
#1983 = CARTESIAN_POINT ( 'NONE',  ( 0.7414698162729663755, -0.6692913385826773087, -0.1292274648535924053 ) ) ;
#1984 = CARTESIAN_POINT ( 'NONE',  ( -1.627296587926508442, -0.5023911411419708095, -0.1820866141732282451 ) ) ;
#1985 = CARTESIAN_POINT ( 'NONE',  ( -1.601049868766403650, -0.6046776061558807314, 0.2411417322834647770 ) ) ;
#1986 = CARTESIAN_POINT ( 'NONE',  ( 0.3458507752293908943, -0.3458507752293908943, -1.358267716535433101 ) ) ;
#1987 = CARTESIAN_POINT ( 'NONE',  ( 1.851299440327910162, 1.063968899401424251, 0.03484477857460829137 ) ) ;
#1988 = CARTESIAN_POINT ( 'NONE',  ( -0.3917322834645670104, -7.196005306013484475E-17, -0.5039370078740157410 ) ) ;
#1989 = CARTESIAN_POINT ( 'NONE',  ( 0.2867679344610366554, -0.2867679344610365444, -2.545275590551181022 ) ) ;
#1990 = CARTESIAN_POINT ( 'NONE',  ( -0.2755905511811015396, -0.6692913385826771977, 8.415575281601705876E-17 ) ) ;
#1991 = CARTESIAN_POINT ( 'NONE',  ( -1.318897637795274802, 0.07958543189024085140, 0.2665933059059887866 ) ) ;
#1992 = CARTESIAN_POINT ( 'NONE',  ( 0.3996062992125985480, 2.446882876249141654E-17, 0.1200787401574802959 ) ) ;
#1994 = CARTESIAN_POINT ( 'NONE',  ( -1.559171609364246924, 0.3937007874015747699, 0.4177787735906735578 ) ) ;
#1993 = CARTESIAN_POINT ( 'NONE',  ( -1.227034120734907585, 0.2952755905511811885, 0.1292274648535926551 ) ) ;
#1995 = CARTESIAN_POINT ( 'NONE',  ( -1.548556430446193399, 0.2306618581243848609, 0.2411417322834645549 ) ) ;
#1996 = CARTESIAN_POINT ( 'NONE',  ( -0.5774278215223089816, 0.2306618581243847221, -0.2411417322834647770 ) ) ;
#1997 = VECTOR ( 'NONE', #9942, 39.37007874015748143 ) ;
#1998 = CARTESIAN_POINT ( 'NONE',  ( -0.1049643490035306742, 0.3917322834645668994, 0.2283657724747524265 ) ) ;
#1999 = CARTESIAN_POINT ( 'NONE',  ( 0.5643044619422579178, -0.3690944881889765550, -0.3153832671262227771 ) ) ;
#2000 = CARTESIAN_POINT ( 'NONE',  ( -0.3917322834645670104, -7.196005306013484475E-17, -0.1240157480314961758 ) ) ;
#2001 = CARTESIAN_POINT ( 'NONE',  ( 0.1902887139107617975, -0.5511811023622048555, -0.09757992244046775898 ) ) ;
#2002 = CARTESIAN_POINT ( 'NONE',  ( 0.8070866141732288002, 0.07958543189024085140, 0.2665933059059887866 ) ) ;
#2003 = CARTESIAN_POINT ( 'NONE',  ( 1.030183727034121421, -0.3162353388693409650, -0.4822834645669289433 ) ) ;
#2004 = CARTESIAN_POINT ( 'NONE',  ( -0.04593175853018302557, 0.1771653543307087630, 0.09757992244046791164 ) ) ;
#2005 = CARTESIAN_POINT ( 'NONE',  ( -0.3917322834645671215, 0.1049643490035301469, -1.757217847769028340 ) ) ;
#2006 = CARTESIAN_POINT ( 'NONE',  ( -1.292650918635170010, 0.2952755905511810774, -0.1292274648535930714 ) ) ;
#2007 = CARTESIAN_POINT ( 'NONE',  ( -0.1049868766404193215, 0.1283753931104746893, -0.1820866141732285504 ) ) ;
#2008 = CARTESIAN_POINT ( 'NONE',  ( -1.233595800524933894, -0.5023911411419708095, -0.1820866141732282451 ) ) ;
#2009 = CARTESIAN_POINT ( 'NONE',  ( -0.2362204724409451284, 0.4091458600556402425, -0.4048556430446194621 ) ) ;
#2010 = CARTESIAN_POINT ( 'NONE',  ( -0.5708661417322825615, -0.4536011799217367080, 0.2665933059059888421 ) ) ;
#2011 = CARTESIAN_POINT ( 'NONE',  ( 0.4437451894543472664, 1.369490053320156830, -1.614267692121933440 ) ) ;
#2012 = CARTESIAN_POINT ( 'NONE',  ( 0.09842519685039434474, 0.1660481256975885056, 0.3530559997133364547 ) ) ;
#2013 = DIRECTION ( 'NONE',  ( 0.000000000000000000, 0.000000000000000000, -1.000000000000000000 ) ) ;
#2014 = CARTESIAN_POINT ( 'NONE',  ( 0.7414698162729663755, -0.5511811023622048555, -0.09757992244046775898 ) ) ;
#2015 = CARTESIAN_POINT ( 'NONE',  ( -0.2099737532808391705, -0.5023911411419708095, -0.1820866141732282451 ) ) ;
#2016 = CARTESIAN_POINT ( 'NONE',  ( -0.3805774278215216522, 0.05413385826771666132, 0.4176697321401328100 ) ) ;
#2017 = DIRECTION ( 'NONE',  ( 0.000000000000000000, -1.000000000000000000, 0.000000000000000000 ) ) ;
#2018 = CARTESIAN_POINT ( 'NONE',  ( -0.9776902887139098386, 0.1771653543307087075, -0.09757992244046823083 ) ) ;
#2019 = DIRECTION ( 'NONE',  ( -1.000000000000000000, -0.000000000000000000, -0.000000000000000000 ) ) ;
#2020 = CARTESIAN_POINT ( 'NONE',  ( 0.4658792650918641698, -0.05778040916215560624, -0.4822834645669293319 ) ) ;
#2021 = CARTESIAN_POINT ( 'NONE',  ( -0.2925321140481932369, 0.2925321140481931259, -1.356299212598425230 ) ) ;
#2022 = EDGE_CURVE ( 'NONE', #72947, #33617, #60258, .T. ) ;
#2023 = CARTESIAN_POINT ( 'NONE',  ( 0.2867679344610365999, 0.2867679344610365999, -2.584645669291338876 ) ) ;
#2024 = CARTESIAN_POINT ( 'NONE',  ( -0.2296587926509179312, -0.2845877964562161244, -0.3641732283464567121 ) ) ;
#2025 = CARTESIAN_POINT ( 'NONE',  ( -1.404199475065615932, -0.4281496062992127816, -0.4176697321401328100 ) ) ;
#2026 = CARTESIAN_POINT ( 'NONE',  ( -1.653543307086613234, -0.1870078740157479769, 0.3641732283464567677 ) ) ;
#2027 = LINE ( 'NONE', #8344, #38709 ) ;
#2028 = CARTESIAN_POINT ( 'NONE',  ( -0.6955380577427815458, -0.3690944881889765550, -0.3153832671262227771 ) ) ;
#2029 = CARTESIAN_POINT ( 'NONE',  ( -1.089942661822471459, 0.000000000000000000, 0.3464511005275205946 ) ) ;
#2030 = CARTESIAN_POINT ( 'NONE',  ( 0.8333333333333340365, 0.2952755905511810774, -0.1292274648535930714 ) ) ;
#2031 = CARTESIAN_POINT ( 'NONE',  ( -0.2925321140481930704, -0.2925321140481933480, 0.09842519685039367860 ) ) ;
#2032 = CARTESIAN_POINT ( 'NONE',  ( -0.1958661417322836995, 0.3392501089628017219, -2.529546874836956949 ) ) ;
#2033 = PRODUCT_DEFINITION_FORMATION_WITH_SPECIFIED_SOURCE ( 'ANY', '', #59425, .NOT_KNOWN. ) ;
#2034 = CARTESIAN_POINT ( 'NONE',  ( -3.884512598959606322, 2.725419031863056230, -0.5314960629921259283 ) ) ;
#2035 = CARTESIAN_POINT ( 'NONE',  ( -1.666666666666665853, 0.05413385826771626580, -0.4176697321401330321 ) ) ;
#2036 = CARTESIAN_POINT ( 'NONE',  ( -1.391076115485563758, 0.2306618581243848609, 0.2411417322834645549 ) ) ;
#2037 = CARTESIAN_POINT ( 'NONE',  ( 1.167979002624672580, 0.05413385826771626580, -0.4176697321401330321 ) ) ;
#2038 = CARTESIAN_POINT ( 'NONE',  ( -0.1049643490035307020, 0.3917322834645669549, -2.295931758530183497 ) ) ;
#2039 = CARTESIAN_POINT ( 'NONE',  ( 1.476377952755906442, -0.4536011799217367080, 0.2665933059059888421 ) ) ;
#2040 = CARTESIAN_POINT ( 'NONE',  ( 0.5380577427821529035, -0.4281496062992124485, 0.4176697321401328655 ) ) ;
#2041 = CARTESIAN_POINT ( 'NONE',  ( -0.4790026246719152336, -0.05778040916215560624, -0.4822834645669293319 ) ) ;
#2042 = DIRECTION ( 'NONE',  ( 8.673617379884022653E-16, -1.000000000000000000, 3.028377322213053966E-30 ) ) ;
#2043 = CARTESIAN_POINT ( 'NONE',  ( 3.873860110281697189, 2.736617272820978553, 0.5314960629921261503 ) ) ;
#2044 = CARTESIAN_POINT ( 'NONE',  ( 0.9580052493438326877, -0.004921259842519576551, 0.3153832671262227771 ) ) ;
#2045 = EDGE_LOOP ( 'NONE', ( #714, #16160, #27121, #63760 ) ) ;
#2047 = CARTESIAN_POINT ( 'NONE',  ( -0.1958661417322833942, -0.3392501089628018884, -0.2198355887477184134 ) ) ;
#2046 = AXIS2_PLACEMENT_3D ( 'NONE', #6092, #12837, #33442 ) ;
#2048 = ORIENTED_EDGE ( 'NONE', *, *, #25941, .F. ) ;
#2049 = CARTESIAN_POINT ( 'NONE',  ( -0.5052493438320203589, -0.6692913385826771977, 0.1292274648535927661 ) ) ;
#2050 = CARTESIAN_POINT ( 'NONE',  ( 1.404199475065617264, -0.4281496062992124485, 0.4176697321401328655 ) ) ;
#2051 = CARTESIAN_POINT ( 'NONE',  ( 0.09842519685039434474, 0.1660481256975885056, 0.3530559997133364547 ) ) ;
#2052 = CARTESIAN_POINT ( 'NONE',  ( -0.3346456692913377662, 0.07958543189024071263, -0.2665933059059888421 ) ) ;
#2053 = CARTESIAN_POINT ( 'NONE',  ( 1.102362204724410155, -0.1870078740157480879, -0.4822834645669291653 ) ) ;
#2054 = CARTESIAN_POINT ( 'NONE',  ( -0.9908136482939626788, 0.2952755905511811885, 0.1292274648535926551 ) ) ;
#2055 = CARTESIAN_POINT ( 'NONE',  ( -0.06561679790026180015, -0.4281496062992127816, -0.4176697321401328100 ) ) ;
#2056 = CARTESIAN_POINT ( 'NONE',  ( -0.8989501312335946848, 0.2952755905511810774, -0.1292274648535930714 ) ) ;
#2057 = CARTESIAN_POINT ( 'NONE',  ( 1.167979002624672580, 0.05413385826771626580, -0.4176697321401330321 ) ) ;
#2058 = CARTESIAN_POINT ( 'NONE',  ( 1.043307086614173818, -0.5400638737290845981, -0.3530559997133363437 ) ) ;
#2059 = CARTESIAN_POINT ( 'NONE',  ( 1.220472440944882608, 0.2952755905511811885, 0.000000000000000000 ) ) ;
#2060 = CARTESIAN_POINT ( 'NONE',  ( -0.2867679344610365999, 0.2867679344610364889, -0.6417322834645668994 ) ) ;
#2061 = CARTESIAN_POINT ( 'NONE',  ( -0.05905511811023545637, 0.07958543189024085140, 0.2665933059059887866 ) ) ;
#2062 = ORIENTED_EDGE ( 'NONE', *, *, #29607, .F. ) ;
#2063 = CARTESIAN_POINT ( 'NONE',  ( 0.3949938075777411073, -0.1058382717557499464, -1.213910761154855633 ) ) ;
#2064 = EDGE_LOOP ( 'NONE', ( #49645, #3322, #8878, #74804 ) ) ;
#2065 = CARTESIAN_POINT ( 'NONE',  ( -0.8398950131233589023, -0.5023911411419708095, -0.1820866141732282451 ) ) ;
#2066 = CARTESIAN_POINT ( 'NONE',  ( -0.1049868766404193215, -0.6046776061558807314, 0.2411417322834647770 ) ) ;
#2067 = CARTESIAN_POINT ( 'NONE',  ( 2.565164815102312534, 1.469861850861822861, 0.4698711669589720197 ) ) ;
#2068 = CARTESIAN_POINT ( 'NONE',  ( -0.1246719160104980823, 0.2952755905511811885, 0.1292274648535926551 ) ) ;
#2069 = CARTESIAN_POINT ( 'NONE',  ( -0.4461942257217840213, 0.2306618581243848609, 0.2411417322834645549 ) ) ;
#2070 = CARTESIAN_POINT ( 'NONE',  ( -0.7808398950131222316, -0.3162353388693409650, -0.4822834645669289433 ) ) ;
#2071 = CARTESIAN_POINT ( 'NONE',  ( -0.9645669291338575535, -0.5400638737290844871, 0.3530559997133364547 ) ) ;
#2072 = B_SPLINE_CURVE_WITH_KNOTS ( 'NONE', 3,
 ( #19943, #7309, #16917, #30756, #31157, #24433, #82521 ),
 .UNSPECIFIED., .F., .F.,
 ( 4, 3, 4 ),
 ( 3.469446951953614189E-18, 0.001246230184515596025, 0.002492489877932668914 ),
 .UNSPECIFIED. ) ;
#2073 = CARTESIAN_POINT ( 'NONE',  ( 1.417322834645670104, -0.1870078740157480601, -0.3641732283464567677 ) ) ;
#2074 = CARTESIAN_POINT ( 'NONE',  ( -1.450131233595799651, 0.2952755905511810774, -0.1292274648535930714 ) ) ;
#2075 = CARTESIAN_POINT ( 'NONE',  ( -2.554262525012342966, 1.537401574803149984, -0.4744094488188975722 ) ) ;
#2076 = CARTESIAN_POINT ( 'NONE',  ( 0.5577427821522314977, -0.2845877964562161244, -0.3641732283464567121 ) ) ;
#2077 = CARTESIAN_POINT ( 'NONE',  ( 0.1246719160104994284, 0.2952755905511810774, -0.1292274648535930714 ) ) ;
#2078 = CARTESIAN_POINT ( 'NONE',  ( 0.5118110236220480003, -0.6692913385826771977, 8.415575281601705876E-17 ) ) ;
#2079 = ORIENTED_EDGE ( 'NONE', *, *, #29846, .T. ) ;
#2080 = CARTESIAN_POINT ( 'NONE',  ( -0.1998031496062991907, -0.3460692066303959757, -1.325459317585301777 ) ) ;
#2081 = CARTESIAN_POINT ( 'NONE',  ( -0.5643044619422565855, 0.05413385826771626580, -0.4176697321401330321 ) ) ;
#2082 = CARTESIAN_POINT ( 'NONE',  ( 0.2925321140481932369, 0.2925321140481932369, -1.001968503937007871 ) ) ;
#2083 = CARTESIAN_POINT ( 'NONE',  ( 0.1998031496062994128, -0.3460692066303957537, -0.4835958005249343938 ) ) ;
#2084 = CARTESIAN_POINT ( 'NONE',  ( -0.5971128608923877978, 0.2952755905511811885, 0.1292274648535926551 ) ) ;
#2085 = CARTESIAN_POINT ( 'NONE',  ( -0.2362204724409447953, -0.4091458600556404646, 0.09186351706036745279 ) ) ;
#2086 = CARTESIAN_POINT ( 'NONE',  ( 0.3917322834645670104, -0.1049643490035303411, -2.243438320209974357 ) ) ;
#2087 = CARTESIAN_POINT ( 'NONE',  ( -1.594488188976377119, 0.07958543189024071263, -0.2665933059059888421 ) ) ;
#2088 = CARTESIAN_POINT ( 'NONE',  ( 0.7939632545931766261, -0.05778040916215522460, 0.4822834645669289988 ) ) ;
#2089 = CARTESIAN_POINT ( 'NONE',  ( 1.036745406824147731, 0.05413385826771666132, 0.4176697321401328100 ) ) ;
#2090 = CARTESIAN_POINT ( 'NONE',  ( -0.3608923884514428360, 0.1771653543307087630, 0.09757992244046791164 ) ) ;
#2091 = CARTESIAN_POINT ( 'NONE',  ( 0.3805774278215230400, 0.05413385826771626580, -0.4176697321401330321 ) ) ;
#2092 = CARTESIAN_POINT ( 'NONE',  ( 0.4724409448818897572, -0.1265901696524988906, -1.763123359580051952 ) ) ;
#2093 = CARTESIAN_POINT ( 'NONE',  ( -0.05905511811023545637, 0.07958543189024085140, 0.2665933059059887866 ) ) ;
#2094 = CARTESIAN_POINT ( 'NONE',  ( -0.06561679790026180015, -0.4281496062992127816, -0.4176697321401328100 ) ) ;
#2095 = CARTESIAN_POINT ( 'NONE',  ( -0.2891555358219911054, 0.2891555358219909388, -1.198818897637795589 ) ) ;
#2096 = CARTESIAN_POINT ( 'NONE',  ( -1.489501312335957062, -0.3162353388693409650, -0.4822834645669289433 ) ) ;
#2097 = CARTESIAN_POINT ( 'NONE',  ( -0.04593175853018302557, -0.5511811023622048555, -0.09757992244046775898 ) ) ;
#2098 = CARTESIAN_POINT ( 'NONE',  ( 1.594488188976378673, -0.4536011799217368745, -0.2665933059059886201 ) ) ;
#2099 = CARTESIAN_POINT ( 'NONE',  ( -0.8989501312335946848, 0.2952755905511810774, -0.1292274648535930714 ) ) ;
#2100 = CARTESIAN_POINT ( 'NONE',  ( -0.7874015748031489847, -0.1870078740157480601, -0.3641732283464567677 ) ) ;
#2101 = DIRECTION ( 'NONE',  ( 0.7071067811865474617, 0.000000000000000000, -0.7071067811865474617 ) ) ;
#2102 = CARTESIAN_POINT ( 'NONE',  ( -0.8858267716535425107, 0.1660481256975883668, -0.3530559997133364547 ) ) ;
#2103 = CARTESIAN_POINT ( 'NONE',  ( -0.6299212598425188991, -0.1870078740157480879, -0.4822834645669291653 ) ) ;
#2104 = CARTESIAN_POINT ( 'NONE',  ( 8.195543980992789655E-16, -0.1870078740157480879, -0.4822834645669291653 ) ) ;
#2105 = CARTESIAN_POINT ( 'NONE',  ( 0.1998031496062992463, 0.3460692066303959202, -2.583333333333333481 ) ) ;
#2106 = CARTESIAN_POINT ( 'NONE',  ( 0.3917322834645669549, 2.398668435337827645E-17, -2.087907193404512363 ) ) ;
#2107 = AXIS2_PLACEMENT_3D ( 'NONE', #62108, #62940, #23802 ) ;
#2108 = CARTESIAN_POINT ( 'NONE',  ( 0.5314960629920850721, 2.687524476698321507, 3.900447471620236861 ) ) ;
#2109 = CARTESIAN_POINT ( 'NONE',  ( 0.8858267716535438430, 0.07958543189024085140, 0.2665933059059887866 ) ) ;
#2110 = CARTESIAN_POINT ( 'NONE',  ( 1.581364829396326277, -0.05778040916215522460, 0.4822834645669289988 ) ) ;
#2111 = CARTESIAN_POINT ( 'NONE',  ( -1.259842519685038686, -0.1870078740157479769, 0.3641732283464567677 ) ) ;
#2112 = CARTESIAN_POINT ( 'NONE',  ( 1.286089238845145033, -0.6046776061558809534, -0.2411417322834644161 ) ) ;
#2113 = CARTESIAN_POINT ( 'NONE',  ( -0.9711286089238838626, -0.5023911411419708095, 0.1820866141732285504 ) ) ;
#2114 = CARTESIAN_POINT ( 'NONE',  ( -0.5839895013123351797, 0.2952755905511810774, -0.1292274648535930714 ) ) ;
#2115 = CARTESIAN_POINT ( 'NONE',  ( 0.2952755905511819101, 0.07958543189024071263, -0.2665933059059888421 ) ) ;
#2116 = CARTESIAN_POINT ( 'NONE',  ( -0.2362204724409447953, -0.4091458600556404646, -0.8530183727034120755 ) ) ;
#2117 = CARTESIAN_POINT ( 'NONE',  ( 1.056430446194226436, -0.5511811023622048555, -0.09757992244046775898 ) ) ;
#2118 = CARTESIAN_POINT ( 'NONE',  ( 0.4330708661417329575, 0.2952755905511811885, 0.000000000000000000 ) ) ;
#2119 = CARTESIAN_POINT ( 'NONE',  ( -0.2925321140481930149, -0.2925321140481933480, -0.4507874015748031815 ) ) ;
#2120 = EDGE_CURVE ( 'NONE', #49642, #43005, #35002, .T. ) ;
#2121 = CARTESIAN_POINT ( 'NONE',  ( -0.6167979002624665030, 0.05413385826771666132, 0.4176697321401328100 ) ) ;
#2122 = CARTESIAN_POINT ( 'NONE',  ( -0.1049643490035307020, 0.3917322834645669549, -1.508530183727033736 ) ) ;
#2123 = CARTESIAN_POINT ( 'NONE',  ( 1.213910761154856299, -0.5511811023622048555, -0.09757992244046775898 ) ) ;
#2124 = CARTESIAN_POINT ( 'NONE',  ( 0.5183727034120741983, -0.6692913385826771977, 0.1292274648535927661 ) ) ;
#2125 = CARTESIAN_POINT ( 'NONE',  ( -0.2821522309711278487, -0.6692913385826773087, -0.1292274648535924053 ) ) ;
#2126 = CARTESIAN_POINT ( 'NONE',  ( -0.1771653543307080136, 0.07958543189024071263, -0.2665933059059888421 ) ) ;
#2127 = DIRECTION ( 'NONE',  ( -1.000000000000000000, 0.000000000000000000, 0.000000000000000000 ) ) ;
#2128 = CARTESIAN_POINT ( 'NONE',  ( 0.1181102362204730916, 0.1771653543307087630, 0.000000000000000000 ) ) ;
#2129 = CARTESIAN_POINT ( 'NONE',  ( 0.6102362204724416372, 0.1660481256975883668, -0.3530559997133364547 ) ) ;
#2130 = CARTESIAN_POINT ( 'NONE',  ( -0.8989501312335946848, 0.1771653543307087075, -0.09757992244046823083 ) ) ;
#2131 = CARTESIAN_POINT ( 'NONE',  ( -0.2925321140481930149, -0.2925321140481933480, -1.080708661417322691 ) ) ;
#2132 = CARTESIAN_POINT ( 'NONE',  ( -1.161417322834644716, 0.1660481256975885056, 0.3530559997133364547 ) ) ;
#2133 = CARTESIAN_POINT ( 'NONE',  ( 1.348312163386739426, 0.2755905511811023723, 0.5221511799597032821 ) ) ;
#2134 = ORIENTED_EDGE ( 'NONE', *, *, #48920, .T. ) ;
#2135 = CARTESIAN_POINT ( 'NONE',  ( -1.266404199475064773, -0.2845877964562159024, 0.3641732283464567677 ) ) ;
#2136 = CARTESIAN_POINT ( 'NONE',  ( -0.2165354330708654795, -0.5400638737290845981, -0.3530559997133363437 ) ) ;
#2137 = CARTESIAN_POINT ( 'NONE',  ( 0.3992723400743284912, 9.133324503354010218E-17, -1.220472440944882164 ) ) ;
#2138 = CARTESIAN_POINT ( 'NONE',  ( -0.9645669291338575535, 0.1660481256975883668, -0.3530559997133364547 ) ) ;
#2139 = DIRECTION ( 'NONE',  ( -3.491481338843133355E-15, -0.000000000000000000, 1.000000000000000000 ) ) ;
#2141 = CARTESIAN_POINT ( 'NONE',  ( 0.9645669291338588858, 0.1660481256975885056, 0.3530559997133364547 ) ) ;
#2140 = CARTESIAN_POINT ( 'NONE',  ( 1.581364829396326277, -0.3162353388693409650, -0.4822834645669289433 ) ) ;
#2142 = CARTESIAN_POINT ( 'NONE',  ( 1.043307086614173818, 0.1660481256975885056, 0.3530559997133364547 ) ) ;
#2143 = CARTESIAN_POINT ( 'NONE',  ( -0.3917322834645671215, 0.1049643490035301469, -2.702099737532808188 ) ) ;
#2144 = CARTESIAN_POINT ( 'NONE',  ( -1.595398199321656607, 1.309738123151862998, 0.1559797534342480529 ) ) ;
#2145 = AXIS2_PLACEMENT_3D ( 'NONE', #68264, #30762, #4670 ) ;
#2146 = CARTESIAN_POINT ( 'NONE',  ( -1.469816272965878357, -0.6046776061558809534, -0.2411417322834644161 ) ) ;
#2147 = CARTESIAN_POINT ( 'NONE',  ( 0.3996062992125986035, 2.446882876249141962E-17, -0.4330708661417322913 ) ) ;
#2148 = EDGE_LOOP ( 'NONE', ( #71417, #20240, #3302, #914 ) ) ;
#2149 = CARTESIAN_POINT ( 'NONE',  ( -0.6167979002624665030, -0.3690944881889765550, -0.3153832671262227771 ) ) ;
#2150 = CARTESIAN_POINT ( 'NONE',  ( -0.1958661417322834220, -0.3392501089628018884, -2.104986876640420057 ) ) ;
#2151 = ORIENTED_EDGE ( 'NONE', *, *, #58402, .T. ) ;
#2152 = CARTESIAN_POINT ( 'NONE',  ( 0.7217847769028878924, -0.4281496062992127816, -0.4176697321401328100 ) ) ;
#2153 = CARTESIAN_POINT ( 'NONE',  ( 0.1377952755905518800, -0.5400638737290844871, 0.3530559997133364547 ) ) ;
#2154 = CARTESIAN_POINT ( 'NONE',  ( -0.6627296587926501115, 0.2952755905511810774, -0.1292274648535930714 ) ) ;
#2155 = CARTESIAN_POINT ( 'NONE',  ( 1.548556430446194954, 0.2306618581243847221, -0.2411417322834647770 ) ) ;
#2156 = CARTESIAN_POINT ( 'NONE',  ( -0.7874015748031489847, -0.1870078740157480601, -0.3641732283464567677 ) ) ;
#2157 = CARTESIAN_POINT ( 'NONE',  ( -0.2362204724409447953, -0.4091458600556404646, -2.032152230971128848 ) ) ;
#2158 = CARTESIAN_POINT ( 'NONE',  ( 0.8727034120734913358, -0.05778040916215522460, 0.4822834645669289988 ) ) ;
#2159 = EDGE_CURVE ( 'NONE', #42372, #16885, #15658, .T. ) ;
#2160 = CARTESIAN_POINT ( 'NONE',  ( 0.4986876640419954376, 0.1283753931104748280, 0.1820866141732283561 ) ) ;
#2161 = CARTESIAN_POINT ( 'NONE',  ( -0.5511811023622038563, -0.1870078740157479769, 0.4822834645669291653 ) ) ;
#2162 = CARTESIAN_POINT ( 'NONE',  ( 0.2867679344610365999, -0.2867679344610365999, -1.595781209152543845 ) ) ;
#2163 = CARTESIAN_POINT ( 'NONE',  ( -1.135170603674539924, 0.2952755905511810774, -0.1292274648535930714 ) ) ;
#2164 = DIRECTION ( 'NONE',  ( 0.000000000000000000, -1.000000000000000000, 0.000000000000000000 ) ) ;
#2165 = CARTESIAN_POINT ( 'NONE',  ( 1.279527559055118724, -0.5400638737290845981, -0.3530559997133363437 ) ) ;
#2166 = CARTESIAN_POINT ( 'NONE',  ( 1.207349081364829990, 0.1283753931104748280, 0.1820866141732283561 ) ) ;
#2167 = ORIENTED_EDGE ( 'NONE', *, *, #61841, .T. ) ;
#2168 = CARTESIAN_POINT ( 'NONE',  ( 4.837279021331060870E-17, -0.3949938075777409963, 0.07874015748031490403 ) ) ;
#2169 = CARTESIAN_POINT ( 'NONE',  ( -0.1443569553805765515, -0.4281496062992127816, -0.4176697321401328100 ) ) ;
#2170 = ORIENTED_EDGE ( 'NONE', *, *, #4245, .F. ) ;
#2171 = CARTESIAN_POINT ( 'NONE',  ( 0.8661417322834652488, -0.1870078740157480601, -0.3641732283464567677 ) ) ;
#2172 = CARTESIAN_POINT ( 'NONE',  ( -1.102362204724408601, -0.1870078740157479769, 0.4822834645669291653 ) ) ;
#2173 = CARTESIAN_POINT ( 'NONE',  ( 1.017060367454068581, -0.05778040916215560624, -0.4822834645669293319 ) ) ;
#2174 = CARTESIAN_POINT ( 'NONE',  ( 0.6889763779527563470, 0.1660481256975883668, -0.3530559997133364547 ) ) ;
#2175 = CARTESIAN_POINT ( 'NONE',  ( 0.1115485564304467270, -0.6692913385826773087, -0.1292274648535924053 ) ) ;
#2176 = CARTESIAN_POINT ( 'NONE',  ( -0.3937007874015740483, -0.1870078740157479769, 0.4822834645669291653 ) ) ;
#2177 = CARTESIAN_POINT ( 'NONE',  ( 0.3392501089628018329, 0.1958661417322835607, -1.633202099737532942 ) ) ;
#2178 = CARTESIAN_POINT ( 'NONE',  ( -1.719160104986876103, 0.05413385826771666132, 0.4176697321401328100 ) ) ;
#2179 = CARTESIAN_POINT ( 'NONE',  ( -0.5643044619422565855, -0.4281496062992124485, 0.4176697321401328655 ) ) ;
#2180 = CARTESIAN_POINT ( 'NONE',  ( -0.6102362204724400829, -0.4536011799217368745, -0.2665933059059886201 ) ) ;
#2181 = FACE_OUTER_BOUND ( 'NONE', #64280, .T. ) ;
#2182 = CARTESIAN_POINT ( 'NONE',  ( 0.5314960629920847390, 2.755905511811024056, 3.937007874015794773 ) ) ;
#2183 = CARTESIAN_POINT ( 'NONE',  ( -0.5183727034120726440, -0.6692913385826773087, -0.1292274648535924053 ) ) ;
#2184 = CARTESIAN_POINT ( 'NONE',  ( -0.3149606299212733829, 2.559055118110236560, 3.924389226575467404 ) ) ;
#2185 = CARTESIAN_POINT ( 'NONE',  ( 0.6036745406824153282, -0.6046776061558807314, 0.2411417322834647770 ) ) ;
#2186 = CARTESIAN_POINT ( 'NONE',  ( 0.1998031496062992740, 0.3460692066303959757, -2.034120734908136718 ) ) ;
#2187 = CARTESIAN_POINT ( 'NONE',  ( 3.936627864294173218, 1.066117803576733358, -0.06254616550773663131 ) ) ;
#2188 = ADVANCED_FACE ( 'NONE', ( #47199 ), #68532, .T. ) ;
#2189 = CARTESIAN_POINT ( 'NONE',  ( 0.06561679790026316017, -0.4281496062992124485, 0.4176697321401328655 ) ) ;
#2191 = CARTESIAN_POINT ( 'NONE',  ( -0.9324623468618411515, 0.000000000000000000, 0.3464511005275205946 ) ) ;
#2190 = CARTESIAN_POINT ( 'NONE',  ( 1.062992125984252745, 0.1771653543307087630, 0.000000000000000000 ) ) ;
#2192 = CARTESIAN_POINT ( 'NONE',  ( 0.1265901696524990294, -0.4724409448818896462, -0.7919947506561679784 ) ) ;
#2193 = CARTESIAN_POINT ( 'NONE',  ( 1.305774278215223960, -0.5511811023622046335, 0.09757992244046803654 ) ) ;
#2194 = CARTESIAN_POINT ( 'NONE',  ( 1.082677165354331228, -0.5400638737290844871, 0.3530559997133364547 ) ) ;
#2195 = CARTESIAN_POINT ( 'NONE',  ( 0.3420746716998660508, -0.1974969037888704149, -0.1817585301837270073 ) ) ;
#2196 = CARTESIAN_POINT ( 'NONE',  ( -0.3740157480314953431, -0.5400638737290845981, -0.3530559997133363437 ) ) ;
#2197 = CARTESIAN_POINT ( 'NONE',  ( -1.535433070866141225, -0.6692913385826771977, 8.415575281601705876E-17 ) ) ;
#2198 = CARTESIAN_POINT ( 'NONE',  ( -1.673228346456691717, 0.1660481256975883668, -0.3530559997133364547 ) ) ;
#2199 = CARTESIAN_POINT ( 'NONE',  ( -0.1246719160104980823, 0.2952755905511811885, 0.1292274648535926551 ) ) ;
#2200 = CARTESIAN_POINT ( 'NONE',  ( 0.1058382717557499880, 0.3949938075777409408, -0.5426509186351705649 ) ) ;
#2201 = CARTESIAN_POINT ( 'NONE',  ( 1.279527559055118724, -0.5400638737290845981, -0.3530559997133363437 ) ) ;
#2202 = CARTESIAN_POINT ( 'NONE',  ( 0.5511811023622054106, -0.1870078740157480879, -0.4822834645669291653 ) ) ;
#2203 = CARTESIAN_POINT ( 'NONE',  ( 0.7217847769028878924, -0.004921259842519576551, 0.3153832671262227771 ) ) ;
#2204 = CARTESIAN_POINT ( 'NONE',  ( -0.3458507752293906723, -0.3458507752293910609, -0.1358267716535432879 ) ) ;
#2205 = CARTESIAN_POINT ( 'NONE',  ( 0.4265091863517067594, 0.1771653543307087630, 0.09757992244046791164 ) ) ;
#2206 = CARTESIAN_POINT ( 'NONE',  ( -1.036745406824146176, 0.009842519685039144428, -0.3409548833797004797 ) ) ;
#2207 = CARTESIAN_POINT ( 'NONE',  ( -0.2925321140481930149, -0.2925321140481933480, -1.238188976377952999 ) ) ;
#2208 = CARTESIAN_POINT ( 'NONE',  ( 0.6167979002624679463, 0.05413385826771626580, -0.4176697321401330321 ) ) ;
#2209 = CARTESIAN_POINT ( 'NONE',  ( -9.594673741351313045E-17, 0.3917322834645670104, -0.9370078740157480324 ) ) ;
#2210 = AXIS2_PLACEMENT_3D ( 'NONE', #55831, #54600, #81949 ) ;
#2211 = CIRCLE ( 'NONE', #886, 0.5118110236220471121 ) ;
#2212 = FACE_OUTER_BOUND ( 'NONE', #52049, .T. ) ;
#2213 = CARTESIAN_POINT ( 'NONE',  ( -0.3503937007874015630, 0.3044824468161027586, -0.01968503937007903132 ) ) ;
#2214 = CARTESIAN_POINT ( 'NONE',  ( 0.1509186351706042484, -0.2845877964562159024, 0.3641732283464567677 ) ) ;
#2215 = CARTESIAN_POINT ( 'NONE',  ( 0.6233595800524942554, -0.05778040916215560624, -0.4822834645669293319 ) ) ;
#2216 = CARTESIAN_POINT ( 'NONE',  ( 1.364829396325460076, 0.1283753931104748280, 0.1820866141732283561 ) ) ;
#2217 = CARTESIAN_POINT ( 'NONE',  ( -0.8005249343832013809, -0.3690944881889763329, 0.3153832671262228327 ) ) ;
#2218 = CARTESIAN_POINT ( 'NONE',  ( -1.003937007874015297, -0.5400638737290845981, -0.3530559997133363437 ) ) ;
#2219 = CARTESIAN_POINT ( 'NONE',  ( -1.522309711286088607, 0.2306618581243847221, -0.2411417322834647770 ) ) ;
#2220 = CARTESIAN_POINT ( 'NONE',  ( 0.7020997375328090762, -0.3162353388693405765, 0.4822834645669290543 ) ) ;
#2221 = CARTESIAN_POINT ( 'NONE',  ( 1.660104986876641320, -0.05778040916215522460, 0.4822834645669289988 ) ) ;
#2222 =( BOUNDED_CURVE ( )  B_SPLINE_CURVE ( 3, ( #62120, #23815, #36447, #22584 ),
 .UNSPECIFIED., .F., .F. ) 
 B_SPLINE_CURVE_WITH_KNOTS ( ( 4, 4 ),
 ( 0.000000000000000000, 0.6251940424154347475 ),
 .UNSPECIFIED. ) 
 CURVE ( )  GEOMETRIC_REPRESENTATION_ITEM ( )  RATIONAL_B_SPLINE_CURVE ( ( 1.000000000000000000, 0.9676920770090842172, 0.9676920770090842172, 1.000000000000000000 ) ) 
 REPRESENTATION_ITEM ( '' )  );
#2223 = DIRECTION ( 'NONE',  ( 0.000000000000000000, -0.7071067811865376918, 0.7071067811865573427 ) ) ;
#2224 = CARTESIAN_POINT ( 'NONE',  ( 0.7545931758530188826, -0.6692913385826771977, 0.1292274648535927661 ) ) ;
#2225 = CARTESIAN_POINT ( 'NONE',  ( 0.4091458600556404646, -0.2362204724409448231, -2.701443569553806157 ) ) ;
#2226 = CARTESIAN_POINT ( 'NONE',  ( 0.1077486724431487297, 1.075126265569047890, 3.935562984763014249 ) ) ;
#2227 = CARTESIAN_POINT ( 'NONE',  ( 1.259842519685040019, -0.1870078740157480879, -0.4822834645669291653 ) ) ;
#2228 = CARTESIAN_POINT ( 'NONE',  ( -1.397637795275589623, 0.07958543189024085140, 0.2665933059059887866 ) ) ;
#2229 = CARTESIAN_POINT ( 'NONE',  ( 1.161417322834646493, -0.4536011799217367080, 0.2665933059059888421 ) ) ;
#2230 = CARTESIAN_POINT ( 'NONE',  ( -1.227034120734907141, -0.5511811023622048555, -0.09757992244046775898 ) ) ;
#2231 = CARTESIAN_POINT ( 'NONE',  ( -0.8530183727034112984, -0.004921259842519576551, 0.3153832671262227771 ) ) ;
#2232 = CARTESIAN_POINT ( 'NONE',  ( -1.157146581871515012E-16, 0.4724409448818898682, -2.047244094488188892 ) ) ;
#2233 = CARTESIAN_POINT ( 'NONE',  ( 0.5511811023622054106, -0.1870078740157480601, -0.3641732283464567677 ) ) ;
#2234 = CARTESIAN_POINT ( 'NONE',  ( -0.006561679790025524116, -0.05778040916215560624, -0.4822834645669293319 ) ) ;
#2235 = CARTESIAN_POINT ( 'NONE',  ( 0.9317585301837276734, -0.4281496062992124485, 0.4176697321401328655 ) ) ;
#2236 = CARTESIAN_POINT ( 'NONE',  ( 0.1771653543307093182, -0.5400638737290845981, -0.3530559997133363437 ) ) ;
#2237 = CARTESIAN_POINT ( 'NONE',  ( 0.1771653543307093182, 0.07958543189024085140, 0.2665933059059887866 ) ) ;
#2238 = CARTESIAN_POINT ( 'NONE',  ( 1.128608923884514947, 0.2306618581243848609, 0.2411417322834645549 ) ) ;
#2239 = CARTESIAN_POINT ( 'NONE',  ( -1.548556430446193399, -0.6046776061558809534, -0.2411417322834644161 ) ) ;
#2240 = CARTESIAN_POINT ( 'NONE',  ( -0.9186351706036736120, 0.2306618581243848609, 0.2411417322834645549 ) ) ;
#2241 = CARTESIAN_POINT ( 'NONE',  ( -0.2925321140481932369, 0.2925321140481931814, -0.6496062992125984925 ) ) ;
#2242 = CARTESIAN_POINT ( 'NONE',  ( 0.4724409448818898682, 2.892866454678787531E-17, -0.5098425196850393526 ) ) ;
#2243 = CARTESIAN_POINT ( 'NONE',  ( -0.7677165354330699465, -0.5400638737290845981, -0.3530559997133363437 ) ) ;
#2244 = CARTESIAN_POINT ( 'NONE',  ( -0.1902887139107604098, -0.6692913385826771977, 0.1292274648535927661 ) ) ;
#2245 = CARTESIAN_POINT ( 'NONE',  ( 0.2925321140481932369, -0.2925321140481932369, -2.460629921259842146 ) ) ;
#2246 = CARTESIAN_POINT ( 'NONE',  ( 0.3949938075777409408, 0.1058382717557500574, -2.171916010498687655 ) ) ;
#2247 = ORIENTED_EDGE ( 'NONE', *, *, #83113, .T. ) ;
#2248 = CARTESIAN_POINT ( 'NONE',  ( -0.1958661417322834220, -0.3392501089628018884, -0.8451443569553805935 ) ) ;
#2249 = LINE ( 'NONE', #3492, #18588 ) ;
#2250 = CARTESIAN_POINT ( 'NONE',  ( -1.286089238845143479, -0.5023911411419708095, 0.1820866141732285504 ) ) ;
#2251 = CARTESIAN_POINT ( 'NONE',  ( -0.1958661417322834220, -0.3392501089628018884, -1.160104986876640210 ) ) ;
#2252 = EDGE_CURVE ( 'NONE', #41772, #24205, #68941, .T. ) ;
#2253 = CARTESIAN_POINT ( 'NONE',  ( -1.627296587926508442, -0.6046776061558809534, -0.2411417322834644161 ) ) ;
#2254 = CARTESIAN_POINT ( 'NONE',  ( 0.1049643490035304522, -0.3917322834645668994, 0.1496256149944375224 ) ) ;
#2255 = CARTESIAN_POINT ( 'NONE',  ( -0.1246719160104980823, -0.6692913385826773087, -0.1292274648535924053 ) ) ;
#2256 = CARTESIAN_POINT ( 'NONE',  ( -0.3149606299212590610, -0.1870078740157479769, 0.3641732283464567677 ) ) ;
#2257 = CARTESIAN_POINT ( 'NONE',  ( 0.7086614173228352742, -0.1870078740157480879, -0.4822834645669291653 ) ) ;
#2258 = CARTESIAN_POINT ( 'NONE',  ( 0.4658792650918640033, -0.3162353388693405765, 0.4822834645669290543 ) ) ;
#2259 = CARTESIAN_POINT ( 'NONE',  ( -0.2262115530851587786, -2.191421614605370878E-15, 0.4445507791589071167 ) ) ;
#2260 = VECTOR ( 'NONE', #74675, 39.37007874015748143 ) ;
#2261 = CARTESIAN_POINT ( 'NONE',  ( 0.3996062992125986590, -0.1070741851644053111, -2.631233595800525293 ) ) ;
#2262 = CARTESIAN_POINT ( 'NONE',  ( 0.3392501089628018884, -0.1958661417322833942, -1.361567872212285257 ) ) ;
#2263 = CARTESIAN_POINT ( 'NONE',  ( 1.233595800524935227, 0.2306618581243847221, -0.2411417322834647770 ) ) ;
#2264 = CIRCLE ( 'NONE', #38528, 2.362204724409449064 ) ;
#2265 = AXIS2_PLACEMENT_3D ( 'NONE', #17616, #80218, #81040 ) ;
#2266 = CARTESIAN_POINT ( 'NONE',  ( -0.03280839895013062252, -0.6692913385826771977, 0.1292274648535927661 ) ) ;
#2267 = CARTESIAN_POINT ( 'NONE',  ( -0.9776902887139098386, 0.2952755905511810774, -0.1292274648535930714 ) ) ;
#2268 = CARTESIAN_POINT ( 'NONE',  ( -1.633858267716534529, 0.1660481256975885056, 0.3530559997133364547 ) ) ;
#2269 = CARTESIAN_POINT ( 'NONE',  ( 1.030183727034121421, -0.05778040916215522460, 0.4822834645669289988 ) ) ;
#2270 = CARTESIAN_POINT ( 'NONE',  ( -0.3392501089628019995, 0.1958661417322832277, -0.5833333333333334814 ) ) ;
#2271 = CARTESIAN_POINT ( 'NONE',  ( 0.2230971128608929543, 0.05413385826771626580, -0.4176697321401330321 ) ) ;
#2272 = CARTESIAN_POINT ( 'NONE',  ( 0.5052493438320218022, -0.6692913385826773087, -0.1292274648535924053 ) ) ;
#2273 = CARTESIAN_POINT ( 'NONE',  ( -0.2296587926509179312, -0.05778040916215522460, 0.4822834645669289988 ) ) ;
#2274 = CARTESIAN_POINT ( 'NONE',  ( 0.8530183727034128527, -0.3690944881889763329, 0.3153832671262228327 ) ) ;
#2275 = CARTESIAN_POINT ( 'NONE',  ( -1.246719160104986512, 0.05413385826771666132, 0.4176697321401328100 ) ) ;
#2276 = CARTESIAN_POINT ( 'NONE',  ( -1.522309711286088607, 0.2306618581243847221, -0.2411417322834647770 ) ) ;
#2277 = CARTESIAN_POINT ( 'NONE',  ( 0.6299212598425204535, -0.1870078740157479769, 0.4822834645669291653 ) ) ;
#2278 = CARTESIAN_POINT ( 'NONE',  ( 0.1584414948832921777, -0.3588842212252807418, -1.929133858267716883 ) ) ;
#2279 = CARTESIAN_POINT ( 'NONE',  ( -0.1958661417322836718, 0.3392501089628017219, -2.052493438320210029 ) ) ;
#2280 = ORIENTED_EDGE ( 'NONE', *, *, #7637, .T. ) ;
#2281 = EDGE_CURVE ( 'NONE', #39084, #5951, #14402, .T. ) ;
#2282 = CARTESIAN_POINT ( 'NONE',  ( -0.2925321140481932924, 0.2925321140481931814, -0.3346456692913385988 ) ) ;
#2283 = ORIENTED_EDGE ( 'NONE', *, *, #42014, .T. ) ;
#2284 = CARTESIAN_POINT ( 'NONE',  ( 1.036745406824147731, 0.05413385826771666132, 0.4176697321401328100 ) ) ;
#2285 = CARTESIAN_POINT ( 'NONE',  ( 0.6889763779527563470, 0.07958543189024071263, -0.2665933059059888421 ) ) ;
#2286 = CARTESIAN_POINT ( 'NONE',  ( 0.5905511811023629321, 0.2952755905511811885, 0.000000000000000000 ) ) ;
#2287 = ADVANCED_FACE ( 'NONE', ( #4547 ), #41788, .F. ) ;
#2288 = CARTESIAN_POINT ( 'NONE',  ( 0.8761506516392508770, -4.927456884911482678E-16, 0.4445507791589062840 ) ) ;
#2289 = PRESENTATION_STYLE_ASSIGNMENT (( #48543 ) ) ;
#2290 = CARTESIAN_POINT ( 'NONE',  ( 0.1958661417322834775, 0.3392501089628018884, -1.331364829396325611 ) ) ;
#2291 = PRODUCT_RELATED_PRODUCT_CATEGORY ( 'part', '', ( #8366 ) ) ;
#2292 = CARTESIAN_POINT ( 'NONE',  ( -1.496062992125983815, -0.1870078740157479769, 0.4822834645669291653 ) ) ;
#2293 = CARTESIAN_POINT ( 'NONE',  ( -0.4790026246719154557, -0.3162353388693405765, 0.4822834645669290543 ) ) ;
#2294 = CARTESIAN_POINT ( 'NONE',  ( 1.174540682414699111, -0.05778040916215560624, -0.4822834645669293319 ) ) ;
#2295 = VERTEX_POINT ( 'NONE', #38416 ) ;
#2296 = CARTESIAN_POINT ( 'NONE',  ( -1.423884514435694859, -0.3162353388693405765, 0.4822834645669290543 ) ) ;
#2297 = CARTESIAN_POINT ( 'NONE',  ( -1.035641998995818547, 1.340358236468215392, -0.4318304824445497458 ) ) ;
#2298 =( CONVERSION_BASED_UNIT ( 'INCH', #59942 ) LENGTH_UNIT ( ) NAMED_UNIT ( #36792 ) );
#2299 = CARTESIAN_POINT ( 'NONE',  ( 0.4177787735907000366, 1.299212598425196985, -1.736336963694947944 ) ) ;
#2300 = CARTESIAN_POINT ( 'NONE',  ( 4.893765752498283308E-17, -0.3996062992125985480, -2.045275590551181466 ) ) ;
#2301 = CARTESIAN_POINT ( 'NONE',  ( -1.338582677165353729, -0.1870078740157479769, 0.3641732283464567677 ) ) ;
#2302 = CARTESIAN_POINT ( 'NONE',  ( -1.568241469816272105, -0.3162353388693409650, -0.4822834645669289433 ) ) ;
#2303 = CARTESIAN_POINT ( 'NONE',  ( 0.2034120734908144990, -0.6692913385826771977, 0.1292274648535927661 ) ) ;
#2304 = ORIENTED_EDGE ( 'NONE', *, *, #153, .T. ) ;
#2306 = FACE_OUTER_BOUND ( 'NONE', #9636, .T. ) ;
#2305 = CARTESIAN_POINT ( 'NONE',  ( 1.587926509186352586, -0.4281496062992127816, -0.4176697321401328100 ) ) ;
#2307 = CARTESIAN_POINT ( 'NONE',  ( -0.7349081364829390672, 0.1283753931104746893, -0.1820866141732285504 ) ) ;
#2308 = CARTESIAN_POINT ( 'NONE',  ( 0.9120734908136490793, 0.2952755905511810774, -0.1292274648535930714 ) ) ;
#2309 = CARTESIAN_POINT ( 'NONE',  ( 1.076115485564305141, -0.5023911411419708095, 0.1820866141732285504 ) ) ;
#2310 = CARTESIAN_POINT ( 'NONE',  ( 0.1049643490035303689, 0.3917322834645668994, -1.333314017551494368 ) ) ;
#2311 = CARTESIAN_POINT ( 'NONE',  ( -0.6627296587926503335, -0.5511811023622046335, 0.09757992244046803654 ) ) ;
#2312 = CARTESIAN_POINT ( 'NONE',  ( -1.391076115485563314, -0.5023911411419708095, -0.1820866141732282451 ) ) ;
#2313 = CARTESIAN_POINT ( 'NONE',  ( 0.3392501089628018329, 0.1958661417322835607, -1.160761154855643129 ) ) ;
#2315 = EDGE_CURVE ( 'NONE', #16662, #77295, #81626, .T. ) ;
#2314 = CARTESIAN_POINT ( 'NONE',  ( 0.3937007874015754361, -0.1870078740157480879, -0.4822834645669291653 ) ) ;
#2316 = CARTESIAN_POINT ( 'NONE',  ( -0.8005249343832011588, -0.004921259842519870586, -0.3153832671262229437 ) ) ;
#2317 = CARTESIAN_POINT ( 'NONE',  ( -0.1115485564304456306, 0.1771653543307087075, -0.09757992244046823083 ) ) ;
#2318 = CARTESIAN_POINT ( 'NONE',  ( -0.1049868766404193215, 0.2306618581243847221, -0.2411417322834647770 ) ) ;
#2319 = CARTESIAN_POINT ( 'NONE',  ( -1.541994750656167090, -0.5511811023622048555, -0.09757992244046775898 ) ) ;
#2320 = CARTESIAN_POINT ( 'NONE',  ( -0.3917322834645671770, 0.1049643490035302024, 0.1279334401236726371 ) ) ;
#2321 = CARTESIAN_POINT ( 'NONE',  ( 0.6364829396325465405, -0.05778040916215522460, 0.4822834645669289988 ) ) ;
#2322 = CIRCLE ( 'NONE', #27852, 0.1190944881889763746 ) ;
#2323 = AXIS2_PLACEMENT_3D ( 'NONE', #5498, #17736, #57233 ) ;
#2324 = CARTESIAN_POINT ( 'NONE',  ( 0.3307086614173228023, 0.3733313776025732333, 0.000000000000000000 ) ) ;
#2325 = STYLED_ITEM ( 'NONE', ( #31329 ), #59000 ) ;
#2326 = CARTESIAN_POINT ( 'NONE',  ( -1.157146581871515012E-16, 0.4724409448818898682, -1.494094488188976388 ) ) ;
#2327 = AXIS2_PLACEMENT_3D ( 'NONE', #62752, #43773, #24838 ) ;
#2328 = CARTESIAN_POINT ( 'NONE',  ( -0.7611548556430438595, 0.2306618581243848609, 0.2411417322834645549 ) ) ;
#2329 = CARTESIAN_POINT ( 'NONE',  ( -0.3674540682414692561, -0.5023911411419708095, -0.1820866141732282451 ) ) ;
#2330 = CARTESIAN_POINT ( 'NONE',  ( -1.207349081364828436, -0.6046776061558807314, 0.2411417322834647770 ) ) ;
#2331 = CARTESIAN_POINT ( 'NONE',  ( 0.4068241469816281097, -0.004921259842519576551, 0.3153832671262227771 ) ) ;
#2332 = CARTESIAN_POINT ( 'NONE',  ( -0.5511811023622041894, -0.1870078740157480601, -0.3641732283464567677 ) ) ;
#2333 = CARTESIAN_POINT ( 'NONE',  ( -0.9251968503937002541, 0.1660481256975885056, 0.3530559997133364547 ) ) ;
#2334 = CARTESIAN_POINT ( 'NONE',  ( -1.699475065616797398, 0.2952755905511811885, 0.1292274648535926551 ) ) ;
#2335 = CARTESIAN_POINT ( 'NONE',  ( 1.587926509186352586, -0.4281496062992127816, -0.4176697321401328100 ) ) ;
#2336 = CARTESIAN_POINT ( 'NONE',  ( 1.089942661822472569, 9.906153642143428645E-17, -0.3464511005275205946 ) ) ;
#2337 = CARTESIAN_POINT ( 'NONE',  ( 0.8333333333333340365, -0.5511811023622046335, 0.09757992244046803654 ) ) ;
#2338 = CARTESIAN_POINT ( 'NONE',  ( 0.4265091863517067594, 0.2952755905511811885, 0.1292274648535926551 ) ) ;
#2339 = CARTESIAN_POINT ( 'NONE',  ( -1.404199475065615932, -0.4281496062992127816, -0.4176697321401328100 ) ) ;
#2340 = CARTESIAN_POINT ( 'NONE',  ( 1.463254593175853824, 0.1771653543307087075, -0.09757992244046823083 ) ) ;
#2341 = ORIENTED_EDGE ( 'NONE', *, *, #38343, .T. ) ;
#2342 = ADVANCED_FACE ( 'NONE', ( #25780 ), #58181, .T. ) ;
#2343 = CARTESIAN_POINT ( 'NONE',  ( -0.2925321140481932369, 0.2925321140481931259, -2.616141732283464805 ) ) ;
#2344 = CARTESIAN_POINT ( 'NONE',  ( -1.246719160104985846, -0.3690944881889765550, -0.3153832671262227771 ) ) ;
#2345 = CARTESIAN_POINT ( 'NONE',  ( -0.2690288713910754526, -0.6692913385826771977, 0.1292274648535927661 ) ) ;
#2346 = CARTESIAN_POINT ( 'NONE',  ( 0.4068241469816279987, -0.4281496062992127816, -0.4176697321401328100 ) ) ;
#2347 = CARTESIAN_POINT ( 'NONE',  ( -1.614173228346456268, -0.5511811023622047445, 6.969142054262312111E-17 ) ) ;
#2348 = CARTESIAN_POINT ( 'NONE',  ( -0.1070741851644056997, 0.3996062992125984925, -1.815616797900262425 ) ) ;
#2349 = CARTESIAN_POINT ( 'NONE',  ( -1.496062992125983815, -0.1870078740157480879, -0.4822834645669291653 ) ) ;
#2350 = CARTESIAN_POINT ( 'NONE',  ( 0.5971128608923891301, 0.2952755905511810774, -0.1292274648535930714 ) ) ;
#2351 = CARTESIAN_POINT ( 'NONE',  ( 0.1377952755905518800, 0.1660481256975883668, -0.3530559997133364547 ) ) ;
#2352 = CARTESIAN_POINT ( 'NONE',  ( 1.082677165354331228, -0.5400638737290844871, 0.3530559997133364547 ) ) ;
#2353 = CARTESIAN_POINT ( 'NONE',  ( -0.3460692066303957537, -0.1998031496062994405, -0.9166666666666666297 ) ) ;
#2354 = CARTESIAN_POINT ( 'NONE',  ( 0.2925321140481932369, -0.2925321140481932369, -1.358267716535433101 ) ) ;
#2355 = CARTESIAN_POINT ( 'NONE',  ( 0.1974969037888704704, 0.3420746716998660508, -0.7742782152230970327 ) ) ;
#2356 = CARTESIAN_POINT ( 'NONE',  ( 4.797336870675656522E-17, -0.3917322834645670104, -0.07086614173228342195 ) ) ;
#2357 = CARTESIAN_POINT ( 'NONE',  ( -0.01312335958005186876, -0.3690944881889763329, 0.3153832671262228327 ) ) ;
#2358 = CARTESIAN_POINT ( 'NONE',  ( -0.4002624671916004129, -0.05778040916215560624, -0.4822834645669293319 ) ) ;
#2359 = CARTESIAN_POINT ( 'NONE',  ( 1.023622047244095112, -0.1870078740157480879, -0.4822834645669291653 ) ) ;
#2360 = CARTESIAN_POINT ( 'NONE',  ( -0.2891555358219909388, -0.2891555358219912164, -1.868110236220472009 ) ) ;
#2361 = CARTESIAN_POINT ( 'NONE',  ( -0.1181102362204717315, -0.5511811023622047445, 6.969142054262312111E-17 ) ) ;
#2362 = ADVANCED_FACE ( 'NONE', ( #26631 ), #20741, .T. ) ;
#2363 = CARTESIAN_POINT ( 'NONE',  ( -1.332020997375327642, -0.05778040916215522460, 0.4822834645669289988 ) ) ;
#2364 = CARTESIAN_POINT ( 'NONE',  ( -1.509186351706035767, -0.4281496062992124485, 0.4176697321401328655 ) ) ;
#2365 = CARTESIAN_POINT ( 'NONE',  ( -0.3458507752293909498, 0.3458507752293907833, -2.224409448818897239 ) ) ;
#2366 = CARTESIAN_POINT ( 'NONE',  ( 0.1988659768032885744, -0.3401783215957593365, -2.755905511811026276 ) ) ;
#2367 = ORIENTED_EDGE ( 'NONE', *, *, #75384, .F. ) ;
#2368 = ORIENTED_EDGE ( 'NONE', *, *, #32892, .F. ) ;
#2369 = CARTESIAN_POINT ( 'NONE',  ( 0.8661417322834652488, -0.1870078740157480879, -0.4822834645669291653 ) ) ;
#2370 = CARTESIAN_POINT ( 'NONE',  ( -1.725721784776902190, -0.05778040916215522460, 0.4822834645669289988 ) ) ;
#2372 = CARTESIAN_POINT ( 'NONE',  ( -1.010498687664041384, 0.05413385826771666132, 0.4176697321401328100 ) ) ;
#2371 = CARTESIAN_POINT ( 'NONE',  ( -1.384514435695537005, -0.5511811023622048555, -0.09757992244046775898 ) ) ;
#2373 = CARTESIAN_POINT ( 'NONE',  ( 0.1049643490035303689, 0.3917322834645668994, -2.593156537236534387 ) ) ;
#2374 = CARTESIAN_POINT ( 'NONE',  ( 0.3129921259842520787, 1.496062992125984259, 0.000000000000000000 ) ) ;
#2375 = CARTESIAN_POINT ( 'NONE',  ( 1.036745406824147731, 0.05413385826771666132, 0.4176697321401328100 ) ) ;
#2376 = CARTESIAN_POINT ( 'NONE',  ( -0.4091458600556402980, -0.2362204724409451284, -2.414698162729658648 ) ) ;
#2377 = CARTESIAN_POINT ( 'NONE',  ( -0.2624671916010490880, 0.2306618581243847221, -0.2411417322834647770 ) ) ;
#2378 = CARTESIAN_POINT ( 'NONE',  ( -0.2821522309711278487, 0.2952755905511811885, 0.1292274648535926551 ) ) ;
#2379 = CARTESIAN_POINT ( 'NONE',  ( -1.272965879265091305, 0.05413385826771626580, -0.4176697321401330321 ) ) ;
#2380 = CARTESIAN_POINT ( 'NONE',  ( 0.2867679344610365999, -0.2867679344610365999, -2.698143413876953556 ) ) ;
#2381 = CARTESIAN_POINT ( 'NONE',  ( 0.6627296587926515548, 0.2952755905511811885, 0.1292274648535926551 ) ) ;
#2382 = CARTESIAN_POINT ( 'NONE',  ( 0.3917322834645670104, -0.1049643490035303411, -1.993438320209974135 ) ) ;
#2383 = CARTESIAN_POINT ( 'NONE',  ( -1.377952755905511140, -0.5511811023622047445, 6.969142054262312111E-17 ) ) ;
#2384 = EDGE_LOOP ( 'NONE', ( #24775, #59378, #3391, #53814 ) ) ;
#2385 = CARTESIAN_POINT ( 'NONE',  ( 4.837279021331060870E-17, -0.3949938075777409963, -2.440944881889763884 ) ) ;
#2386 = VERTEX_POINT ( 'NONE', #1388 ) ;
#2387 = CARTESIAN_POINT ( 'NONE',  ( 1.586052503253845281, 1.299212598425198095, 0.1653254495020587411 ) ) ;
#2388 = VECTOR ( 'NONE', #42915, 39.37007874015748854 ) ;
#2389 = CARTESIAN_POINT ( 'NONE',  ( -1.496062992125983815, -0.1870078740157480879, -0.4822834645669291653 ) ) ;
#2390 = CARTESIAN_POINT ( 'NONE',  ( -1.318897637795274802, 0.1660481256975885056, 0.3530559997133364547 ) ) ;
#2391 = CARTESIAN_POINT ( 'NONE',  ( -9.787531504996567848E-17, 0.3996062992125986035, -0.4724409448818898127 ) ) ;
#2392 = CARTESIAN_POINT ( 'NONE',  ( -1.607611548556429737, -0.6692913385826771977, 0.1292274648535927661 ) ) ;
#2393 = CARTESIAN_POINT ( 'NONE',  ( -1.719160104986876103, 0.05413385826771666132, 0.4176697321401328100 ) ) ;
#2394 = LINE ( 'NONE', #80257, #1997 ) ;
#2395 = CARTESIAN_POINT ( 'NONE',  ( 0.02500110683995874009, -0.3941128856533797631, -2.755905511810075481 ) ) ;
#2396 = CARTESIAN_POINT ( 'NONE',  ( 0.1049643490035304938, -0.3917322834645669549, -0.01246719160104995359 ) ) ;
#2397 = CARTESIAN_POINT ( 'NONE',  ( 0.08530183727034192087, -0.08942795157527998196, 0.3641732283464567121 ) ) ;
#2398 = CARTESIAN_POINT ( 'NONE',  ( -0.6299212598425188991, -0.1870078740157479769, 0.3641732283464567677 ) ) ;
#2399 = CARTESIAN_POINT ( 'NONE',  ( -1.377952755905511140, -0.6692913385826771977, 8.415575281601705876E-17 ) ) ;
#2400 = CARTESIAN_POINT ( 'NONE',  ( 0.7874015748031503170, -0.1870078740157479769, 0.4822834645669291653 ) ) ;
#2401 = CARTESIAN_POINT ( 'NONE',  ( -0.9711286089238838626, 0.2306618581243847221, -0.2411417322834647770 ) ) ;
#2402 = CARTESIAN_POINT ( 'NONE',  ( -0.1958661417322836718, 0.3392501089628017219, -0.005249343832020952200 ) ) ;
#2403 = ORIENTED_EDGE ( 'NONE', *, *, #16301, .F. ) ;
#2404 = CARTESIAN_POINT ( 'NONE',  ( -1.325459317585300889, 0.05413385826771666132, 0.4176697321401328100 ) ) ;
#2405 = CARTESIAN_POINT ( 'NONE',  ( -1.686351706036744558, 0.1771653543307087075, -0.09757992244046823083 ) ) ;
#2406 = DIRECTION ( 'NONE',  ( 0.000000000000000000, 0.000000000000000000, 1.000000000000000000 ) ) ;
#2407 = CARTESIAN_POINT ( 'NONE',  ( -0.3458507752293906723, -0.3458507752293910609, -1.161417322834645383 ) ) ;
#2408 = CARTESIAN_POINT ( 'NONE',  ( 1.863753233923691965, 1.077434660671932942, -0.1173752429317785756 ) ) ;
#2409 = CARTESIAN_POINT ( 'NONE',  ( 0.3392501089628018884, -0.1958661417322834220, -0.7270341207349080292 ) ) ;
#2410 = CARTESIAN_POINT ( 'NONE',  ( 0.1958661417322836440, -0.3392501089628017219, -2.381233595800524849 ) ) ;
#2411 = CARTESIAN_POINT ( 'NONE',  ( -0.5249343832020990641, 0.2306618581243848609, 0.2411417322834645549 ) ) ;
#2412 = CARTESIAN_POINT ( 'NONE',  ( -1.437007874015747477, 0.07958543189024071263, -0.2665933059059888421 ) ) ;
#2413 = CARTESIAN_POINT ( 'NONE',  ( 0.3460692066303959202, -0.1998031496062991630, 0.1332020997375328031 ) ) ;
#2415 = CARTESIAN_POINT ( 'NONE',  ( 0.4498537592782897998, 0.000000000000000000, 2.118110236220472675 ) ) ;
#2414 = CARTESIAN_POINT ( 'NONE',  ( -1.528871391076114250, 0.2952755905511810774, -0.1292274648535930714 ) ) ;
#2416 = EDGE_CURVE ( 'NONE', #61855, #9282, #51866, .T. ) ;
#2417 = CARTESIAN_POINT ( 'NONE',  ( -1.614173228346456268, -0.6692913385826771977, 8.415575281601705876E-17 ) ) ;
#2418 = CARTESIAN_POINT ( 'NONE',  ( -0.5183727034120726440, -0.6692913385826773087, -0.1292274648535924053 ) ) ;
#2419 = CARTESIAN_POINT ( 'NONE',  ( 0.3917322834645668994, 0.1049643490035304522, 0.1102555362542800566 ) ) ;
#2420 = CARTESIAN_POINT ( 'NONE',  ( 0.4461942257217855201, -0.5023911411419708095, 0.1820866141732285504 ) ) ;
#2421 = CARTESIAN_POINT ( 'NONE',  ( 0.3917322834645669549, 0.1049643490035304660, -0.05183727034120743510 ) ) ;
#2422 = EDGE_CURVE ( 'NONE', #38486, #17299, #71250, .T. ) ;
#2423 = CARTESIAN_POINT ( 'NONE',  ( 0.3674540682414705883, -0.5023911411419708095, 0.1820866141732285504 ) ) ;
#2424 = CARTESIAN_POINT ( 'NONE',  ( 0.7874015748031503170, -0.1870078740157479769, 0.3641732283464567677 ) ) ;
#2425 = CARTESIAN_POINT ( 'NONE',  ( 1.135170603674541256, 0.2952755905511811885, 0.1292274648535926551 ) ) ;
#2426 = CARTESIAN_POINT ( 'NONE',  ( -0.3477690288713902178, 0.1771653543307087075, -0.09757992244046823083 ) ) ;
#2427 = CARTESIAN_POINT ( 'NONE',  ( -0.3392501089628017219, -0.1958661417322836718, -2.091863517060367439 ) ) ;
#2428 = CARTESIAN_POINT ( 'NONE',  ( -1.128608923884513837, 0.2306618581243847221, -0.2411417322834647770 ) ) ;
#2429 = CARTESIAN_POINT ( 'NONE',  ( -0.1115485564304456306, 0.1771653543307087075, -0.09757992244046823083 ) ) ;
#2430 = CARTESIAN_POINT ( 'NONE',  ( -1.384514435695537005, -0.5511811023622048555, -0.09757992244046775898 ) ) ;
#2431 = CARTESIAN_POINT ( 'NONE',  ( 0.3458507752293908943, -0.3458507752293908943, -0.4901574803149606474 ) ) ;
#2432 = CARTESIAN_POINT ( 'NONE',  ( -0.8070866141732276899, 0.07958543189024071263, -0.2665933059059888421 ) ) ;
#2433 = CARTESIAN_POINT ( 'NONE',  ( 0.1181102362204724532, -0.09842519685039369248, 5.158493410915829266E-18 ) ) ;
#2434 = CARTESIAN_POINT ( 'NONE',  ( -0.2165354330708654795, 0.1660481256975885056, 0.3530559997133364547 ) ) ;
#2435 = CARTESIAN_POINT ( 'NONE',  ( 1.555118110236221041, 0.07958543189024071263, -0.2665933059059888421 ) ) ;
#2436 = CARTESIAN_POINT ( 'NONE',  ( 0.3608923884514443348, 0.1771653543307087075, -0.09757992244046823083 ) ) ;
#2437 = CARTESIAN_POINT ( 'NONE',  ( -0.4199475065616791736, 0.1283753931104746893, -0.1820866141732285504 ) ) ;
#2438 = CARTESIAN_POINT ( 'NONE',  ( -0.4396325459317577122, -0.6692913385826773087, -0.1292274648535924053 ) ) ;
#2439 = CARTESIAN_POINT ( 'NONE',  ( -1.719160104986876103, 0.05413385826771666132, 0.4176697321401328100 ) ) ;
#2440 = CARTESIAN_POINT ( 'NONE',  ( -1.240157480314959759, -0.4536011799217368745, -0.2665933059059886201 ) ) ;
#2441 = CARTESIAN_POINT ( 'NONE',  ( -0.9573014326657163231, -2.609869883881465018E-15, -0.3464511005275220379 ) ) ;
#2442 = CARTESIAN_POINT ( 'NONE',  ( 0.6102362204724416372, 0.1660481256975883668, -0.3530559997133364547 ) ) ;
#2443 = EDGE_LOOP ( 'NONE', ( #26697, #75686, #7352, #68019 ) ) ;
#2444 = CARTESIAN_POINT ( 'NONE',  ( -0.2925321140481932369, 0.2925321140481931259, -1.671259842519685179 ) ) ;
#2445 = CARTESIAN_POINT ( 'NONE',  ( -1.604771003085130099, 1.320215725944019480, -0.1466069496707743947 ) ) ;
#2446 = CARTESIAN_POINT ( 'NONE',  ( -0.03937007874015669567, -0.5511811023622047445, 6.969142054262312111E-17 ) ) ;
#2447 = CIRCLE ( 'NONE', #37334, 3.267716535433071279 ) ;
#2448 = CARTESIAN_POINT ( 'NONE',  ( -0.3608923884514428360, -0.6692913385826773087, -0.1292274648535924053 ) ) ;
#2449 = CARTESIAN_POINT ( 'NONE',  ( -1.535433070866141225, -0.6692913385826771977, 8.415575281601705876E-17 ) ) ;
#2450 = CARTESIAN_POINT ( 'NONE',  ( 1.555118110236221041, 0.1660481256975883668, -0.3530559997133364547 ) ) ;
#2451 = CARTESIAN_POINT ( 'NONE',  ( 1.259842519685040019, -0.1870078740157480879, -0.4822834645669291653 ) ) ;
#2452 = CARTESIAN_POINT ( 'NONE',  ( -0.6299212598425188991, -0.1870078740157479769, 0.3641732283464567677 ) ) ;
#2453 = CARTESIAN_POINT ( 'NONE',  ( -1.092353285368623750, -2.191421614605370878E-15, 0.4445507791589071167 ) ) ;
#2454 = CARTESIAN_POINT ( 'NONE',  ( -0.1070741851644051862, -0.3996062992125987146, -0.2296587926509186250 ) ) ;
#2455 = CARTESIAN_POINT ( 'NONE',  ( -0.1049643490035302301, -0.3917322834645671770, -2.588601992947193509 ) ) ;
#2456 = CARTESIAN_POINT ( 'NONE',  ( 0.4741627488320241390, 1.554989095716459380, -2.554874958603176704 ) ) ;
#2457 = CARTESIAN_POINT ( 'NONE',  ( 0.9711286089238851948, 0.1283753931104748280, 0.1820866141732283561 ) ) ;
#2458 = LINE ( 'NONE', #54186, #1122 ) ;
#2459 = CARTESIAN_POINT ( 'NONE',  ( 0.9645669291338588858, 0.1660481256975885056, 0.3530559997133364547 ) ) ;
#2460 = CARTESIAN_POINT ( 'NONE',  ( -0.3917322834645670104, -7.196005306013484475E-17, -2.486220472440944906 ) ) ;
#2461 = CARTESIAN_POINT ( 'NONE',  ( 1.200787401574803681, 0.07958543189024085140, 0.2665933059059887866 ) ) ;
#2462 = CARTESIAN_POINT ( 'NONE',  ( 0.01312335958005323398, -0.4281496062992127816, -0.4176697321401328100 ) ) ;
#2463 = CARTESIAN_POINT ( 'NONE',  ( -0.5905511811023613777, -0.6692913385826771977, 8.415575281601705876E-17 ) ) ;
#2464 = CARTESIAN_POINT ( 'NONE',  ( 1.574803149606299746, -0.1870078740157480879, -0.4822834645669291653 ) ) ;
#2465 = CARTESIAN_POINT ( 'NONE',  ( 0.3460692066303959202, 0.1998031496062993295, -2.020997375328084100 ) ) ;
#2466 = CARTESIAN_POINT ( 'NONE',  ( 0.5183727034120741983, 0.1771653543307087075, -0.09757992244046823083 ) ) ;
#2467 = ORIENTED_EDGE ( 'NONE', *, *, #42363, .F. ) ;
#2468 = CARTESIAN_POINT ( 'NONE',  ( -0.2867679344610365444, -0.2867679344610367664, -0.5282345388789521090 ) ) ;
#2469 = ORIENTED_EDGE ( 'NONE', *, *, #21253, .T. ) ;
#2470 = CARTESIAN_POINT ( 'NONE',  ( -0.4330708661417315697, 0.2952755905511811885, 0.000000000000000000 ) ) ;
#2471 = CARTESIAN_POINT ( 'NONE',  ( 1.305774278215223960, 0.2952755905511810774, -0.1292274648535930714 ) ) ;
#2472 = CARTESIAN_POINT ( 'NONE',  ( 0.1443569553805781891, 0.05413385826771626580, -0.4176697321401330321 ) ) ;
#2473 = CARTESIAN_POINT ( 'NONE',  ( -0.4986876640419939388, 0.1283753931104746893, -0.1820866141732285504 ) ) ;
#2474 = CARTESIAN_POINT ( 'NONE',  ( 0.6561679790026253567, -0.6046776061558809534, -0.2411417322834644161 ) ) ;
#2475 = CARTESIAN_POINT ( 'NONE',  ( -0.9186351706036736120, -0.6046776061558809534, -0.2411417322834644161 ) ) ;
#2476 = CARTESIAN_POINT ( 'NONE',  ( -0.4133858267716528645, 0.1660481256975883668, -0.3530559997133364547 ) ) ;
#2477 = CARTESIAN_POINT ( 'NONE',  ( -0.7874015748031489847, -0.1870078740157479769, 0.4822834645669291653 ) ) ;
#2478 = CARTESIAN_POINT ( 'NONE',  ( 1.108923884514436242, -0.05778040916215522460, 0.4822834645669289988 ) ) ;
#2479 = CARTESIAN_POINT ( 'NONE',  ( 0.7611548556430451917, -0.6046776061558807314, 0.2411417322834647770 ) ) ;
#2480 = CARTESIAN_POINT ( 'NONE',  ( 0.8989501312335964611, 0.2952755905511811885, 0.1292274648535926551 ) ) ;
#2481 = CARTESIAN_POINT ( 'NONE',  ( 0.2867679344610365999, -0.2867679344610365444, -0.4055118110236220486 ) ) ;
#2482 = CARTESIAN_POINT ( 'NONE',  ( 0.1968503937007881344, -0.5511811023622047445, 6.969142054262312111E-17 ) ) ;
#2483 = VERTEX_POINT ( 'NONE', #78829 ) ;
#2484 = CARTESIAN_POINT ( 'NONE',  ( 0.1058382717557500713, -0.3949938075777409408, -0.8727034120734908917 ) ) ;
#2485 = ORIENTED_EDGE ( 'NONE', *, *, #41074, .T. ) ;
#2486 = CARTESIAN_POINT ( 'NONE',  ( -1.010498687664041384, -0.3690944881889765550, -0.3153832671262227771 ) ) ;
#2487 = CARTESIAN_POINT ( 'NONE',  ( -0.1443569553805765515, -0.4281496062992127816, -0.4176697321401328100 ) ) ;
#2488 = CARTESIAN_POINT ( 'NONE',  ( 2.647175254740889105, 1.326002914239470920, 0.4256865378621380591 ) ) ;
#2489 = CARTESIAN_POINT ( 'NONE',  ( -0.1574803149606292529, -0.1870078740157479769, 0.4822834645669291653 ) ) ;
#2490 = CARTESIAN_POINT ( 'NONE',  ( -0.3149606299212590610, -0.1870078740157479769, 0.4822834645669291653 ) ) ;
#2491 = CARTESIAN_POINT ( 'NONE',  ( -1.489501312335957062, -0.05778040916215522460, 0.4822834645669289988 ) ) ;
#2492 = CARTESIAN_POINT ( 'NONE',  ( -1.469816272965878357, -0.6046776061558809534, -0.2411417322834644161 ) ) ;
#2493 = CARTESIAN_POINT ( 'NONE',  ( 1.410761154855643795, -0.08942795157528024563, -0.3641732283464568787 ) ) ;
#2494 = CARTESIAN_POINT ( 'NONE',  ( 0.3149606299212185934, 2.755905511811024056, 3.924389226575471845 ) ) ;
#2495 = CARTESIAN_POINT ( 'NONE',  ( 0.2952755905511810774, 3.597759587968672259E-17, 5.524802951929911998 ) ) ;
#2496 = CARTESIAN_POINT ( 'NONE',  ( 0.6758530183727039509, 0.1771653543307087075, -0.09757992244046823083 ) ) ;
#2497 = APPLICATION_CONTEXT ( 'automotive_design' ) ;
#2498 = CARTESIAN_POINT ( 'NONE',  ( 0.1902887139107617975, -0.6692913385826773087, -0.1292274648535924053 ) ) ;
#2499 = CARTESIAN_POINT ( 'NONE',  ( 0.3018372703412079971, 0.05413385826771626580, -0.4176697321401330321 ) ) ;
#2500 = VERTEX_POINT ( 'NONE', #7271 ) ;
#2501 = CARTESIAN_POINT ( 'NONE',  ( 0.3996062992125986035, 0.1070741851644054776, -1.856955380577427928 ) ) ;
#2502 = CARTESIAN_POINT ( 'NONE',  ( -0.5774278215223089816, 0.2306618581243847221, -0.2411417322834647770 ) ) ;
#2503 = CARTESIAN_POINT ( 'NONE',  ( -0.3460692066303960313, 0.1998031496062989965, -1.205380577427821454 ) ) ;
#2504 = CARTESIAN_POINT ( 'NONE',  ( 0.1998031496062994128, -0.3460692066303957537, -0.6410761154855643129 ) ) ;
#2505 = CARTESIAN_POINT ( 'NONE',  ( -0.7545931758530177724, 0.2952755905511811885, 0.1292274648535926551 ) ) ;
#2506 = CARTESIAN_POINT ( 'NONE',  ( 0.1265901696524989462, 0.4724409448818897572, 0.006561679790026246628 ) ) ;
#2507 = CARTESIAN_POINT ( 'NONE',  ( 0.2867679344610365999, 0.2867679344610365999, -2.427165354330708347 ) ) ;
#2508 = CARTESIAN_POINT ( 'NONE',  ( -1.541994750656167090, -0.5511811023622048555, -0.09757992244046775898 ) ) ;
#2509 = CARTESIAN_POINT ( 'NONE',  ( 0.7808398950131240079, -0.3162353388693405765, 0.4822834645669290543 ) ) ;
#2510 = CARTESIAN_POINT ( 'NONE',  ( 0.7677165354330716118, 0.1660481256975883668, -0.3530559997133364547 ) ) ;
#2511 = CARTESIAN_POINT ( 'NONE',  ( -0.04593175853018302557, 0.1771653543307087630, 0.09757992244046791164 ) ) ;
#2512 = CARTESIAN_POINT ( 'NONE',  ( -0.05249343832020938322, -0.6046776061558809534, -0.2411417322834644161 ) ) ;
#2513 = CARTESIAN_POINT ( 'NONE',  ( -0.1265901696524993347, 0.4724409448818895907, -2.130577427821522374 ) ) ;
#2514 = CARTESIAN_POINT ( 'NONE',  ( -0.2099737532808391705, 0.1283753931104748280, 0.1820866141732283561 ) ) ;
#2515 = CARTESIAN_POINT ( 'NONE',  ( -0.4921259842519677963, -0.5400638737290844871, 0.3530559997133364547 ) ) ;
#2516 = EDGE_CURVE ( 'NONE', #22229, #4461, #79229, .T. ) ;
#2517 = CARTESIAN_POINT ( 'NONE',  ( -0.1974969037888704149, -0.3420746716998661063, -2.032152230971128848 ) ) ;
#2518 = CARTESIAN_POINT ( 'NONE',  ( -1.692913385826770645, 0.2952755905511811885, 0.000000000000000000 ) ) ;
#2519 = CARTESIAN_POINT ( 'NONE',  ( 0.08530183727034192087, -0.2845877964562161244, -0.3641732283464567121 ) ) ;
#2520 = CARTESIAN_POINT ( 'NONE',  ( 1.692913385826772421, 0.1771653543307087630, 0.000000000000000000 ) ) ;
#2521 = CARTESIAN_POINT ( 'NONE',  ( -1.062992125984250968, 0.2952755905511811885, 0.000000000000000000 ) ) ;
#2522 = CARTESIAN_POINT ( 'NONE',  ( -0.5971128608923877978, -0.5511811023622048555, -0.09757992244046775898 ) ) ;
#2523 = DIRECTION ( 'NONE',  ( -0.000000000000000000, -1.000000000000000000, -0.000000000000000000 ) ) ;
#2524 = CARTESIAN_POINT ( 'NONE',  ( -0.6233595800524928121, -0.05778040916215522460, 0.4822834645669289988 ) ) ;
#2525 = CARTESIAN_POINT ( 'NONE',  ( -0.6233595800524928121, -0.3162353388693409650, -0.4822834645669289433 ) ) ;
#2526 = CARTESIAN_POINT ( 'NONE',  ( -0.09186351706036663400, -0.4281496062992124485, 0.4176697321401328655 ) ) ;
#2527 = CARTESIAN_POINT ( 'NONE',  ( -0.3460692066303957537, -0.1998031496062994405, -2.491469816272966042 ) ) ;
#2528 = CARTESIAN_POINT ( 'NONE',  ( -0.2867679344610364334, -0.2867679344610368219, -1.871371760333646606 ) ) ;
#2529 = CARTESIAN_POINT ( 'NONE',  ( -2.131037067002753194, 1.408244132531263570, -0.4567322424080928478 ) ) ;
#2530 = CARTESIAN_POINT ( 'NONE',  ( 0.4724409448818904789, -0.1870078740157480601, -0.3641732283464567677 ) ) ;
#2531 = CARTESIAN_POINT ( 'NONE',  ( 1.082677165354331228, -0.5400638737290844871, 0.3530559997133364547 ) ) ;
#2532 = CARTESIAN_POINT ( 'NONE',  ( -1.167979002624671470, -0.3690944881889765550, -0.3153832671262227771 ) ) ;
#2533 = CARTESIAN_POINT ( 'NONE',  ( 1.266404199475066328, -0.3162353388693409650, -0.4822834645669289433 ) ) ;
#2534 = CARTESIAN_POINT ( 'NONE',  ( -1.286089238845143479, -0.5023911411419708095, 0.1820866141732285504 ) ) ;
#2535 = CARTESIAN_POINT ( 'NONE',  ( -0.4330708661417315697, 0.2952755905511811885, 0.000000000000000000 ) ) ;
#2536 = CARTESIAN_POINT ( 'NONE',  ( 0.1574803149606306130, -0.1870078740157480601, -0.3641732283464567677 ) ) ;
#2537 = CARTESIAN_POINT ( 'NONE',  ( 1.606179739637289439, 0.2952685183143916592, 0.01196341948705389145 ) ) ;
#2538 = CARTESIAN_POINT ( 'NONE',  ( 0.6955380577427828781, -0.004921259842519870586, -0.3153832671262229437 ) ) ;
#2539 = CARTESIAN_POINT ( 'NONE',  ( 0.2230971128608932319, -0.4281496062992124485, 0.4176697321401328655 ) ) ;
#2540 = CARTESIAN_POINT ( 'NONE',  ( -0.2925321140481932369, 0.2925321140481931259, -0.09645669291338582196 ) ) ;
#2541 = CARTESIAN_POINT ( 'NONE',  ( -0.8267716535433065062, -0.6692913385826771977, 8.415575281601705876E-17 ) ) ;
#2542 = CARTESIAN_POINT ( 'NONE',  ( -0.3917322834645671215, 0.1049643490035301469, -1.692257217847769057 ) ) ;
#2543 = CARTESIAN_POINT ( 'NONE',  ( 1.141732283464567566, 0.1771653543307087630, 0.000000000000000000 ) ) ;
#2544 = CARTESIAN_POINT ( 'NONE',  ( 0.2230971128608932319, -0.4281496062992124485, 0.4176697321401328655 ) ) ;
#2545 = CARTESIAN_POINT ( 'NONE',  ( -0.3477690288713902178, 0.2952755905511810774, -0.1292274648535930714 ) ) ;
#2546 = CARTESIAN_POINT ( 'NONE',  ( -0.4658792650918627265, -0.2845877964562161244, -0.3641732283464567121 ) ) ;
#2547 = LINE ( 'NONE', #74080, #7790 ) ;
#2548 = CARTESIAN_POINT ( 'NONE',  ( -0.01968503937007793844, 0.07958543189024071263, -0.2665933059059888421 ) ) ;
#2549 = CARTESIAN_POINT ( 'NONE',  ( 0.3412073490813655186, -0.6046776061558809534, -0.2411417322834644161 ) ) ;
#2550 = CARTESIAN_POINT ( 'NONE',  ( -0.7086614173228339419, -0.1870078740157480601, -0.3641732283464567677 ) ) ;
#2551 = CARTESIAN_POINT ( 'NONE',  ( -0.3460692066303960313, 0.1998031496062989965, -0.8904199475065617264 ) ) ;
#2552 = CARTESIAN_POINT ( 'NONE',  ( -1.253280839895012377, -0.3162353388693409650, -0.4822834645669289433 ) ) ;
#2553 = CARTESIAN_POINT ( 'NONE',  ( -0.8550440751474861489, -4.966502543501560364E-15, 0.3954985857520076920 ) ) ;
#2554 = ORIENTED_EDGE ( 'NONE', *, *, #42674, .T. ) ;
#2555 = CARTESIAN_POINT ( 'NONE',  ( -1.049868766404198794, 0.1283753931104746893, -0.1820866141732285504 ) ) ;
#2556 = CARTESIAN_POINT ( 'NONE',  ( 0.1181102362204730916, -0.6692913385826771977, 8.415575281601705876E-17 ) ) ;
#2557 = CARTESIAN_POINT ( 'NONE',  ( -1.627296587926508442, -0.6046776061558809534, -0.2411417322834644161 ) ) ;
#2558 = CARTESIAN_POINT ( 'NONE',  ( -0.6692913385826764205, 0.2952755905511811885, 0.000000000000000000 ) ) ;
#2559 = DIRECTION ( 'NONE',  ( 0.000000000000000000, 0.000000000000000000, -1.000000000000000000 ) ) ;
#2560 = CARTESIAN_POINT ( 'NONE',  ( 1.358267716535433323, 0.1660481256975885056, 0.3530559997133364547 ) ) ;
#2561 = CARTESIAN_POINT ( 'NONE',  ( 0.7020997375328090762, -0.3162353388693405765, 0.4822834645669290543 ) ) ;
#2562 = CARTESIAN_POINT ( 'NONE',  ( -0.2559055118110230564, 0.1012011053420775880, -0.2882089793578257453 ) ) ;
#2563 = DIRECTION ( 'NONE',  ( -1.332267629550188539E-16, -1.000000000000000000, 0.000000000000000000 ) ) ;
#2564 = CARTESIAN_POINT ( 'NONE',  ( 0.2710655044954047299, -0.1174279065223611668, 5.568826803765086986 ) ) ;
#2565 = CARTESIAN_POINT ( 'NONE',  ( -1.607611548556429737, -0.6692913385826771977, 0.1292274648535927661 ) ) ;
#2566 = CARTESIAN_POINT ( 'NONE',  ( 0.1998031496062994405, -0.3460692066303958092, -0.4068241469816273326 ) ) ;
#2567 = ORIENTED_EDGE ( 'NONE', *, *, #11147, .F. ) ;
#2568 = CARTESIAN_POINT ( 'NONE',  ( -0.4658792650918627265, -0.2845877964562161244, -0.3641732283464567121 ) ) ;
#2569 = CARTESIAN_POINT ( 'NONE',  ( -0.2867679344610365999, 0.2867679344610364889, -2.216535433070866201 ) ) ;
#2570 = VERTEX_POINT ( 'NONE', #45553 ) ;
#2571 = CARTESIAN_POINT ( 'NONE',  ( 1.023622047244095112, -0.1870078740157480879, -0.4822834645669291653 ) ) ;
#2572 = CARTESIAN_POINT ( 'NONE',  ( 0.07874015748031558404, -0.1870078740157480879, -0.4822834645669291653 ) ) ;
#2573 = CARTESIAN_POINT ( 'NONE',  ( -0.6299212598425188991, -0.1870078740157480879, -0.4822834645669291653 ) ) ;
#2574 = CARTESIAN_POINT ( 'NONE',  ( 1.614173228346457378, -0.6692913385826771977, 8.415575281601705876E-17 ) ) ;
#2575 = CARTESIAN_POINT ( 'NONE',  ( -0.7808398950131222316, -0.2845877964562161244, -0.3641732283464567121 ) ) ;
#2576 = CYLINDRICAL_SURFACE ( 'NONE', #22505, 0.4724409448818898682 ) ;
#2577 = CARTESIAN_POINT ( 'NONE',  ( 0.3280839895013130669, -0.4281496062992127816, -0.4176697321401328100 ) ) ;
#2578 = CARTESIAN_POINT ( 'NONE',  ( 0.4068241469816279987, -0.3690944881889765550, -0.3153832671262227771 ) ) ;
#2579 = CARTESIAN_POINT ( 'NONE',  ( -0.6299212598425188991, -0.1870078740157480879, -0.4822834645669291653 ) ) ;
#2580 = CARTESIAN_POINT ( 'NONE',  ( -0.2867679344610366554, 0.2867679344610365444, -1.674521366632859110 ) ) ;
#2581 = CARTESIAN_POINT ( 'NONE',  ( -1.154855643044618851, 0.2306618581243848609, 0.2411417322834645549 ) ) ;
#2582 = DIRECTION ( 'NONE',  ( -3.096699300667737957E-16, 1.000000000000000000, -0.000000000000000000 ) ) ;
#2583 = CARTESIAN_POINT ( 'NONE',  ( 1.010498687664042716, -0.4281496062992124485, 0.4176697321401328655 ) ) ;
#2584 = CARTESIAN_POINT ( 'NONE',  ( 1.148293963254593875, -0.5511811023622046335, 0.09757992244046803654 ) ) ;
#2585 = VERTEX_POINT ( 'NONE', #45972 ) ;
#2586 = CARTESIAN_POINT ( 'NONE',  ( 0.3917322834645670659, 2.398668435337828261E-17, -2.949494381398636733 ) ) ;
#2587 = CARTESIAN_POINT ( 'NONE',  ( -0.5183727034120726440, 0.2952755905511811885, 0.1292274648535926551 ) ) ;
#2588 = VERTEX_POINT ( 'NONE', #46392 ) ;
#2589 = CARTESIAN_POINT ( 'NONE',  ( 0.4790026246719167324, -0.08942795157527998196, 0.3641732283464567121 ) ) ;
#2590 = CARTESIAN_POINT ( 'NONE',  ( -1.246719160104986512, 0.05413385826771666132, 0.4176697321401328100 ) ) ;
#2591 = CARTESIAN_POINT ( 'NONE',  ( 0.8792650918635177559, -0.4281496062992127816, -0.4176697321401328100 ) ) ;
#2592 = CARTESIAN_POINT ( 'NONE',  ( 0.6561679790026253567, 0.2306618581243848609, 0.2411417322834645549 ) ) ;
#2593 =( BOUNDED_SURFACE ( )  B_SPLINE_SURFACE ( 1, 2, ( 
 ( #66691, #9026, #79743, #22059, #70181, #12534, #30022, #67931, #80577, #22887, #49380, #68751, #80162, #48140, #55686, #48552, #29613, #68348, #75076, #11093, #61184, #17423, #42651, #73837, #10272, #56104, #61609, #3952, #43054, #36750, #28788, #42237, #55274, #67104, #9435, #35105, #74249, #23709, #81393, #10688, #16592, #35940, #54450, #80984, #62426, #81808, #60771, #3122, #22479, #67514, #16177, #4763, #30439, #23297, #41824, #47721, #35522, #73419, #9851, #48967, #3538, #29205, #54871, #74667, #17011, #36343, #62018, #4354, #15768, #41420, #5184, #18643, #63665, #43464, #69161, #11512, #50605, #115, #32092, #44695, #82619, #44287, #30848, #6005, #57753, #58171, #37168, #62848, #56513, #43877, #50200, #51431, #45117, #69575, #25354, #24935, #11923, #69977, #37578, #12332, #25770, #70825, #82216, #83031, #24534, #51016, #75897, #64086, #18237, #63251, #76715, #24120, #5591, #31257, #56925, #77134, #13172, #19048, #57335, #38822, #70392, #64500, #32508, #76312, #37989, #31674, #12747, #38406, #49789, #6423, #19467, #6838, #75491, #17830, #14008, #21146, #58598, #59023, #72904, #64923, #967, #26621, #52275, #32933, #7261, #77979, #14841, #65773, #46801, #72075, #77561, #46382, #66182, #14434, #72492, #27447, #20309, #59432, #40501, #34186, #39665, #7693, #2202, #65355, #33360, #52691, #1379, #53108, #27030, #78817, #39238, #45959, #66597, #26193, #8519, #20731, #78399, #40086, #27870, #21553, #71656, #8105, #59850, #33771, #1787, #53530, #79238, #47214, #15256, #40915, #8931, #34608, #540, #51854, #19895, #45542, #71240, #13584, #15673, #3031, #42961, #2623, #42555, #80482, #9757, #35429, #61920, #81300, #9347, #60682, #68259, #61094, #42146, #80889, #4262, #23614, #73749, #29925, #55180, #28697, #22795, #68655, #74155, #16502, #55588, #49283, #41334, #54779, #67841, #79653, #21970, #47632, #3445, #36251, #10595, #23202, #29109, #48455, #67014, #10180, #74986, #10992, #73326, #35018, #54359, #80071, #22388, #17331, #60273, #48048, #61514, #35845, #16085, #3859, #41730, #29519, #28279, #53941, #67424, #48873, #74573, #16918, #37068, #76618, #62753, #69063, #5903, #70715, #30757, #5089, #56419, #6315, #25669, #31575, #69882, #15, #12236, #77033, #45015, #43774, #11830, #31158, #50507, #57230, #36653, #18949, #31992, #76211, #4665, #18547, #50101, #82932, #11413, #37483, #51329, #17734, #82119, #24434, #75797, #18140, #43362, #69477, #50918, #44192, #25254, #24839, #30338, #82522, #44596, #37892, #70291, #63568, #63156, #12643, #38305, #63979, #5496, #56825, #57653, #19365, #62328, #56004, #81715, #24025, #49693, #75388, #6734, #26089, #71134, #32405, #58067, #19787, #46279, #33668, #72393, #77452, #45855, #71975, #33258, #13066, #13477, #51749, #434, #47111, #71553, #38720, #14743, #45439, #78716, #32827, #39135, #8004, #53429, #64398, #8414, #20628, #66078, #64815, #14329, #13902, #40396, #21041, #7156, #46700, #39987, #52588, #78296, #58495, #39560, #58920, #859, #26516, #52171, #34081, #26928, #20204, #77874, #59745, #65677, #65249, #7586, #59330, #1279, #2099, #1686, #27345, #53003, #27764, #79137, #21454, #21863, #80786, #3755, #40807, #23102, #15988, #60992, #41635, #54254, #29419, #8826, #66491, #74051, #67325, #2933, #4162, #34503, #60167, #2521, #3341, #41229, #48770, #29005, #35329, #79970, #28179, #23515, #54671, #66916, #53836, #29827, #60582, #55490, #79550, #80382, #34920, #15569, #73219, #28597, #47528, #9248, #22283, #74469, #16816, #42452, #61822, #55078, #47943, #73646, #9659, #22695, #68152, #10496, #16399, #48354, #72801, #42045, #67741, #10074, #35738, #61406, #36150, #81200, #15150, #69793, #37392, #42863, #11737, #31478, #63064, #12139, #76116, #17636, #24749, #37795, #82836, #4995, #56326, #50826, #30663, #82025, #18047, #50008, #18457, #24338, #44100, #4572, #75293, #31895, #74887, #57139, #69383, #75706, #43680, #76528, #70193, #81618, #49599, #25158, #5401, #31064, #63473, #18856, #12548, #62654, #44503, #5808, #43268, #56732, #57556, #82430, #50416, #38206, #63880, #30243, #6219, #83247, #68556, #10897, #36557, #49184 ),
 ( #17233, #62234, #68966, #55906, #23932, #36974, #11315, #45343, #20110, #27247, #72297, #32308, #1181, #57969, #26832, #25991, #65574, #51649, #336, #78198, #59646, #19685, #77353, #71039, #78620, #14643, #20529, #58824, #40299, #52490, #65980, #33984, #32729, #756, #45758, #39462, #46181, #25570, #7908, #20943, #65149, #76934, #7485, #39036, #71878, #13383, #26417, #8317, #6636, #64719, #7060, #58396, #52070, #52906, #64302, #33569, #77777, #71455, #14227, #51235, #19262, #46601, #33155, #44915, #70612, #39887, #13804, #12967, #59231, #1592, #38624, #60894, #41541, #67230, #60069, #28494, #22186, #53330, #15471, #36056, #35644, #15892, #9152, #21765, #80694, #3245, #34825, #54154, #35230, #79869, #74370, #48260, #47843, #73956, #79039, #9560, #60482, #34401, #9974, #16303, #21358, #61304, #73549, #28909, #54572, #66819, #41945, #47011, #72705, #80286, #22599, #41128, #16714, #15052, #40708, #66393, #67641, #53738, #3662, #29325, #54986, #2833, #8731, #2002, #23007, #79446, #2424, #42354, #73120, #68052, #28080, #48674, #47428, #10399, #27664, #17539, #81101, #17135, #55394, #69694, #37694, #12037, #50728, #76015, #81512, #75195, #23834, #62554, #31375, #5703, #62967, #81927, #61728, #5305, #17947, #23418, #29732, #68463, #76427, #37292, #44399, #49084, #74784, #36461, #42767, #10801, #62135, #11632, #82332, #63369, #4475, #11216, #30964, #24238, #4065, #30145, #55806, #49502, #12445, #36876, #43171, #68867, #4889, #30563, #56229, #18357, #43584, #24650, #49911, #75608, #69285, #44001, #56631, #50318, #57040, #82734, #25053, #18755, #70091, #77249, #45238, #39774, #19578, #70938, #6953, #38935, #65037, #13283, #33042, #76827, #64204, #20839, #63780, #20423, #58285, #64615, #32623, #65469, #59130, #70506, #38521, #46076, #651, #20004, #58711, #7803, #1487, #51545, #33468, #1076, #6538, #26308, #46491, #51966, #77674, #27141, #52805, #19160, #45655, #71350, #57454, #83147, #25467, #13697, #14122, #71769, #26729, #39353, #7373, #44810, #52383, #78515, #72186, #51133, #12864, #32208, #57866, #233, #38104, #6119, #25884, #78092, #31791, #2317, #9045, #34300, #34720, #16197, #62340, #21252, #73437, #46907, #15787, #14948, #54470, #40607, #72602, #67123, #49706, #8629, #66290, #59961, #67533, #4679, #9453, #47739, #30350, #41439, #56019, #24036, #21663, #73014, #60380, #28389, #35124, #14544, #80183, #9871, #54049, #65879, #79763, #27977, #60790, #53635, #15365, #81727, #78930, #79343, #47323, #59545, #33879, #41026, #73856, #22498, #3143, #66712, #2728, #22080, #28806, #48161, #40196, #1900, #27561, #53220, #41843, #35540, #8214, #13081, #11840, #76628, #76225, #63168, #69892, #37493, #12246, #77044, #38734, #82131, #50930, #24445, #18959, #75810, #32005, #18153, #50113, #44607, #26101, #69491, #43785, #5506, #45028, #64411, #70303, #25264, #6746, #12656, #32418, #446, #82533, #50519, #37902, #5913, #38317, #75401, #57665, #70727, #31587, #43376, #57242, #31169, #63991, #56835, #18558, #58080, #56429, #24851, #44202, #63579, #82946, #6332, #27, #25680, #51340, #19376, #17747, #69076, #11426, #37080, #62767, #5101, #30768, #20219, #27357, #40410, #2113, #7599, #58933, #53442, #33273, #1291, #20640, #52602, #78730, #26940, #46714, #7169, #77888, #34516, #77465, #34095, #71988, #78308, #46292, #79150, #72815, #872, #52184, #59758, #14341, #33680, #72406, #21467, #15164, #65263, #47125, #14755, #45868, #40001, #60181, #65689, #8017, #40821, #66506, #32840, #59342, #1699, #71149, #71566, #53016, #13916, #21054, #8840, #2534, #66091, #8426, #51763, #27778, #19802, #45451, #13490, #58509, #39146, #64830, #26531, #39573, #41241, #2945, #47542, #73232, #34933, #61418, #48783, #4174, #9261, #61005, #3768, #48366, #28192, #28609, #66929, #15583, #62243, #3354, #53850, #29838, #60596, #10507, #47956, #54267, #23116, #68566, #79563, #23525, #35752, #81210, #79982, #29432, #29019, #55501, #36160, #22295, #61834, #55090, #67753, #10087, #73659, #54685, #74065, #21877, #41648, #16001, #49195, #42057, #35342, #67339, #74896, #80799, #80396, #22708, #74481, #16411 ) ),
 .UNSPECIFIED., .F., .F., .F. ) 
 B_SPLINE_SURFACE_WITH_KNOTS ( ( 2, 2 ),
 ( 3, 2, 2, 2, 2, 2, 2, 2, 2, 2, 2, 2, 2, 2, 2, 2, 2, 2, 2, 2, 2, 2, 2, 2, 2, 2, 2, 2, 2, 2, 2, 2, 2, 2, 2, 2, 2, 2, 2, 2, 2, 2, 2, 2, 2, 2, 2, 2, 2, 2, 2, 2, 2, 2, 2, 2, 2, 2, 2, 2, 2, 2, 2, 2, 2, 2, 2, 2, 2, 2, 2, 2, 2, 2, 2, 2, 2, 2, 2, 2, 2, 2, 2, 2, 2, 2, 2, 2, 2, 2, 2, 2, 2, 2, 2, 2, 2, 2, 2, 2, 2, 2, 2, 2, 2, 2, 2, 2, 2, 2, 2, 2, 2, 2, 2, 2, 2, 2, 2, 2, 2, 2, 2, 2, 2, 2, 2, 2, 2, 2, 2, 2, 2, 2, 2, 2, 2, 2, 2, 2, 2, 2, 2, 2, 2, 2, 2, 2, 2, 2, 2, 2, 2, 2, 2, 2, 2, 2, 2, 2, 2, 2, 2, 2, 2, 2, 2, 2, 2, 2, 2, 2, 2, 2, 2, 2, 2, 2, 2, 2, 2, 2, 2, 2, 2, 2, 2, 2, 2, 2, 2, 2, 2, 2, 2, 2, 2, 2, 2, 2, 2, 2, 2, 2, 2, 2, 2, 2, 2, 2, 2, 2, 2, 2, 2, 2, 2, 2, 2, 2, 2, 2, 2, 2, 2, 2, 2, 2, 2, 2, 2, 2, 2, 2, 2, 2, 2, 2, 2, 2, 2, 2, 2, 2, 2, 2, 2, 2, 2, 2, 2, 2, 2, 2, 2, 3 ),
 ( 0.000000000000000000, 1.000000000000000000 ),
 ( 0.000000000000000000, 0.003787878787878787984, 0.007575757575757575968, 0.01136363636363636395, 0.01515151515151515194, 0.01893939393939393992, 0.02272727272727272790, 0.02651515151515151589, 0.03030303030303030387, 0.03409090909090908839, 0.03787878787878787984, 0.04166666666666666435, 0.04545454545454545581, 0.04924242424242424032, 0.05303030303030303177, 0.05681818181818181629, 0.06060606060606060774, 0.06439393939393939226, 0.06818181818181817677, 0.07196969696969697516, 0.07575757575757575968, 0.07954545454545454419, 0.08333333333333332871, 0.08712121212121212710, 0.09090909090909091161, 0.09469696969696969613, 0.09848484848484848064, 0.1022727272727272790, 0.1060606060606060635, 0.1098484848484848481, 0.1136363636363636326, 0.1174242424242424310, 0.1212121212121212155, 0.1250000000000000000, 0.1287878787878787845, 0.1325757575757575690, 0.1363636363636363535, 0.1401515151515151381, 0.1439393939393939503, 0.1477272727272727348, 0.1515151515151515194, 0.1553030303030303039, 0.1590909090909090884, 0.1628787878787878729, 0.1666666666666666574, 0.1704545454545454419, 0.1742424242424242542, 0.1780303030303030387, 0.1818181818181818232, 0.1856060606060606077, 0.1893939393939393923, 0.1931818181818181768, 0.1969696969696969613, 0.2007575757575757458, 0.2045454545454545581, 0.2083333333333333426, 0.2121212121212121271, 0.2159090909090909116, 0.2196969696969696961, 0.2234848484848484806, 0.2272727272727272652, 0.2310606060606060497, 0.2348484848484848619, 0.2386363636363636465, 0.2424242424242424310, 0.2462121212121212155, 0.2500000000000000000, 0.2537878787878787845, 0.2575757575757575690, 0.2613636363636363535, 0.2651515151515151381, 0.2689393939393939226, 0.2727272727272727071, 0.2765151515151514916, 0.2803030303030302761, 0.2840909090909091161, 0.2878787878787879007, 0.2916666666666666852, 0.2954545454545454697, 0.2992424242424242542, 0.3030303030303030387, 0.3068181818181818232, 0.3106060606060606077, 0.3143939393939393923, 0.3181818181818181768, 0.3219696969696969613, 0.3257575757575757458, 0.3295454545454545303, 0.3333333333333333148, 0.3371212121212120993, 0.3409090909090908839, 0.3446969696969697239, 0.3484848484848485084, 0.3522727272727272929, 0.3560606060606060774, 0.3598484848484848619, 0.3636363636363636465, 0.3674242424242424310, 0.3712121212121212155, 0.3750000000000000000, 0.3787878787878787845, 0.3825757575757575690, 0.3863636363636363535, 0.3901515151515151381, 0.3939393939393939226, 0.3977272727272727071, 0.4015151515151514916, 0.4053030303030302761, 0.4090909090909091161, 0.4128787878787879007, 0.4166666666666666852, 0.4204545454545454697, 0.4242424242424242542, 0.4280303030303030387, 0.4318181818181818232, 0.4356060606060606077, 0.4393939393939393923, 0.4431818181818181768, 0.4469696969696969613, 0.4507575757575757458, 0.4545454545454545303, 0.4583333333333333148, 0.4621212121212120993, 0.4659090909090908839, 0.4696969696969697239, 0.4734848484848485084, 0.4772727272727272929, 0.4810606060606060774, 0.4848484848484848619, 0.4886363636363636465, 0.4924242424242424310, 0.4962121212121212155, 0.5000000000000000000, 0.5037878787878787845, 0.5075757575757575690, 0.5113636363636363535, 0.5151515151515151381, 0.5189393939393939226, 0.5227272727272727071, 0.5265151515151514916, 0.5303030303030302761, 0.5340909090909090606, 0.5378787878787878451, 0.5416666666666666297, 0.5454545454545454142, 0.5492424242424241987, 0.5530303030303029832, 0.5568181818181817677, 0.5606060606060605522, 0.5643939393939394478, 0.5681818181818182323, 0.5719696969696970168, 0.5757575757575758013, 0.5795454545454545858, 0.5833333333333333703, 0.5871212121212121549, 0.5909090909090909394, 0.5946969696969697239, 0.5984848484848485084, 0.6022727272727272929, 0.6060606060606060774, 0.6098484848484848619, 0.6136363636363636465, 0.6174242424242424310, 0.6212121212121212155, 0.6250000000000000000, 0.6287878787878787845, 0.6325757575757575690, 0.6363636363636363535, 0.6401515151515151381, 0.6439393939393939226, 0.6477272727272727071, 0.6515151515151514916, 0.6553030303030302761, 0.6590909090909090606, 0.6628787878787878451, 0.6666666666666666297, 0.6704545454545454142, 0.6742424242424241987, 0.6780303030303029832, 0.6818181818181817677, 0.6856060606060605522, 0.6893939393939394478, 0.6931818181818182323, 0.6969696969696970168, 0.7007575757575758013, 0.7045454545454545858, 0.7083333333333333703, 0.7121212121212121549, 0.7159090909090909394, 0.7196969696969697239, 0.7234848484848485084, 0.7272727272727272929, 0.7310606060606060774, 0.7348484848484848619, 0.7386363636363636465, 0.7424242424242424310, 0.7462121212121212155, 0.7500000000000000000, 0.7537878787878787845, 0.7575757575757575690, 0.7613636363636363535, 0.7651515151515151381, 0.7689393939393939226, 0.7727272727272727071, 0.7765151515151514916, 0.7803030303030302761, 0.7840909090909090606, 0.7878787878787878451, 0.7916666666666666297, 0.7954545454545454142, 0.7992424242424241987, 0.8030303030303029832, 0.8068181818181817677, 0.8106060606060605522, 0.8143939393939394478, 0.8181818181818182323, 0.8219696969696970168, 0.8257575757575758013, 0.8295454545454545858, 0.8333333333333333703, 0.8371212121212121549, 0.8409090909090909394, 0.8446969696969697239, 0.8484848484848485084, 0.8522727272727272929, 0.8560606060606060774, 0.8598484848484848619, 0.8636363636363636465, 0.8674242424242424310, 0.8712121212121212155, 0.8750000000000000000, 0.8787878787878787845, 0.8825757575757575690, 0.8863636363636363535, 0.8901515151515151381, 0.8939393939393939226, 0.8977272727272727071, 0.9015151515151514916, 0.9053030303030302761, 0.9090909090909090606, 0.9128787878787878451, 0.9166666666666666297, 0.9204545454545454142, 0.9242424242424241987, 0.9280303030303029832, 0.9318181818181817677, 0.9356060606060605522, 0.9393939393939394478, 0.9431818181818182323, 0.9469696969696970168, 0.9507575757575758013, 0.9545454545454545858, 0.9583333333333333703, 0.9621212121212121549, 0.9659090909090909394 ),
 .UNSPECIFIED. ) 
 GEOMETRIC_REPRESENTATION_ITEM ( )  RATIONAL_B_SPLINE_SURFACE ( (
 ( 1.000000000000000000, 0.9659258262890683122, 1.000000000000000000, 0.9659258262890683122, 1.000000000000000000, 0.9659258262890683122, 1.000000000000000000, 0.9659258262890683122, 1.000000000000000000, 0.9659258262890683122, 1.000000000000000000, 0.9659258262890683122, 1.000000000000000000, 0.9659258262890683122, 1.000000000000000000, 0.9659258262890683122, 1.000000000000000000, 0.9659258262890683122, 1.000000000000000000, 0.9659258262890683122, 1.000000000000000000, 0.9659258262890683122, 1.000000000000000000, 0.9659258262890683122, 1.000000000000000000, 0.9659258262890683122, 1.000000000000000000, 0.9659258262890683122, 1.000000000000000000, 0.9659258262890683122, 1.000000000000000000, 0.9659258262890683122, 1.000000000000000000, 0.9659258262890683122, 1.000000000000000000, 0.9659258262890683122, 1.000000000000000000, 0.9659258262890683122, 1.000000000000000000, 0.9659258262890683122, 1.000000000000000000, 0.9659258262890683122, 1.000000000000000000, 0.9659258262890683122, 1.000000000000000000, 0.9659258262890683122, 1.000000000000000000, 0.9659258262890683122, 1.000000000000000000, 0.9659258262890683122, 1.000000000000000000, 0.9659258262890683122, 1.000000000000000000, 0.9659258262890683122, 1.000000000000000000, 0.9659258262890683122, 1.000000000000000000, 0.9659258262890683122, 1.000000000000000000, 0.9659258262890683122, 1.000000000000000000, 0.9659258262890683122, 1.000000000000000000, 0.9659258262890683122, 1.000000000000000000, 0.9659258262890683122, 1.000000000000000000, 0.9659258262890683122, 1.000000000000000000, 0.9659258262890683122, 1.000000000000000000, 0.9659258262890683122, 1.000000000000000000, 0.9659258262890683122, 1.000000000000000000, 0.9659258262890683122, 1.000000000000000000, 0.9659258262890683122, 1.000000000000000000, 0.9659258262890683122, 1.000000000000000000, 0.9659258262890683122, 1.000000000000000000, 0.9659258262890683122, 1.000000000000000000, 0.9659258262890683122, 1.000000000000000000, 0.9659258262890683122, 1.000000000000000000, 0.9659258262890683122, 1.000000000000000000, 0.9659258262890683122, 1.000000000000000000, 0.9659258262890683122, 1.000000000000000000, 0.9659258262890683122, 1.000000000000000000, 0.9659258262890683122, 1.000000000000000000, 0.9659258262890683122, 1.000000000000000000, 0.9659258262890683122, 1.000000000000000000, 0.9659258262890683122, 1.000000000000000000, 0.9659258262890683122, 1.000000000000000000, 0.9659258262890683122, 1.000000000000000000, 0.9659258262890683122, 1.000000000000000000, 0.9659258262890683122, 1.000000000000000000, 0.9659258262890683122, 1.000000000000000000, 0.9659258262890683122, 1.000000000000000000, 0.9659258262890683122, 1.000000000000000000, 0.9659258262890683122, 1.000000000000000000, 0.9659258262890683122, 1.000000000000000000, 0.9659258262890683122, 1.000000000000000000, 0.9659258262890683122, 1.000000000000000000, 0.9659258262890683122, 1.000000000000000000, 0.9659258262890683122, 1.000000000000000000, 0.9659258262890683122, 1.000000000000000000, 0.9659258262890683122, 1.000000000000000000, 0.9659258262890683122, 1.000000000000000000, 0.9659258262890683122, 1.000000000000000000, 0.9659258262890683122, 1.000000000000000000, 0.9659258262890683122, 1.000000000000000000, 0.9659258262890683122, 1.000000000000000000, 0.9659258262890683122, 1.000000000000000000, 0.9659258262890683122, 1.000000000000000000, 0.9659258262890683122, 1.000000000000000000, 0.9659258262890683122, 1.000000000000000000, 0.9659258262890683122, 1.000000000000000000, 0.9659258262890683122, 1.000000000000000000, 0.9659258262890683122, 1.000000000000000000, 0.9659258262890683122, 1.000000000000000000, 0.9659258262890683122, 1.000000000000000000, 0.9659258262890683122, 1.000000000000000000, 0.9659258262890683122, 1.000000000000000000, 0.9659258262890683122, 1.000000000000000000, 0.9659258262890683122, 1.000000000000000000, 0.9659258262890683122, 1.000000000000000000, 0.9659258262890683122, 1.000000000000000000, 0.9659258262890683122, 1.000000000000000000, 0.9659258262890683122, 1.000000000000000000, 0.9659258262890683122, 1.000000000000000000, 0.9659258262890683122, 1.000000000000000000, 0.9659258262890683122, 1.000000000000000000, 0.9659258262890683122, 1.000000000000000000, 0.9659258262890683122, 1.000000000000000000, 0.9659258262890683122, 1.000000000000000000, 0.9659258262890683122, 1.000000000000000000, 0.9659258262890683122, 1.000000000000000000, 0.9659258262890683122, 1.000000000000000000, 0.9659258262890683122, 1.000000000000000000, 0.9659258262890683122, 1.000000000000000000, 0.9659258262890683122, 1.000000000000000000, 0.9659258262890683122, 1.000000000000000000, 0.9659258262890683122, 1.000000000000000000, 0.9659258262890683122, 1.000000000000000000, 0.9659258262890683122, 1.000000000000000000, 0.9659258262890683122, 1.000000000000000000, 0.9659258262890683122, 1.000000000000000000, 0.9659258262890683122, 1.000000000000000000, 0.9659258262890683122, 1.000000000000000000, 0.9659258262890683122, 1.000000000000000000, 0.9659258262890683122, 1.000000000000000000, 0.9659258262890683122, 1.000000000000000000, 0.9659258262890683122, 1.000000000000000000, 0.9659258262890683122, 1.000000000000000000, 0.9659258262890683122, 1.000000000000000000, 0.9659258262890683122, 1.000000000000000000, 0.9659258262890683122, 1.000000000000000000, 0.9659258262890683122, 1.000000000000000000, 0.9659258262890683122, 1.000000000000000000, 0.9659258262890683122, 1.000000000000000000, 0.9659258262890683122, 1.000000000000000000, 0.9659258262890683122, 1.000000000000000000, 0.9659258262890683122, 1.000000000000000000, 0.9659258262890683122, 1.000000000000000000, 0.9659258262890683122, 1.000000000000000000, 0.9659258262890683122, 1.000000000000000000, 0.9659258262890683122, 1.000000000000000000, 0.9659258262890683122, 1.000000000000000000, 0.9659258262890683122, 1.000000000000000000, 0.9659258262890683122, 1.000000000000000000, 0.9659258262890683122, 1.000000000000000000, 0.9659258262890683122, 1.000000000000000000, 0.9659258262890683122, 1.000000000000000000, 0.9659258262890683122, 1.000000000000000000, 0.9659258262890683122, 1.000000000000000000, 0.9659258262890683122, 1.000000000000000000, 0.9659258262890683122, 1.000000000000000000, 0.9659258262890683122, 1.000000000000000000, 0.9659258262890683122, 1.000000000000000000, 0.9659258262890683122, 1.000000000000000000, 0.9659258262890683122, 1.000000000000000000, 0.9659258262890683122, 1.000000000000000000, 0.9659258262890683122, 1.000000000000000000, 0.9659258262890683122, 1.000000000000000000, 0.9659258262890683122, 1.000000000000000000, 0.9659258262890683122, 1.000000000000000000, 0.9659258262890683122, 1.000000000000000000, 0.9659258262890683122, 1.000000000000000000, 0.9659258262890683122, 1.000000000000000000, 0.9659258262890683122, 1.000000000000000000, 0.9659258262890683122, 1.000000000000000000, 0.9659258262890683122, 1.000000000000000000, 0.9659258262890683122, 1.000000000000000000, 0.9659258262890683122, 1.000000000000000000, 0.9659258262890683122, 1.000000000000000000, 0.9659258262890683122, 1.000000000000000000, 0.9659258262890683122, 1.000000000000000000, 0.9659258262890683122, 1.000000000000000000, 0.9659258262890683122, 1.000000000000000000, 0.9659258262890683122, 1.000000000000000000, 0.9659258262890683122, 1.000000000000000000, 0.9659258262890683122, 1.000000000000000000, 0.9659258262890683122, 1.000000000000000000, 0.9659258262890683122, 1.000000000000000000, 0.9659258262890683122, 1.000000000000000000, 0.9659258262890683122, 1.000000000000000000, 0.9659258262890683122, 1.000000000000000000, 0.9659258262890683122, 1.000000000000000000, 0.9659258262890683122, 1.000000000000000000, 0.9659258262890683122, 1.000000000000000000, 0.9659258262890683122, 1.000000000000000000, 0.9659258262890683122, 1.000000000000000000, 0.9659258262890683122, 1.000000000000000000, 0.9659258262890683122, 1.000000000000000000, 0.9659258262890683122, 1.000000000000000000, 0.9659258262890683122, 1.000000000000000000, 0.9659258262890683122, 1.000000000000000000, 0.9659258262890683122, 1.000000000000000000, 0.9659258262890683122, 1.000000000000000000, 0.9659258262890683122, 1.000000000000000000, 0.9659258262890683122, 1.000000000000000000, 0.9659258262890683122, 1.000000000000000000, 0.9659258262890683122, 1.000000000000000000, 0.9659258262890683122, 1.000000000000000000, 0.9659258262890683122, 1.000000000000000000, 0.9659258262890683122, 1.000000000000000000, 0.9659258262890683122, 1.000000000000000000, 0.9659258262890683122, 1.000000000000000000, 0.9659258262890683122, 1.000000000000000000, 0.9659258262890683122, 1.000000000000000000, 0.9659258262890683122, 1.000000000000000000, 0.9659258262890683122, 1.000000000000000000, 0.9659258262890683122, 1.000000000000000000, 0.9659258262890683122, 1.000000000000000000, 0.9659258262890683122, 1.000000000000000000, 0.9659258262890683122, 1.000000000000000000, 0.9659258262890683122, 1.000000000000000000, 0.9659258262890683122, 1.000000000000000000, 0.9659258262890683122, 1.000000000000000000, 0.9659258262890683122, 1.000000000000000000, 0.9659258262890683122, 1.000000000000000000, 0.9659258262890683122, 1.000000000000000000, 0.9659258262890683122, 1.000000000000000000, 0.9659258262890683122, 1.000000000000000000, 0.9659258262890683122, 1.000000000000000000, 0.9659258262890683122, 1.000000000000000000, 0.9659258262890683122, 1.000000000000000000, 0.9659258262890683122, 1.000000000000000000, 0.9659258262890683122, 1.000000000000000000, 0.9659258262890683122, 1.000000000000000000, 0.9659258262890683122, 1.000000000000000000, 0.9659258262890683122, 1.000000000000000000, 0.9659258262890683122, 1.000000000000000000, 0.9659258262890683122, 1.000000000000000000, 0.9659258262890683122, 1.000000000000000000, 0.9659258262890683122, 1.000000000000000000, 0.9659258262890683122, 1.000000000000000000, 0.9659258262890683122, 1.000000000000000000, 0.9659258262890683122, 1.000000000000000000, 0.9659258262890683122, 1.000000000000000000, 0.9659258262890683122, 1.000000000000000000, 0.9659258262890683122, 1.000000000000000000, 0.9659258262890683122, 1.000000000000000000, 0.9659258262890683122, 1.000000000000000000, 0.9659258262890683122, 1.000000000000000000, 0.9659258262890683122, 1.000000000000000000, 0.9659258262890683122, 1.000000000000000000, 0.9659258262890683122, 1.000000000000000000, 0.9659258262890683122, 1.000000000000000000, 0.9659258262890683122, 1.000000000000000000, 0.9659258262890683122, 1.000000000000000000, 0.9659258262890683122, 1.000000000000000000, 0.9659258262890683122, 1.000000000000000000, 0.9659258262890683122, 1.000000000000000000, 0.9659258262890683122, 1.000000000000000000, 0.9659258262890683122, 1.000000000000000000, 0.9659258262890683122, 1.000000000000000000, 0.9659258262890683122, 1.000000000000000000, 0.9659258262890683122, 1.000000000000000000, 0.9659258262890683122, 1.000000000000000000, 0.9659258262890683122, 1.000000000000000000, 0.9659258262890683122, 1.000000000000000000, 0.9659258262890683122, 1.000000000000000000, 0.9659258262890683122, 1.000000000000000000, 0.9659258262890683122, 1.000000000000000000, 0.9659258262890683122, 1.000000000000000000, 0.9659258262890683122, 1.000000000000000000, 0.9659258262890683122, 1.000000000000000000, 0.9659258262890683122, 1.000000000000000000, 0.9659258262890683122, 1.000000000000000000, 0.9659258262890683122, 1.000000000000000000, 0.9659258262890683122, 1.000000000000000000, 0.9659258262890683122, 1.000000000000000000, 0.9659258262890683122, 1.000000000000000000, 0.9659258262890683122, 1.000000000000000000),
 ( 1.000000000000000000, 0.9659258262890683122, 1.000000000000000000, 0.9659258262890683122, 1.000000000000000000, 0.9659258262890683122, 1.000000000000000000, 0.9659258262890683122, 1.000000000000000000, 0.9659258262890683122, 1.000000000000000000, 0.9659258262890683122, 1.000000000000000000, 0.9659258262890683122, 1.000000000000000000, 0.9659258262890683122, 1.000000000000000000, 0.9659258262890683122, 1.000000000000000000, 0.9659258262890683122, 1.000000000000000000, 0.9659258262890683122, 1.000000000000000000, 0.9659258262890683122, 1.000000000000000000, 0.9659258262890683122, 1.000000000000000000, 0.9659258262890683122, 1.000000000000000000, 0.9659258262890683122, 1.000000000000000000, 0.9659258262890683122, 1.000000000000000000, 0.9659258262890683122, 1.000000000000000000, 0.9659258262890683122, 1.000000000000000000, 0.9659258262890683122, 1.000000000000000000, 0.9659258262890683122, 1.000000000000000000, 0.9659258262890683122, 1.000000000000000000, 0.9659258262890683122, 1.000000000000000000, 0.9659258262890683122, 1.000000000000000000, 0.9659258262890683122, 1.000000000000000000, 0.9659258262890683122, 1.000000000000000000, 0.9659258262890683122, 1.000000000000000000, 0.9659258262890683122, 1.000000000000000000, 0.9659258262890683122, 1.000000000000000000, 0.9659258262890683122, 1.000000000000000000, 0.9659258262890683122, 1.000000000000000000, 0.9659258262890683122, 1.000000000000000000, 0.9659258262890683122, 1.000000000000000000, 0.9659258262890683122, 1.000000000000000000, 0.9659258262890683122, 1.000000000000000000, 0.9659258262890683122, 1.000000000000000000, 0.9659258262890683122, 1.000000000000000000, 0.9659258262890683122, 1.000000000000000000, 0.9659258262890683122, 1.000000000000000000, 0.9659258262890683122, 1.000000000000000000, 0.9659258262890683122, 1.000000000000000000, 0.9659258262890683122, 1.000000000000000000, 0.9659258262890683122, 1.000000000000000000, 0.9659258262890683122, 1.000000000000000000, 0.9659258262890683122, 1.000000000000000000, 0.9659258262890683122, 1.000000000000000000, 0.9659258262890683122, 1.000000000000000000, 0.9659258262890683122, 1.000000000000000000, 0.9659258262890683122, 1.000000000000000000, 0.9659258262890683122, 1.000000000000000000, 0.9659258262890683122, 1.000000000000000000, 0.9659258262890683122, 1.000000000000000000, 0.9659258262890683122, 1.000000000000000000, 0.9659258262890683122, 1.000000000000000000, 0.9659258262890683122, 1.000000000000000000, 0.9659258262890683122, 1.000000000000000000, 0.9659258262890683122, 1.000000000000000000, 0.9659258262890683122, 1.000000000000000000, 0.9659258262890683122, 1.000000000000000000, 0.9659258262890683122, 1.000000000000000000, 0.9659258262890683122, 1.000000000000000000, 0.9659258262890683122, 1.000000000000000000, 0.9659258262890683122, 1.000000000000000000, 0.9659258262890683122, 1.000000000000000000, 0.9659258262890683122, 1.000000000000000000, 0.9659258262890683122, 1.000000000000000000, 0.9659258262890683122, 1.000000000000000000, 0.9659258262890683122, 1.000000000000000000, 0.9659258262890683122, 1.000000000000000000, 0.9659258262890683122, 1.000000000000000000, 0.9659258262890683122, 1.000000000000000000, 0.9659258262890683122, 1.000000000000000000, 0.9659258262890683122, 1.000000000000000000, 0.9659258262890683122, 1.000000000000000000, 0.9659258262890683122, 1.000000000000000000, 0.9659258262890683122, 1.000000000000000000, 0.9659258262890683122, 1.000000000000000000, 0.9659258262890683122, 1.000000000000000000, 0.9659258262890683122, 1.000000000000000000, 0.9659258262890683122, 1.000000000000000000, 0.9659258262890683122, 1.000000000000000000, 0.9659258262890683122, 1.000000000000000000, 0.9659258262890683122, 1.000000000000000000, 0.9659258262890683122, 1.000000000000000000, 0.9659258262890683122, 1.000000000000000000, 0.9659258262890683122, 1.000000000000000000, 0.9659258262890683122, 1.000000000000000000, 0.9659258262890683122, 1.000000000000000000, 0.9659258262890683122, 1.000000000000000000, 0.9659258262890683122, 1.000000000000000000, 0.9659258262890683122, 1.000000000000000000, 0.9659258262890683122, 1.000000000000000000, 0.9659258262890683122, 1.000000000000000000, 0.9659258262890683122, 1.000000000000000000, 0.9659258262890683122, 1.000000000000000000, 0.9659258262890683122, 1.000000000000000000, 0.9659258262890683122, 1.000000000000000000, 0.9659258262890683122, 1.000000000000000000, 0.9659258262890683122, 1.000000000000000000, 0.9659258262890683122, 1.000000000000000000, 0.9659258262890683122, 1.000000000000000000, 0.9659258262890683122, 1.000000000000000000, 0.9659258262890683122, 1.000000000000000000, 0.9659258262890683122, 1.000000000000000000, 0.9659258262890683122, 1.000000000000000000, 0.9659258262890683122, 1.000000000000000000, 0.9659258262890683122, 1.000000000000000000, 0.9659258262890683122, 1.000000000000000000, 0.9659258262890683122, 1.000000000000000000, 0.9659258262890683122, 1.000000000000000000, 0.9659258262890683122, 1.000000000000000000, 0.9659258262890683122, 1.000000000000000000, 0.9659258262890683122, 1.000000000000000000, 0.9659258262890683122, 1.000000000000000000, 0.9659258262890683122, 1.000000000000000000, 0.9659258262890683122, 1.000000000000000000, 0.9659258262890683122, 1.000000000000000000, 0.9659258262890683122, 1.000000000000000000, 0.9659258262890683122, 1.000000000000000000, 0.9659258262890683122, 1.000000000000000000, 0.9659258262890683122, 1.000000000000000000, 0.9659258262890683122, 1.000000000000000000, 0.9659258262890683122, 1.000000000000000000, 0.9659258262890683122, 1.000000000000000000, 0.9659258262890683122, 1.000000000000000000, 0.9659258262890683122, 1.000000000000000000, 0.9659258262890683122, 1.000000000000000000, 0.9659258262890683122, 1.000000000000000000, 0.9659258262890683122, 1.000000000000000000, 0.9659258262890683122, 1.000000000000000000, 0.9659258262890683122, 1.000000000000000000, 0.9659258262890683122, 1.000000000000000000, 0.9659258262890683122, 1.000000000000000000, 0.9659258262890683122, 1.000000000000000000, 0.9659258262890683122, 1.000000000000000000, 0.9659258262890683122, 1.000000000000000000, 0.9659258262890683122, 1.000000000000000000, 0.9659258262890683122, 1.000000000000000000, 0.9659258262890683122, 1.000000000000000000, 0.9659258262890683122, 1.000000000000000000, 0.9659258262890683122, 1.000000000000000000, 0.9659258262890683122, 1.000000000000000000, 0.9659258262890683122, 1.000000000000000000, 0.9659258262890683122, 1.000000000000000000, 0.9659258262890683122, 1.000000000000000000, 0.9659258262890683122, 1.000000000000000000, 0.9659258262890683122, 1.000000000000000000, 0.9659258262890683122, 1.000000000000000000, 0.9659258262890683122, 1.000000000000000000, 0.9659258262890683122, 1.000000000000000000, 0.9659258262890683122, 1.000000000000000000, 0.9659258262890683122, 1.000000000000000000, 0.9659258262890683122, 1.000000000000000000, 0.9659258262890683122, 1.000000000000000000, 0.9659258262890683122, 1.000000000000000000, 0.9659258262890683122, 1.000000000000000000, 0.9659258262890683122, 1.000000000000000000, 0.9659258262890683122, 1.000000000000000000, 0.9659258262890683122, 1.000000000000000000, 0.9659258262890683122, 1.000000000000000000, 0.9659258262890683122, 1.000000000000000000, 0.9659258262890683122, 1.000000000000000000, 0.9659258262890683122, 1.000000000000000000, 0.9659258262890683122, 1.000000000000000000, 0.9659258262890683122, 1.000000000000000000, 0.9659258262890683122, 1.000000000000000000, 0.9659258262890683122, 1.000000000000000000, 0.9659258262890683122, 1.000000000000000000, 0.9659258262890683122, 1.000000000000000000, 0.9659258262890683122, 1.000000000000000000, 0.9659258262890683122, 1.000000000000000000, 0.9659258262890683122, 1.000000000000000000, 0.9659258262890683122, 1.000000000000000000, 0.9659258262890683122, 1.000000000000000000, 0.9659258262890683122, 1.000000000000000000, 0.9659258262890683122, 1.000000000000000000, 0.9659258262890683122, 1.000000000000000000, 0.9659258262890683122, 1.000000000000000000, 0.9659258262890683122, 1.000000000000000000, 0.9659258262890683122, 1.000000000000000000, 0.9659258262890683122, 1.000000000000000000, 0.9659258262890683122, 1.000000000000000000, 0.9659258262890683122, 1.000000000000000000, 0.9659258262890683122, 1.000000000000000000, 0.9659258262890683122, 1.000000000000000000, 0.9659258262890683122, 1.000000000000000000, 0.9659258262890683122, 1.000000000000000000, 0.9659258262890683122, 1.000000000000000000, 0.9659258262890683122, 1.000000000000000000, 0.9659258262890683122, 1.000000000000000000, 0.9659258262890683122, 1.000000000000000000, 0.9659258262890683122, 1.000000000000000000, 0.9659258262890683122, 1.000000000000000000, 0.9659258262890683122, 1.000000000000000000, 0.9659258262890683122, 1.000000000000000000, 0.9659258262890683122, 1.000000000000000000, 0.9659258262890683122, 1.000000000000000000, 0.9659258262890683122, 1.000000000000000000, 0.9659258262890683122, 1.000000000000000000, 0.9659258262890683122, 1.000000000000000000, 0.9659258262890683122, 1.000000000000000000, 0.9659258262890683122, 1.000000000000000000, 0.9659258262890683122, 1.000000000000000000, 0.9659258262890683122, 1.000000000000000000, 0.9659258262890683122, 1.000000000000000000, 0.9659258262890683122, 1.000000000000000000, 0.9659258262890683122, 1.000000000000000000, 0.9659258262890683122, 1.000000000000000000, 0.9659258262890683122, 1.000000000000000000, 0.9659258262890683122, 1.000000000000000000, 0.9659258262890683122, 1.000000000000000000, 0.9659258262890683122, 1.000000000000000000, 0.9659258262890683122, 1.000000000000000000, 0.9659258262890683122, 1.000000000000000000, 0.9659258262890683122, 1.000000000000000000, 0.9659258262890683122, 1.000000000000000000, 0.9659258262890683122, 1.000000000000000000, 0.9659258262890683122, 1.000000000000000000, 0.9659258262890683122, 1.000000000000000000, 0.9659258262890683122, 1.000000000000000000, 0.9659258262890683122, 1.000000000000000000, 0.9659258262890683122, 1.000000000000000000, 0.9659258262890683122, 1.000000000000000000, 0.9659258262890683122, 1.000000000000000000, 0.9659258262890683122, 1.000000000000000000, 0.9659258262890683122, 1.000000000000000000, 0.9659258262890683122, 1.000000000000000000, 0.9659258262890683122, 1.000000000000000000, 0.9659258262890683122, 1.000000000000000000, 0.9659258262890683122, 1.000000000000000000, 0.9659258262890683122, 1.000000000000000000, 0.9659258262890683122, 1.000000000000000000, 0.9659258262890683122, 1.000000000000000000, 0.9659258262890683122, 1.000000000000000000, 0.9659258262890683122, 1.000000000000000000, 0.9659258262890683122, 1.000000000000000000, 0.9659258262890683122, 1.000000000000000000, 0.9659258262890683122, 1.000000000000000000, 0.9659258262890683122, 1.000000000000000000, 0.9659258262890683122, 1.000000000000000000, 0.9659258262890683122, 1.000000000000000000, 0.9659258262890683122, 1.000000000000000000, 0.9659258262890683122, 1.000000000000000000, 0.9659258262890683122, 1.000000000000000000, 0.9659258262890683122, 1.000000000000000000, 0.9659258262890683122, 1.000000000000000000, 0.9659258262890683122, 1.000000000000000000, 0.9659258262890683122, 1.000000000000000000, 0.9659258262890683122, 1.000000000000000000, 0.9659258262890683122, 1.000000000000000000, 0.9659258262890683122, 1.000000000000000000, 0.9659258262890683122, 1.000000000000000000, 0.9659258262890683122, 1.000000000000000000, 0.9659258262890683122, 1.000000000000000000, 0.9659258262890683122, 1.000000000000000000, 0.9659258262890683122, 1.000000000000000000) ) ) 
 REPRESENTATION_ITEM ( '' )  SURFACE ( )  );
#2594 = CARTESIAN_POINT ( 'NONE',  ( -0.1312335958005241554, 0.2306618581243848609, 0.2411417322834645549 ) ) ;
#2595 = CARTESIAN_POINT ( 'NONE',  ( -0.3805774278215216522, 0.05413385826771666132, 0.4176697321401328100 ) ) ;
#2596 = CARTESIAN_POINT ( 'NONE',  ( -0.3392501089628017219, -0.1958661417322836718, -2.026902887139107712 ) ) ;
#2597 = CARTESIAN_POINT ( 'NONE',  ( -1.725721784776902190, -0.05778040916215522460, 0.4822834645669289988 ) ) ;
#2598 = CARTESIAN_POINT ( 'NONE',  ( -0.4593175853018364174, -0.4281496062992127816, -0.4176697321401328100 ) ) ;
#2599 = CARTESIAN_POINT ( 'NONE',  ( -0.3412073490813641308, 0.1283753931104746893, -0.1820866141732285504 ) ) ;
#2600 = CARTESIAN_POINT ( 'NONE',  ( 1.286089238845145033, -0.6046776061558809534, -0.2411417322834644161 ) ) ;
#2601 = LINE ( 'NONE', #79218, #82724 ) ;
#2602 = CARTESIAN_POINT ( 'NONE',  ( -0.8202099737532801971, -0.6692913385826771977, 0.1292274648535927661 ) ) ;
#2603 = CARTESIAN_POINT ( 'NONE',  ( 4.893765752498283308E-17, -0.3996062992125985480, 0.1594488188976377896 ) ) ;
#2604 = CARTESIAN_POINT ( 'NONE',  ( 0.8923884514435701520, -0.6046776061558809534, -0.2411417322834644161 ) ) ;
#2605 = CARTESIAN_POINT ( 'NONE',  ( -0.1070741851644056997, 0.3996062992125986035, -2.053805774278214979 ) ) ;
#2606 = CARTESIAN_POINT ( 'NONE',  ( 3.936638708481129623, 1.066027760652975553, 0.06186723695104996007 ) ) ;
#2607 = EDGE_CURVE ( 'NONE', #26484, #9025, #73534, .T. ) ;
#2608 = CARTESIAN_POINT ( 'NONE',  ( 0.01968503937007957949, -0.5400638737290845981, -0.3530559997133363437 ) ) ;
#2609 = CARTESIAN_POINT ( 'NONE',  ( -1.187664041994749731, -0.2845877964562159024, 0.3641732283464567677 ) ) ;
#2611 = LINE ( 'NONE', #53519, #82778 ) ;
#2610 = CARTESIAN_POINT ( 'NONE',  ( 1.213910761154856299, 0.1771653543307087630, 0.09757992244046791164 ) ) ;
#2612 = CARTESIAN_POINT ( 'NONE',  ( 0.4724409448818898682, 2.892866454678787531E-17, -0.5098425196850393526 ) ) ;
#2613 = CARTESIAN_POINT ( 'NONE',  ( 1.227034120734908917, 0.1771653543307087075, -0.09757992244046823083 ) ) ;
#2614 = VECTOR ( 'NONE', #59202, 39.37007874015748143 ) ;
#2615 = CARTESIAN_POINT ( 'NONE',  ( 1.371391076115485719, -0.6692913385826773087, -0.1292274648535924053 ) ) ;
#2616 = CARTESIAN_POINT ( 'NONE',  ( -0.2891555358219911054, 0.2891555358219909388, -0.5688976377952756902 ) ) ;
#2617 = CARTESIAN_POINT ( 'NONE',  ( -0.3083989501312330295, -0.05778040916215522460, 0.4822834645669289988 ) ) ;
#2618 = PLANE ( 'NONE',  #39133 ) ;
#2619 = CARTESIAN_POINT ( 'NONE',  ( 1.351706036745407458, -0.3690944881889765550, -0.3153832671262227771 ) ) ;
#2620 = CARTESIAN_POINT ( 'NONE',  ( -0.1902887139107604098, -0.6692913385826771977, 0.1292274648535927661 ) ) ;
#2621 = CARTESIAN_POINT ( 'NONE',  ( -0.1974969037888704149, -0.3420746716998661063, -0.4573490813648294906 ) ) ;
#2622 = CARTESIAN_POINT ( 'NONE',  ( 1.141732283464567788, -0.6692913385826771977, 8.415575281601705876E-17 ) ) ;
#2623 = CARTESIAN_POINT ( 'NONE',  ( 0.2952755905511816326, -0.5400638737290844871, 0.3530559997133364547 ) ) ;
#2624 = CARTESIAN_POINT ( 'NONE',  ( 0.6758530183727039509, -0.5511811023622046335, 0.09757992244046803654 ) ) ;
#2625 = DIRECTION ( 'NONE',  ( 0.000000000000000000, 1.000000000000000000, 0.000000000000000000 ) ) ;
#2626 = CARTESIAN_POINT ( 'NONE',  ( 0.4790026246719168435, -0.2845877964562161244, -0.3641732283464567121 ) ) ;
#2627 = PLANE ( 'NONE',  #12150 ) ;
#2628 = CARTESIAN_POINT ( 'NONE',  ( -0.3996062992125985480, -7.340648628747423112E-17, -1.533464566929134021 ) ) ;
#2629 = CARTESIAN_POINT ( 'NONE',  ( 0.9383202099737538715, -0.05778040916215560624, -0.4822834645669293319 ) ) ;
#2630 = CARTESIAN_POINT ( 'NONE',  ( -0.1049643490035307020, 0.3917322834645669549, -0.9435695538057740084 ) ) ;
#2631 = CARTESIAN_POINT ( 'NONE',  ( 0.1265901696524990572, -0.4724409448818897017, -0.4770341207349080848 ) ) ;
#2632 = CARTESIAN_POINT ( 'NONE',  ( 0.1181102362204730916, 0.2952755905511811885, 0.000000000000000000 ) ) ;
#2633 = CARTESIAN_POINT ( 'NONE',  ( -0.1443569553805768291, -0.004921259842519576551, 0.3153832671262227771 ) ) ;
#2634 = CARTESIAN_POINT ( 'NONE',  ( 0.1706036745406830368, -0.4281496062992127816, -0.4176697321401328100 ) ) ;
#2635 = CARTESIAN_POINT ( 'NONE',  ( 1.227034120734908917, 0.1771653543307087075, -0.09757992244046823083 ) ) ;
#2636 = CARTESIAN_POINT ( 'NONE',  ( -1.509186351706035767, -0.004921259842519870586, -0.3153832671262229437 ) ) ;
#2637 = CARTESIAN_POINT ( 'NONE',  ( -1.345144356955379816, -0.05778040916215560624, -0.4822834645669293319 ) ) ;
#2638 = CARTESIAN_POINT ( 'NONE',  ( 0.6430446194225729606, -0.4281496062992127816, -0.4176697321401328100 ) ) ;
#2639 = CARTESIAN_POINT ( 'NONE',  ( 1.417322834645670104, -0.1870078740157480879, -0.4822834645669291653 ) ) ;
#2640 = CARTESIAN_POINT ( 'NONE',  ( -0.3458507752293909498, 0.3458507752293908388, -0.2539370078740156855 ) ) ;
#2641 = CARTESIAN_POINT ( 'NONE',  ( 0.4002624671916016896, -0.3162353388693409650, -0.4822834645669289433 ) ) ;
#2642 = CARTESIAN_POINT ( 'NONE',  ( -0.1070741851644051862, -0.3996062992125986590, 0.1660104986876640154 ) ) ;
#2643 = CARTESIAN_POINT ( 'NONE',  ( 1.528871391076116026, 0.2952755905511811885, 0.1292274648535926551 ) ) ;
#2644 = CARTESIAN_POINT ( 'NONE',  ( 1.141732283464567788, -0.6692913385826771977, 8.415575281601705876E-17 ) ) ;
#2645 = CARTESIAN_POINT ( 'NONE',  ( -1.594488188976377563, -0.4536011799217367080, 0.2665933059059888421 ) ) ;
#2646 = CARTESIAN_POINT ( 'NONE',  ( 1.220472440944882608, 0.1771653543307087630, 0.000000000000000000 ) ) ;
#2647 = CARTESIAN_POINT ( 'NONE',  ( -1.594488188976377119, 0.07958543189024071263, -0.2665933059059888421 ) ) ;
#2648 = CARTESIAN_POINT ( 'NONE',  ( -0.8202099737532799750, 0.1771653543307087075, -0.09757992244046823083 ) ) ;
#2649 = CARTESIAN_POINT ( 'NONE',  ( 1.574803149606299746, -0.1870078740157479769, 0.4822834645669291653 ) ) ;
#2650 = CARTESIAN_POINT ( 'NONE',  ( 0.4199475065616803948, -0.5023911411419708095, -0.1820866141732282451 ) ) ;
#2651 = CARTESIAN_POINT ( 'NONE',  ( 0.1574803149606306130, -0.1870078740157480879, -0.4822834645669291653 ) ) ;
#2652 = CARTESIAN_POINT ( 'NONE',  ( 0.8595800524934390507, -0.05778040916215560624, -0.4822834645669293319 ) ) ;
#2653 = CARTESIAN_POINT ( 'NONE',  ( -0.3674540682414689785, 0.2306618581243848609, 0.2411417322834645549 ) ) ;
#2654 = CARTESIAN_POINT ( 'NONE',  ( 0.3149606299212603933, -0.1870078740157479769, 0.3641732283464567677 ) ) ;
#2655 = CARTESIAN_POINT ( 'NONE',  ( 1.023622047244095112, -0.1870078740157480879, -0.4822834645669291653 ) ) ;
#2656 = DIRECTION ( 'NONE',  ( 1.000000000000000000, 3.096699300667737957E-16, 0.000000000000000000 ) ) ;
#2657 = CARTESIAN_POINT ( 'NONE',  ( -0.8333333333333323711, -0.6692913385826773087, -0.1292274648535924053 ) ) ;
#2659 = CARTESIAN_POINT ( 'NONE',  ( 0.3996062992125986035, -0.1070741851644053111, -0.8989501312335956840 ) ) ;
#2658 = CARTESIAN_POINT ( 'NONE',  ( -1.568241469816272105, -0.08942795157527998196, 0.3641732283464567121 ) ) ;
#2660 = CARTESIAN_POINT ( 'NONE',  ( 2.138346301250393822, 1.653225543546886112, -0.4603267246303516802 ) ) ;
#2661 = CARTESIAN_POINT ( 'NONE',  ( -0.8070866141732276899, 0.1660481256975883668, -0.3530559997133364547 ) ) ;
#2662 = CARTESIAN_POINT ( 'NONE',  ( -0.2099737532808391705, -0.6046776061558809534, -0.2411417322834644161 ) ) ;
#2663 = CARTESIAN_POINT ( 'NONE',  ( -0.2362204724409451284, 0.4091458600556402425, 0.1443569553805774397 ) ) ;
#2664 = CARTESIAN_POINT ( 'NONE',  ( 0.1058382717557499880, 0.3949938075777411073, -2.355643044619422533 ) ) ;
#2665 = ORIENTED_EDGE ( 'NONE', *, *, #46607, .T. ) ;
#2666 = CARTESIAN_POINT ( 'NONE',  ( 0.8530183727034128527, -0.3690944881889763329, 0.3153832671262228327 ) ) ;
#2667 = CARTESIAN_POINT ( 'NONE',  ( 0.1958661417322834775, 0.3392501089628018884, -0.9238845144356954142 ) ) ;
#2668 = CARTESIAN_POINT ( 'NONE',  ( 1.167979002624672580, 0.05413385826771626580, -0.4176697321401330321 ) ) ;
#2669 = CARTESIAN_POINT ( 'NONE',  ( -0.2486400153428821869, 2.660739321503277841E-15, -0.3464511005275191513 ) ) ;
#2670 = CARTESIAN_POINT ( 'NONE',  ( -1.515748031496062076, 0.07958543189024071263, -0.2665933059059888421 ) ) ;
#2671 = CARTESIAN_POINT ( 'NONE',  ( 1.528871391076116026, 0.2952755905511811885, 0.1292274648535926551 ) ) ;
#2672 = CARTESIAN_POINT ( 'NONE',  ( -1.377952755905511140, 0.2952755905511811885, 0.000000000000000000 ) ) ;
#2673 = CARTESIAN_POINT ( 'NONE',  ( 0.3392501089628018329, -0.1958661417322834497, -0.4999806842181608868 ) ) ;
#2674 = CARTESIAN_POINT ( 'NONE',  ( 0.03280839895013198948, -0.6692913385826773087, -0.1292274648535924053 ) ) ;
#2675 = CARTESIAN_POINT ( 'NONE',  ( -0.3871391076115479057, -0.2845877964562161244, -0.3641732283464567121 ) ) ;
#2676 = CARTESIAN_POINT ( 'NONE',  ( 1.062992125984252745, -0.6692913385826771977, 8.415575281601705876E-17 ) ) ;
#2677 = CARTESIAN_POINT ( 'NONE',  ( -0.1049868766404193215, 0.2306618581243847221, -0.2411417322834647770 ) ) ;
#2678 = CARTESIAN_POINT ( 'NONE',  ( -0.4732023222440167043, 1.572318554836807936, -2.167187561710682608 ) ) ;
#2679 = CARTESIAN_POINT ( 'NONE',  ( 0.2925321140481932369, 0.2925321140481932369, -2.814960629921259727 ) ) ;
#2680 = CARTESIAN_POINT ( 'NONE',  ( 0.3392501089628018884, -0.1958661417322833942, -1.519048187172915343 ) ) ;
#2681 = CARTESIAN_POINT ( 'NONE',  ( 1.003937007874016407, -0.5400638737290844871, 0.3530559997133364547 ) ) ;
#2682 = CARTESIAN_POINT ( 'NONE',  ( 0.2690288713910767848, -0.6692913385826773087, -0.1292274648535924053 ) ) ;
#2683 = CARTESIAN_POINT ( 'NONE',  ( -1.240157480314959759, -0.5400638737290845981, -0.3530559997133363437 ) ) ;
#2684 = CARTESIAN_POINT ( 'NONE',  ( 1.456692913385827515, 0.2952755905511811885, 0.000000000000000000 ) ) ;
#2685 = CARTESIAN_POINT ( 'NONE',  ( 0.7086614173228353852, -0.1870078740157479769, 0.4822834645669291653 ) ) ;
#2686 = CARTESIAN_POINT ( 'NONE',  ( 0.1958661417322834775, 0.3392501089628018884, -0.8589238845144357981 ) ) ;
#2687 = CARTESIAN_POINT ( 'NONE',  ( -0.4002624671916004129, -0.05778040916215560624, -0.4822834645669293319 ) ) ;
#2688 = CARTESIAN_POINT ( 'NONE',  ( 0.6889763779527566800, -0.5400638737290844871, 0.3530559997133364547 ) ) ;
#2689 = CARTESIAN_POINT ( 'NONE',  ( -0.09842519685039295696, -0.5400638737290844871, 0.3530559997133364547 ) ) ;
#2690 = CARTESIAN_POINT ( 'NONE',  ( 0.8595800524934390507, -0.2845877964562159024, 0.3641732283464567677 ) ) ;
#2691 = CARTESIAN_POINT ( 'NONE',  ( -1.141732283464566011, -0.6692913385826771977, 8.415575281601705876E-17 ) ) ;
#2692 = CARTESIAN_POINT ( 'NONE',  ( -1.706036745406823485, 0.2306618581243848609, 0.2411417322834645549 ) ) ;
#2693 = CARTESIAN_POINT ( 'NONE',  ( 0.5839895013123367340, -0.6692913385826773087, -0.1292274648535924053 ) ) ;
#2694 = DIRECTION ( 'NONE',  ( 1.000000000000000000, -0.000000000000000000, -0.000000000000000000 ) ) ;
#2695 = CARTESIAN_POINT ( 'NONE',  ( 0.3392501089628018884, -0.1958661417322834220, -2.459317585301837195 ) ) ;
#2696 = EDGE_LOOP ( 'NONE', ( #66226, #52117, #33223, #17176, #68911, #34788, #10944, #71203, #15875, #69962, #67305, #18404, #77329, #39611 ) ) ;
#2697 = ORIENTED_EDGE ( 'NONE', *, *, #5292, .T. ) ;
#2698 = CARTESIAN_POINT ( 'NONE',  ( 1.259842519685040019, -0.1870078740157480879, -0.4822834645669291653 ) ) ;
#2699 = CARTESIAN_POINT ( 'NONE',  ( 0.4002624671916016896, -0.2845877964562161244, -0.3641732283464567121 ) ) ;
#2700 = CARTESIAN_POINT ( 'NONE',  ( 0.5774278215223104249, 0.2306618581243848609, 0.2411417322834645549 ) ) ;
#2701 = DIRECTION ( 'NONE',  ( -0.000000000000000000, -1.000000000000000000, -0.000000000000000000 ) ) ;
#2702 = FACE_OUTER_BOUND ( 'NONE', #52644, .T. ) ;
#2703 = CARTESIAN_POINT ( 'NONE',  ( 0.3917322834645670104, 2.398668435337828261E-17, -1.305118110236220375 ) ) ;
#2704 = CARTESIAN_POINT ( 'NONE',  ( 0.3996062992125984925, 0.1070741851644054637, -2.091207349081364519 ) ) ;
#2705 = CARTESIAN_POINT ( 'NONE',  ( -0.9645669291338575535, 0.1660481256975883668, -0.3530559997133364547 ) ) ;
#2706 = CARTESIAN_POINT ( 'NONE',  ( -0.6955380577427815458, -0.4281496062992127816, -0.4176697321401328100 ) ) ;
#2707 = CARTESIAN_POINT ( 'NONE',  ( 1.299212598425197429, 0.2952755905511811885, 0.000000000000000000 ) ) ;
#2708 = ORIENTED_EDGE ( 'NONE', *, *, #73731, .T. ) ;
#2709 = CARTESIAN_POINT ( 'NONE',  ( -1.509186351706035767, 0.05413385826771626580, -0.4176697321401330321 ) ) ;
#2710 = CARTESIAN_POINT ( 'NONE',  ( -1.170403185795210632, -4.983732387537991731E-15, 0.4118484887281982920 ) ) ;
#2711 = CARTESIAN_POINT ( 'NONE',  ( 1.587926509186352586, -0.3690944881889765550, -0.3153832671262227771 ) ) ;
#2712 = CARTESIAN_POINT ( 'NONE',  ( 0.3460692066303958092, 0.1998031496062993018, -2.097769028871391050 ) ) ;
#2713 = CARTESIAN_POINT ( 'NONE',  ( -1.259842519685038686, -0.1870078740157480601, -0.3641732283464567677 ) ) ;
#2714 =( BOUNDED_CURVE ( )  B_SPLINE_CURVE ( 2, ( #22978, #74756, #69258, #10368, #55778, #80666, #29705, #49475, #23389, #68435, #62521, #17513, #56198 ),
 .UNSPECIFIED., .F., .F. ) 
 B_SPLINE_CURVE_WITH_KNOTS ( ( 3, 2, 2, 2, 2, 2, 3 ),
 ( 0.4581241751160508580, 0.4583333333333333703, 0.4621212121212121549, 0.4659090909090909394, 0.4696969696969697239, 0.4734848484848485084, 0.4736940067021309653 ),
 .UNSPECIFIED. ) 
 CURVE ( )  GEOMETRIC_REPRESENTATION_ITEM ( )  RATIONAL_B_SPLINE_CURVE ( ( 0.9964447847208419695, 0.9981185001348091834, 1.000000000000000000, 0.9659258262890683122, 1.000000000000000000, 0.9659258262890683122, 1.000000000000000000, 0.9659258262890683122, 1.000000000000000000, 0.9659258262890683122, 1.000000000000000000, 0.9981185001348097385, 0.9964447847208430797 ) ) 
 REPRESENTATION_ITEM ( '' )  );
#2715 = CARTESIAN_POINT ( 'NONE',  ( 0.3392501089628018329, 0.1958661417322835607, 0.03412073490813653104 ) ) ;
#2716 = CARTESIAN_POINT ( 'NONE',  ( 0.2821522309711292364, 0.2952755905511810774, -0.1292274648535930714 ) ) ;
#2718 = DIRECTION ( 'NONE',  ( -0.000000000000000000, -1.000000000000000000, -0.000000000000000000 ) ) ;
#2717 = CARTESIAN_POINT ( 'NONE',  ( 1.482939632545932307, -0.4281496062992124485, 0.4176697321401328655 ) ) ;
#2719 = CARTESIAN_POINT ( 'NONE',  ( -0.9317585301837263412, -0.004921259842519576551, 0.3153832671262227771 ) ) ;
#2720 = CARTESIAN_POINT ( 'NONE',  ( 0.7677165354330716118, 0.1660481256975883668, -0.3530559997133364547 ) ) ;
#2721 = CARTESIAN_POINT ( 'NONE',  ( 1.463254593175853824, 0.1771653543307087075, -0.09757992244046823083 ) ) ;
#2722 = CARTESIAN_POINT ( 'NONE',  ( -0.3917322834645670659, 0.1049643490035301607, -1.215203781331021915 ) ) ;
#2723 = CARTESIAN_POINT ( 'NONE',  ( -0.8530183727034112984, -0.3690944881889765550, -0.3153832671262227771 ) ) ;
#2724 = CARTESIAN_POINT ( 'NONE',  ( 1.187664041994751285, -0.05778040916215522460, 0.4822834645669289988 ) ) ;
#2725 = CARTESIAN_POINT ( 'NONE',  ( 3.833048050305355326E-17, 1.954428616053095924, 0.3129921259842520787 ) ) ;
#2726 = CARTESIAN_POINT ( 'NONE',  ( 0.3412073490813655186, 0.2306618581243848609, 0.2411417322834645549 ) ) ;
#2727 = CARTESIAN_POINT ( 'NONE',  ( -0.7808398950131222316, -0.2845877964562161244, -0.3641732283464567121 ) ) ;
#2728 = CARTESIAN_POINT ( 'NONE',  ( -0.4593175853018366950, -0.004921259842519576551, 0.3153832671262227771 ) ) ;
#2729 = EDGE_CURVE ( 'NONE', #71941, #63010, #550, .T. ) ;
#2730 = CARTESIAN_POINT ( 'NONE',  ( -0.2296587926509179312, -0.3162353388693409650, -0.4822834645669289433 ) ) ;
#2731 = CARTESIAN_POINT ( 'NONE',  ( 1.686351706036745890, 0.2952755905511811885, 0.1292274648535926551 ) ) ;
#2732 = CARTESIAN_POINT ( 'NONE',  ( 0.3392501089628018329, 0.1958661417322835607, -0.2854523866479808936 ) ) ;
#2733 = CARTESIAN_POINT ( 'NONE',  ( 0.5249343832021003964, 0.2306618581243847221, -0.2411417322834647770 ) ) ;
#2734 = EDGE_CURVE ( 'NONE', #9013, #10037, #67629, .T. ) ;
#2735 = ADVANCED_FACE ( 'NONE', ( #14444 ), #65368, .F. ) ;
#2736 = DIRECTION ( 'NONE',  ( -3.096699300667737957E-16, 1.000000000000000000, -0.000000000000000000 ) ) ;
#2737 = CARTESIAN_POINT ( 'NONE',  ( 0.2362204724409451007, -0.4091458600556402980, -1.743438320209973469 ) ) ;
#2738 = CARTESIAN_POINT ( 'NONE',  ( -0.9908136482939626788, -0.6692913385826773087, -0.1292274648535924053 ) ) ;
#2739 = CARTESIAN_POINT ( 'NONE',  ( -0.3937007874015740483, -0.1870078740157480601, -0.3641732283464567677 ) ) ;
#2740 = CARTESIAN_POINT ( 'NONE',  ( -1.233595800524933894, -0.6046776061558809534, -0.2411417322834644161 ) ) ;
#2741 = CARTESIAN_POINT ( 'NONE',  ( 0.2296587926509192634, -0.3162353388693405765, 0.4822834645669290543 ) ) ;
#2742 = CARTESIAN_POINT ( 'NONE',  ( 0.3149606299212606708, -0.1870078740157480601, -0.3641732283464567677 ) ) ;
#2743 = CARTESIAN_POINT ( 'NONE',  ( -0.6167979002624665030, -0.004921259842519576551, 0.3153832671262227771 ) ) ;
#2744 = CARTESIAN_POINT ( 'NONE',  ( -1.141732283464566011, -0.6692913385826771977, 8.415575281601705876E-17 ) ) ;
#2745 = CARTESIAN_POINT ( 'NONE',  ( 1.614173228346457378, 0.1771653543307087630, 0.000000000000000000 ) ) ;
#2746 = CARTESIAN_POINT ( 'NONE',  ( 1.200787401574803681, 0.1660481256975885056, 0.3530559997133364547 ) ) ;
#2747 = DIRECTION ( 'NONE',  ( -0.000000000000000000, -1.000000000000000000, -0.000000000000000000 ) ) ;
#2748 = CARTESIAN_POINT ( 'NONE',  ( 0.7808398950131241190, -0.08942795157528024563, -0.3641732283464568787 ) ) ;
#2749 = CARTESIAN_POINT ( 'NONE',  ( 0.5511811023622055217, -0.1870078740157479769, 0.4822834645669291653 ) ) ;
#2750 = CARTESIAN_POINT ( 'NONE',  ( -1.854472803289052507, 2.716535433070866645, 0.5314960629921260393 ) ) ;
#2751 = CARTESIAN_POINT ( 'NONE',  ( 1.496062992125984703, -0.1870078740157480601, -0.3641732283464567677 ) ) ;
#2752 = ORIENTED_EDGE ( 'NONE', *, *, #26244, .T. ) ;
#2753 = CARTESIAN_POINT ( 'NONE',  ( -0.1998031496062991630, -0.3460692066303959202, -2.662073490813648746 ) ) ;
#2754 = EDGE_CURVE ( 'NONE', #50981, #74234, #27338, .T. ) ;
#2755 = CARTESIAN_POINT ( 'NONE',  ( -1.128608923884513837, 0.1283753931104746893, -0.1820866141732285504 ) ) ;
#2756 = CARTESIAN_POINT ( 'NONE',  ( -0.4921259842519677963, 0.1660481256975883668, -0.3530559997133364547 ) ) ;
#2757 = CARTESIAN_POINT ( 'NONE',  ( 0.2296587926509192634, -0.05778040916215560624, -0.4822834645669293319 ) ) ;
#2758 = CARTESIAN_POINT ( 'NONE',  ( -1.679790026246718693, 0.1283753931104746893, -0.1820866141732285504 ) ) ;
#2759 = CARTESIAN_POINT ( 'NONE',  ( -0.1070741851644051862, -0.3996062992125986590, -2.196194225721784576 ) ) ;
#2760 = CARTESIAN_POINT ( 'NONE',  ( -1.318897637795274802, -0.5400638737290845981, -0.3530559997133363437 ) ) ;
#2761 = CARTESIAN_POINT ( 'NONE',  ( 0.5774278215223104249, 0.2306618581243848609, 0.2411417322834645549 ) ) ;
#2762 = CARTESIAN_POINT ( 'NONE',  ( -0.1115485564304453947, -0.6692913385826771977, 0.1292274648535927661 ) ) ;
#2763 = CARTESIAN_POINT ( 'NONE',  ( 1.266404199475066328, -0.05778040916215522460, 0.4822834645669289988 ) ) ;
#2764 = CARTESIAN_POINT ( 'NONE',  ( 1.627296587926509996, -0.6046776061558807314, 0.2411417322834647770 ) ) ;
#2765 = CARTESIAN_POINT ( 'NONE',  ( 0.1070741851644054915, -0.3996062992125986035, -1.975065616797900381 ) ) ;
#2766 = CARTESIAN_POINT ( 'NONE',  ( -0.1974969037888703871, -0.3420746716998661063, -1.167979002624671914 ) ) ;
#2767 = CARTESIAN_POINT ( 'NONE',  ( 0.2925321140481932369, -0.2925321140481932369, -2.618110236220472675 ) ) ;
#2768 = CARTESIAN_POINT ( 'NONE',  ( 0.4091458600556403535, 0.2362204724409449896, -0.6036745406824146620 ) ) ;
#2769 = CARTESIAN_POINT ( 'NONE',  ( -0.3917322834645670104, -7.196005306013484475E-17, -0.3464566929133857665 ) ) ;
#2770 = CARTESIAN_POINT ( 'NONE',  ( -0.1246719160104980823, 0.1771653543307087630, 0.09757992244046791164 ) ) ;
#2771 = CARTESIAN_POINT ( 'NONE',  ( -0.1377952755905504645, 0.1660481256975885056, 0.3530559997133364547 ) ) ;
#2772 = CARTESIAN_POINT ( 'NONE',  ( 0.7283464566929140904, -0.5400638737290845981, -0.3530559997133363437 ) ) ;
#2773 = CARTESIAN_POINT ( 'NONE',  ( 0.1974969037888704704, 0.3420746716998660508, -2.110892388451443225 ) ) ;
#2774 = CARTESIAN_POINT ( 'NONE',  ( -0.2362204724409440182, -0.1870078740157479769, 0.3641732283464567677 ) ) ;
#2775 = CARTESIAN_POINT ( 'NONE',  ( -1.089238845144356427, -0.4281496062992127816, -0.4176697321401328100 ) ) ;
#2776 = CARTESIAN_POINT ( 'NONE',  ( -1.601049868766403650, 0.2306618581243847221, -0.2411417322834647770 ) ) ;
#2777 = CARTESIAN_POINT ( 'NONE',  ( 0.4091458600556404646, -0.2362204724409448231, -1.994750656167979086 ) ) ;
#2778 = CARTESIAN_POINT ( 'NONE',  ( 0.1324727617108047706, 0.3692639355350287866, -2.755905511811024944 ) ) ;
#2779 = ORIENTED_EDGE ( 'NONE', *, *, #31371, .T. ) ;
#2780 = VERTEX_POINT ( 'NONE', #27879 ) ;
#2781 = CARTESIAN_POINT ( 'NONE',  ( 0.9645669291338588858, 0.1660481256975885056, 0.3530559997133364547 ) ) ;
#2782 = CARTESIAN_POINT ( 'NONE',  ( -1.587926509186350810, -0.4281496062992124485, 0.4176697321401328655 ) ) ;
#2784 = CARTESIAN_POINT ( 'NONE',  ( -1.089238845144356427, -0.4281496062992127816, -0.4176697321401328100 ) ) ;
#2783 = CARTESIAN_POINT ( 'NONE',  ( -1.391076115485563314, -0.5023911411419708095, -0.1820866141732282451 ) ) ;
#2785 = CARTESIAN_POINT ( 'NONE',  ( 0.2867679344610365999, -0.2867679344610365999, -2.225702468995064187 ) ) ;
#2786 = CARTESIAN_POINT ( 'NONE',  ( -1.614173228346456712, 1.267785121476993737, -0.1372047244094478091 ) ) ;
#2787 = CARTESIAN_POINT ( 'NONE',  ( 1.364829396325460076, 0.2306618581243848609, 0.2411417322834645549 ) ) ;
#2788 = CARTESIAN_POINT ( 'NONE',  ( -0.3458507752293906723, -0.3458507752293910609, -2.421259842519684735 ) ) ;
#2789 = CARTESIAN_POINT ( 'NONE',  ( -0.1115485564304456306, 0.2952755905511810774, -0.1292274648535930714 ) ) ;
#2790 = CARTESIAN_POINT ( 'NONE',  ( -0.1771653543307080136, -0.5400638737290844871, 0.3530559997133364547 ) ) ;
#2791 = CONICAL_SURFACE ( 'NONE', #82100, 0.1181102362204724116, 0.7853981633974536081 ) ;
#2792 = CARTESIAN_POINT ( 'NONE',  ( -1.200787401574802349, -0.5400638737290844871, 0.3530559997133364547 ) ) ;
#2793 = CARTESIAN_POINT ( 'NONE',  ( -9.594673741351313045E-17, 0.3917322834645670104, 0.07283464566929125084 ) ) ;
#2794 = CARTESIAN_POINT ( 'NONE',  ( 0.1443569553805781891, -0.4281496062992124485, 0.4176697321401328655 ) ) ;
#2795 = CARTESIAN_POINT ( 'NONE',  ( -0.3917322834645671215, 0.1049643490035301469, -1.757217847769028340 ) ) ;
#2796 = CARTESIAN_POINT ( 'NONE',  ( -1.056430446194224881, -0.5511811023622046335, 0.09757992244046803654 ) ) ;
#2797 = VERTEX_POINT ( 'NONE', #53539 ) ;
#2798 = CARTESIAN_POINT ( 'NONE',  ( 0.3949938075777409408, 0.1058382717557500574, -2.486876640419947382 ) ) ;
#2799 = ORIENTED_EDGE ( 'NONE', *, *, #25562, .T. ) ;
#2800 = CARTESIAN_POINT ( 'NONE',  ( -1.496204327613243068, 1.365504603163548047, 0.4422373666565095895 ) ) ;
#2801 = CARTESIAN_POINT ( 'NONE',  ( -1.456692913385826182, -0.6692913385826771977, 8.415575281601705876E-17 ) ) ;
#2802 = CARTESIAN_POINT ( 'NONE',  ( 0.1070741851644053527, 0.3996062992125986590, -0.4658792650918635592 ) ) ;
#2803 = CARTESIAN_POINT ( 'NONE',  ( -1.456692913385826182, -0.6692913385826771977, 8.415575281601705876E-17 ) ) ;
#2804 = CARTESIAN_POINT ( 'NONE',  ( 1.028575266362749208, 1.695109487299528261, -0.4485632242333315589 ) ) ;
#2805 = DIRECTION ( 'NONE',  ( -0.8660254037844431485, 0.000000000000000000, 0.4999999999999918954 ) ) ;
#2806 = DIRECTION ( 'NONE',  ( 0.000000000000000000, 0.000000000000000000, 1.000000000000000000 ) ) ;
#2807 = CARTESIAN_POINT ( 'NONE',  ( 0.3392501089628018884, -0.1958661417322834220, -0.1896325459317586282 ) ) ;
#2808 = CARTESIAN_POINT ( 'NONE',  ( -0.3280839895013117347, -0.004921259842519870586, -0.3153832671262229437 ) ) ;
#2809 = CARTESIAN_POINT ( 'NONE',  ( -0.8070866141732276899, -0.4536011799217367080, 0.2665933059059888421 ) ) ;
#2810 = CARTESIAN_POINT ( 'NONE',  ( -1.207349081364828436, -0.6046776061558807314, 0.2411417322834647770 ) ) ;
#2811 = CARTESIAN_POINT ( 'NONE',  ( 0.9973753280839902091, 0.2306618581243847221, -0.2411417322834647770 ) ) ;
#2812 = CARTESIAN_POINT ( 'NONE',  ( -1.017060367454067249, -0.05778040916215522460, 0.4822834645669289988 ) ) ;
#2813 = CARTESIAN_POINT ( 'NONE',  ( -0.2867679344610364334, -0.2867679344610367109, -0.05118110236220468900 ) ) ;
#2814 = ORIENTED_EDGE ( 'NONE', *, *, #55092, .T. ) ;
#2815 = CARTESIAN_POINT ( 'NONE',  ( -1.430446194225720724, 0.05413385826771626580, -0.4176697321401330321 ) ) ;
#2816 = FACE_BOUND ( 'NONE', #44463, .T. ) ;
#2817 = CARTESIAN_POINT ( 'NONE',  ( 0.2362204724409449064, 0.4091458600556404646, -1.246719160104986734 ) ) ;
#2818 = EDGE_CURVE ( 'NONE', #52641, #21745, #47224, .T. ) ;
#2819 = LINE ( 'NONE', #34387, #49252 ) ;
#2820 = CARTESIAN_POINT ( 'NONE',  ( 0.1049643490035304938, -0.3917322834645669549, -0.7073490813648293241 ) ) ;
#2821 = CARTESIAN_POINT ( 'NONE',  ( 0.1958661417322836440, -0.3392501089628017219, -2.538713910761154491 ) ) ;
#2822 = CARTESIAN_POINT ( 'NONE',  ( -0.7742782152230962556, -0.4281496062992127816, -0.4176697321401328100 ) ) ;
#2823 = CARTESIAN_POINT ( 'NONE',  ( 1.509186351706037543, 0.05413385826771666132, 0.4176697321401328100 ) ) ;
#2824 = CARTESIAN_POINT ( 'NONE',  ( 0.2925321140481932369, 0.2925321140481932369, -0.2145669291338583029 ) ) ;
#2826 = CARTESIAN_POINT ( 'NONE',  ( 0.1990279662527742466, 0.1990279662527742466, 0.1112963449492364726 ) ) ;
#2825 = LINE ( 'NONE', #66811, #26107 ) ;
#2827 = CARTESIAN_POINT ( 'NONE',  ( -1.391076115485563758, 0.2306618581243848609, 0.2411417322834645549 ) ) ;
#2828 = CARTESIAN_POINT ( 'NONE',  ( -0.6036745406824141069, 0.2306618581243848609, 0.2411417322834645549 ) ) ;
#2829 = CARTESIAN_POINT ( 'NONE',  ( 0.1049643490035304522, -0.3917322834645668994, -0.007854699966192403571 ) ) ;
#2830 = CARTESIAN_POINT ( 'NONE',  ( 0.3543307086614179147, 0.1771653543307087630, 0.000000000000000000 ) ) ;
#2831 = CARTESIAN_POINT ( 'NONE',  ( -0.2867679344610364334, -0.2867679344610367109, -0.3011811023622048000 ) ) ;
#2832 = CARTESIAN_POINT ( 'NONE',  ( 0.3477690288713918276, -0.5511811023622048555, -0.09757992244046775898 ) ) ;
#2833 = CARTESIAN_POINT ( 'NONE',  ( 0.8202099737532813073, 0.1771653543307087630, 0.09757992244046791164 ) ) ;
#2834 = CARTESIAN_POINT ( 'NONE',  ( 0.9448818897637802916, -0.1870078740157479769, 0.4822834645669291653 ) ) ;
#2835 = CARTESIAN_POINT ( 'NONE',  ( -0.4921259842519677963, 0.07958543189024071263, -0.2665933059059888421 ) ) ;
#2836 = CARTESIAN_POINT ( 'NONE',  ( -9.594673741351313045E-17, 0.3917322834645670104, -1.724409448818897683 ) ) ;
#2837 = CARTESIAN_POINT ( 'NONE',  ( -1.076115485564303809, -0.6046776061558809534, -0.2411417322834644161 ) ) ;
#2838 = B_SPLINE_CURVE_WITH_KNOTS ( 'NONE', 3,
 ( #62091, #69649, #75151, #62504 ),
 .UNSPECIFIED., .F., .F.,
 ( 4, 4 ),
 ( 3.593986969187450165E-07, 0.001287825409103201223 ),
 .UNSPECIFIED. ) ;
#2839 = CARTESIAN_POINT ( 'NONE',  ( -1.279527559055116948, 0.07958543189024071263, -0.2665933059059888421 ) ) ;
#2840 = CARTESIAN_POINT ( 'NONE',  ( 0.1265901696524989462, 0.4724409448818897572, -0.5426509186351704539 ) ) ;
#2841 = CARTESIAN_POINT ( 'NONE',  ( -1.003937007874014853, 0.07958543189024085140, 0.2665933059059887866 ) ) ;
#2842 = CARTESIAN_POINT ( 'NONE',  ( -0.2755905511811015396, -0.6692913385826771977, 8.415575281601705876E-17 ) ) ;
#2843 = CARTESIAN_POINT ( 'NONE',  ( 1.620734908136483465, -0.5511811023622046335, 0.09757992244046803654 ) ) ;
#2844 = CARTESIAN_POINT ( 'NONE',  ( 0.5643044619422579178, -0.3690944881889765550, -0.3153832671262227771 ) ) ;
#2845 = CARTESIAN_POINT ( 'NONE',  ( -0.1181102362204717315, 0.1771653543307087630, 0.000000000000000000 ) ) ;
#2846 = CARTESIAN_POINT ( 'NONE',  ( -0.8923884514435688198, -0.6046776061558807314, 0.2411417322834647770 ) ) ;
#2847 = FACE_OUTER_BOUND ( 'NONE', #21596, .T. ) ;
#2848 = FACE_OUTER_BOUND ( 'NONE', #8362, .T. ) ;
#2849 = CARTESIAN_POINT ( 'NONE',  ( -0.03280839895013062252, 0.2952755905511810774, -0.1292274648535930714 ) ) ;
#2850 = AXIS2_PLACEMENT_3D ( 'NONE', #63849, #17605, #18426 ) ;
#2851 = VERTEX_POINT ( 'NONE', #40925 ) ;
#2852 = CARTESIAN_POINT ( 'NONE',  ( -0.3460692066303957537, -0.1998031496062994405, -1.704068241469816058 ) ) ;
#2853 = CARTESIAN_POINT ( 'NONE',  ( 1.391076115485564868, -0.6046776061558807314, 0.2411417322834647770 ) ) ;
#2854 = CARTESIAN_POINT ( 'NONE',  ( -0.1246719160104980823, 0.1771653543307087630, 0.09757992244046791164 ) ) ;
#2855 = CARTESIAN_POINT ( 'NONE',  ( -0.1181102362204717315, 0.2952755905511811885, 0.000000000000000000 ) ) ;
#2856 = CARTESIAN_POINT ( 'NONE',  ( -1.620734908136482577, 0.2952755905511811885, 0.1292274648535926551 ) ) ;
#2857 = CARTESIAN_POINT ( 'NONE',  ( -1.607611548556429737, 0.1771653543307087075, -0.09757992244046823083 ) ) ;
#2858 = CARTESIAN_POINT ( 'NONE',  ( 1.141732283464567788, -0.6692913385826771977, 8.415575281601705876E-17 ) ) ;
#2859 = CARTESIAN_POINT ( 'NONE',  ( -0.7020997375328076329, -0.2845877964562161244, -0.3641732283464567121 ) ) ;
#2860 = CARTESIAN_POINT ( 'NONE',  ( 0.4531182788721078158, 1.535433070866141447, 0.5309055118110234117 ) ) ;
#2861 = CARTESIAN_POINT ( 'NONE',  ( 0.1998031496062992740, 0.3460692066303959757, -0.3018372703412073310 ) ) ;
#2862 = CARTESIAN_POINT ( 'NONE',  ( -0.3420746716998661618, 0.1974969037888702206, -0.02624671916010504202 ) ) ;
#2863 = VECTOR ( 'NONE', #13796, 39.37007874015748143 ) ;
#2864 = CARTESIAN_POINT ( 'NONE',  ( -0.01966910102760595011, -0.3928700489057011525, -1.862014699505723656E-17 ) ) ;
#2865 = CARTESIAN_POINT ( 'NONE',  ( 1.345144356955381593, -0.2845877964562161244, -0.3641732283464567121 ) ) ;
#2866 = CARTESIAN_POINT ( 'NONE',  ( -1.601049868766403650, -0.6046776061558807314, 0.2411417322834647770 ) ) ;
#2867 = CARTESIAN_POINT ( 'NONE',  ( 0.9776902887139113929, 0.2952755905511811885, 0.1292274648535926551 ) ) ;
#2868 = CARTESIAN_POINT ( 'NONE',  ( 0.3392501089628018329, 0.1958661417322835607, -2.420603674540682260 ) ) ;
#2869 = CARTESIAN_POINT ( 'NONE',  ( 1.417322834645670104, -0.1870078740157480601, -0.3641732283464567677 ) ) ;
#2870 = CARTESIAN_POINT ( 'NONE',  ( 0.06561679790026316017, -0.4281496062992124485, 0.4176697321401328655 ) ) ;
#2871 = CARTESIAN_POINT ( 'NONE',  ( -0.3412073490813641308, 0.2306618581243847221, -0.2411417322834647770 ) ) ;
#2872 = CARTESIAN_POINT ( 'NONE',  ( 1.476377952755906442, -0.5400638737290844871, 0.3530559997133364547 ) ) ;
#2873 = CARTESIAN_POINT ( 'NONE',  ( -0.1265901696524986964, -0.4724409448818899238, -0.7020997375328084100 ) ) ;
#2874 = CARTESIAN_POINT ( 'NONE',  ( 3.881211926161857395, 2.729373344522950884, 0.5314960629921260393 ) ) ;
#2875 = CARTESIAN_POINT ( 'NONE',  ( 0.5577427821522314977, -0.2845877964562161244, -0.3641732283464567121 ) ) ;
#2876 = EDGE_CURVE ( 'NONE', #59294, #78599, #21767, .T. ) ;
#2877 = ORIENTED_EDGE ( 'NONE', *, *, #3202, .F. ) ;
#2878 = CARTESIAN_POINT ( 'NONE',  ( 0.1049643490035304799, -0.3917322834645670104, -0.2395206281177972019 ) ) ;
#2879 = ORIENTED_EDGE ( 'NONE', *, *, #24425, .T. ) ;
#2880 = CARTESIAN_POINT ( 'NONE',  ( -0.2427821522309703550, -0.05778040916215560624, -0.4822834645669293319 ) ) ;
#2881 = CARTESIAN_POINT ( 'NONE',  ( 0.7020997375328090762, -0.05778040916215560624, -0.4822834645669293319 ) ) ;
#2882 = CARTESIAN_POINT ( 'NONE',  ( 0.1574803149606306130, -0.1870078740157480879, -0.4822834645669291653 ) ) ;
#2883 = CARTESIAN_POINT ( 'NONE',  ( -0.5052493438320203589, 0.1771653543307087075, -0.09757992244046823083 ) ) ;
#2884 = CARTESIAN_POINT ( 'NONE',  ( 0.9711286089238851948, -0.6046776061558809534, -0.2411417322834644161 ) ) ;
#2885 = EDGE_CURVE ( 'NONE', #60134, #49144, #47453, .T. ) ;
#2886 = CARTESIAN_POINT ( 'NONE',  ( -0.7086614173228339419, -0.1870078740157479769, 0.4822834645669291653 ) ) ;
#2887 = CARTESIAN_POINT ( 'NONE',  ( -0.5774278215223089816, 0.2306618581243847221, -0.2411417322834647770 ) ) ;
#2888 = CARTESIAN_POINT ( 'NONE',  ( -0.9645669291338575535, -0.5400638737290844871, 0.3530559997133364547 ) ) ;
#2889 = CARTESIAN_POINT ( 'NONE',  ( 1.358267716535433323, -0.5400638737290845981, -0.3530559997133363437 ) ) ;
#2890 = CARTESIAN_POINT ( 'NONE',  ( 0.8858267716535438430, -0.5400638737290845981, -0.3530559997133363437 ) ) ;
#2891 = CARTESIAN_POINT ( 'NONE',  ( 0.8267716535433078384, -0.6692913385826771977, 8.415575281601705876E-17 ) ) ;
#2892 = CARTESIAN_POINT ( 'NONE',  ( -0.1049643490035307020, 0.3917322834645669549, -0.6286089238845143923 ) ) ;
#2893 = CARTESIAN_POINT ( 'NONE',  ( 0.07217847769028949700, -0.2845877964562159024, 0.3641732283464567677 ) ) ;
#2894 = ORIENTED_EDGE ( 'NONE', *, *, #75879, .T. ) ;
#2895 = CARTESIAN_POINT ( 'NONE',  ( 0.3420746716998660508, -0.1974969037888703871, -0.8923884514435694859 ) ) ;
#2896 = ORIENTED_EDGE ( 'NONE', *, *, #31624, .T. ) ;
#2897 = CARTESIAN_POINT ( 'NONE',  ( -0.9973753280839886548, -0.5023911411419708095, -0.1820866141732282451 ) ) ;
#2898 = CARTESIAN_POINT ( 'NONE',  ( -0.4527559055118102749, -0.5400638737290845981, -0.3530559997133363437 ) ) ;
#2899 = DIRECTION ( 'NONE',  ( 0.000000000000000000, -1.000000000000000000, 0.000000000000000000 ) ) ;
#2900 = CARTESIAN_POINT ( 'NONE',  ( -0.3346456692913377662, -0.5400638737290844871, 0.3530559997133364547 ) ) ;
#2901 = CARTESIAN_POINT ( 'NONE',  ( -0.4002624671916004129, -0.05778040916215560624, -0.4822834645669293319 ) ) ;
#2902 = CARTESIAN_POINT ( 'NONE',  ( -1.476377952755905110, 0.1660481256975885056, 0.3530559997133364547 ) ) ;
#2903 = CARTESIAN_POINT ( 'NONE',  ( -1.384514435695537005, 0.2952755905511811885, 0.1292274648535926551 ) ) ;
#2904 = CARTESIAN_POINT ( 'NONE',  ( 1.056430446194226658, 0.1771653543307087630, 0.09757992244046791164 ) ) ;
#2905 = CARTESIAN_POINT ( 'NONE',  ( 0.000000000000000000, 2.755905511811024056, 0.000000000000000000 ) ) ;
#2906 = CARTESIAN_POINT ( 'NONE',  ( 0.2814587350932031828, 0.08983405572796258898, 5.548838678696989213 ) ) ;
#2907 = CARTESIAN_POINT ( 'NONE',  ( 0.4724409448818904789, -0.1870078740157479769, 0.3641732283464567677 ) ) ;
#2908 = CARTESIAN_POINT ( 'NONE',  ( -0.1049868766404193215, -0.6046776061558807314, 0.2411417322834647770 ) ) ;
#2909 = CARTESIAN_POINT ( 'NONE',  ( 0.3674540682414705883, -0.6046776061558807314, 0.2411417322834647770 ) ) ;
#2910 = VERTEX_POINT ( 'NONE', #48057 ) ;
#2911 = AXIS2_PLACEMENT_3D ( 'NONE', #35097, #47712, #60355 ) ;
#2912 = CARTESIAN_POINT ( 'NONE',  ( 4.893765752498283924E-17, -0.3996062992125986035, -1.653543307086614123 ) ) ;
#2913 = CARTESIAN_POINT ( 'NONE',  ( -0.5774278215223089816, 0.1539470093639521697, -0.1968503937007875793 ) ) ;
#2914 = VERTEX_POINT ( 'NONE', #9356 ) ;
#2915 = CARTESIAN_POINT ( 'NONE',  ( -0.2925321140481930149, -0.2925321140481933480, -1.238188976377952999 ) ) ;
#2916 = CARTESIAN_POINT ( 'NONE',  ( -0.3996062992125984925, -0.1070741851644056858, -0.5951443569553805935 ) ) ;
#2917 = CARTESIAN_POINT ( 'NONE',  ( -0.5971128608923877978, 0.1771653543307087630, 0.09757992244046791164 ) ) ;
#2918 = CARTESIAN_POINT ( 'NONE',  ( -0.5118110236220466680, -0.6692913385826771977, 8.415575281601705876E-17 ) ) ;
#2919 = CARTESIAN_POINT ( 'NONE',  ( -0.3458507752293906723, -0.3458507752293910609, 0.09842519685039372024 ) ) ;
#2920 = CARTESIAN_POINT ( 'NONE',  ( -0.1049643490035302024, -0.3917322834645671215, -2.519028871391075786 ) ) ;
#2921 = CARTESIAN_POINT ( 'NONE',  ( 1.601049868766404982, -0.6046776061558809534, -0.2411417322834644161 ) ) ;
#2922 = CARTESIAN_POINT ( 'NONE',  ( 0.6955380577427828781, 0.05413385826771626580, -0.4176697321401330321 ) ) ;
#2923 = CARTESIAN_POINT ( 'NONE',  ( 1.003937007874016407, -0.5400638737290844871, 0.3530559997133364547 ) ) ;
#2924 = CARTESIAN_POINT ( 'NONE',  ( -0.5577427821522301654, -0.2845877964562159024, 0.3641732283464567677 ) ) ;
#2925 = CARTESIAN_POINT ( 'NONE',  ( 0.2099737532808405305, 0.2306618581243847221, -0.2411417322834647770 ) ) ;
#2926 = CARTESIAN_POINT ( 'NONE',  ( -0.4091458600556405756, 0.2362204724409446288, -1.992782152230971437 ) ) ;
#2927 = CARTESIAN_POINT ( 'NONE',  ( -0.07874015748031421014, -0.1870078740157479769, 0.3641732283464567677 ) ) ;
#2928 = CARTESIAN_POINT ( 'NONE',  ( -0.6299212598425188991, -0.1870078740157479769, 0.4822834645669291653 ) ) ;
#2929 = CARTESIAN_POINT ( 'NONE',  ( -0.3949938075777409963, -7.255918531996591613E-17, -1.848425196850393970 ) ) ;
#2930 = CARTESIAN_POINT ( 'NONE',  ( 1.528871391076116026, -0.5511811023622048555, -0.09757992244046775898 ) ) ;
#2931 = CARTESIAN_POINT ( 'NONE',  ( 0.2427821522309716595, -0.2845877964562161244, -0.3641732283464567121 ) ) ;
#2932 = CYLINDRICAL_SURFACE ( 'NONE', #72948, 0.2952755905511810774 ) ;
#2933 = CARTESIAN_POINT ( 'NONE',  ( -1.036745406824146176, 0.05413385826771626580, -0.4176697321401330321 ) ) ;
#2934 = CARTESIAN_POINT ( 'NONE',  ( -0.5905511811023613777, -0.5511811023622047445, 6.969142054262312111E-17 ) ) ;
#2935 = CARTESIAN_POINT ( 'NONE',  ( -1.313877454013331780, 0.2755905511811023723, 0.6792347910202041206 ) ) ;
#2936 = CARTESIAN_POINT ( 'NONE',  ( -1.036745406824146176, 0.05413385826771626580, -0.4176697321401330321 ) ) ;
#2937 = CARTESIAN_POINT ( 'NONE',  ( 0.09186351706036827158, 0.05413385826771666132, 0.4176697321401328100 ) ) ;
#2938 = CARTESIAN_POINT ( 'NONE',  ( -0.3460692066303957537, -0.1998031496062994405, -2.648950131233595684 ) ) ;
#2939 = CARTESIAN_POINT ( 'NONE',  ( 0.3917322834645668994, 0.1049643490035304522, -2.409429503115799065 ) ) ;
#2940 = CARTESIAN_POINT ( 'NONE',  ( -2.058022911372341834, 1.301102360844738515, -0.4123394245947631376 ) ) ;
#2941 = CARTESIAN_POINT ( 'NONE',  ( 0.2559055118110243332, 0.07958543189024085140, 0.2665933059059887866 ) ) ;
#2942 = CARTESIAN_POINT ( 'NONE',  ( 0.8989501312335963501, -0.6692913385826773087, -0.1292274648535924053 ) ) ;
#2943 = CARTESIAN_POINT ( 'NONE',  ( -1.246719160104986512, -0.004921259842519576551, 0.3153832671262227771 ) ) ;
#2944 = CARTESIAN_POINT ( 'NONE',  ( 1.056430446194226658, 0.2952755905511811885, 0.1292274648535926551 ) ) ;
#2945 = CARTESIAN_POINT ( 'NONE',  ( -1.377952755905511140, 0.1771653543307087630, 0.000000000000000000 ) ) ;
#2946 = CARTESIAN_POINT ( 'NONE',  ( -0.6102362204724400829, 0.1660481256975885056, 0.3530559997133364547 ) ) ;
#2947 = CARTESIAN_POINT ( 'NONE',  ( 0.1443569553805781891, -0.004921259842519870586, -0.3153832671262229437 ) ) ;
#2948 = CARTESIAN_POINT ( 'NONE',  ( 0.3458507752293908943, -0.3458507752293908943, -0.8858267716535431768 ) ) ;
#2949 = CARTESIAN_POINT ( 'NONE',  ( 0.5118110236220478892, 0.1771653543307087630, 0.000000000000000000 ) ) ;
#2950 = CARTESIAN_POINT ( 'NONE',  ( 0.09842519685039434474, 0.1660481256975885056, 0.3530559997133364547 ) ) ;
#2951 = CARTESIAN_POINT ( 'NONE',  ( 0.3460692066303958092, 0.1998031496062993018, -0.3654855643044619407 ) ) ;
#2952 = CARTESIAN_POINT ( 'NONE',  ( -1.207349081364828880, 0.2306618581243847221, -0.2411417322834647770 ) ) ;
#2953 = CARTESIAN_POINT ( 'NONE',  ( -0.2867679344610364334, -0.2867679344610367109, -1.875984251968503935 ) ) ;
#2954 = CARTESIAN_POINT ( 'NONE',  ( 1.095800524934383846, -0.2845877964562159024, 0.3641732283464567677 ) ) ;
#2955 = CARTESIAN_POINT ( 'NONE',  ( -0.04593175853018302557, 0.2952755905511811885, 0.1292274648535926551 ) ) ;
#2956 = CARTESIAN_POINT ( 'NONE',  ( -0.4265091863517051496, -0.6692913385826771977, 0.1292274648535927661 ) ) ;
#2957 = CARTESIAN_POINT ( 'NONE',  ( -0.2690288713910754526, -0.5511811023622046335, 0.09757992244046803654 ) ) ;
#2958 = CARTESIAN_POINT ( 'NONE',  ( 1.200787401574803903, 0.1660481256975885056, 0.3530559997133364547 ) ) ;
#2959 = CARTESIAN_POINT ( 'NONE',  ( -0.4527559055118102749, -0.4536011799217368745, -0.2665933059059886201 ) ) ;
#2960 = CARTESIAN_POINT ( 'NONE',  ( 0.2624671916010504757, 0.2306618581243848609, 0.2411417322834645549 ) ) ;
#2961 = CARTESIAN_POINT ( 'NONE',  ( -0.9186351706036736120, 0.1283753931104748280, 0.1820866141732283561 ) ) ;
#2962 = CARTESIAN_POINT ( 'NONE',  ( 0.3996062992125985480, 2.446882876249141654E-17, -0.9822834645669291653 ) ) ;
#2963 = CARTESIAN_POINT ( 'NONE',  ( -1.200787401574802349, -0.5400638737290844871, 0.3530559997133364547 ) ) ;
#2964 = DIRECTION ( 'NONE',  ( -0.000000000000000000, -1.000000000000000000, -0.000000000000000000 ) ) ;
#2965 = ORIENTED_EDGE ( 'NONE', *, *, #41074, .F. ) ;
#2966 = CARTESIAN_POINT ( 'NONE',  ( -1.069553805774277722, 0.1771653543307087630, 0.09757992244046791164 ) ) ;
#2967 = AXIS2_PLACEMENT_3D ( 'NONE', #5229, #75124, #23343 ) ;
#2968 = CARTESIAN_POINT ( 'NONE',  ( -0.2755905511811018171, 0.2952755905511811885, 0.000000000000000000 ) ) ;
#2969 = CARTESIAN_POINT ( 'NONE',  ( 0.3960428127060660608, 0.01218835185196203222, -1.220472440944882386 ) ) ;
#2970 = CARTESIAN_POINT ( 'NONE',  ( -1.345144356955379816, -0.3162353388693405765, 0.4822834645669290543 ) ) ;
#2971 = DIRECTION ( 'NONE',  ( -1.000000000000000000, -2.312964634635741971E-16, 0.000000000000000000 ) ) ;
#2972 = CARTESIAN_POINT ( 'NONE',  ( 1.528871391076116026, 0.2952755905511811885, 0.1292274648535926551 ) ) ;
#2973 = CARTESIAN_POINT ( 'NONE',  ( 0.6561679790026253567, -0.6046776061558809534, -0.2411417322834644161 ) ) ;
#2974 = DIRECTION ( 'NONE',  ( 0.000000000000000000, 0.000000000000000000, -1.000000000000000000 ) ) ;
#2975 = CARTESIAN_POINT ( 'NONE',  ( 0.2917579853797115930, -0.04689358074580353419, 5.530719428720964892 ) ) ;
#2976 = CARTESIAN_POINT ( 'NONE',  ( -1.719160104986876103, 0.05413385826771666132, 0.4176697321401328100 ) ) ;
#2977 = ADVANCED_FACE ( 'NONE', ( #73336 ), #66183, .F. ) ;
#2978 = CARTESIAN_POINT ( 'NONE',  ( 0.1998031496062994405, -0.3460692066303958092, -0.5643044619422572516 ) ) ;
#2979 = VERTEX_POINT ( 'NONE', #15685 ) ;
#2980 = CARTESIAN_POINT ( 'NONE',  ( -0.6233595800524928121, -0.2845877964562161244, -0.3641732283464567121 ) ) ;
#2981 = CARTESIAN_POINT ( 'NONE',  ( -0.1049643490035302024, -0.3917322834645671215, -2.426509186351705427 ) ) ;
#2982 = ORIENTED_EDGE ( 'NONE', *, *, #64100, .F. ) ;
#2983 = CARTESIAN_POINT ( 'NONE',  ( 0.6430446194225728496, 0.05413385826771666132, 0.4176697321401328100 ) ) ;
#2984 = CARTESIAN_POINT ( 'NONE',  ( -0.3937007874015740483, -0.1870078740157480879, -0.4822834645669291653 ) ) ;
#2985 = CARTESIAN_POINT ( 'NONE',  ( -0.7217847769028863381, -0.4281496062992124485, 0.4176697321401328655 ) ) ;
#2986 = CARTESIAN_POINT ( 'NONE',  ( 1.299212598425197429, -0.6692913385826771977, 8.415575281601705876E-17 ) ) ;
#2987 = CARTESIAN_POINT ( 'NONE',  ( -1.502624671916009680, -0.2845877964562159024, 0.3641732283464567677 ) ) ;
#2988 = CARTESIAN_POINT ( 'NONE',  ( -0.4724409448818914226, -0.1265901696524962816, -2.012467191601050143 ) ) ;
#2989 = CARTESIAN_POINT ( 'NONE',  ( 0.5380577427821529035, -0.4281496062992124485, 0.4176697321401328655 ) ) ;
#2990 = CARTESIAN_POINT ( 'NONE',  ( -0.7939632545931750718, -0.05778040916215560624, -0.4822834645669293319 ) ) ;
#2991 = CARTESIAN_POINT ( 'NONE',  ( 4.797336870675655290E-17, -0.3917322834645669549, -1.576096169782465140 ) ) ;
#2992 = CARTESIAN_POINT ( 'NONE',  ( -1.161417322834644716, 0.1660481256975885056, 0.3530559997133364547 ) ) ;
#2993 = PLANE ( 'NONE',  #27790 ) ;
#2994 = CARTESIAN_POINT ( 'NONE',  ( 1.036745406824147731, 0.05413385826771666132, 0.4176697321401328100 ) ) ;
#2995 = CARTESIAN_POINT ( 'NONE',  ( 1.082677165354331228, 0.07958543189024071263, -0.2665933059059888421 ) ) ;
#2996 = EDGE_LOOP ( 'NONE', ( #15859, #23992, #77417, #3808 ) ) ;
#2997 = CARTESIAN_POINT ( 'NONE',  ( 0.3420746716998659953, 0.1974969037888705536, 0.02624671916010492753 ) ) ;
#2998 = CARTESIAN_POINT ( 'NONE',  ( -0.6299212598425188991, -0.1870078740157480879, -0.4822834645669291653 ) ) ;
#2999 = EDGE_LOOP ( 'NONE', ( #27644, #63108, #51265, #67302 ) ) ;
#3000 = CARTESIAN_POINT ( 'NONE',  ( 0.2165354330708668673, 0.07958543189024071263, -0.2665933059059888421 ) ) ;
#3001 = CARTESIAN_POINT ( 'NONE',  ( -1.010498687664041384, -0.4281496062992127816, -0.4176697321401328100 ) ) ;
#3002 = CARTESIAN_POINT ( 'NONE',  ( 0.9055118110236227702, -0.6692913385826771977, 8.415575281601705876E-17 ) ) ;
#3003 = CARTESIAN_POINT ( 'NONE',  ( 0.8661417322834652488, -0.1870078740157480879, -0.4822834645669291653 ) ) ;
#3004 = CARTESIAN_POINT ( 'NONE',  ( -0.3149606299212590610, -0.1870078740157479769, 0.4822834645669291653 ) ) ;
#3005 = CARTESIAN_POINT ( 'NONE',  ( -0.8333333333333323711, 0.2952755905511811885, 0.1292274648535926551 ) ) ;
#3006 = CARTESIAN_POINT ( 'NONE',  ( -0.3392501089628017219, -0.1958661417322836718, -2.341863517060367439 ) ) ;
#3007 = CARTESIAN_POINT ( 'NONE',  ( -1.456692913385826182, -0.6692913385826771977, 8.415575281601705876E-17 ) ) ;
#3008 = CARTESIAN_POINT ( 'NONE',  ( -0.6561679790026240244, 0.2306618581243847221, -0.2411417322834647770 ) ) ;
#3009 = CARTESIAN_POINT ( 'NONE',  ( -0.5380577427821514602, -0.004921259842519576551, 0.3153832671262227771 ) ) ;
#3010 = CARTESIAN_POINT ( 'NONE',  ( 1.482939632545932307, -0.4281496062992124485, 0.4176697321401328655 ) ) ;
#3011 = CARTESIAN_POINT ( 'NONE',  ( 1.482939632545932307, -0.4281496062992124485, 0.4176697321401328655 ) ) ;
#3012 = CARTESIAN_POINT ( 'NONE',  ( -0.7939632545931754048, -0.3162353388693405765, 0.4822834645669290543 ) ) ;
#3013 = CARTESIAN_POINT ( 'NONE',  ( -0.5314960629921371416, 2.742783271717982974, 3.197598480811213673 ) ) ;
#3014 = CARTESIAN_POINT ( 'NONE',  ( 0.8202099737532813073, 0.2952755905511811885, 0.1292274648535926551 ) ) ;
#3015 = CARTESIAN_POINT ( 'NONE',  ( -0.2925321140481930704, -0.2925321140481933480, -1.791338582677165059 ) ) ;
#3016 = DIRECTION ( 'NONE',  ( -0.000000000000000000, 1.000000000000000000, -0.000000000000000000 ) ) ;
#3017 = CARTESIAN_POINT ( 'NONE',  ( -0.2624671916010490880, -0.6046776061558807314, 0.2411417322834647770 ) ) ;
#3018 = CARTESIAN_POINT ( 'NONE',  ( -1.023622047244093558, -0.1870078740157479769, 0.3641732283464567677 ) ) ;
#3019 = CARTESIAN_POINT ( 'NONE',  ( 0.9448818897637802916, -0.1870078740157480601, -0.3641732283464567677 ) ) ;
#3020 = CARTESIAN_POINT ( 'NONE',  ( 0.1265901696524990294, -0.4724409448818896462, -0.6345144356955381149 ) ) ;
#3021 = CARTESIAN_POINT ( 'NONE',  ( 1.325459317585302665, -0.3690944881889763329, 0.3153832671262228327 ) ) ;
#3022 = CARTESIAN_POINT ( 'NONE',  ( 0.6824146981627303710, 0.2306618581243847221, -0.2411417322834647770 ) ) ;
#3023 = CARTESIAN_POINT ( 'NONE',  ( 0.1058382717557499880, 0.3949938075777409408, -0.3851706036745406458 ) ) ;
#3024 = PRODUCT ( 'Reversible Hardened Steel Jaws', 'Reversible Hardened Steel Jaws', '', ( #41826 ) ) ;
#3025 = CARTESIAN_POINT ( 'NONE',  ( -0.3215223097112853146, -0.3162353388693405765, 0.4822834645669290543 ) ) ;
#3026 = DIRECTION ( 'NONE',  ( 0.000000000000000000, 0.000000000000000000, -1.000000000000000000 ) ) ;
#3027 = CARTESIAN_POINT ( 'NONE',  ( 1.312335958005249825, 0.1283753931104746893, -0.1820866141732285504 ) ) ;
#3028 = CARTESIAN_POINT ( 'NONE',  ( -0.3937007874015740483, -0.1870078740157480879, -0.4822834645669291653 ) ) ;
#3029 = CARTESIAN_POINT ( 'NONE',  ( -0.1058382717557503072, 0.3949938075777408852, -0.5557742782152231831 ) ) ;
#3030 = CARTESIAN_POINT ( 'NONE',  ( 1.292650918635171564, -0.6692913385826773087, -0.1292274648535924053 ) ) ;
#3031 = CARTESIAN_POINT ( 'NONE',  ( 0.3083989501312343062, -0.3162353388693405765, 0.4822834645669290543 ) ) ;
#3032 = AXIS2_PLACEMENT_3D ( 'NONE', #58636, #79273, #2656 ) ;
#3033 = CARTESIAN_POINT ( 'NONE',  ( 0.5971128608923891301, 0.1771653543307087075, -0.09757992244046823083 ) ) ;
#3034 = DIRECTION ( 'NONE',  ( 0.000000000000000000, 0.000000000000000000, -1.000000000000000000 ) ) ;
#3035 = CARTESIAN_POINT ( 'NONE',  ( 0.5314960629921267055, -0.4536011799217367080, 0.2665933059059888421 ) ) ;
#3036 = CARTESIAN_POINT ( 'NONE',  ( -1.509186351706035767, -0.4281496062992124485, 0.4176697321401328655 ) ) ;
#3037 = CARTESIAN_POINT ( 'NONE',  ( 0.3996062992125985480, 2.446882876249141654E-17, -1.297244094488189115 ) ) ;
#3038 = CARTESIAN_POINT ( 'NONE',  ( 0.9120734908136490793, 0.2952755905511810774, -0.1292274648535930714 ) ) ;
#3039 = CARTESIAN_POINT ( 'NONE',  ( -0.3392501089628017219, -0.1958661417322836718, -1.146981627296587813 ) ) ;
#3040 = DIRECTION ( 'NONE',  ( -1.000000000000000000, -0.000000000000000000, -0.000000000000000000 ) ) ;
#3041 = CARTESIAN_POINT ( 'NONE',  ( -0.2661962643026954400, 0.2881610400590603471, -1.506228638669167268E-17 ) ) ;
#3042 = CARTESIAN_POINT ( 'NONE',  ( -0.05249343832020938322, -0.5023911411419708095, -0.1820866141732282451 ) ) ;
#3043 = CARTESIAN_POINT ( 'NONE',  ( 0.2362204724409456558, -0.1870078740157479769, 0.4822834645669291653 ) ) ;
#3044 = CARTESIAN_POINT ( 'NONE',  ( 1.312335958005250269, -0.5023911411419708095, 0.1820866141732285504 ) ) ;
#3045 = CARTESIAN_POINT ( 'NONE',  ( -1.181102362204723644, -0.1870078740157480601, -0.3641732283464567677 ) ) ;
#3046 = CARTESIAN_POINT ( 'NONE',  ( -1.515748031496062076, 0.1660481256975883668, -0.3530559997133364547 ) ) ;
#3047 = CARTESIAN_POINT ( 'NONE',  ( 0.3871391076115493490, -0.3162353388693405765, 0.4822834645669290543 ) ) ;
#3048 = CARTESIAN_POINT ( 'NONE',  ( 1.102362204724410155, -0.1870078740157480879, -0.4822834645669291653 ) ) ;
#3049 = CARTESIAN_POINT ( 'NONE',  ( 1.603475055217291612, 0.7793870273546370520, 0.04573490813648269093 ) ) ;
#3050 = CARTESIAN_POINT ( 'NONE',  ( 0.6692913385826777528, 0.2952755905511811885, 0.000000000000000000 ) ) ;
#3051 = CARTESIAN_POINT ( 'NONE',  ( 1.384514435695538559, 0.2952755905511810774, -0.1292274648535930714 ) ) ;
#3052 = CARTESIAN_POINT ( 'NONE',  ( 1.122047244094488860, -0.5400638737290845981, -0.3530559997133363437 ) ) ;
#3053 = CARTESIAN_POINT ( 'NONE',  ( -0.4091458600556402980, -0.2362204724409451284, -0.2867454068241469534 ) ) ;
#3054 = CARTESIAN_POINT ( 'NONE',  ( 0.6364829396325465405, -0.2845877964562161244, -0.3641732283464567121 ) ) ;
#3055 = CARTESIAN_POINT ( 'NONE',  ( -1.555118110236219930, -0.4536011799217368745, -0.2665933059059886201 ) ) ;
#3056 = CARTESIAN_POINT ( 'NONE',  ( -0.7217847769028863381, -0.3690944881889763329, 0.3153832671262228327 ) ) ;
#3057 = CARTESIAN_POINT ( 'NONE',  ( 0.6627296587926515548, 0.1771653543307087630, 0.09757992244046791164 ) ) ;
#3058 = CARTESIAN_POINT ( 'NONE',  ( 0.03280839895013198948, -0.6692913385826773087, -0.1292274648535924053 ) ) ;
#3059 = CARTESIAN_POINT ( 'NONE',  ( 0.6233595800524939223, -0.3162353388693405765, 0.4822834645669290543 ) ) ;
#3060 = CARTESIAN_POINT ( 'NONE',  ( -0.4921259842519677963, 0.1660481256975883668, -0.3530559997133364547 ) ) ;
#3061 = CARTESIAN_POINT ( 'NONE',  ( 0.3018372703412079971, -0.3690944881889763329, 0.3153832671262228327 ) ) ;
#3062 = CARTESIAN_POINT ( 'NONE',  ( 0.8661417322834652488, -0.1870078740157480879, -0.4822834645669291653 ) ) ;
#3063 = EDGE_CURVE ( 'NONE', #8792, #38980, #1493, .T. ) ;
#3064 = DIRECTION ( 'NONE',  ( 0.000000000000000000, -1.000000000000000000, -0.000000000000000000 ) ) ;
#3065 = CARTESIAN_POINT ( 'NONE',  ( -0.7874015748031489847, -0.1870078740157479769, 0.4822834645669291653 ) ) ;
#3067 = CARTESIAN_POINT ( 'NONE',  ( -0.2925321140481930704, -0.2925321140481933480, -0.8464566929133857665 ) ) ;
#3066 = CARTESIAN_POINT ( 'NONE',  ( 0.000000000000000000, 0.03937007874015747977, 0.000000000000000000 ) ) ;
#3068 = CARTESIAN_POINT ( 'NONE',  ( 1.012125901091929681, 2.412178165100495768E-16, -0.3791483426435169890 ) ) ;
#3069 = CARTESIAN_POINT ( 'NONE',  ( -0.6955380577427815458, 0.05413385826771666132, 0.4176697321401328100 ) ) ;
#3070 = CARTESIAN_POINT ( 'NONE',  ( -0.6233595800524928121, -0.05778040916215522460, 0.4822834645669289988 ) ) ;
#3071 =( BOUNDED_SURFACE ( )  B_SPLINE_SURFACE ( 1, 2, ( 
 ( #13545, #26994, #19856, #45505, #25732, #33326, #14807, #46345, #64884, #58562, #33735, #78782, #71202, #39201, #65739, #928, #26585, #52657, #77942, #20271, #45921, #78363, #27410, #20694, #46766, #72040, #40466, #79, #1344, #59395, #13971, #58988, #41695, #74118, #72869, #79202, #42109, #34569, #61058, #35393, #66978, #47594, #48010, #80853, #67806, #42519, #53493, #27832, #80031, #21934, #3409, #16881, #74535, #48834, #10143, #28661, #40877, #16464, #23165, #29071, #34150, #80447, #61474, #21518, #8481, #54742, #47177, #35808, #3822, #29483, #59811, #22350, #15217, #41293, #2166, #9311, #55142, #66559, #9722, #73709, #8892, #60236, #15636, #2584, #28243, #73288, #22757, #34981, #54322, #53903, #79617, #60645, #48419, #2995, #16049, #67388, #29888, #82898, #37448, #55551, #76176, #44156, #18513, #57196, #82084, #81260, #17697, #68222, #69025, #37857, #12199, #69443, #56385, #50884, #36214, #61883, #4224, #23575, #74949, #25218, #43738, #76584, #49246, #17295, #10957, #11795, #18913, #63122, #18105, #5460, #69848, #42922, #43325, #31122, #5053, #10556, #68617, #36615, #62293, #4630, #30301, #63533, #55967, #81680, #50472, #23991, #49659, #56789, #5864, #24805, #82489, #50068, #75349, #31540, #30723, #11376, #37033, #62715, #24398, #75763, #20168, #819, #26481, #19328, #20590, #77414, #58033, #81349, #78680, #78259, #58459, #51713, #64363, #39951, #45818, #19750, #13863, #14287, #26891, #63944, #6281, #7967, #1650, #65637, #33630, #7547, #44980, #45404, #52550, #76997, #7119, #51294, #59293, #70676, #12609, #6700, #38267, #27307, #58883, #64781, #46242, #52966, #31957, #32790, #57618, #52132, #13032, #71938, #44563, #38685, #25631, #70254, #32369, #39522, #71517, #71100, #396, #77839, #26054, #13443, #39099, #65210, #33220, #1242, #34462, #73607, #29381, #60542, #2482, #60951, #28141, #53797, #21825, #16359, #72357, #47899, #40768, #8378, #66453, #79509, #55041, #8789, #3717, #47072, #53392, #15949, #21001, #2893, #15114, #66040, #34043, #10034, #41595, #54213, #67698, #59706, #74012, #46663, #14705, #47488, #15530, #34881, #67285, #40360, #3301, #42004, #28557, #2061, #72763, #9208, #27725, #79099, #73180, #35698, #21418, #60131, #41188, #66878, #79929, #22244, #9618, #35289, #28966, #54630, #80343, #22656, #48315, #61365, #43227, #43638, #24296, #4123, #23474, #42823, #69341, #36932, #68924, #49141, #56689, #62193, #49557, #81572, #49966, #4530, #75664, #36111, #74846, #74427, #81982, #63428, #11692, #30200, #55862, #82388, #18414, #29788, #81158, #5360, #23891, #55449, #18004, #68516, #75251, #61783, #37349, #76072, #63022, #12095, #31021, #37753, #5764, #24706, #50374, #44057, #31433, #30620, #69749, #17190, #10857, #36517, #80748, #62610, #11273, #17595, #23062, #4950, #56285, #48730, #16774, #42412, #68109, #10457, #83205, #50785, #58350, #39842, #71414, #6595, #32267, #58778, #78155, #6177, #57514, #65102, #57927, #31852, #52028, #19220, #64261, #38165, #77734, #52445, #45717, #71835, #20065, #14184, #65531, #26370, #13761, #39418, #7864, #7015, #7439, #63839, #44460, #33110, #25527, #1138, #711, #291, #12923, #13339, #46140, #26788, #57096, #18813, #76486, #45300, #70569, #20486, #82791, #38993, #38582, #25113, #25947, #51605, #77310, #70151, #12504, #51192, #76890, #44870, #19640, #70996, #64676, #32683, #16263, #59606, #65940, #2796, #67602, #15430, #27623, #78577, #20903, #22564, #28455, #66779, #80248, #72254, #3208, #33528, #27204, #8692, #28040, #47389, #54115, #41908, #73508, #28870, #73080, #59191, #1961, #21726, #14603, #8276, #34362, #48225, #40257, #33942, #53286, #78997, #21317, #46970, #72664, #47805, #41090, #34785, #22147, #15013, #40669, #15856, #79407, #79830, #60444, #66354, #60028, #1550, #2383, #52867, #53698, #9113, #41505, #46556, #67190, #9521, #35193, #60854, #73921, #54532, #43137, #56596, #48637, #62932, #9933, #3621, #68427, #4443, #23794, #30526, #18321, #49873, #5265, #49466, #35605, #36020, #81477, #74331, #68016, #10767, #82296, #16678, #10360, #61692, #4032, #42317, #29697, #55360, #24202, #75160, #11180 ),
 ( #37256, #17913, #81065, #75573, #68834, #17505, #36841, #23381, #69250, #42731, #49049, #74747, #43962, #43549, #62513, #17096, #36427, #30929, #4851, #62100, #56189, #24615, #11596, #29288, #54951, #50282, #75980, #61267, #80658, #81891, #30108, #55770, #22970, #32486, #13562, #58149, #71635, #518, #12002, #26171, #69658, #39643, #77959, #64901, #45937, #13987, #63334, #7238, #6816, #32912, #51832, #65334, #37656, #39216, #26601, #77537, #58578, #52253, #19872, #20288, #45521, #943, #71217, #13654, #39307, #6494, #57411, #32164, #6075, #58242, #38477, #78049, #52762, #76785, #77204, #78470, #57820, #51499, #64994, #19533, #59088, #7330, #19117, #25423, #32998, #12402, #58668, #39732, #31749, #1443, #1033, #83104, #20378, #46030, #71724, #27100, #608, #51088, #45190, #70047, #70893, #65428, #14080, #71307, #26264, #20795, #38059, #63736, #44766, #70463, #12820, #64161, #45613, #187, #25840, #13243, #38892, #26687, #64571, #52342, #19962, #7761, #33427, #6908, #32580, #51925, #77630, #46451, #21209, #1855, #65837, #80552, #78888, #22458, #59502, #8584, #28764, #66246, #53173, #41398, #41799, #3100, #79721, #28348, #35496, #35082, #9005, #16152, #73815, #54427, #46864, #80137, #22038, #2688, #54009, #72558, #48117, #79302, #59917, #27517, #72144, #67490, #60340, #53593, #34256, #9826, #47698, #21620, #15744, #61161, #3512, #8170, #33835, #29181, #54848, #14500, #40153, #9412, #14905, #47280, #40565, #2272, #34677, #27935, #72970, #15321, #40986, #66666, #73393, #67080, #60748, #43031, #82193, #75872, #16570, #11067, #18215, #67911, #37555, #75466, #10247, #30826, #24510, #56491, #11901, #36725, #35918, #55660, #22864, #23683, #43850, #50177, #24097, #62401, #5569, #74225, #42215, #61584, #3929, #29588, #63229, #81786, #31234, #55251, #80958, #48942, #49766, #56901, #17805, #56081, #43439, #69553, #23273, #81370, #69136, #68726, #48525, #74644, #16986, #42629, #68326, #10664, #36319, #61994, #4331, #5162, #29997, #49357, #11488, #75054, #62827, #37142, #4740, #17401, #30413, #45092, #52250, #26598, #7235, #83006, #64898, #58146, #38799, #64475, #57308, #58575, #32067, #12721, #37965, #33339, #32908, #13148, #6397, #19023, #77955, #515, #57728, #51829, #20284, #940, #18620, #44263, #45933, #39640, #71632, #13984, #45518, #25327, #91, #65331, #31650, #70796, #5979, #7668, #50991, #50582, #44671, #76289, #82595, #13557, #19441, #24914, #69954, #12308, #6812, #63641, #32483, #76689, #70366, #38381, #64057, #25744, #51407, #77109, #26168, #77534, #19869, #71214, #39213, #65751, #14410, #79630, #1356, #47607, #34994, #40479, #27846, #59824, #2598, #66157, #53917, #40064, #1765, #52669, #60250, #41710, #73301, #8496, #34163, #60659, #80046, #8084, #59408, #66992, #2179, #33747, #21948, #21120, #53507, #27422, #15650, #54336, #41306, #73724, #9324, #16063, #67402, #28256, #3008, #28675, #9737, #8906, #22365, #53083, #46359, #48024, #78796, #59001, #27007, #79215, #14820, #15231, #78376, #20707, #72053, #46780, #72471, #47190, #21531, #72882, #40890, #66572, #34582, #75363, #16895, #10157, #75777, #35408, #62307, #4644, #55156, #22771, #80867, #10571, #43751, #23179, #18118, #61489, #67820, #30315, #69457, #17309, #29497, #80462, #48434, #24411, #55983, #68631, #82097, #74133, #5067, #61072, #29086, #36228, #29902, #49261, #81694, #3423, #17711, #30736, #74963, #54756, #3837, #23590, #16478, #35823, #61897, #50081, #42125, #48849, #74550, #42534, #68236, #4238, #55566, #49673, #42937, #36630, #24005, #81274, #10971, #43339, #69040, #11390, #37047, #62729, #56399, #58360, #59201, #52455, #58790, #37871, #59616, #27214, #33120, #72265, #65950, #5474, #1148, #31136, #26799, #64686, #20913, #79008, #18526, #20076, #21328, #32693, #77744, #39852, #45727, #1971, #33538, #44169, #50485, #1560, #37462, #52877, #8286, #56803, #27634, #65543, #82502, #46566, #14613, #40267, #53296, #78165, #24818, #71424, #11807, #13771, #33952, #46980, #14195, #20496, #63135, #76189, #69862, #12213, #7025, #722, #26380, #71845, #52040, #39428, #65112, #7450, #7874, #46150, #78587 ) ),
 .UNSPECIFIED., .F., .F., .F. ) 
 B_SPLINE_SURFACE_WITH_KNOTS ( ( 2, 2 ),
 ( 3, 2, 2, 2, 2, 2, 2, 2, 2, 2, 2, 2, 2, 2, 2, 2, 2, 2, 2, 2, 2, 2, 2, 2, 2, 2, 2, 2, 2, 2, 2, 2, 2, 2, 2, 2, 2, 2, 2, 2, 2, 2, 2, 2, 2, 2, 2, 2, 2, 2, 2, 2, 2, 2, 2, 2, 2, 2, 2, 2, 2, 2, 2, 2, 2, 2, 2, 2, 2, 2, 2, 2, 2, 2, 2, 2, 2, 2, 2, 2, 2, 2, 2, 2, 2, 2, 2, 2, 2, 2, 2, 2, 2, 2, 2, 2, 2, 2, 2, 2, 2, 2, 2, 2, 2, 2, 2, 2, 2, 2, 2, 2, 2, 2, 2, 2, 2, 2, 2, 2, 2, 2, 2, 2, 2, 2, 2, 2, 2, 2, 2, 2, 2, 2, 2, 2, 2, 2, 2, 2, 2, 2, 2, 2, 2, 2, 2, 2, 2, 2, 2, 2, 2, 2, 2, 2, 2, 2, 2, 2, 2, 2, 2, 2, 2, 2, 2, 2, 2, 2, 2, 2, 2, 2, 2, 2, 2, 2, 2, 2, 2, 2, 2, 2, 2, 2, 2, 2, 2, 2, 2, 2, 2, 2, 2, 2, 2, 2, 2, 2, 2, 2, 2, 2, 2, 2, 2, 2, 2, 2, 2, 2, 2, 2, 2, 2, 2, 2, 2, 2, 2, 2, 2, 2, 2, 2, 2, 2, 2, 2, 2, 2, 2, 2, 2, 2, 2, 2, 2, 2, 2, 2, 2, 2, 2, 2, 2, 2, 2, 2, 2, 2, 2, 2, 2, 3 ),
 ( 0.000000000000000000, 1.000000000000000000 ),
 ( 0.000000000000000000, 0.003787878787878787984, 0.007575757575757575968, 0.01136363636363636395, 0.01515151515151515194, 0.01893939393939393992, 0.02272727272727272790, 0.02651515151515151589, 0.03030303030303030387, 0.03409090909090908839, 0.03787878787878787984, 0.04166666666666666435, 0.04545454545454545581, 0.04924242424242424032, 0.05303030303030303177, 0.05681818181818181629, 0.06060606060606060774, 0.06439393939393939226, 0.06818181818181817677, 0.07196969696969697516, 0.07575757575757575968, 0.07954545454545454419, 0.08333333333333332871, 0.08712121212121212710, 0.09090909090909091161, 0.09469696969696969613, 0.09848484848484848064, 0.1022727272727272790, 0.1060606060606060635, 0.1098484848484848481, 0.1136363636363636326, 0.1174242424242424310, 0.1212121212121212155, 0.1250000000000000000, 0.1287878787878787845, 0.1325757575757575690, 0.1363636363636363535, 0.1401515151515151381, 0.1439393939393939503, 0.1477272727272727348, 0.1515151515151515194, 0.1553030303030303039, 0.1590909090909090884, 0.1628787878787878729, 0.1666666666666666574, 0.1704545454545454419, 0.1742424242424242542, 0.1780303030303030387, 0.1818181818181818232, 0.1856060606060606077, 0.1893939393939393923, 0.1931818181818181768, 0.1969696969696969613, 0.2007575757575757458, 0.2045454545454545581, 0.2083333333333333426, 0.2121212121212121271, 0.2159090909090909116, 0.2196969696969696961, 0.2234848484848484806, 0.2272727272727272652, 0.2310606060606060497, 0.2348484848484848619, 0.2386363636363636465, 0.2424242424242424310, 0.2462121212121212155, 0.2500000000000000000, 0.2537878787878787845, 0.2575757575757575690, 0.2613636363636363535, 0.2651515151515151381, 0.2689393939393939226, 0.2727272727272727071, 0.2765151515151514916, 0.2803030303030302761, 0.2840909090909091161, 0.2878787878787879007, 0.2916666666666666852, 0.2954545454545454697, 0.2992424242424242542, 0.3030303030303030387, 0.3068181818181818232, 0.3106060606060606077, 0.3143939393939393923, 0.3181818181818181768, 0.3219696969696969613, 0.3257575757575757458, 0.3295454545454545303, 0.3333333333333333148, 0.3371212121212120993, 0.3409090909090908839, 0.3446969696969697239, 0.3484848484848485084, 0.3522727272727272929, 0.3560606060606060774, 0.3598484848484848619, 0.3636363636363636465, 0.3674242424242424310, 0.3712121212121212155, 0.3750000000000000000, 0.3787878787878787845, 0.3825757575757575690, 0.3863636363636363535, 0.3901515151515151381, 0.3939393939393939226, 0.3977272727272727071, 0.4015151515151514916, 0.4053030303030302761, 0.4090909090909091161, 0.4128787878787879007, 0.4166666666666666852, 0.4204545454545454697, 0.4242424242424242542, 0.4280303030303030387, 0.4318181818181818232, 0.4356060606060606077, 0.4393939393939393923, 0.4431818181818181768, 0.4469696969696969613, 0.4507575757575757458, 0.4545454545454545303, 0.4583333333333333148, 0.4621212121212120993, 0.4659090909090908839, 0.4696969696969697239, 0.4734848484848485084, 0.4772727272727272929, 0.4810606060606060774, 0.4848484848484848619, 0.4886363636363636465, 0.4924242424242424310, 0.4962121212121212155, 0.5000000000000000000, 0.5037878787878787845, 0.5075757575757575690, 0.5113636363636363535, 0.5151515151515151381, 0.5189393939393939226, 0.5227272727272727071, 0.5265151515151514916, 0.5303030303030302761, 0.5340909090909090606, 0.5378787878787878451, 0.5416666666666666297, 0.5454545454545454142, 0.5492424242424241987, 0.5530303030303029832, 0.5568181818181817677, 0.5606060606060605522, 0.5643939393939394478, 0.5681818181818182323, 0.5719696969696970168, 0.5757575757575758013, 0.5795454545454545858, 0.5833333333333333703, 0.5871212121212121549, 0.5909090909090909394, 0.5946969696969697239, 0.5984848484848485084, 0.6022727272727272929, 0.6060606060606060774, 0.6098484848484848619, 0.6136363636363636465, 0.6174242424242424310, 0.6212121212121212155, 0.6250000000000000000, 0.6287878787878787845, 0.6325757575757575690, 0.6363636363636363535, 0.6401515151515151381, 0.6439393939393939226, 0.6477272727272727071, 0.6515151515151514916, 0.6553030303030302761, 0.6590909090909090606, 0.6628787878787878451, 0.6666666666666666297, 0.6704545454545454142, 0.6742424242424241987, 0.6780303030303029832, 0.6818181818181817677, 0.6856060606060605522, 0.6893939393939394478, 0.6931818181818182323, 0.6969696969696970168, 0.7007575757575758013, 0.7045454545454545858, 0.7083333333333333703, 0.7121212121212121549, 0.7159090909090909394, 0.7196969696969697239, 0.7234848484848485084, 0.7272727272727272929, 0.7310606060606060774, 0.7348484848484848619, 0.7386363636363636465, 0.7424242424242424310, 0.7462121212121212155, 0.7500000000000000000, 0.7537878787878787845, 0.7575757575757575690, 0.7613636363636363535, 0.7651515151515151381, 0.7689393939393939226, 0.7727272727272727071, 0.7765151515151514916, 0.7803030303030302761, 0.7840909090909090606, 0.7878787878787878451, 0.7916666666666666297, 0.7954545454545454142, 0.7992424242424241987, 0.8030303030303029832, 0.8068181818181817677, 0.8106060606060605522, 0.8143939393939394478, 0.8181818181818182323, 0.8219696969696970168, 0.8257575757575758013, 0.8295454545454545858, 0.8333333333333333703, 0.8371212121212121549, 0.8409090909090909394, 0.8446969696969697239, 0.8484848484848485084, 0.8522727272727272929, 0.8560606060606060774, 0.8598484848484848619, 0.8636363636363636465, 0.8674242424242424310, 0.8712121212121212155, 0.8750000000000000000, 0.8787878787878787845, 0.8825757575757575690, 0.8863636363636363535, 0.8901515151515151381, 0.8939393939393939226, 0.8977272727272727071, 0.9015151515151514916, 0.9053030303030302761, 0.9090909090909090606, 0.9128787878787878451, 0.9166666666666666297, 0.9204545454545454142, 0.9242424242424241987, 0.9280303030303029832, 0.9318181818181817677, 0.9356060606060605522, 0.9393939393939394478, 0.9431818181818182323, 0.9469696969696970168, 0.9507575757575758013, 0.9545454545454545858, 0.9583333333333333703, 0.9621212121212121549, 0.9659090909090909394 ),
 .UNSPECIFIED. ) 
 GEOMETRIC_REPRESENTATION_ITEM ( )  RATIONAL_B_SPLINE_SURFACE ( (
 ( 1.000000000000000000, 0.9659258262890683122, 1.000000000000000000, 0.9659258262890683122, 1.000000000000000000, 0.9659258262890683122, 1.000000000000000000, 0.9659258262890683122, 1.000000000000000000, 0.9659258262890683122, 1.000000000000000000, 0.9659258262890683122, 1.000000000000000000, 0.9659258262890683122, 1.000000000000000000, 0.9659258262890683122, 1.000000000000000000, 0.9659258262890683122, 1.000000000000000000, 0.9659258262890683122, 1.000000000000000000, 0.9659258262890683122, 1.000000000000000000, 0.9659258262890683122, 1.000000000000000000, 0.9659258262890683122, 1.000000000000000000, 0.9659258262890683122, 1.000000000000000000, 0.9659258262890683122, 1.000000000000000000, 0.9659258262890683122, 1.000000000000000000, 0.9659258262890683122, 1.000000000000000000, 0.9659258262890683122, 1.000000000000000000, 0.9659258262890683122, 1.000000000000000000, 0.9659258262890683122, 1.000000000000000000, 0.9659258262890683122, 1.000000000000000000, 0.9659258262890683122, 1.000000000000000000, 0.9659258262890683122, 1.000000000000000000, 0.9659258262890683122, 1.000000000000000000, 0.9659258262890683122, 1.000000000000000000, 0.9659258262890683122, 1.000000000000000000, 0.9659258262890683122, 1.000000000000000000, 0.9659258262890683122, 1.000000000000000000, 0.9659258262890683122, 1.000000000000000000, 0.9659258262890683122, 1.000000000000000000, 0.9659258262890683122, 1.000000000000000000, 0.9659258262890683122, 1.000000000000000000, 0.9659258262890683122, 1.000000000000000000, 0.9659258262890683122, 1.000000000000000000, 0.9659258262890683122, 1.000000000000000000, 0.9659258262890683122, 1.000000000000000000, 0.9659258262890683122, 1.000000000000000000, 0.9659258262890683122, 1.000000000000000000, 0.9659258262890683122, 1.000000000000000000, 0.9659258262890683122, 1.000000000000000000, 0.9659258262890683122, 1.000000000000000000, 0.9659258262890683122, 1.000000000000000000, 0.9659258262890683122, 1.000000000000000000, 0.9659258262890683122, 1.000000000000000000, 0.9659258262890683122, 1.000000000000000000, 0.9659258262890683122, 1.000000000000000000, 0.9659258262890683122, 1.000000000000000000, 0.9659258262890683122, 1.000000000000000000, 0.9659258262890683122, 1.000000000000000000, 0.9659258262890683122, 1.000000000000000000, 0.9659258262890683122, 1.000000000000000000, 0.9659258262890683122, 1.000000000000000000, 0.9659258262890683122, 1.000000000000000000, 0.9659258262890683122, 1.000000000000000000, 0.9659258262890683122, 1.000000000000000000, 0.9659258262890683122, 1.000000000000000000, 0.9659258262890683122, 1.000000000000000000, 0.9659258262890683122, 1.000000000000000000, 0.9659258262890683122, 1.000000000000000000, 0.9659258262890683122, 1.000000000000000000, 0.9659258262890683122, 1.000000000000000000, 0.9659258262890683122, 1.000000000000000000, 0.9659258262890683122, 1.000000000000000000, 0.9659258262890683122, 1.000000000000000000, 0.9659258262890683122, 1.000000000000000000, 0.9659258262890683122, 1.000000000000000000, 0.9659258262890683122, 1.000000000000000000, 0.9659258262890683122, 1.000000000000000000, 0.9659258262890683122, 1.000000000000000000, 0.9659258262890683122, 1.000000000000000000, 0.9659258262890683122, 1.000000000000000000, 0.9659258262890683122, 1.000000000000000000, 0.9659258262890683122, 1.000000000000000000, 0.9659258262890683122, 1.000000000000000000, 0.9659258262890683122, 1.000000000000000000, 0.9659258262890683122, 1.000000000000000000, 0.9659258262890683122, 1.000000000000000000, 0.9659258262890683122, 1.000000000000000000, 0.9659258262890683122, 1.000000000000000000, 0.9659258262890683122, 1.000000000000000000, 0.9659258262890683122, 1.000000000000000000, 0.9659258262890683122, 1.000000000000000000, 0.9659258262890683122, 1.000000000000000000, 0.9659258262890683122, 1.000000000000000000, 0.9659258262890683122, 1.000000000000000000, 0.9659258262890683122, 1.000000000000000000, 0.9659258262890683122, 1.000000000000000000, 0.9659258262890683122, 1.000000000000000000, 0.9659258262890683122, 1.000000000000000000, 0.9659258262890683122, 1.000000000000000000, 0.9659258262890683122, 1.000000000000000000, 0.9659258262890683122, 1.000000000000000000, 0.9659258262890683122, 1.000000000000000000, 0.9659258262890683122, 1.000000000000000000, 0.9659258262890683122, 1.000000000000000000, 0.9659258262890683122, 1.000000000000000000, 0.9659258262890683122, 1.000000000000000000, 0.9659258262890683122, 1.000000000000000000, 0.9659258262890683122, 1.000000000000000000, 0.9659258262890683122, 1.000000000000000000, 0.9659258262890683122, 1.000000000000000000, 0.9659258262890683122, 1.000000000000000000, 0.9659258262890683122, 1.000000000000000000, 0.9659258262890683122, 1.000000000000000000, 0.9659258262890683122, 1.000000000000000000, 0.9659258262890683122, 1.000000000000000000, 0.9659258262890683122, 1.000000000000000000, 0.9659258262890683122, 1.000000000000000000, 0.9659258262890683122, 1.000000000000000000, 0.9659258262890683122, 1.000000000000000000, 0.9659258262890683122, 1.000000000000000000, 0.9659258262890683122, 1.000000000000000000, 0.9659258262890683122, 1.000000000000000000, 0.9659258262890683122, 1.000000000000000000, 0.9659258262890683122, 1.000000000000000000, 0.9659258262890683122, 1.000000000000000000, 0.9659258262890683122, 1.000000000000000000, 0.9659258262890683122, 1.000000000000000000, 0.9659258262890683122, 1.000000000000000000, 0.9659258262890683122, 1.000000000000000000, 0.9659258262890683122, 1.000000000000000000, 0.9659258262890683122, 1.000000000000000000, 0.9659258262890683122, 1.000000000000000000, 0.9659258262890683122, 1.000000000000000000, 0.9659258262890683122, 1.000000000000000000, 0.9659258262890683122, 1.000000000000000000, 0.9659258262890683122, 1.000000000000000000, 0.9659258262890683122, 1.000000000000000000, 0.9659258262890683122, 1.000000000000000000, 0.9659258262890683122, 1.000000000000000000, 0.9659258262890683122, 1.000000000000000000, 0.9659258262890683122, 1.000000000000000000, 0.9659258262890683122, 1.000000000000000000, 0.9659258262890683122, 1.000000000000000000, 0.9659258262890683122, 1.000000000000000000, 0.9659258262890683122, 1.000000000000000000, 0.9659258262890683122, 1.000000000000000000, 0.9659258262890683122, 1.000000000000000000, 0.9659258262890683122, 1.000000000000000000, 0.9659258262890683122, 1.000000000000000000, 0.9659258262890683122, 1.000000000000000000, 0.9659258262890683122, 1.000000000000000000, 0.9659258262890683122, 1.000000000000000000, 0.9659258262890683122, 1.000000000000000000, 0.9659258262890683122, 1.000000000000000000, 0.9659258262890683122, 1.000000000000000000, 0.9659258262890683122, 1.000000000000000000, 0.9659258262890683122, 1.000000000000000000, 0.9659258262890683122, 1.000000000000000000, 0.9659258262890683122, 1.000000000000000000, 0.9659258262890683122, 1.000000000000000000, 0.9659258262890683122, 1.000000000000000000, 0.9659258262890683122, 1.000000000000000000, 0.9659258262890683122, 1.000000000000000000, 0.9659258262890683122, 1.000000000000000000, 0.9659258262890683122, 1.000000000000000000, 0.9659258262890683122, 1.000000000000000000, 0.9659258262890683122, 1.000000000000000000, 0.9659258262890683122, 1.000000000000000000, 0.9659258262890683122, 1.000000000000000000, 0.9659258262890683122, 1.000000000000000000, 0.9659258262890683122, 1.000000000000000000, 0.9659258262890683122, 1.000000000000000000, 0.9659258262890683122, 1.000000000000000000, 0.9659258262890683122, 1.000000000000000000, 0.9659258262890683122, 1.000000000000000000, 0.9659258262890683122, 1.000000000000000000, 0.9659258262890683122, 1.000000000000000000, 0.9659258262890683122, 1.000000000000000000, 0.9659258262890683122, 1.000000000000000000, 0.9659258262890683122, 1.000000000000000000, 0.9659258262890683122, 1.000000000000000000, 0.9659258262890683122, 1.000000000000000000, 0.9659258262890683122, 1.000000000000000000, 0.9659258262890683122, 1.000000000000000000, 0.9659258262890683122, 1.000000000000000000, 0.9659258262890683122, 1.000000000000000000, 0.9659258262890683122, 1.000000000000000000, 0.9659258262890683122, 1.000000000000000000, 0.9659258262890683122, 1.000000000000000000, 0.9659258262890683122, 1.000000000000000000, 0.9659258262890683122, 1.000000000000000000, 0.9659258262890683122, 1.000000000000000000, 0.9659258262890683122, 1.000000000000000000, 0.9659258262890683122, 1.000000000000000000, 0.9659258262890683122, 1.000000000000000000, 0.9659258262890683122, 1.000000000000000000, 0.9659258262890683122, 1.000000000000000000, 0.9659258262890683122, 1.000000000000000000, 0.9659258262890683122, 1.000000000000000000, 0.9659258262890683122, 1.000000000000000000, 0.9659258262890683122, 1.000000000000000000, 0.9659258262890683122, 1.000000000000000000, 0.9659258262890683122, 1.000000000000000000, 0.9659258262890683122, 1.000000000000000000, 0.9659258262890683122, 1.000000000000000000, 0.9659258262890683122, 1.000000000000000000, 0.9659258262890683122, 1.000000000000000000, 0.9659258262890683122, 1.000000000000000000, 0.9659258262890683122, 1.000000000000000000, 0.9659258262890683122, 1.000000000000000000, 0.9659258262890683122, 1.000000000000000000, 0.9659258262890683122, 1.000000000000000000, 0.9659258262890683122, 1.000000000000000000, 0.9659258262890683122, 1.000000000000000000, 0.9659258262890683122, 1.000000000000000000, 0.9659258262890683122, 1.000000000000000000, 0.9659258262890683122, 1.000000000000000000, 0.9659258262890683122, 1.000000000000000000, 0.9659258262890683122, 1.000000000000000000, 0.9659258262890683122, 1.000000000000000000, 0.9659258262890683122, 1.000000000000000000, 0.9659258262890683122, 1.000000000000000000, 0.9659258262890683122, 1.000000000000000000, 0.9659258262890683122, 1.000000000000000000, 0.9659258262890683122, 1.000000000000000000, 0.9659258262890683122, 1.000000000000000000, 0.9659258262890683122, 1.000000000000000000, 0.9659258262890683122, 1.000000000000000000, 0.9659258262890683122, 1.000000000000000000, 0.9659258262890683122, 1.000000000000000000, 0.9659258262890683122, 1.000000000000000000, 0.9659258262890683122, 1.000000000000000000, 0.9659258262890683122, 1.000000000000000000, 0.9659258262890683122, 1.000000000000000000, 0.9659258262890683122, 1.000000000000000000, 0.9659258262890683122, 1.000000000000000000, 0.9659258262890683122, 1.000000000000000000, 0.9659258262890683122, 1.000000000000000000, 0.9659258262890683122, 1.000000000000000000, 0.9659258262890683122, 1.000000000000000000, 0.9659258262890683122, 1.000000000000000000, 0.9659258262890683122, 1.000000000000000000, 0.9659258262890683122, 1.000000000000000000, 0.9659258262890683122, 1.000000000000000000, 0.9659258262890683122, 1.000000000000000000, 0.9659258262890683122, 1.000000000000000000, 0.9659258262890683122, 1.000000000000000000, 0.9659258262890683122, 1.000000000000000000, 0.9659258262890683122, 1.000000000000000000, 0.9659258262890683122, 1.000000000000000000, 0.9659258262890683122, 1.000000000000000000, 0.9659258262890683122, 1.000000000000000000, 0.9659258262890683122, 1.000000000000000000, 0.9659258262890683122, 1.000000000000000000, 0.9659258262890683122, 1.000000000000000000, 0.9659258262890683122, 1.000000000000000000, 0.9659258262890683122, 1.000000000000000000, 0.9659258262890683122, 1.000000000000000000, 0.9659258262890683122, 1.000000000000000000, 0.9659258262890683122, 1.000000000000000000, 0.9659258262890683122, 1.000000000000000000, 0.9659258262890683122, 1.000000000000000000, 0.9659258262890683122, 1.000000000000000000, 0.9659258262890683122, 1.000000000000000000),
 ( 1.000000000000000000, 0.9659258262890683122, 1.000000000000000000, 0.9659258262890683122, 1.000000000000000000, 0.9659258262890683122, 1.000000000000000000, 0.9659258262890683122, 1.000000000000000000, 0.9659258262890683122, 1.000000000000000000, 0.9659258262890683122, 1.000000000000000000, 0.9659258262890683122, 1.000000000000000000, 0.9659258262890683122, 1.000000000000000000, 0.9659258262890683122, 1.000000000000000000, 0.9659258262890683122, 1.000000000000000000, 0.9659258262890683122, 1.000000000000000000, 0.9659258262890683122, 1.000000000000000000, 0.9659258262890683122, 1.000000000000000000, 0.9659258262890683122, 1.000000000000000000, 0.9659258262890683122, 1.000000000000000000, 0.9659258262890683122, 1.000000000000000000, 0.9659258262890683122, 1.000000000000000000, 0.9659258262890683122, 1.000000000000000000, 0.9659258262890683122, 1.000000000000000000, 0.9659258262890683122, 1.000000000000000000, 0.9659258262890683122, 1.000000000000000000, 0.9659258262890683122, 1.000000000000000000, 0.9659258262890683122, 1.000000000000000000, 0.9659258262890683122, 1.000000000000000000, 0.9659258262890683122, 1.000000000000000000, 0.9659258262890683122, 1.000000000000000000, 0.9659258262890683122, 1.000000000000000000, 0.9659258262890683122, 1.000000000000000000, 0.9659258262890683122, 1.000000000000000000, 0.9659258262890683122, 1.000000000000000000, 0.9659258262890683122, 1.000000000000000000, 0.9659258262890683122, 1.000000000000000000, 0.9659258262890683122, 1.000000000000000000, 0.9659258262890683122, 1.000000000000000000, 0.9659258262890683122, 1.000000000000000000, 0.9659258262890683122, 1.000000000000000000, 0.9659258262890683122, 1.000000000000000000, 0.9659258262890683122, 1.000000000000000000, 0.9659258262890683122, 1.000000000000000000, 0.9659258262890683122, 1.000000000000000000, 0.9659258262890683122, 1.000000000000000000, 0.9659258262890683122, 1.000000000000000000, 0.9659258262890683122, 1.000000000000000000, 0.9659258262890683122, 1.000000000000000000, 0.9659258262890683122, 1.000000000000000000, 0.9659258262890683122, 1.000000000000000000, 0.9659258262890683122, 1.000000000000000000, 0.9659258262890683122, 1.000000000000000000, 0.9659258262890683122, 1.000000000000000000, 0.9659258262890683122, 1.000000000000000000, 0.9659258262890683122, 1.000000000000000000, 0.9659258262890683122, 1.000000000000000000, 0.9659258262890683122, 1.000000000000000000, 0.9659258262890683122, 1.000000000000000000, 0.9659258262890683122, 1.000000000000000000, 0.9659258262890683122, 1.000000000000000000, 0.9659258262890683122, 1.000000000000000000, 0.9659258262890683122, 1.000000000000000000, 0.9659258262890683122, 1.000000000000000000, 0.9659258262890683122, 1.000000000000000000, 0.9659258262890683122, 1.000000000000000000, 0.9659258262890683122, 1.000000000000000000, 0.9659258262890683122, 1.000000000000000000, 0.9659258262890683122, 1.000000000000000000, 0.9659258262890683122, 1.000000000000000000, 0.9659258262890683122, 1.000000000000000000, 0.9659258262890683122, 1.000000000000000000, 0.9659258262890683122, 1.000000000000000000, 0.9659258262890683122, 1.000000000000000000, 0.9659258262890683122, 1.000000000000000000, 0.9659258262890683122, 1.000000000000000000, 0.9659258262890683122, 1.000000000000000000, 0.9659258262890683122, 1.000000000000000000, 0.9659258262890683122, 1.000000000000000000, 0.9659258262890683122, 1.000000000000000000, 0.9659258262890683122, 1.000000000000000000, 0.9659258262890683122, 1.000000000000000000, 0.9659258262890683122, 1.000000000000000000, 0.9659258262890683122, 1.000000000000000000, 0.9659258262890683122, 1.000000000000000000, 0.9659258262890683122, 1.000000000000000000, 0.9659258262890683122, 1.000000000000000000, 0.9659258262890683122, 1.000000000000000000, 0.9659258262890683122, 1.000000000000000000, 0.9659258262890683122, 1.000000000000000000, 0.9659258262890683122, 1.000000000000000000, 0.9659258262890683122, 1.000000000000000000, 0.9659258262890683122, 1.000000000000000000, 0.9659258262890683122, 1.000000000000000000, 0.9659258262890683122, 1.000000000000000000, 0.9659258262890683122, 1.000000000000000000, 0.9659258262890683122, 1.000000000000000000, 0.9659258262890683122, 1.000000000000000000, 0.9659258262890683122, 1.000000000000000000, 0.9659258262890683122, 1.000000000000000000, 0.9659258262890683122, 1.000000000000000000, 0.9659258262890683122, 1.000000000000000000, 0.9659258262890683122, 1.000000000000000000, 0.9659258262890683122, 1.000000000000000000, 0.9659258262890683122, 1.000000000000000000, 0.9659258262890683122, 1.000000000000000000, 0.9659258262890683122, 1.000000000000000000, 0.9659258262890683122, 1.000000000000000000, 0.9659258262890683122, 1.000000000000000000, 0.9659258262890683122, 1.000000000000000000, 0.9659258262890683122, 1.000000000000000000, 0.9659258262890683122, 1.000000000000000000, 0.9659258262890683122, 1.000000000000000000, 0.9659258262890683122, 1.000000000000000000, 0.9659258262890683122, 1.000000000000000000, 0.9659258262890683122, 1.000000000000000000, 0.9659258262890683122, 1.000000000000000000, 0.9659258262890683122, 1.000000000000000000, 0.9659258262890683122, 1.000000000000000000, 0.9659258262890683122, 1.000000000000000000, 0.9659258262890683122, 1.000000000000000000, 0.9659258262890683122, 1.000000000000000000, 0.9659258262890683122, 1.000000000000000000, 0.9659258262890683122, 1.000000000000000000, 0.9659258262890683122, 1.000000000000000000, 0.9659258262890683122, 1.000000000000000000, 0.9659258262890683122, 1.000000000000000000, 0.9659258262890683122, 1.000000000000000000, 0.9659258262890683122, 1.000000000000000000, 0.9659258262890683122, 1.000000000000000000, 0.9659258262890683122, 1.000000000000000000, 0.9659258262890683122, 1.000000000000000000, 0.9659258262890683122, 1.000000000000000000, 0.9659258262890683122, 1.000000000000000000, 0.9659258262890683122, 1.000000000000000000, 0.9659258262890683122, 1.000000000000000000, 0.9659258262890683122, 1.000000000000000000, 0.9659258262890683122, 1.000000000000000000, 0.9659258262890683122, 1.000000000000000000, 0.9659258262890683122, 1.000000000000000000, 0.9659258262890683122, 1.000000000000000000, 0.9659258262890683122, 1.000000000000000000, 0.9659258262890683122, 1.000000000000000000, 0.9659258262890683122, 1.000000000000000000, 0.9659258262890683122, 1.000000000000000000, 0.9659258262890683122, 1.000000000000000000, 0.9659258262890683122, 1.000000000000000000, 0.9659258262890683122, 1.000000000000000000, 0.9659258262890683122, 1.000000000000000000, 0.9659258262890683122, 1.000000000000000000, 0.9659258262890683122, 1.000000000000000000, 0.9659258262890683122, 1.000000000000000000, 0.9659258262890683122, 1.000000000000000000, 0.9659258262890683122, 1.000000000000000000, 0.9659258262890683122, 1.000000000000000000, 0.9659258262890683122, 1.000000000000000000, 0.9659258262890683122, 1.000000000000000000, 0.9659258262890683122, 1.000000000000000000, 0.9659258262890683122, 1.000000000000000000, 0.9659258262890683122, 1.000000000000000000, 0.9659258262890683122, 1.000000000000000000, 0.9659258262890683122, 1.000000000000000000, 0.9659258262890683122, 1.000000000000000000, 0.9659258262890683122, 1.000000000000000000, 0.9659258262890683122, 1.000000000000000000, 0.9659258262890683122, 1.000000000000000000, 0.9659258262890683122, 1.000000000000000000, 0.9659258262890683122, 1.000000000000000000, 0.9659258262890683122, 1.000000000000000000, 0.9659258262890683122, 1.000000000000000000, 0.9659258262890683122, 1.000000000000000000, 0.9659258262890683122, 1.000000000000000000, 0.9659258262890683122, 1.000000000000000000, 0.9659258262890683122, 1.000000000000000000, 0.9659258262890683122, 1.000000000000000000, 0.9659258262890683122, 1.000000000000000000, 0.9659258262890683122, 1.000000000000000000, 0.9659258262890683122, 1.000000000000000000, 0.9659258262890683122, 1.000000000000000000, 0.9659258262890683122, 1.000000000000000000, 0.9659258262890683122, 1.000000000000000000, 0.9659258262890683122, 1.000000000000000000, 0.9659258262890683122, 1.000000000000000000, 0.9659258262890683122, 1.000000000000000000, 0.9659258262890683122, 1.000000000000000000, 0.9659258262890683122, 1.000000000000000000, 0.9659258262890683122, 1.000000000000000000, 0.9659258262890683122, 1.000000000000000000, 0.9659258262890683122, 1.000000000000000000, 0.9659258262890683122, 1.000000000000000000, 0.9659258262890683122, 1.000000000000000000, 0.9659258262890683122, 1.000000000000000000, 0.9659258262890683122, 1.000000000000000000, 0.9659258262890683122, 1.000000000000000000, 0.9659258262890683122, 1.000000000000000000, 0.9659258262890683122, 1.000000000000000000, 0.9659258262890683122, 1.000000000000000000, 0.9659258262890683122, 1.000000000000000000, 0.9659258262890683122, 1.000000000000000000, 0.9659258262890683122, 1.000000000000000000, 0.9659258262890683122, 1.000000000000000000, 0.9659258262890683122, 1.000000000000000000, 0.9659258262890683122, 1.000000000000000000, 0.9659258262890683122, 1.000000000000000000, 0.9659258262890683122, 1.000000000000000000, 0.9659258262890683122, 1.000000000000000000, 0.9659258262890683122, 1.000000000000000000, 0.9659258262890683122, 1.000000000000000000, 0.9659258262890683122, 1.000000000000000000, 0.9659258262890683122, 1.000000000000000000, 0.9659258262890683122, 1.000000000000000000, 0.9659258262890683122, 1.000000000000000000, 0.9659258262890683122, 1.000000000000000000, 0.9659258262890683122, 1.000000000000000000, 0.9659258262890683122, 1.000000000000000000, 0.9659258262890683122, 1.000000000000000000, 0.9659258262890683122, 1.000000000000000000, 0.9659258262890683122, 1.000000000000000000, 0.9659258262890683122, 1.000000000000000000, 0.9659258262890683122, 1.000000000000000000, 0.9659258262890683122, 1.000000000000000000, 0.9659258262890683122, 1.000000000000000000, 0.9659258262890683122, 1.000000000000000000, 0.9659258262890683122, 1.000000000000000000, 0.9659258262890683122, 1.000000000000000000, 0.9659258262890683122, 1.000000000000000000, 0.9659258262890683122, 1.000000000000000000, 0.9659258262890683122, 1.000000000000000000, 0.9659258262890683122, 1.000000000000000000, 0.9659258262890683122, 1.000000000000000000, 0.9659258262890683122, 1.000000000000000000, 0.9659258262890683122, 1.000000000000000000, 0.9659258262890683122, 1.000000000000000000, 0.9659258262890683122, 1.000000000000000000, 0.9659258262890683122, 1.000000000000000000, 0.9659258262890683122, 1.000000000000000000, 0.9659258262890683122, 1.000000000000000000, 0.9659258262890683122, 1.000000000000000000, 0.9659258262890683122, 1.000000000000000000, 0.9659258262890683122, 1.000000000000000000, 0.9659258262890683122, 1.000000000000000000, 0.9659258262890683122, 1.000000000000000000, 0.9659258262890683122, 1.000000000000000000, 0.9659258262890683122, 1.000000000000000000, 0.9659258262890683122, 1.000000000000000000, 0.9659258262890683122, 1.000000000000000000, 0.9659258262890683122, 1.000000000000000000, 0.9659258262890683122, 1.000000000000000000, 0.9659258262890683122, 1.000000000000000000, 0.9659258262890683122, 1.000000000000000000, 0.9659258262890683122, 1.000000000000000000, 0.9659258262890683122, 1.000000000000000000, 0.9659258262890683122, 1.000000000000000000, 0.9659258262890683122, 1.000000000000000000, 0.9659258262890683122, 1.000000000000000000, 0.9659258262890683122, 1.000000000000000000, 0.9659258262890683122, 1.000000000000000000, 0.9659258262890683122, 1.000000000000000000, 0.9659258262890683122, 1.000000000000000000, 0.9659258262890683122, 1.000000000000000000) ) ) 
 REPRESENTATION_ITEM ( '' )  SURFACE ( )  );
#3072 = CARTESIAN_POINT ( 'NONE',  ( -0.4724409448818898682, -8.678599364036362592E-17, 0.1181102362204724532 ) ) ;
#3073 = CARTESIAN_POINT ( 'NONE',  ( 0.2891555358219910499, -0.2891555358219909944, -2.460629921259842590 ) ) ;
#3074 = ORIENTED_EDGE ( 'NONE', *, *, #76299, .F. ) ;
#3075 = CARTESIAN_POINT ( 'NONE',  ( 0.6364829396325465405, -0.2845877964562161244, -0.3641732283464567121 ) ) ;
#3077 = CARTESIAN_POINT ( 'NONE',  ( -0.1049643490035302024, -0.3917322834645671215, -1.166666666666666519 ) ) ;
#3076 = AXIS2_PLACEMENT_3D ( 'NONE', #17291, #17694, #10954 ) ;
#3078 = ADVANCED_FACE ( 'NONE', ( #35438 ), #1646, .F. ) ;
#3079 = CARTESIAN_POINT ( 'NONE',  ( 1.266404199475066328, -0.05778040916215522460, 0.4822834645669289988 ) ) ;
#3080 = LINE ( 'NONE', #79283, #82937 ) ;
#3081 = CARTESIAN_POINT ( 'NONE',  ( -1.227034120734907585, 0.1771653543307087630, 0.09757992244046791164 ) ) ;
#3082 = CARTESIAN_POINT ( 'NONE',  ( 1.535433070866142558, 0.2952755905511811885, 0.000000000000000000 ) ) ;
#3083 = CARTESIAN_POINT ( 'NONE',  ( -1.410761154855642463, -0.05778040916215522460, 0.4822834645669289988 ) ) ;
#3084 = CARTESIAN_POINT ( 'NONE',  ( 0.2952755905511819101, 0.1660481256975883668, -0.3530559997133364547 ) ) ;
#3085 = CARTESIAN_POINT ( 'NONE',  ( -0.1049643490035301746, -0.3917322834645670659, -0.1522116553467698086 ) ) ;
#3086 = CARTESIAN_POINT ( 'NONE',  ( -0.1837270341207340729, 0.2306618581243847221, -0.2411417322834647770 ) ) ;
#3087 = CARTESIAN_POINT ( 'NONE',  ( -0.8530183727034112984, -0.3690944881889765550, -0.3153832671262227771 ) ) ;
#3088 = CARTESIAN_POINT ( 'NONE',  ( 0.8398950131233602345, 0.2306618581243847221, -0.2411417322834647770 ) ) ;
#3089 = CARTESIAN_POINT ( 'NONE',  ( 5.463695987328526437E-16, -0.1870078740157479769, 0.4822834645669291653 ) ) ;
#3090 = CARTESIAN_POINT ( 'NONE',  ( 0.5395952360118035918, 0.02791078216816508459, -0.4328096321851889194 ) ) ;
#3091 = CARTESIAN_POINT ( 'NONE',  ( 0.1998031496062992740, 0.3460692066303959757, -2.821522309711286258 ) ) ;
#3092 = CARTESIAN_POINT ( 'NONE',  ( -0.2867679344610365444, -0.2867679344610367664, -1.630596743603361265 ) ) ;
#3093 = CARTESIAN_POINT ( 'NONE',  ( 0.9842519685039378130, -0.6692913385826771977, 8.415575281601705876E-17 ) ) ;
#3094 = CARTESIAN_POINT ( 'NONE',  ( 0.09186351706036799403, -0.4281496062992127816, -0.4176697321401328100 ) ) ;
#3095 = CARTESIAN_POINT ( 'NONE',  ( -0.9120734908136475250, -0.6692913385826773087, -0.1292274648535924053 ) ) ;
#3096 = CARTESIAN_POINT ( 'NONE',  ( 0.9514435695538062676, -0.05778040916215522460, 0.4822834645669289988 ) ) ;
#3097 = CARTESIAN_POINT ( 'NONE',  ( 1.036745406824147731, 0.05413385826771666132, 0.4176697321401328100 ) ) ;
#3098 = CARTESIAN_POINT ( 'NONE',  ( 0.3392501089628018884, -0.1958661417322834220, -0.8195538057742782767 ) ) ;
#3099 = CARTESIAN_POINT ( 'NONE',  ( -0.4921259842519677963, -0.5400638737290844871, 0.3530559997133364547 ) ) ;
#3100 = CARTESIAN_POINT ( 'NONE',  ( 0.7677165354330716118, 0.1660481256975883668, -0.3530559997133364547 ) ) ;
#3101 = CARTESIAN_POINT ( 'NONE',  ( -0.1377952755905504645, -0.5400638737290845981, -0.3530559997133363437 ) ) ;
#3102 = CARTESIAN_POINT ( 'NONE',  ( 0.8792650918635177559, -0.004921259842519576551, 0.3153832671262227771 ) ) ;
#3103 = CARTESIAN_POINT ( 'NONE',  ( -1.463254593175852492, -0.6692913385826773087, -0.1292274648535924053 ) ) ;
#3104 = CARTESIAN_POINT ( 'NONE',  ( -1.633858267716534529, -0.5400638737290845981, -0.3530559997133363437 ) ) ;
#3105 = CARTESIAN_POINT ( 'NONE',  ( 0.4658792650918640033, -0.3162353388693405765, 0.4822834645669290543 ) ) ;
#3106 =( LENGTH_UNIT ( ) NAMED_UNIT ( * ) SI_UNIT ( $, .METRE. ) );
#3107 = CARTESIAN_POINT ( 'NONE',  ( -9.594673741351313045E-17, 0.3917322834645670104, -2.511811023622047223 ) ) ;
#3108 = ORIENTED_EDGE ( 'NONE', *, *, #19583, .F. ) ;
#3109 = ORIENTED_EDGE ( 'NONE', *, *, #31497, .T. ) ;
#3110 = CARTESIAN_POINT ( 'NONE',  ( 0.9251968503937015864, 0.1660481256975883668, -0.3530559997133364547 ) ) ;
#3111 = CARTESIAN_POINT ( 'NONE',  ( 0.5511811023622054106, -0.1870078740157480601, -0.3641732283464567677 ) ) ;
#3113 = LINE ( 'NONE', #40166, #43760 ) ;
#3112 = CARTESIAN_POINT ( 'NONE',  ( 0.000000000000000000, 0.000000000000000000, -2.755905511811024056 ) ) ;
#3114 = CARTESIAN_POINT ( 'NONE',  ( -0.7478466213799872531, 2.204724409448818978, -0.5309055118110235227 ) ) ;
#3115 = CARTESIAN_POINT ( 'NONE',  ( -0.1958661417322834220, -0.3392501089628018884, -1.095144356955380704 ) ) ;
#3116 = CARTESIAN_POINT ( 'NONE',  ( 0.3460692066303958092, 0.1998031496062993018, -2.412729658792650778 ) ) ;
#3117 = CARTESIAN_POINT ( 'NONE',  ( -0.6430446194225712953, 0.05413385826771626580, -0.4176697321401330321 ) ) ;
#3118 = CIRCLE ( 'NONE', #50133, 0.2952755905511810774 ) ;
#3119 = CARTESIAN_POINT ( 'NONE',  ( -0.5446194225721777693, -0.3162353388693409650, -0.4822834645669289433 ) ) ;
#3120 = CARTESIAN_POINT ( 'NONE',  ( 0.5183727034120741983, 0.2952755905511810774, -0.1292274648535930714 ) ) ;
#3121 = VERTEX_POINT ( 'NONE', #48465 ) ;
#3122 = CARTESIAN_POINT ( 'NONE',  ( 1.305774278215223960, 0.2952755905511810774, -0.1292274648535930714 ) ) ;
#3123 = CARTESIAN_POINT ( 'NONE',  ( 1.213910761154856077, 0.2066929133858248224, 0.1054918080437525219 ) ) ;
#3124 = ITEM_DEFINED_TRANSFORMATION ( 'NONE', 'NONE', #6042,  #22098 ) ;
#3125 = CARTESIAN_POINT ( 'NONE',  ( 1.607611548556431069, -0.5511811023622048555, -0.09757992244046775898 ) ) ;
#3126 = CARTESIAN_POINT ( 'NONE',  ( 0.000000000000000000, 2.165354330708661568, 0.000000000000000000 ) ) ;
#3127 = CARTESIAN_POINT ( 'NONE',  ( -1.482939632545930975, -0.004921259842519576551, 0.3153832671262227771 ) ) ;
#3128 = CARTESIAN_POINT ( 'NONE',  ( 4.797336870675656522E-17, -0.3917322834645670104, 0.08661417322834649712 ) ) ;
#3129 = CARTESIAN_POINT ( 'NONE',  ( 0.03280839895013198948, -0.6692913385826773087, -0.1292274648535924053 ) ) ;
#3131 = CARTESIAN_POINT ( 'NONE',  ( -1.313877454013331780, 0.2755905511811023723, 0.7983292792091805090 ) ) ;
#3130 = CARTESIAN_POINT ( 'NONE',  ( 1.607611548556431069, -0.6692913385826773087, -0.1292274648535924053 ) ) ;
#3132 = B_SPLINE_CURVE_WITH_KNOTS ( 'NONE', 3,
 ( #60581, #66490, #71974, #53835 ),
 .UNSPECIFIED., .F., .F.,
 ( 4, 4 ),
 ( 1.734723475976807094E-18, 0.001434885020664811769 ),
 .UNSPECIFIED. ) ;
#3133 = CARTESIAN_POINT ( 'NONE',  ( -1.240157480314959759, 0.07958543189024085140, 0.2665933059059887866 ) ) ;
#3134 = CARTESIAN_POINT ( 'NONE',  ( 0.8398950131233602345, -0.6046776061558807314, 0.2411417322834647770 ) ) ;
#3135 = CARTESIAN_POINT ( 'NONE',  ( 1.233595800524935227, -0.5023911411419708095, 0.1820866141732285504 ) ) ;
#3136 = CARTESIAN_POINT ( 'NONE',  ( -0.3392501089628019439, 0.1958661417322832554, -1.051161786580365742 ) ) ;
#3137 = CIRCLE ( 'NONE', #71688, 0.09842519685039344268 ) ;
#3138 = CARTESIAN_POINT ( 'NONE',  ( -1.056430446194224881, 0.1771653543307087075, -0.09757992244046823083 ) ) ;
#3139 = CARTESIAN_POINT ( 'NONE',  ( 1.358267716535433323, 0.1660481256975885056, 0.3530559997133364547 ) ) ;
#3140 = CARTESIAN_POINT ( 'NONE',  ( 0.3126275856726307700, 1.620602844568471479, 0.01575678725321194573 ) ) ;
#3141 = CARTESIAN_POINT ( 'NONE',  ( -0.06561679790026180015, -0.4281496062992127816, -0.4176697321401328100 ) ) ;
#3142 = CARTESIAN_POINT ( 'NONE',  ( -1.496062992125983815, -0.1870078740157479769, 0.3641732283464567677 ) ) ;
#3143 = CARTESIAN_POINT ( 'NONE',  ( -0.4461942257217840213, 0.1283753931104748280, 0.1820866141732283561 ) ) ;
#3144 = CARTESIAN_POINT ( 'NONE',  ( -0.2230971128608915943, -0.4281496062992127816, -0.4176697321401328100 ) ) ;
#3145 = CARTESIAN_POINT ( 'NONE',  ( -1.377952755905511140, -0.5511811023622047445, 6.969142054262312111E-17 ) ) ;
#3146 = CARTESIAN_POINT ( 'NONE',  ( 0.3917322834645670104, 0.1049643490035304660, -0.4363710218185846146 ) ) ;
#3147 = CARTESIAN_POINT ( 'NONE',  ( 0.3740157480314966754, 0.1660481256975883668, -0.3530559997133364547 ) ) ;
#3148 = CARTESIAN_POINT ( 'NONE',  ( 0.2362204724409451007, -0.4091458600556402980, -0.2493438320209973857 ) ) ;
#3149 = CARTESIAN_POINT ( 'NONE',  ( 0.4091458600556404646, -0.2362204724409448231, -1.756561679790026309 ) ) ;
#3150 = CARTESIAN_POINT ( 'NONE',  ( -1.095800524934382292, -0.05778040916215522460, 0.4822834645669289988 ) ) ;
#3151 = CARTESIAN_POINT ( 'NONE',  ( -0.4199475065616791736, 0.1283753931104746893, -0.1820866141732285504 ) ) ;
#3152 = CARTESIAN_POINT ( 'NONE',  ( -1.292650918635170010, 0.2952755905511810774, -0.1292274648535930714 ) ) ;
#3153 = CARTESIAN_POINT ( 'NONE',  ( 0.2099737532808405305, -0.6046776061558807314, 0.2411417322834647770 ) ) ;
#3154 = CARTESIAN_POINT ( 'NONE',  ( 0.4265091863517067594, 0.1771653543307087630, 0.09757992244046791164 ) ) ;
#3155 = CARTESIAN_POINT ( 'NONE',  ( -0.7874015748031489847, -0.1870078740157479769, 0.3641732283464567677 ) ) ;
#3156 = CARTESIAN_POINT ( 'NONE',  ( -1.108923884514435132, -0.3162353388693405765, 0.4822834645669290543 ) ) ;
#3157 = CARTESIAN_POINT ( 'NONE',  ( -1.443569553805773564, -0.6046776061558807314, 0.2411417322834647770 ) ) ;
#3158 = CARTESIAN_POINT ( 'NONE',  ( 1.410761154855643795, -0.05778040916215560624, -0.4822834645669293319 ) ) ;
#3159 = DIRECTION ( 'NONE',  ( -3.096699300667737957E-16, 1.000000000000000000, -0.000000000000000000 ) ) ;
#3160 = CARTESIAN_POINT ( 'NONE',  ( 0.6627296587926517768, -0.5511811023622048555, -0.09757992244046775898 ) ) ;
#3161 = CARTESIAN_POINT ( 'NONE',  ( 0.9514435695538062676, -0.3162353388693409650, -0.4822834645669289433 ) ) ;
#3162 = CARTESIAN_POINT ( 'NONE',  ( 0.000000000000000000, 0.000000000000000000, -2.755905511811024056 ) ) ;
#3163 = CARTESIAN_POINT ( 'NONE',  ( 1.489501312335958172, -0.08942795157528024563, -0.3641732283464568787 ) ) ;
#3164 = ORIENTED_EDGE ( 'NONE', *, *, #174, .F. ) ;
#3165 = CARTESIAN_POINT ( 'NONE',  ( -0.7414698162729651543, -0.6692913385826771977, 0.1292274648535927661 ) ) ;
#3166 = CARTESIAN_POINT ( 'NONE',  ( -0.9120734908136475250, -0.6692913385826773087, -0.1292274648535924053 ) ) ;
#3167 = CARTESIAN_POINT ( 'NONE',  ( 0.4199475065616803948, -0.6046776061558809534, -0.2411417322834644161 ) ) ;
#3168 = CARTESIAN_POINT ( 'NONE',  ( -1.574803149606298636, -0.1870078740157479769, 0.3641732283464567677 ) ) ;
#3169 = CARTESIAN_POINT ( 'NONE',  ( -0.1998031496062991630, -0.3460692066303959202, -2.347112860892388575 ) ) ;
#3170 = CARTESIAN_POINT ( 'NONE',  ( -1.325459317585300889, -0.4281496062992127816, -0.4176697321401328100 ) ) ;
#3171 = CARTESIAN_POINT ( 'NONE',  ( 0.2559055118110243332, 0.1660481256975885056, 0.3530559997133364547 ) ) ;
#3172 = CARTESIAN_POINT ( 'NONE',  ( 0.9711286089238851948, 0.2306618581243848609, 0.2411417322834645549 ) ) ;
#3173 = CARTESIAN_POINT ( 'NONE',  ( -1.586052503253847501, 1.299212598425198095, -0.1653254495020571035 ) ) ;
#3174 = CARTESIAN_POINT ( 'NONE',  ( -0.1070741851644051862, -0.3996062992125987146, -1.804461942257217677 ) ) ;
#3175 = CARTESIAN_POINT ( 'NONE',  ( -0.1058382717557503211, 0.3949938075777409408, -1.108923884514435798 ) ) ;
#3176 = CARTESIAN_POINT ( 'NONE',  ( 0.2925321140481932369, -0.2925321140481932369, -2.303149606299212060 ) ) ;
#3177 = CARTESIAN_POINT ( 'NONE',  ( -0.1265901696524993347, 0.4724409448818896462, -0.6364829396325458744 ) ) ;
#3178 = CIRCLE ( 'NONE', #34119, 3.937007874015748143 ) ;
#3179 = CARTESIAN_POINT ( 'NONE',  ( 4.797336870675656522E-17, -0.3917322834645670104, -0.3858267716535432879 ) ) ;
#3180 = CARTESIAN_POINT ( 'NONE',  ( -0.1377952755905504645, 0.07958543189024085140, 0.2665933059059887866 ) ) ;
#3181 = CARTESIAN_POINT ( 'NONE',  ( -0.4986876640419942164, -0.6046776061558807314, 0.2411417322834647770 ) ) ;
#3182 = CARTESIAN_POINT ( 'NONE',  ( 0.7742782152230978099, -0.4281496062992124485, 0.4176697321401328655 ) ) ;
#3183 = CARTESIAN_POINT ( 'NONE',  ( -0.1058382717557497660, -0.3949938075777411073, -2.038713910761155379 ) ) ;
#3184 = CARTESIAN_POINT ( 'NONE',  ( 0.1115485564304470323, 0.1771653543307087630, 0.09757992244046791164 ) ) ;
#3185 = CARTESIAN_POINT ( 'NONE',  ( -1.003937007874014853, 0.1660481256975885056, 0.3530559997133364547 ) ) ;
#3186 = CARTESIAN_POINT ( 'NONE',  ( 1.325459317585302665, 0.05413385826771626580, -0.4176697321401330321 ) ) ;
#3187 = CARTESIAN_POINT ( 'NONE',  ( 0.4091458600556404646, -0.2362204724409448231, -2.624671916010498762 ) ) ;
#3188 = CARTESIAN_POINT ( 'NONE',  ( -0.1070741851644056997, 0.3996062992125986035, -1.896325459317584894 ) ) ;
#3189 = CARTESIAN_POINT ( 'NONE',  ( 1.141732283464567566, 0.2952755905511811885, 0.000000000000000000 ) ) ;
#3190 = ORIENTED_EDGE ( 'NONE', *, *, #52265, .T. ) ;
#3191 = VERTEX_POINT ( 'NONE', #81725 ) ;
#3192 = CARTESIAN_POINT ( 'NONE',  ( 0.8989501312335963501, -0.6692913385826773087, -0.1292274648535924053 ) ) ;
#3193 = CARTESIAN_POINT ( 'NONE',  ( -1.555118110236219930, 0.1660481256975885056, 0.3530559997133364547 ) ) ;
#3195 = CARTESIAN_POINT ( 'NONE',  ( -1.095800524934382292, -0.3162353388693409650, -0.4822834645669289433 ) ) ;
#3194 = CARTESIAN_POINT ( 'NONE',  ( -1.148293963254592542, 0.1771653543307087630, 0.09757992244046791164 ) ) ;
#3196 = CARTESIAN_POINT ( 'NONE',  ( 0.1958661417322836440, -0.3392501089628017219, 0.1384514435695537171 ) ) ;
#3197 = CARTESIAN_POINT ( 'NONE',  ( -0.9711286089238838626, 0.1539470093639521697, -0.1968503937007875793 ) ) ;
#3198 = CARTESIAN_POINT ( 'NONE',  ( 1.351706036745407680, 0.05413385826771666132, 0.4176697321401328100 ) ) ;
#3199 = CARTESIAN_POINT ( 'NONE',  ( 0.4724409448818898127, -0.1265901696524988629, -2.473753280839894764 ) ) ;
#3200 = CARTESIAN_POINT ( 'NONE',  ( -0.2887139107611542133, 0.2306618581243848609, 0.2411417322834645549 ) ) ;
#3201 = CARTESIAN_POINT ( 'NONE',  ( -0.6627296587926503335, -0.6692913385826771977, 0.1292274648535927661 ) ) ;
#3202 = EDGE_CURVE ( 'NONE', #46767, #50394, #10096, .T. ) ;
#3203 = CARTESIAN_POINT ( 'NONE',  ( 1.561679790026247350, -0.4281496062992124485, 0.4176697321401328655 ) ) ;
#3204 = CARTESIAN_POINT ( 'NONE',  ( 0.1958661417322836440, -0.3392501089628017219, -0.01902887139107619849 ) ) ;
#3205 = CARTESIAN_POINT ( 'NONE',  ( 0.3412073490813655186, 0.2306618581243848609, 0.2411417322834645549 ) ) ;
#3206 =( BOUNDED_CURVE ( )  B_SPLINE_CURVE ( 2, ( #2191, #26610, #46370, #33758, #14423, #72481, #52262, #71645, #40074, #65761, #59420, #78806, #21135 ),
 .UNSPECIFIED., .F., .F. ) 
 B_SPLINE_CURVE_WITH_KNOTS ( ( 3, 2, 2, 2, 2, 2, 3 ),
 ( 0.2308514478433235373, 0.2310606060606060774, 0.2348484848484848619, 0.2386363636363636465, 0.2424242424242424310, 0.2462121212121212155, 0.2464212794294037556 ),
 .UNSPECIFIED. ) 
 CURVE ( )  GEOMETRIC_REPRESENTATION_ITEM ( )  RATIONAL_B_SPLINE_CURVE ( ( 0.9964447847208416364, 0.9981185001348089614, 1.000000000000000000, 0.9659258262890683122, 1.000000000000000000, 0.9659258262890683122, 1.000000000000000000, 0.9659258262890683122, 1.000000000000000000, 0.9659258262890683122, 1.000000000000000000, 0.9981185001348089614, 0.9964447847208417475 ) ) 
 REPRESENTATION_ITEM ( '' )  );
#3207 = CARTESIAN_POINT ( 'NONE',  ( -0.3917322834645670104, -7.196005306013484475E-17, -2.236220472440944906 ) ) ;
#3208 = CARTESIAN_POINT ( 'NONE',  ( -1.128608923884513837, 0.1283753931104746893, -0.1820866141732285504 ) ) ;
#3209 = EDGE_LOOP ( 'NONE', ( #41488, #68601, #43311, #7771, #25736, #17193, #15767, #68017 ) ) ;
#3210 = CARTESIAN_POINT ( 'NONE',  ( -0.1058382717557497937, -0.3949938075777411628, -2.119422572178478070 ) ) ;
#3211 = VERTEX_POINT ( 'NONE', #4676 ) ;
#3212 = CARTESIAN_POINT ( 'NONE',  ( -1.576474796205048490, 1.384328893707485131, 0.4490365374974934487 ) ) ;
#3213 = CARTESIAN_POINT ( 'NONE',  ( -1.594488188976377563, -0.5400638737290844871, 0.3530559997133364547 ) ) ;
#3214 = CARTESIAN_POINT ( 'NONE',  ( -0.2925321140481932924, 0.2925321140481931814, -1.122047244094488194 ) ) ;
#3215 = CARTESIAN_POINT ( 'NONE',  ( 1.568241469816273659, -0.08942795157528024563, -0.3641732283464568787 ) ) ;
#3216 = CARTESIAN_POINT ( 'NONE',  ( -1.712598425196849572, 0.1660481256975885056, 0.3530559997133364547 ) ) ;
#3217 = DIRECTION ( 'NONE',  ( -3.096699300667737957E-16, 1.000000000000000000, -0.000000000000000000 ) ) ;
#3218 = CARTESIAN_POINT ( 'NONE',  ( 0.9341826970036752886, -6.978086149529499157E-16, -0.4118477457932994135 ) ) ;
#3219 = CARTESIAN_POINT ( 'NONE',  ( 0.1049643490035304938, -0.3917322834645669549, 0.1450131233595799429 ) ) ;
#3220 = CARTESIAN_POINT ( 'NONE',  ( -0.2427821522309703550, -0.2845877964562159024, 0.3641732283464567677 ) ) ;
#3221 = CARTESIAN_POINT ( 'NONE',  ( -0.8202099737532801971, -0.5511811023622046335, 0.09757992244046803654 ) ) ;
#3222 = CARTESIAN_POINT ( 'NONE',  ( -1.318897637795274802, 0.1660481256975885056, 0.3530559997133364547 ) ) ;
#3223 = CARTESIAN_POINT ( 'NONE',  ( 0.5249343832021003964, 0.2306618581243847221, -0.2411417322834647770 ) ) ;
#3224 = CARTESIAN_POINT ( 'NONE',  ( -1.069553805774277722, -0.6692913385826773087, -0.1292274648535924053 ) ) ;
#3225 = DIRECTION ( 'NONE',  ( -1.000000000000000000, -0.000000000000000000, -0.000000000000000000 ) ) ;
#3226 = EDGE_LOOP ( 'NONE', ( #28969, #55849, #31093, #69712 ) ) ;
#3227 = CARTESIAN_POINT ( 'NONE',  ( -1.194225721784776262, -0.4281496062992124485, 0.4176697321401328655 ) ) ;
#3228 = DIRECTION ( 'NONE',  ( 0.000000000000000000, 0.000000000000000000, 1.000000000000000000 ) ) ;
#3229 = CARTESIAN_POINT ( 'NONE',  ( 0.2362204724409449064, 0.4091458600556404646, -1.876640419947506411 ) ) ;
#3230 = CARTESIAN_POINT ( 'NONE',  ( -1.595398199321656829, 1.034147571970760238, -0.1559797534342476366 ) ) ;
#3231 = ADVANCED_FACE ( 'NONE', ( #37078 ), #31584, .T. ) ;
#3232 = CARTESIAN_POINT ( 'NONE',  ( 0.3917322834645670104, -0.1049643490035303411, -0.7335958005249343383 ) ) ;
#3233 = CARTESIAN_POINT ( 'NONE',  ( 0.4724409448818898682, 2.892866454678787531E-17, -0.9822834645669291653 ) ) ;
#3234 = CARTESIAN_POINT ( 'NONE',  ( -0.6758530183727028406, 0.2952755905511811885, 0.1292274648535926551 ) ) ;
#3235 = CARTESIAN_POINT ( 'NONE',  ( 1.430446194225722500, -0.4281496062992127816, -0.4176697321401328100 ) ) ;
#3237 = CARTESIAN_POINT ( 'NONE',  ( -0.4724409448818898682, 5.785732909357575061E-17, -2.755905511811024056 ) ) ;
#3236 = CARTESIAN_POINT ( 'NONE',  ( -1.712598425196849572, 0.1660481256975885056, 0.3530559997133364547 ) ) ;
#3238 = CARTESIAN_POINT ( 'NONE',  ( -1.384514435695537005, 0.2952755905511811885, 0.1292274648535926551 ) ) ;
#3239 = CARTESIAN_POINT ( 'NONE',  ( -0.8923884514435688198, 0.2306618581243847221, -0.2411417322834647770 ) ) ;
#3240 = CARTESIAN_POINT ( 'NONE',  ( 0.1049643490035303689, 0.3917322834645668994, 0.08400881709417505616 ) ) ;
#3241 = CARTESIAN_POINT ( 'NONE',  ( 0.2887139107611556010, -0.5023911411419708095, 0.1820866141732285504 ) ) ;
#3242 = CARTESIAN_POINT ( 'NONE',  ( 0.1958661417322836440, -0.3392501089628017219, -0.4914698162729659869 ) ) ;
#3243 = AXIS2_PLACEMENT_3D ( 'NONE', #4335, #3934, #28352 ) ;
#3244 = CARTESIAN_POINT ( 'NONE',  ( -0.1115485564304453947, -0.5511811023622046335, 0.09757992244046803654 ) ) ;
#3245 = CARTESIAN_POINT ( 'NONE',  ( 1.056430446194226436, -0.5511811023622048555, -0.09757992244046775898 ) ) ;
#3246 = CARTESIAN_POINT ( 'NONE',  ( 0.9055118110236227702, -0.6692913385826771977, 8.415575281601705876E-17 ) ) ;
#3247 = UNCERTAINTY_MEASURE_WITH_UNIT (LENGTH_MEASURE( 1.000000000000000082E-05 ), #79023, 'distance_accuracy_value', 'NONE');
#3248 = CARTESIAN_POINT ( 'NONE',  ( -0.2690288713910754526, -0.5511811023622046335, 0.09757992244046803654 ) ) ;
#3249 = CARTESIAN_POINT ( 'NONE',  ( 0.2867679344610365999, 0.2867679344610365999, -2.334645669291338432 ) ) ;
#3250 = CARTESIAN_POINT ( 'NONE',  ( 1.391076115485564868, -0.6046776061558807314, 0.2411417322834647770 ) ) ;
#3251 = EDGE_CURVE ( 'NONE', #68517, #7209, #62522, .T. ) ;
#3252 = CARTESIAN_POINT ( 'NONE',  ( -1.397637795275589623, -0.4536011799217368745, -0.2665933059059886201 ) ) ;
#3253 = CARTESIAN_POINT ( 'NONE',  ( 0.4724409448818896462, 0.1265901696524990294, -0.3589238845144357426 ) ) ;
#3254 = CARTESIAN_POINT ( 'NONE',  ( 0.07217847769028949700, -0.3162353388693405765, 0.4822834645669290543 ) ) ;
#3255 = CARTESIAN_POINT ( 'NONE',  ( 1.679790026246720025, 0.1283753931104748280, 0.1820866141732283561 ) ) ;
#3256 = VECTOR ( 'NONE', #49580, 39.37007874015748143 ) ;
#3257 = CARTESIAN_POINT ( 'NONE',  ( 0.6889763779527563470, 0.07958543189024071263, -0.2665933059059888421 ) ) ;
#3258 = CARTESIAN_POINT ( 'NONE',  ( -0.1968503937007867743, -0.5511811023622047445, 6.969142054262312111E-17 ) ) ;
#3259 = CARTESIAN_POINT ( 'NONE',  ( -0.6364829396325453192, -0.05778040916215560624, -0.4822834645669293319 ) ) ;
#3260 = DIRECTION ( 'NONE',  ( 0.000000000000000000, 0.000000000000000000, -1.000000000000000000 ) ) ;
#3261 = CARTESIAN_POINT ( 'NONE',  ( 3.937007874015748143, 2.559055118110236560, 0.3149606299212599492 ) ) ;
#3262 = CARTESIAN_POINT ( 'NONE',  ( -0.006561679790025524116, -0.05778040916215560624, -0.4822834645669293319 ) ) ;
#3263 = CARTESIAN_POINT ( 'NONE',  ( -0.1998031496062991630, -0.3460692066303959202, -1.402230971128609172 ) ) ;
#3264 = DIRECTION ( 'NONE',  ( 1.000000000000000000, 0.000000000000000000, 0.000000000000000000 ) ) ;
#3265 = CARTESIAN_POINT ( 'NONE',  ( -0.09842519685039295696, 0.07958543189024071263, -0.2665933059059888421 ) ) ;
#3266 = CARTESIAN_POINT ( 'NONE',  ( -0.03280839895013062252, -0.6692913385826771977, 0.1292274648535927661 ) ) ;
#3267 = CARTESIAN_POINT ( 'NONE',  ( -1.489501312335957062, -0.05778040916215522460, 0.4822834645669289988 ) ) ;
#3268 = CARTESIAN_POINT ( 'NONE',  ( -1.528871391076114250, -0.5511811023622046335, 0.09757992244046803654 ) ) ;
#3269 = CARTESIAN_POINT ( 'NONE',  ( 1.404199475065617708, 0.05413385826771626580, -0.4176697321401330321 ) ) ;
#3270 = CARTESIAN_POINT ( 'NONE',  ( -1.332020997375327642, -0.05778040916215522460, 0.4822834645669289988 ) ) ;
#3271 = CARTESIAN_POINT ( 'NONE',  ( -0.5839895013123351797, 0.1771653543307087075, -0.09757992244046823083 ) ) ;
#3272 = CARTESIAN_POINT ( 'NONE',  ( -0.3996062992125985480, -7.340648628747423112E-17, -0.2736220472440945017 ) ) ;
#3273 = CARTESIAN_POINT ( 'NONE',  ( -0.1070741851644051862, -0.3996062992125987146, -0.7020997375328084100 ) ) ;
#3274 = CARTESIAN_POINT ( 'NONE',  ( -0.1958661417322836995, 0.3392501089628017219, -2.844507504758217120 ) ) ;
#3275 = CARTESIAN_POINT ( 'NONE',  ( 1.443569553805774897, -0.5023911411419708095, -0.1820866141732282451 ) ) ;
#3276 = CARTESIAN_POINT ( 'NONE',  ( 1.194225721784777594, -0.3690944881889765550, -0.3153832671262227771 ) ) ;
#3277 = CARTESIAN_POINT ( 'NONE',  ( 0.4061203303035133549, 3.421639014772782816E-16, 0.3464511005275203726 ) ) ;
#3278 = CARTESIAN_POINT ( 'NONE',  ( 0.8989501312335963501, -0.6692913385826773087, -0.1292274648535924053 ) ) ;
#3279 = CARTESIAN_POINT ( 'NONE',  ( 4.837279021331061486E-17, -0.3949938075777409963, -0.9429133858267715329 ) ) ;
#3280 = CARTESIAN_POINT ( 'NONE',  ( 1.076115485564305141, 0.1283753931104746893, -0.1820866141732285504 ) ) ;
#3281 = CARTESIAN_POINT ( 'NONE',  ( 0.2427821522309719648, -0.05778040916215522460, 0.4822834645669289988 ) ) ;
#3282 = CARTESIAN_POINT ( 'NONE',  ( -0.9317585301837263412, -0.4281496062992127816, -0.4176697321401328100 ) ) ;
#3283 = CARTESIAN_POINT ( 'NONE',  ( 2.795275590551181466, 2.401574803149606474, 0.000000000000000000 ) ) ;
#3284 = CARTESIAN_POINT ( 'NONE',  ( -0.2362204724409447953, -0.4091458600556404646, -1.325459317585301777 ) ) ;
#3285 = CARTESIAN_POINT ( 'NONE',  ( 4.893765752498283924E-17, -0.3996062992125986035, -2.283464566929133799 ) ) ;
#3286 = CARTESIAN_POINT ( 'NONE',  ( 0.4068241469816279987, -0.3690944881889765550, -0.3153832671262227771 ) ) ;
#3287 = EDGE_LOOP ( 'NONE', ( #48332, #50283, #2170, #53603 ) ) ;
#3288 = CARTESIAN_POINT ( 'NONE',  ( -0.3392501089628019995, 0.1958661417322831999, -0.4954261399288207857 ) ) ;
#3289 = ORIENTED_EDGE ( 'NONE', *, *, #62867, .T. ) ;
#3290 = CARTESIAN_POINT ( 'NONE',  ( -0.6299212598425188991, -0.1870078740157479769, 0.4822834645669291653 ) ) ;
#3291 = CARTESIAN_POINT ( 'NONE',  ( -0.03280839895013062252, 0.2952755905511810774, -0.1292274648535930714 ) ) ;
#3292 = CARTESIAN_POINT ( 'NONE',  ( -0.3477690288713902178, 0.1771653543307087075, -0.09757992244046823083 ) ) ;
#3293 = VECTOR ( 'NONE', #63232, 39.37007874015748143 ) ;
#3294 = CARTESIAN_POINT ( 'NONE',  ( 0.6036745406824154392, 0.2306618581243847221, -0.2411417322834647770 ) ) ;
#3295 = CARTESIAN_POINT ( 'NONE',  ( -0.7480314960629914633, -0.6692913385826771977, 8.415575281601705876E-17 ) ) ;
#3296 = CARTESIAN_POINT ( 'NONE',  ( -0.3477690288713905509, -0.6692913385826771977, 0.1292274648535927661 ) ) ;
#3297 = CARTESIAN_POINT ( 'NONE',  ( 1.286089238845145033, 0.2306618581243848609, 0.2411417322834645549 ) ) ;
#3298 = CARTESIAN_POINT ( 'NONE',  ( 0.8989501312335963501, -0.6692913385826773087, -0.1292274648535924053 ) ) ;
#3299 = CARTESIAN_POINT ( 'NONE',  ( 0.8858267716535438430, 0.1660481256975885056, 0.3530559997133364547 ) ) ;
#3300 = CARTESIAN_POINT ( 'NONE',  ( 0.1958661417322836440, -0.3392501089628017219, -0.8713910761154854967 ) ) ;
#3301 = CARTESIAN_POINT ( 'NONE',  ( -0.03937007874015669567, 0.1771653543307087630, 0.000000000000000000 ) ) ;
#3302 = ORIENTED_EDGE ( 'NONE', *, *, #16262, .F. ) ;
#3303 = CARTESIAN_POINT ( 'NONE',  ( -0.3949938075777411628, 0.1058382717557497937, -1.135170603674540812 ) ) ;
#3304 = EDGE_LOOP ( 'NONE', ( #4196, #61026, #70766 ) ) ;
#3305 = CARTESIAN_POINT ( 'NONE',  ( -0.6692913385826764205, -0.5511811023622047445, 6.969142054262312111E-17 ) ) ;
#3306 = CARTESIAN_POINT ( 'NONE',  ( -0.4265091863517051496, -0.6692913385826771977, 0.1292274648535927661 ) ) ;
#3307 = CARTESIAN_POINT ( 'NONE',  ( -0.3460692066303958092, -0.1998031496062994683, 0.1049868766404199322 ) ) ;
#3308 = CARTESIAN_POINT ( 'NONE',  ( -0.1312335958005241554, 0.2306618581243848609, 0.2411417322834645549 ) ) ;
#3309 = CARTESIAN_POINT ( 'NONE',  ( -0.6233595800524928121, -0.05778040916215522460, 0.4822834645669289988 ) ) ;
#3310 = CARTESIAN_POINT ( 'NONE',  ( -1.181102362204723644, -0.1870078740157479769, 0.4822834645669291653 ) ) ;
#3311 = CARTESIAN_POINT ( 'NONE',  ( -1.318897637795274802, -0.5400638737290845981, -0.3530559997133363437 ) ) ;
#3312 = VECTOR ( 'NONE', #47726, 39.37007874015748143 ) ;
#3313 = CARTESIAN_POINT ( 'NONE',  ( 1.102362204724410155, -0.1870078740157480601, -0.3641732283464567677 ) ) ;
#3314 = CARTESIAN_POINT ( 'NONE',  ( 0.4744094488188940750, 1.537401574803149984, 1.016821367227985329 ) ) ;
#3315 = CARTESIAN_POINT ( 'NONE',  ( -0.4724409448818904789, -0.1265901696524977804, -0.5951443569553804824 ) ) ;
#3316 = CARTESIAN_POINT ( 'NONE',  ( 0.6692913385826777528, 0.1771653543307087630, 0.000000000000000000 ) ) ;
#3317 = CARTESIAN_POINT ( 'NONE',  ( 0.09186351706036827158, 0.05413385826771666132, 0.4176697321401328100 ) ) ;
#3318 = CARTESIAN_POINT ( 'NONE',  ( 0.3083989501312343062, -0.05778040916215560624, -0.4822834645669293319 ) ) ;
#3319 = EDGE_LOOP ( 'NONE', ( #38671, #58428, #41407 ) ) ;
#3320 = CARTESIAN_POINT ( 'NONE',  ( 0.3996062992125986035, 2.446882876249141962E-17, -1.535433070866141669 ) ) ;
#3321 = CARTESIAN_POINT ( 'NONE',  ( -0.5839895013123352907, 0.2952755905511810219, -0.1292274648535930437 ) ) ;
#3322 = ORIENTED_EDGE ( 'NONE', *, *, #33628, .F. ) ;
#3323 = CARTESIAN_POINT ( 'NONE',  ( -0.1998031496062994405, 0.3460692066303957537, -1.034776902887139194 ) ) ;
#3324 = CARTESIAN_POINT ( 'NONE',  ( -0.3460692066303957537, -0.1998031496062994405, -0.4442257217847768724 ) ) ;
#3325 = CARTESIAN_POINT ( 'NONE',  ( -0.5774278215223089816, 0.1283753931104746893, -0.1820866141732285504 ) ) ;
#3326 = CARTESIAN_POINT ( 'NONE',  ( -0.8005249343832013809, -0.4281496062992124485, 0.4176697321401328655 ) ) ;
#3327 = CARTESIAN_POINT ( 'NONE',  ( -0.4091458600556402980, -0.2362204724409451284, -0.05249343832020997302 ) ) ;
#3328 = CARTESIAN_POINT ( 'NONE',  ( -0.1049643490035302024, -0.3917322834645671215, -2.676509186351705871 ) ) ;
#3329 = CARTESIAN_POINT ( 'NONE',  ( 1.568241469816273659, -0.05778040916215560624, -0.4822834645669293319 ) ) ;
#3330 = CARTESIAN_POINT ( 'NONE',  ( 0.8923884514435701520, -0.6046776061558809534, -0.2411417322834644161 ) ) ;
#3331 = CARTESIAN_POINT ( 'NONE',  ( 0.7020997375328090762, -0.3162353388693405765, 0.4822834645669290543 ) ) ;
#3332 = CARTESIAN_POINT ( 'NONE',  ( -0.6430446194225712953, -0.004921259842519870586, -0.3153832671262229437 ) ) ;
#3333 = CARTESIAN_POINT ( 'NONE',  ( 0.07874015748031558404, -0.1870078740157480879, -0.4822834645669291653 ) ) ;
#3334 = CARTESIAN_POINT ( 'NONE',  ( -0.4091458600556405756, 0.2362204724409446288, -2.307742782152230721 ) ) ;
#3335 = CARTESIAN_POINT ( 'NONE',  ( -0.5249343832020990641, 0.1283753931104748280, 0.1820866141732283561 ) ) ;
#3336 = CARTESIAN_POINT ( 'NONE',  ( -0.2821522309711278487, 0.2952755905511811885, 0.1292274648535926551 ) ) ;
#3337 = CARTESIAN_POINT ( 'NONE',  ( -9.674558042662122972E-17, 0.3949938075777409963, -1.651574803149606474 ) ) ;
#3338 = CARTESIAN_POINT ( 'NONE',  ( -1.456692913385826182, -0.6692913385826771977, 8.415575281601705876E-17 ) ) ;
#3339 = CARTESIAN_POINT ( 'NONE',  ( -0.09842519685039295696, 0.07958543189024071263, -0.2665933059059888421 ) ) ;
#3340 = CARTESIAN_POINT ( 'NONE',  ( 1.489501312335958172, -0.2845877964562159024, 0.3641732283464567677 ) ) ;
#3341 = CARTESIAN_POINT ( 'NONE',  ( -1.069553805774277722, 0.2952755905511811885, 0.1292274648535926551 ) ) ;
#3342 = CARTESIAN_POINT ( 'NONE',  ( -0.5183727034120726440, 0.1771653543307087630, 0.09757992244046791164 ) ) ;
#3343 = CARTESIAN_POINT ( 'NONE',  ( 0.1181102362204724532, 0.09842519685039372024, 0.000000000000000000 ) ) ;
#3344 = CARTESIAN_POINT ( 'NONE',  ( -0.9580052493438311334, -0.4281496062992124485, 0.4176697321401328655 ) ) ;
#3345 = CARTESIAN_POINT ( 'NONE',  ( -0.4724409448818890911, -0.1870078740157480879, -0.4822834645669291653 ) ) ;
#3346 = CARTESIAN_POINT ( 'NONE',  ( 0.3346456692913393205, -0.5400638737290845981, -0.3530559997133363437 ) ) ;
#3347 = CARTESIAN_POINT ( 'NONE',  ( -0.1958661417322834497, -0.3392501089628018884, -2.350374385005562505 ) ) ;
#3348 = CARTESIAN_POINT ( 'NONE',  ( -1.916165371950965257, 1.134815007188454627, -0.2514610820057113783 ) ) ;
#3349 = CARTESIAN_POINT ( 'NONE',  ( 0.2034120734908144990, -0.5511811023622046335, 0.09757992244046803654 ) ) ;
#3350 = CARTESIAN_POINT ( 'NONE',  ( 0.9711286089238851948, 0.2306618581243848609, 0.2411417322834645549 ) ) ;
#3351 = CARTESIAN_POINT ( 'NONE',  ( -1.397637795275589623, 0.07958543189024085140, 0.2665933059059887866 ) ) ;
#3352 = EDGE_CURVE ( 'NONE', #25849, #81942, #50111, .T. ) ;
#3353 = CARTESIAN_POINT ( 'NONE',  ( 1.030183727034121421, -0.05778040916215522460, 0.4822834645669289988 ) ) ;
#3354 = CARTESIAN_POINT ( 'NONE',  ( -1.482939632545930975, -0.3690944881889765550, -0.3153832671262227771 ) ) ;
#3355 = CARTESIAN_POINT ( 'NONE',  ( -0.5577427821522301654, -0.05778040916215560624, -0.4822834645669293319 ) ) ;
#3356 = CARTESIAN_POINT ( 'NONE',  ( 0.2755905511811031494, 0.1771653543307087630, 0.000000000000000000 ) ) ;
#3357 = CARTESIAN_POINT ( 'NONE',  ( -0.8764808517432188806, 2.130908986194174812E-15, -0.4281993546915511817 ) ) ;
#3358 = CARTESIAN_POINT ( 'NONE',  ( 0.4461942257217855201, -0.5023911411419708095, 0.1820866141732285504 ) ) ;
#3359 = CARTESIAN_POINT ( 'NONE',  ( -0.01968503937007793844, -0.5400638737290844871, 0.3530559997133364547 ) ) ;
#3360 = EDGE_CURVE ( 'NONE', #56464, #69946, #43407, .T. ) ;
#3361 = CARTESIAN_POINT ( 'NONE',  ( -0.2099737532808391705, 0.2306618581243848609, 0.2411417322834645549 ) ) ;
#3362 = CARTESIAN_POINT ( 'NONE',  ( -0.1070741851644051862, -0.3996062992125986590, -0.4639107611548556331 ) ) ;
#3363 = CARTESIAN_POINT ( 'NONE',  ( -1.253280839895012377, -0.05778040916215522460, 0.4822834645669289988 ) ) ;
#3364 = CARTESIAN_POINT ( 'NONE',  ( -0.1049643490035307020, 0.3917322834645669549, -1.666010498687664043 ) ) ;
#3365 = CARTESIAN_POINT ( 'NONE',  ( 0.9186351706036751663, -0.5023911411419708095, 0.1820866141732285504 ) ) ;
#3366 = CARTESIAN_POINT ( 'NONE',  ( 0.06561679790026316017, -0.4281496062992124485, 0.4176697321401328655 ) ) ;
#3367 = CARTESIAN_POINT ( 'NONE',  ( -0.2690288713910754526, -0.6692913385826771977, 0.1292274648535927661 ) ) ;
#3368 = CARTESIAN_POINT ( 'NONE',  ( -0.3674540682414689785, 0.1283753931104748280, 0.1820866141732283561 ) ) ;
#3369 = DIRECTION ( 'NONE',  ( -6.226572250490765667E-17, 0.7071067811865368036, 0.7071067811865582309 ) ) ;
#3370 = CARTESIAN_POINT ( 'NONE',  ( -0.2624671916010490880, -0.5023911411419708095, 0.1820866141732285504 ) ) ;
#3371 = CARTESIAN_POINT ( 'NONE',  ( 0.3740157480314966754, -0.5400638737290844871, 0.3530559997133364547 ) ) ;
#3372 = CARTESIAN_POINT ( 'NONE',  ( -1.332020997375327642, -0.2845877964562161244, -0.3641732283464567121 ) ) ;
#3374 = CARTESIAN_POINT ( 'NONE',  ( -0.3460692066303960313, 0.1998031496062989965, -1.047900262467191590 ) ) ;
#3373 = VECTOR ( 'NONE', #51517, 39.37007874015748143 ) ;
#3375 = CARTESIAN_POINT ( 'NONE',  ( -1.043307086614172041, -0.5400638737290844871, 0.3530559997133364547 ) ) ;
#3376 = CARTESIAN_POINT ( 'NONE',  ( 3.937007874015748143, 2.559055118110236560, -0.3149606299212596716 ) ) ;
#3377 = VERTEX_POINT ( 'NONE', #75808 ) ;
#3378 = CARTESIAN_POINT ( 'NONE',  ( -1.443569553805773564, -0.5023911411419708095, 0.1820866141732285504 ) ) ;
#3379 = CARTESIAN_POINT ( 'NONE',  ( -0.2624671916010490880, 0.2306618581243847221, -0.2411417322834647770 ) ) ;
#3380 = EDGE_CURVE ( 'NONE', #80676, #37563, #44605, .T. ) ;
#3381 = CARTESIAN_POINT ( 'NONE',  ( 0.2893625497513035438, 1.161323636346416777, -1.436460574497700371 ) ) ;
#3382 = CARTESIAN_POINT ( 'NONE',  ( -1.364829396325458521, -0.6046776061558807314, 0.2411417322834647770 ) ) ;
#3383 = CARTESIAN_POINT ( 'NONE',  ( -0.2867679344610365999, 0.2867679344610364889, -1.679133858267716661 ) ) ;
#3384 = FACE_OUTER_BOUND ( 'NONE', #39495, .T. ) ;
#3385 = CARTESIAN_POINT ( 'NONE',  ( 1.371391076115485941, 0.2952755905511811885, 0.1292274648535926551 ) ) ;
#3386 = CARTESIAN_POINT ( 'NONE',  ( 0.8005249343832028242, -0.4281496062992127816, -0.4176697321401328100 ) ) ;
#3387 = FACE_OUTER_BOUND ( 'NONE', #20860, .T. ) ;
#3388 = CARTESIAN_POINT ( 'NONE',  ( 0.2925321140481931814, -0.2925321140481931259, -2.222440944881889813 ) ) ;
#3389 = CARTESIAN_POINT ( 'NONE',  ( 1.568241469816273437, -0.2845877964562159024, 0.3641732283464567677 ) ) ;
#3390 = CARTESIAN_POINT ( 'NONE',  ( 4.893765752498283924E-17, -0.3996062992125986035, -0.5511811023622047445 ) ) ;
#3392 = EDGE_CURVE ( 'NONE', #82899, #20923, #18685, .T. ) ;
#3391 = ORIENTED_EDGE ( 'NONE', *, *, #79579, .T. ) ;
#3393 = CARTESIAN_POINT ( 'NONE',  ( -0.6758530183727028406, 0.1771653543307087630, 0.09757992244046791164 ) ) ;
#3394 = CARTESIAN_POINT ( 'NONE',  ( -0.1049643490035302024, -0.3917322834645671215, -2.111548556430446144 ) ) ;
#3395 = ORIENTED_EDGE ( 'NONE', *, *, #75224, .F. ) ;
#3396 = CARTESIAN_POINT ( 'NONE',  ( 1.030183727034121421, -0.3162353388693409650, -0.4822834645669289433 ) ) ;
#3397 = CARTESIAN_POINT ( 'NONE',  ( -0.2755905511811018171, 0.2952755905511811885, 0.000000000000000000 ) ) ;
#3398 = CARTESIAN_POINT ( 'NONE',  ( -1.220472440944881054, -0.6692913385826771977, 8.415575281601705876E-17 ) ) ;
#3399 = CARTESIAN_POINT ( 'NONE',  ( 1.417322834645670104, -0.1870078740157480879, -0.4822834645669291653 ) ) ;
#3400 = CARTESIAN_POINT ( 'NONE',  ( -1.161417322834644716, 0.07958543189024085140, 0.2665933059059887866 ) ) ;
#3401 = CARTESIAN_POINT ( 'NONE',  ( 0.4996603843015406943, 1.493546695279807990, -0.5309055118110237448 ) ) ;
#3402 = CARTESIAN_POINT ( 'NONE',  ( 0.3608923884514443348, -0.6692913385826771977, 0.1292274648535927661 ) ) ;
#3403 = CARTESIAN_POINT ( 'NONE',  ( -0.6824146981627288167, 0.2306618581243848609, 0.2411417322834645549 ) ) ;
#3404 = CARTESIAN_POINT ( 'NONE',  ( -0.2867679344610364334, -0.2867679344610368219, -1.398930815451756793 ) ) ;
#3405 = CARTESIAN_POINT ( 'NONE',  ( -1.417322834645668772, -0.1870078740157480879, -0.4822834645669291653 ) ) ;
#3406 = CARTESIAN_POINT ( 'NONE',  ( 0.1341302950245132075, 1.082049466318357300, -2.856398576552468427 ) ) ;
#3407 = EDGE_CURVE ( 'NONE', #58566, #35196, #5274, .T. ) ;
#3408 = CARTESIAN_POINT ( 'NONE',  ( 0.9055118110236227702, 0.2952755905511811885, 0.000000000000000000 ) ) ;
#3409 = CARTESIAN_POINT ( 'NONE',  ( 1.364829396325460076, 0.1283753931104748280, 0.1820866141732283561 ) ) ;
#3410 = ORIENTED_EDGE ( 'NONE', *, *, #52110, .F. ) ;
#3411 = CARTESIAN_POINT ( 'NONE',  ( -0.1049643490035307158, 0.3917322834645670104, -2.837945824968191477 ) ) ;
#3412 = CARTESIAN_POINT ( 'NONE',  ( -0.3608923884514428360, 0.2952755905511811885, 0.1292274648535926551 ) ) ;
#3413 = EDGE_LOOP ( 'NONE', ( #79310, #76893, #82001, #45320 ) ) ;
#3414 = CARTESIAN_POINT ( 'NONE',  ( 0.4527559055118117182, -0.4536011799217367080, 0.2665933059059888421 ) ) ;
#3415 = CARTESIAN_POINT ( 'NONE',  ( -1.581364829396324945, -0.3162353388693405765, 0.4822834645669290543 ) ) ;
#3416 = CARTESIAN_POINT ( 'NONE',  ( 0.9317585301837276734, -0.4281496062992124485, 0.4176697321401328655 ) ) ;
#3417 = CARTESIAN_POINT ( 'NONE',  ( 0.8464566929133865436, 0.1660481256975883668, -0.3530559997133364547 ) ) ;
#3418 = CARTESIAN_POINT ( 'NONE',  ( -0.1574803149606292529, -0.1870078740157479769, 0.4822834645669291653 ) ) ;
#3419 = CARTESIAN_POINT ( 'NONE',  ( 0.3917322834645670659, -0.1049643490035303273, -1.053168922081052283 ) ) ;
#3420 = CARTESIAN_POINT ( 'NONE',  ( -0.6692913385826764205, 0.2952755905511811885, 0.000000000000000000 ) ) ;
#3421 = CARTESIAN_POINT ( 'NONE',  ( 0.3917322834645670104, 2.398668435337828261E-17, -2.407480314960630086 ) ) ;
#3422 = CARTESIAN_POINT ( 'NONE',  ( -1.686351706036744558, 0.2952755905511810774, -0.1292274648535930714 ) ) ;
#3423 = CARTESIAN_POINT ( 'NONE',  ( -1.043307086614172041, -0.5400638737290844871, 0.3530559997133364547 ) ) ;
#3424 = CARTESIAN_POINT ( 'NONE',  ( 1.154855643044620184, -0.6046776061558807314, 0.2411417322834647770 ) ) ;
#3425 = CARTESIAN_POINT ( 'NONE',  ( 1.469816272965879911, -0.6046776061558807314, 0.2411417322834647770 ) ) ;
#3426 = CARTESIAN_POINT ( 'NONE',  ( -1.043307086614172707, 0.1660481256975883668, -0.3530559997133364547 ) ) ;
#3427 = CARTESIAN_POINT ( 'NONE',  ( -0.3460692066303957537, -0.1998031496062994405, 0.1856955380577427484 ) ) ;
#3428 = CARTESIAN_POINT ( 'NONE',  ( 0.1771653543307093182, 0.1660481256975885056, 0.3530559997133364547 ) ) ;
#3429 = CARTESIAN_POINT ( 'NONE',  ( 0.1070741851644053527, 0.3996062992125986590, -1.725721784776903078 ) ) ;
#3430 = CARTESIAN_POINT ( 'NONE',  ( -0.7414698162729651543, -0.6692913385826771977, 0.1292274648535927661 ) ) ;
#3431 = VECTOR ( 'NONE', #51039, 39.37007874015748143 ) ;
#3432 = CARTESIAN_POINT ( 'NONE',  ( 1.587926509186352586, -0.4281496062992127816, -0.4176697321401328100 ) ) ;
#3433 = CARTESIAN_POINT ( 'NONE',  ( 0.5511811023622055217, -0.1870078740157479769, 0.3641732283464567677 ) ) ;
#3434 = CARTESIAN_POINT ( 'NONE',  ( 1.423884514435696191, -0.05778040916215522460, 0.4822834645669289988 ) ) ;
#3435 = CARTESIAN_POINT ( 'NONE',  ( -0.4724409448818895907, -0.1265901696524993070, -0.5951443569553805935 ) ) ;
#3436 = CARTESIAN_POINT ( 'NONE',  ( 1.371391076115485941, 0.1771653543307087630, 0.09757992244046791164 ) ) ;
#3437 = CARTESIAN_POINT ( 'NONE',  ( 0.8070866141732288002, 0.1660481256975885056, 0.3530559997133364547 ) ) ;
#3438 = CARTESIAN_POINT ( 'NONE',  ( -0.3949938075777408852, -0.1058382717557502933, -0.5951443569553805935 ) ) ;
#3439 = CARTESIAN_POINT ( 'NONE',  ( -0.5380577427821514602, -0.4281496062992127816, -0.4176697321401328100 ) ) ;
#3440 = CARTESIAN_POINT ( 'NONE',  ( 1.586052503253845281, 1.299212598425198095, 0.1653254495020587411 ) ) ;
#3441 = CARTESIAN_POINT ( 'NONE',  ( 1.259842519685040019, -0.1870078740157479769, 0.3641732283464567677 ) ) ;
#3442 = CARTESIAN_POINT ( 'NONE',  ( -0.6561679790026240244, -0.6046776061558807314, 0.2411417322834647770 ) ) ;
#3443 = CARTESIAN_POINT ( 'NONE',  ( 0.1974969037888704704, 0.3420746716998660508, -0.5360892388451443669 ) ) ;
#3444 = CARTESIAN_POINT ( 'NONE',  ( 1.423884514435696413, -0.3162353388693409650, -0.4822834645669289433 ) ) ;
#3445 = CARTESIAN_POINT ( 'NONE',  ( 0.09186351706036799403, -0.4281496062992127816, -0.4176697321401328100 ) ) ;
#3446 = CARTESIAN_POINT ( 'NONE',  ( 0.5118110236220480003, -0.5511811023622047445, 6.969142054262312111E-17 ) ) ;
#3447 = FACE_OUTER_BOUND ( 'NONE', #52967, .T. ) ;
#3448 = CARTESIAN_POINT ( 'NONE',  ( -0.1049868766404193215, -0.5023911411419708095, 0.1820866141732285504 ) ) ;
#3449 = CARTESIAN_POINT ( 'NONE',  ( -1.522309711286088607, -0.6046776061558807314, 0.2411417322834647770 ) ) ;
#3450 = CARTESIAN_POINT ( 'NONE',  ( 4.893765752498283308E-17, -0.3996062992125985480, -1.415354330708661568 ) ) ;
#3451 = CARTESIAN_POINT ( 'NONE',  ( 0.8267716535433078384, -0.6692913385826771977, 8.415575281601705876E-17 ) ) ;
#3452 = CARTESIAN_POINT ( 'NONE',  ( 0.1049643490035303689, 0.3917322834645670104, -1.087926509186351476 ) ) ;
#3453 = CARTESIAN_POINT ( 'NONE',  ( 1.653543307086614789, -0.1870078740157479769, 0.3641732283464567677 ) ) ;
#3454 = CARTESIAN_POINT ( 'NONE',  ( -0.3738583250858234508, -0.1188761721681601269, 7.390873527593494894E-17 ) ) ;
#3455 = B_SPLINE_CURVE_WITH_KNOTS ( 'NONE', 3,
 ( #23915, #23498, #74870, #82006, #18029, #55062, #80770, #62634, #17213, #10879 ),
 .UNSPECIFIED., .F., .F.,
 ( 4, 2, 2, 2, 4 ),
 ( 0.000000000000000000, 0.001551611299846701337, 0.002327416949770050921, 0.002715319774731725280, 0.003103222599693400072 ),
 .UNSPECIFIED. ) ;
#3456 = CARTESIAN_POINT ( 'NONE',  ( -0.1377952755905504645, 0.07958543189024085140, 0.2665933059059887866 ) ) ;
#3457 = EDGE_CURVE ( 'NONE', #61268, #4549, #29861, .T. ) ;
#3458 = CARTESIAN_POINT ( 'NONE',  ( 0.2755905511811031494, 0.2952755905511811885, 0.000000000000000000 ) ) ;
#3459 = CARTESIAN_POINT ( 'NONE',  ( 1.332020997375329197, -0.2845877964562159024, 0.3641732283464567677 ) ) ;
#3460 = CARTESIAN_POINT ( 'NONE',  ( -1.312335958005248715, -0.5023911411419708095, -0.1820866141732282451 ) ) ;
#3461 = CARTESIAN_POINT ( 'NONE',  ( -1.627296587926508442, -0.6046776061558809534, -0.2411417322834644161 ) ) ;
#3462 = CARTESIAN_POINT ( 'NONE',  ( 0.4199475065616805614, 0.2306618581243848609, 0.2411417322834645549 ) ) ;
#3463 = CARTESIAN_POINT ( 'NONE',  ( 1.332020997375329197, -0.3162353388693405765, 0.4822834645669290543 ) ) ;
#3464 = CARTESIAN_POINT ( 'NONE',  ( 0.4091458600556403535, 0.2362204724409449896, -0.2080052493438320216 ) ) ;
#3465 = CARTESIAN_POINT ( 'NONE',  ( 0.06561679790026316017, 0.05413385826771626580, -0.4176697321401330321 ) ) ;
#3466 = CARTESIAN_POINT ( 'NONE',  ( 1.299212598425197429, -0.6692913385826771977, 8.415575281601705876E-17 ) ) ;
#3467 = CARTESIAN_POINT ( 'NONE',  ( 1.115485564304462551, -0.4281496062992127816, -0.4176697321401328100 ) ) ;
#3468 = CARTESIAN_POINT ( 'NONE',  ( 1.895394334970792016, 2.755905511811024056, 0.5314960629921260393 ) ) ;
#3469 = CARTESIAN_POINT ( 'NONE',  ( 0.7020997375328090762, -0.2845877964562159024, 0.3641732283464567677 ) ) ;
#3470 = CARTESIAN_POINT ( 'NONE',  ( 1.561679790026247350, 0.05413385826771626580, -0.4176697321401330321 ) ) ;
#3471 = CARTESIAN_POINT ( 'NONE',  ( 0.3477690288713918276, 0.1771653543307087630, 0.09757992244046791164 ) ) ;
#3472 = CARTESIAN_POINT ( 'NONE',  ( 0.3018372703412079971, 0.05413385826771626580, -0.4176697321401330321 ) ) ;
#3473 = CARTESIAN_POINT ( 'NONE',  ( 0.5577427821522314977, -0.3162353388693409650, -0.4822834645669289433 ) ) ;
#3474 = CARTESIAN_POINT ( 'NONE',  ( -0.3477690288713902178, 0.2952755905511810774, -0.1292274648535930714 ) ) ;
#3475 = CARTESIAN_POINT ( 'NONE',  ( 0.1968503937007881344, 0.1771653543307087630, 0.000000000000000000 ) ) ;
#3476 = CARTESIAN_POINT ( 'NONE',  ( 0.9973753280839902091, 0.2306618581243847221, -0.2411417322834647770 ) ) ;
#3477 = DIRECTION ( 'NONE',  ( 0.000000000000000000, 1.000000000000000000, -0.000000000000000000 ) ) ;
#3478 = CARTESIAN_POINT ( 'NONE',  ( -1.135170603674539924, -0.6692913385826771977, 0.1292274648535927661 ) ) ;
#3480 = CARTESIAN_POINT ( 'NONE',  ( 0.1070741851644054915, -0.3996062992125985480, -1.030183727034120533 ) ) ;
#3479 = DIRECTION ( 'NONE',  ( -0.000000000000000000, 1.000000000000000000, -0.000000000000000000 ) ) ;
#3481 = CARTESIAN_POINT ( 'NONE',  ( 1.348312163386739426, 1.062992125984252079, 0.7386866130305692613 ) ) ;
#3483 = VECTOR ( 'NONE', #32080, 39.37007874015748143 ) ;
#3482 = CARTESIAN_POINT ( 'NONE',  ( -1.082677165354329896, -0.5400638737290845981, -0.3530559997133363437 ) ) ;
#3484 = CARTESIAN_POINT ( 'NONE',  ( -0.4593175853018366950, 0.05413385826771666132, 0.4176697321401328100 ) ) ;
#3485 = CARTESIAN_POINT ( 'NONE',  ( -0.3458507752293909498, 0.3458507752293907833, -0.01968503937007874335 ) ) ;
#3486 = CARTESIAN_POINT ( 'NONE',  ( -0.2891555358219911054, 0.2891555358219909388, -2.539370078740157854 ) ) ;
#3487 = VERTEX_POINT ( 'NONE', #30766 ) ;
#3488 = CARTESIAN_POINT ( 'NONE',  ( 0.9317585301837276734, -0.004921259842519870586, -0.3153832671262229437 ) ) ;
#3489 = CARTESIAN_POINT ( 'NONE',  ( -0.3917322834645671215, 0.1049643490035301469, -0.9698162729658791337 ) ) ;
#3490 = CARTESIAN_POINT ( 'NONE',  ( 1.161417322834646271, 0.1660481256975883668, -0.3530559997133364547 ) ) ;
#3491 = CARTESIAN_POINT ( 'NONE',  ( 0.2362204724409449064, 0.4091458600556404646, -2.349081364829396446 ) ) ;
#3492 = CARTESIAN_POINT ( 'NONE',  ( 0.4606732211678790101, 2.401574803149606030, 0.5309055118110234117 ) ) ;
#3493 = CARTESIAN_POINT ( 'NONE',  ( -1.555118110236219930, 0.07958543189024085140, 0.2665933059059887866 ) ) ;
#3494 = CARTESIAN_POINT ( 'NONE',  ( 1.430446194225722500, -0.4281496062992127816, -0.4176697321401328100 ) ) ;
#3495 = CARTESIAN_POINT ( 'NONE',  ( 1.305774278215223960, 0.1771653543307087075, -0.09757992244046823083 ) ) ;
#3496 = CARTESIAN_POINT ( 'NONE',  ( 0.5380577427821529035, -0.4281496062992124485, 0.4176697321401328655 ) ) ;
#3497 = CARTESIAN_POINT ( 'NONE',  ( 0.3392501089628018329, -0.1958661417322834497, -0.1850200542969010764 ) ) ;
#3498 = CARTESIAN_POINT ( 'NONE',  ( -0.08530183727034056085, -0.3162353388693405765, 0.4822834645669290543 ) ) ;
#3499 = CARTESIAN_POINT ( 'NONE',  ( -0.8333333333333323711, -0.5511811023622048555, -0.09757992244046775898 ) ) ;
#3500 = CARTESIAN_POINT ( 'NONE',  ( 0.8727034120734912248, -0.3162353388693409650, -0.4822834645669289433 ) ) ;
#3501 = CARTESIAN_POINT ( 'NONE',  ( -0.2165354330708654795, -0.5400638737290845981, -0.3530559997133363437 ) ) ;
#3502 = CARTESIAN_POINT ( 'NONE',  ( 0.5183727034120741983, 0.2952755905511810219, -0.1292274648535930437 ) ) ;
#3503 = CARTESIAN_POINT ( 'NONE',  ( -0.2925321140481932924, 0.2925321140481931814, -2.854330708661417138 ) ) ;
#3504 = CARTESIAN_POINT ( 'NONE',  ( -0.3392501089628019995, 0.1958661417322831999, -1.755268659613860249 ) ) ;
#3505 = CARTESIAN_POINT ( 'NONE',  ( 0.8792650918635177559, 0.05413385826771666132, 0.4176697321401328100 ) ) ;
#3506 = CARTESIAN_POINT ( 'NONE',  ( 0.09842519685039434474, -0.5400638737290845981, -0.3530559997133363437 ) ) ;
#3507 = CARTESIAN_POINT ( 'NONE',  ( -1.115485564304461219, 0.05413385826771626580, -0.4176697321401330321 ) ) ;
#3508 = CARTESIAN_POINT ( 'NONE',  ( 0.9842519685039375910, 0.2952755905511811885, 0.000000000000000000 ) ) ;
#3509 = CARTESIAN_POINT ( 'NONE',  ( 0.5774278215223104249, 0.2306618581243848609, 0.2411417322834645549 ) ) ;
#3510 = CARTESIAN_POINT ( 'NONE',  ( -0.1958661417322834220, -0.3392501089628018884, -0.9376640419947508409 ) ) ;
#3511 = CARTESIAN_POINT ( 'NONE',  ( -0.2427821522309703550, -0.05778040916215560624, -0.4822834645669293319 ) ) ;
#3512 = CARTESIAN_POINT ( 'NONE',  ( 0.5774278215223104249, 0.2306618581243848609, 0.2411417322834645549 ) ) ;
#3513 = CARTESIAN_POINT ( 'NONE',  ( -0.1312335958005241554, -0.6046776061558809534, -0.2411417322834644161 ) ) ;
#3514 = CARTESIAN_POINT ( 'NONE',  ( 0.6102362204724416372, 0.07958543189024071263, -0.2665933059059888421 ) ) ;
#3515 = CARTESIAN_POINT ( 'NONE',  ( -2.787279214012418738, 0.000000000000000000, 0.000000000000000000 ) ) ;
#3516 = CARTESIAN_POINT ( 'NONE',  ( -1.653543307086613234, -0.1870078740157480879, -0.4822834645669291653 ) ) ;
#3517 = CARTESIAN_POINT ( 'NONE',  ( 0.1443569553805781891, -0.4281496062992124485, 0.4176697321401328655 ) ) ;
#3518 = CARTESIAN_POINT ( 'NONE',  ( -0.3458507752293906723, -0.3458507752293910609, -0.9232283464566929387 ) ) ;
#3519 = CARTESIAN_POINT ( 'NONE',  ( 0.1958661417322834775, 0.3392501089628018884, -2.498687664041994605 ) ) ;
#3520 = ORIENTED_EDGE ( 'NONE', *, *, #72820, .F. ) ;
#3521 = ORIENTED_EDGE ( 'NONE', *, *, #17984, .T. ) ;
#3522 = CIRCLE ( 'NONE', #25000, 0.1190944881889763746 ) ;
#3523 = CARTESIAN_POINT ( 'NONE',  ( 0.6627296587926517768, -0.6692913385826773087, -0.1292274648535924053 ) ) ;
#3524 = CARTESIAN_POINT ( 'NONE',  ( 0.4593175853018379162, -0.3690944881889763329, 0.3153832671262228327 ) ) ;
#3525 = TOROIDAL_SURFACE ( 'NONE', #45125, 0.1574803149606295860, 0.01968503937007873988 ) ;
#3526 = CONICAL_SURFACE ( 'NONE', #50531, 1.889763779527559251, 0.7853981633974500554 ) ;
#3528 = DIRECTION ( 'NONE',  ( 3.096699300667737957E-16, -1.000000000000000000, 0.000000000000000000 ) ) ;
#3527 = DIRECTION ( 'NONE',  ( -1.000000000000000000, -8.326672684688674053E-16, 0.000000000000000000 ) ) ;
#3529 = CARTESIAN_POINT ( 'NONE',  ( -0.3917322834645669549, -0.1049643490035306603, -0.9179790026246721357 ) ) ;
#3530 = DIRECTION ( 'NONE',  ( -0.000000000000000000, -1.000000000000000000, -0.000000000000000000 ) ) ;
#3531 = CARTESIAN_POINT ( 'NONE',  ( 0.3980111619244091625, 0.03175677952935741788, -1.929133858267720436 ) ) ;
#3532 = CARTESIAN_POINT ( 'NONE',  ( 0.3917322834645669549, 0.1049643490035304660, -1.469160104986876769 ) ) ;
#3533 = CARTESIAN_POINT ( 'NONE',  ( 0.1998031496062992463, 0.3460692066303959202, -2.583333333333333481 ) ) ;
#3534 = CARTESIAN_POINT ( 'NONE',  ( 0.8727034120734912248, -0.3162353388693409650, -0.4822834645669289433 ) ) ;
#3535 = CARTESIAN_POINT ( 'NONE',  ( -0.6364829396325453192, -0.05778040916215560624, -0.4822834645669293319 ) ) ;
#3536 = CARTESIAN_POINT ( 'NONE',  ( -0.8005249343832013809, -0.4281496062992124485, 0.4176697321401328655 ) ) ;
#3537 = CARTESIAN_POINT ( 'NONE',  ( 0.5971128608923890191, -0.6692913385826771977, 0.1292274648535927661 ) ) ;
#3538 = CARTESIAN_POINT ( 'NONE',  ( 1.220472440944882386, -0.6692913385826771977, 8.415575281601705876E-17 ) ) ;
#3539 = CARTESIAN_POINT ( 'NONE',  ( 1.633858267716535639, -0.4536011799217367080, 0.2665933059059888421 ) ) ;
#3540 = APPLICATION_PROTOCOL_DEFINITION ( 'draft international standard', 'automotive_design', 1998, #12679 ) ;
#3541 = CARTESIAN_POINT ( 'NONE',  ( 1.069553805774278832, 0.1771653543307087075, -0.09757992244046823083 ) ) ;
#3542 = CARTESIAN_POINT ( 'NONE',  ( -9.787531504996566615E-17, 0.3996062992125985480, -1.966535433070866201 ) ) ;
#3543 = CARTESIAN_POINT ( 'NONE',  ( -1.430446194225720724, -0.004921259842519870586, -0.3153832671262229437 ) ) ;
#3544 = CARTESIAN_POINT ( 'NONE',  ( -0.1049643490035307020, 0.3917322834645669549, 0.1587926509186352031 ) ) ;
#3545 = CARTESIAN_POINT ( 'NONE',  ( 0.08530183727034192087, -0.05778040916215522460, 0.4822834645669289988 ) ) ;
#3546 = VECTOR ( 'NONE', #11617, 39.37007874015748143 ) ;
#3548 = CARTESIAN_POINT ( 'NONE',  ( -1.603475055217291612, 1.543447618314657932, 0.04573490813648255215 ) ) ;
#3547 = CARTESIAN_POINT ( 'NONE',  ( 1.614173228346457378, -0.6692913385826771977, 8.415575281601705876E-17 ) ) ;
#3549 = CARTESIAN_POINT ( 'NONE',  ( -1.213910761154854745, 0.1771653543307087075, -0.09757992244046823083 ) ) ;
#3550 = CARTESIAN_POINT ( 'NONE',  ( 0.5380577427821529035, -0.4281496062992124485, 0.4176697321401328655 ) ) ;
#3551 = CARTESIAN_POINT ( 'NONE',  ( 1.384514435695538337, -0.5511811023622046335, 0.09757992244046803654 ) ) ;
#3552 = EDGE_CURVE ( 'NONE', #23894, #61368, #47286, .T. ) ;
#3553 = CARTESIAN_POINT ( 'NONE',  ( -0.2867679344610364334, -0.2867679344610368219, -1.398930815451756793 ) ) ;
#3554 = CARTESIAN_POINT ( 'NONE',  ( -1.286089238845143479, -0.5023911411419708095, 0.1820866141732285504 ) ) ;
#3555 = CARTESIAN_POINT ( 'NONE',  ( 1.213910761154856299, 0.2952755905511811885, 0.1292274648535926551 ) ) ;
#3556 = CARTESIAN_POINT ( 'NONE',  ( 0.07836124490824399047, 1.950604500417927323, 0.3034306265812344305 ) ) ;
#3557 = CARTESIAN_POINT ( 'NONE',  ( -0.1049868766404193215, 0.2306618581243847221, -0.2411417322834647770 ) ) ;
#3558 = CARTESIAN_POINT ( 'NONE',  ( -1.410761154855641575, -0.2845877964562161244, -0.3641732283464567121 ) ) ;
#3559 = CARTESIAN_POINT ( 'NONE',  ( -0.5314960629921254842, -0.5400638737290845981, -0.3530559997133363437 ) ) ;
#3560 = CARTESIAN_POINT ( 'NONE',  ( -1.640419947506561060, -0.004921259842519576551, 0.3153832671262227771 ) ) ;
#3561 = CARTESIAN_POINT ( 'NONE',  ( -0.3917322834645670104, -0.1049643490035307020, -0.6725914942595296875 ) ) ;
#3562 = CARTESIAN_POINT ( 'NONE',  ( 0.4199475065616803948, -0.6046776061558809534, -0.2411417322834644161 ) ) ;
#3563 = CARTESIAN_POINT ( 'NONE',  ( 1.443569553805774897, 0.2306618581243848609, 0.2411417322834645549 ) ) ;
#3564 = CARTESIAN_POINT ( 'NONE',  ( -0.4724409448818899238, 0.1265901696524986686, -1.999343832020997525 ) ) ;
#3565 = CARTESIAN_POINT ( 'NONE',  ( -1.240157480314959759, 0.1660481256975885056, 0.3530559997133364547 ) ) ;
#3566 = CARTESIAN_POINT ( 'NONE',  ( -0.6496062992125976043, -0.4536011799217367080, 0.2665933059059888421 ) ) ;
#3567 = CARTESIAN_POINT ( 'NONE',  ( -1.627296587926508442, 0.2306618581243848609, 0.2411417322834645549 ) ) ;
#3568 = CARTESIAN_POINT ( 'NONE',  ( 0.1049868766404206816, 0.2306618581243848609, 0.2411417322834645549 ) ) ;
#3569 = CARTESIAN_POINT ( 'NONE',  ( 0.2296587926509192634, -0.2845877964562159024, 0.3641732283464567677 ) ) ;
#3570 = CARTESIAN_POINT ( 'NONE',  ( -1.194225721784776262, -0.004921259842519870586, -0.3153832671262229437 ) ) ;
#3571 = CARTESIAN_POINT ( 'NONE',  ( -1.594488188976377563, -0.5400638737290844871, 0.3530559997133364547 ) ) ;
#3572 = CARTESIAN_POINT ( 'NONE',  ( -1.568241469816272105, -0.05778040916215522460, 0.4822834645669289988 ) ) ;
#3573 = CARTESIAN_POINT ( 'NONE',  ( 1.463254593175853824, -0.6692913385826771977, 0.1292274648535927661 ) ) ;
#3574 = CARTESIAN_POINT ( 'NONE',  ( 0.4698793137518422203, 1.469922167998567897, 2.159263675096192436 ) ) ;
#3575 = CARTESIAN_POINT ( 'NONE',  ( 0.4265091863517067594, 0.1771653543307087630, 0.09757992244046791164 ) ) ;
#3576 = CARTESIAN_POINT ( 'NONE',  ( 1.030183727034121421, -0.05778040916215522460, 0.4822834645669289988 ) ) ;
#3577 = CARTESIAN_POINT ( 'NONE',  ( -1.595398199321657051, 0.7375059713363285585, 0.1559797534342473035 ) ) ;
#3578 = CARTESIAN_POINT ( 'NONE',  ( 1.325459317585302665, -0.004921259842519870586, -0.3153832671262229437 ) ) ;
#3579 = ORIENTED_EDGE ( 'NONE', *, *, #3352, .F. ) ;
#3580 = CARTESIAN_POINT ( 'NONE',  ( -1.036745406824146176, -0.4281496062992124485, 0.4176697321401328655 ) ) ;
#3581 = CARTESIAN_POINT ( 'NONE',  ( -0.8858267716535425107, -0.5400638737290844871, 0.3530559997133364547 ) ) ;
#3582 = CARTESIAN_POINT ( 'NONE',  ( 0.3083989501312343062, -0.3162353388693405765, 0.4822834645669290543 ) ) ;
#3583 = AXIS2_PLACEMENT_3D ( 'NONE', #3131, #56113, #9860 ) ;
#3584 = CARTESIAN_POINT ( 'NONE',  ( 0.5411721830064198935, 8.471767977567108961E-16, -0.4445507791589058955 ) ) ;
#3585 = CARTESIAN_POINT ( 'NONE',  ( 0.3996062992125985480, 2.446882876249141654E-17, -2.242125984251968518 ) ) ;
#3586 = CARTESIAN_POINT ( 'NONE',  ( 1.023622047244095112, -0.1870078740157480879, -0.4822834645669291653 ) ) ;
#3587 = CARTESIAN_POINT ( 'NONE',  ( 1.476377952755906220, 0.07958543189024071263, -0.2665933059059888421 ) ) ;
#3588 = VECTOR ( 'NONE', #70655, 39.37007874015748143 ) ;
#3589 = CARTESIAN_POINT ( 'NONE',  ( 0.3412073490813655186, -0.6046776061558809534, -0.2411417322834644161 ) ) ;
#3590 = CARTESIAN_POINT ( 'NONE',  ( 0.6430446194225728496, 0.05413385826771666132, 0.4176697321401328100 ) ) ;
#3591 = CARTESIAN_POINT ( 'NONE',  ( 0.2925321140481932369, -0.2925321140481932369, -1.830708661417322913 ) ) ;
#3592 = CARTESIAN_POINT ( 'NONE',  ( 0.2891555358219910499, -0.2891555358219909944, -1.200787401574803237 ) ) ;
#3593 = CARTESIAN_POINT ( 'NONE',  ( -0.3996062992125987146, 0.1070741851644051862, -2.395013123359580387 ) ) ;
#3594 = CARTESIAN_POINT ( 'NONE',  ( -0.1752652180395700143, -0.2378425880835044193, 0.1496354662858539464 ) ) ;
#3595 = CARTESIAN_POINT ( 'NONE',  ( 0.3392501089628018329, 0.1958661417322835607, -0.1233595800524933811 ) ) ;
#3596 = CARTESIAN_POINT ( 'NONE',  ( -0.2230971128608915943, -0.3690944881889765550, -0.3153832671262227771 ) ) ;
#3597 = CARTESIAN_POINT ( 'NONE',  ( -0.1574803149606292529, -0.1870078740157479769, 0.4822834645669291653 ) ) ;
#3598 = CARTESIAN_POINT ( 'NONE',  ( 0.7349081364829402885, -0.6046776061558809534, -0.2411417322834644161 ) ) ;
#3599 = CARTESIAN_POINT ( 'NONE',  ( -0.1058382717557503072, 0.3949938075777408852, -2.288057742782152459 ) ) ;
#3600 = CARTESIAN_POINT ( 'NONE',  ( -0.1968503937007867743, 0.1771653543307087630, 0.000000000000000000 ) ) ;
#3601 = CARTESIAN_POINT ( 'NONE',  ( -1.010498687664041384, 0.05413385826771666132, 0.4176697321401328100 ) ) ;
#3602 = CARTESIAN_POINT ( 'NONE',  ( 1.056430446194226436, -0.6692913385826773087, -0.1292274648535924053 ) ) ;
#3603 = CARTESIAN_POINT ( 'NONE',  ( 0.4724409448818898682, 2.892866454678787531E-17, -2.637795275590551380 ) ) ;
#3604 = CARTESIAN_POINT ( 'NONE',  ( 0.2925321140481932369, 0.2925321140481932369, -1.870078740157480546 ) ) ;
#3605 = CARTESIAN_POINT ( 'NONE',  ( 0.5387615594602676028, 2.409604939980833412E-17, -0.3464511005275205946 ) ) ;
#3606 = VERTEX_POINT ( 'NONE', #31166 ) ;
#3607 = CARTESIAN_POINT ( 'NONE',  ( 0.9908136482939640111, 0.2952755905511810774, -0.1292274648535930714 ) ) ;
#3608 = CARTESIAN_POINT ( 'NONE',  ( 1.299212598425197429, 0.1771653543307087630, 0.000000000000000000 ) ) ;
#3610 = CARTESIAN_POINT ( 'NONE',  ( -1.482939632545930975, 0.05413385826771666132, 0.4176697321401328100 ) ) ;
#3609 = CARTESIAN_POINT ( 'NONE',  ( -1.443569553805773564, 0.1283753931104746893, -0.1820866141732285504 ) ) ;
#3611 = CARTESIAN_POINT ( 'NONE',  ( -0.2867679344610365999, 0.2867679344610364889, 0.2106299212598424508 ) ) ;
#3612 = CARTESIAN_POINT ( 'NONE',  ( 1.193035393573956160, 6.860680731889873434E-16, 0.3627989612356145033 ) ) ;
#3613 = CARTESIAN_POINT ( 'NONE',  ( 1.122047244094488860, -0.5400638737290845981, -0.3530559997133363437 ) ) ;
#3614 = CARTESIAN_POINT ( 'NONE',  ( -1.640419947506561060, -0.4281496062992127816, -0.4176697321401328100 ) ) ;
#3615 = CARTESIAN_POINT ( 'NONE',  ( -0.006561679790025524116, -0.3162353388693405765, 0.4822834645669290543 ) ) ;
#3616 = CARTESIAN_POINT ( 'NONE',  ( -0.6496062992125976043, -0.5400638737290844871, 0.3530559997133364547 ) ) ;
#3617 = CARTESIAN_POINT ( 'NONE',  ( 1.509186351706037543, -0.4281496062992127816, -0.4176697321401328100 ) ) ;
#3618 = CARTESIAN_POINT ( 'NONE',  ( -0.3917322834645670104, -7.196005306013484475E-17, 0.03346456692913377107 ) ) ;
#3619 = CARTESIAN_POINT ( 'NONE',  ( 0.3346456692913390985, 0.1660481256975885056, 0.3530559997133364547 ) ) ;
#3620 = CARTESIAN_POINT ( 'NONE',  ( 0.1958661417322836440, -0.3392501089628017219, -2.288713910761154935 ) ) ;
#3621 = CARTESIAN_POINT ( 'NONE',  ( -1.489501312335957062, -0.08942795157527998196, 0.3641732283464567121 ) ) ;
#3622 = ORIENTED_EDGE ( 'NONE', *, *, #38964, .T. ) ;
#3623 = CARTESIAN_POINT ( 'NONE',  ( -0.1974969037888703871, -0.3420746716998661063, -2.585301837270341352 ) ) ;
#3624 = ORIENTED_EDGE ( 'NONE', *, *, #22798, .T. ) ;
#3625 = LINE ( 'NONE', #47809, #52958 ) ;
#3626 = CARTESIAN_POINT ( 'NONE',  ( -1.719160104986876103, 0.05413385826771666132, 0.4176697321401328100 ) ) ;
#3627 = CARTESIAN_POINT ( 'NONE',  ( 0.2925321140481932369, 0.2925321140481932369, -0.9251968503937008093 ) ) ;
#3628 = CARTESIAN_POINT ( 'NONE',  ( 1.436417322834643961, 0.4405861044731111953, 0.3149606299212599492 ) ) ;
#3629 = CARTESIAN_POINT ( 'NONE',  ( 0.1406185367545949305, 0.1377952755905511861, -1.409564117849439802 ) ) ;
#3630 = CARTESIAN_POINT ( 'NONE',  ( -1.010498687664041384, 0.05413385826771666132, 0.4176697321401328100 ) ) ;
#3631 = CARTESIAN_POINT ( 'NONE',  ( 0.08106202739151405212, -0.3841287887292352266, -2.755905511811023612 ) ) ;
#3632 = CARTESIAN_POINT ( 'NONE',  ( -9.594673741351313045E-17, 0.3917322834645670104, 0.07283464566929125084 ) ) ;
#3633 = CARTESIAN_POINT ( 'NONE',  ( -0.1837270341207340729, 0.1283753931104746893, -0.1820866141732285504 ) ) ;
#3634 = CARTESIAN_POINT ( 'NONE',  ( -1.069553805774277722, 0.1771653543307087630, 0.09757992244046791164 ) ) ;
#3635 = CARTESIAN_POINT ( 'NONE',  ( -1.404199475065615932, -0.4281496062992127816, -0.4176697321401328100 ) ) ;
#3636 = CARTESIAN_POINT ( 'NONE',  ( 0.4593175853018379162, -0.4281496062992124485, 0.4176697321401328655 ) ) ;
#3637 = CARTESIAN_POINT ( 'NONE',  ( -1.266404199475064773, -0.05778040916215560624, -0.4822834645669293319 ) ) ;
#3638 = CARTESIAN_POINT ( 'NONE',  ( -0.2867679344610365999, 0.2867679344610364889, -0.01181102362204719709 ) ) ;
#3639 = ORIENTED_EDGE ( 'NONE', *, *, #62545, .F. ) ;
#3640 = CARTESIAN_POINT ( 'NONE',  ( -1.207349081364828436, -0.6046776061558807314, 0.2411417322834647770 ) ) ;
#3641 = LINE ( 'NONE', #41930, #8427 ) ;
#3642 =( NAMED_UNIT ( * ) SI_UNIT ( $, .STERADIAN. ) SOLID_ANGLE_UNIT ( ) );
#3643 = AXIS2_PLACEMENT_3D ( 'NONE', #28529, #34855, #29357 ) ;
#3644 = CARTESIAN_POINT ( 'NONE',  ( -0.3458507752293909498, 0.3458507752293907833, -1.594488188976378229 ) ) ;
#3645 = CARTESIAN_POINT ( 'NONE',  ( 1.852066570651488719, 1.064797240280316748, -0.04222672046128581047 ) ) ;
#3646 = ADVANCED_FACE ( 'NONE', ( #63166 ), #27286, .F. ) ;
#3647 = CARTESIAN_POINT ( 'NONE',  ( -0.3917322834645670104, -7.196005306013484475E-17, -0.6614173228346454936 ) ) ;
#3648 = CIRCLE ( 'NONE', #27856, 0.09842519685039372024 ) ;
#3649 = LINE ( 'NONE', #62124, #47966 ) ;
#3650 = CARTESIAN_POINT ( 'NONE',  ( -0.9186351706036736120, -0.6046776061558809534, -0.2411417322834644161 ) ) ;
#3651 = CARTESIAN_POINT ( 'NONE',  ( 1.377952755905512472, 0.2952755905511811885, 0.000000000000000000 ) ) ;
#3652 = CONICAL_SURFACE ( 'NONE', #14421, 3.307086614173228689, 0.7853981633974500554 ) ;
#3653 = CIRCLE ( 'NONE', #62764, 1.122047244094488194 ) ;
#3655 = CARTESIAN_POINT ( 'NONE',  ( -0.1265901696524986964, -0.4724409448818899238, -1.961942257217847763 ) ) ;
#3654 = CARTESIAN_POINT ( 'NONE',  ( 0.01968503937007875723, 0.000000000000000000, 0.1968503937007874405 ) ) ;
#3656 = CARTESIAN_POINT ( 'NONE',  ( 1.515748031496063408, 0.1660481256975885056, 0.3530559997133364547 ) ) ;
#3657 = CARTESIAN_POINT ( 'NONE',  ( -0.8398950131233589023, -0.6046776061558809534, -0.2411417322834644161 ) ) ;
#3658 = CARTESIAN_POINT ( 'NONE',  ( -0.3917322834645669549, -7.196005306013483243E-17, 0.03807705856399132283 ) ) ;
#3659 = CARTESIAN_POINT ( 'NONE',  ( 0.2165354330708668673, 0.07958543189024071263, -0.2665933059059888421 ) ) ;
#3660 = CARTESIAN_POINT ( 'NONE',  ( 0.2867679344610366554, 0.2867679344610366554, -0.3799212598425197318 ) ) ;
#3661 = CARTESIAN_POINT ( 'NONE',  ( 0.03280839895013198948, -0.5511811023622048555, -0.09757992244046775898 ) ) ;
#3662 = CARTESIAN_POINT ( 'NONE',  ( 0.8398950131233602345, 0.1283753931104746893, -0.1820866141732285504 ) ) ;
#3663 = CARTESIAN_POINT ( 'NONE',  ( 0.7480314960629927956, -0.6692913385826771977, 8.415575281601705876E-17 ) ) ;
#3664 = CARTESIAN_POINT ( 'NONE',  ( -0.3805774278215216522, -0.004921259842519576551, 0.3153832671262227771 ) ) ;
#3665 = CARTESIAN_POINT ( 'NONE',  ( 0.3392501089628018884, -0.1958661417322834220, -2.459317585301837195 ) ) ;
#3666 = CARTESIAN_POINT ( 'NONE',  ( -1.555118110236219930, -0.5400638737290845981, -0.3530559997133363437 ) ) ;
#3667 = CARTESIAN_POINT ( 'NONE',  ( -1.174540682414697335, -0.08942795157527998196, 0.3641732283464567121 ) ) ;
#3668 = CARTESIAN_POINT ( 'NONE',  ( -0.4091458600556402980, -0.2362204724409451284, -0.9166666666666666297 ) ) ;
#3669 = CARTESIAN_POINT ( 'NONE',  ( 0.1115485564304467270, -0.6692913385826773087, -0.1292274648535924053 ) ) ;
#3670 = CARTESIAN_POINT ( 'NONE',  ( -0.5643044619422565855, -0.4281496062992124485, 0.4176697321401328655 ) ) ;
#3671 = CYLINDRICAL_SURFACE ( 'NONE', #57254, 0.3129921259842520787 ) ;
#3672 = CARTESIAN_POINT ( 'NONE',  ( 0.4527559055118117182, -0.4536011799217367080, 0.2665933059059888421 ) ) ;
#3673 = CARTESIAN_POINT ( 'NONE',  ( -0.2952755905511804668, 0.1660481256975885056, 0.3530559997133364547 ) ) ;
#3674 = CARTESIAN_POINT ( 'NONE',  ( -0.7677165354330699465, -0.5400638737290845981, -0.3530559997133363437 ) ) ;
#3675 = CARTESIAN_POINT ( 'NONE',  ( -1.604771003085129433, 2.146987379487327985, 0.1466069496707750608 ) ) ;
#3676 = CARTESIAN_POINT ( 'NONE',  ( -3.900966923095589678, 2.755905511811024056, -0.5314960629921260393 ) ) ;
#3677 = CARTESIAN_POINT ( 'NONE',  ( 0.06561679790026316017, -0.4281496062992124485, 0.4176697321401328655 ) ) ;
#3678 = CARTESIAN_POINT ( 'NONE',  ( -0.3460692066303960313, 0.1998031496062989965, -1.677821522309711266 ) ) ;
#3679 = DIRECTION ( 'NONE',  ( -0.000000000000000000, 1.000000000000000000, -0.000000000000000000 ) ) ;
#3680 = CARTESIAN_POINT ( 'NONE',  ( -0.05905511811023545637, -0.4536011799217368745, -0.2665933059059886201 ) ) ;
#3681 = CARTESIAN_POINT ( 'NONE',  ( -0.3937007874015740483, -0.1870078740157480879, -0.4822834645669291653 ) ) ;
#3682 = CARTESIAN_POINT ( 'NONE',  ( -1.594488188976377119, 0.07958543189024071263, -0.2665933059059888421 ) ) ;
#3683 = CARTESIAN_POINT ( 'NONE',  ( 1.154855643044620184, -0.6046776061558807314, 0.2411417322834647770 ) ) ;
#3684 = CARTESIAN_POINT ( 'NONE',  ( -1.469816272965878357, 0.2306618581243848609, 0.2411417322834645549 ) ) ;
#3685 = CARTESIAN_POINT ( 'NONE',  ( -0.8267716535433065062, -0.5511811023622047445, 6.969142054262312111E-17 ) ) ;
#3686 = CARTESIAN_POINT ( 'NONE',  ( 0.3996062992125984925, 0.1070741851644054499, -0.2014435695538057958 ) ) ;
#3687 = CARTESIAN_POINT ( 'NONE',  ( 0.2925321140481932369, -0.2925321140481932369, -0.7283464566929134243 ) ) ;
#3688 = CARTESIAN_POINT ( 'NONE',  ( -0.3917322834645671770, 0.1049643490035302024, -2.864192544128295825 ) ) ;
#3689 = CARTESIAN_POINT ( 'NONE',  ( 1.673228346456693494, 0.07958543189024085140, 0.2665933059059887866 ) ) ;
#3690 = CARTESIAN_POINT ( 'NONE',  ( 1.181102362204724976, -0.1870078740157480601, -0.3641732283464567677 ) ) ;
#3691 = CARTESIAN_POINT ( 'NONE',  ( 0.9776902887139113929, 0.2952755905511811885, 0.1292274648535926551 ) ) ;
#3692 = CARTESIAN_POINT ( 'NONE',  ( -1.541994750656167090, 0.2952755905511811885, 0.1292274648535926551 ) ) ;
#3693 = CARTESIAN_POINT ( 'NONE',  ( 0.7545931758530188826, -0.6692913385826771977, 0.1292274648535927661 ) ) ;
#3694 = CARTESIAN_POINT ( 'NONE',  ( 0.1058382717557500852, -0.3949938075777408852, -0.7919947506561679784 ) ) ;
#3695 = CARTESIAN_POINT ( 'NONE',  ( 1.181102362204725198, -0.1870078740157479769, 0.3641732283464567677 ) ) ;
#3696 = CARTESIAN_POINT ( 'NONE',  ( -0.01968503937007793844, 0.1660481256975883668, -0.3530559997133364547 ) ) ;
#3697 = CARTESIAN_POINT ( 'NONE',  ( -0.7611548556430438595, -0.6046776061558809534, -0.2411417322834644161 ) ) ;
#3698 = CARTESIAN_POINT ( 'NONE',  ( -3.908814775713581824, 1.601606672327087644, 0.4703198478456566689 ) ) ;
#3699 = VECTOR ( 'NONE', #46610, 39.37007874015748143 ) ;
#3700 = CARTESIAN_POINT ( 'NONE',  ( -0.2362204724409451284, 0.4091458600556402425, -1.272965879265091749 ) ) ;
#3701 = CIRCLE ( 'NONE', #66860, 0.3051181102362204856 ) ;
#3702 = CARTESIAN_POINT ( 'NONE',  ( -0.3460692066303960868, 0.1998031496062990242, -2.388451443569553856 ) ) ;
#3703 = CARTESIAN_POINT ( 'NONE',  ( 0.3215223097112867578, -0.08942795157527998196, 0.3641732283464567121 ) ) ;
#3704 = ORIENTED_EDGE ( 'NONE', *, *, #54370, .F. ) ;
#3705 = CARTESIAN_POINT ( 'NONE',  ( -9.594673741351313045E-17, 0.3917322834645670659, -0.7841400506899758316 ) ) ;
#3706 = VERTEX_POINT ( 'NONE', #49014 ) ;
#3707 = CARTESIAN_POINT ( 'NONE',  ( -0.5577427821522301654, -0.05778040916215560624, -0.4822834645669293319 ) ) ;
#3708 = CARTESIAN_POINT ( 'NONE',  ( -0.1706036745406816491, 0.05413385826771626580, -0.4176697321401330321 ) ) ;
#3709 = CARTESIAN_POINT ( 'NONE',  ( -0.1640419947506553400, -0.05778040916215560624, -0.4822834645669293319 ) ) ;
#3710 = CARTESIAN_POINT ( 'NONE',  ( 0.8005249343832028242, -0.4281496062992127816, -0.4176697321401328100 ) ) ;
#3711 = CARTESIAN_POINT ( 'NONE',  ( -0.8595800524934373854, -0.05778040916215522460, 0.4822834645669289988 ) ) ;
#3712 = CARTESIAN_POINT ( 'NONE',  ( -0.4855643044619415427, -0.4281496062992124485, 0.4176697321401328655 ) ) ;
#3713 = CARTESIAN_POINT ( 'NONE',  ( 1.279527559055118724, 0.1660481256975885056, 0.3530559997133364547 ) ) ;
#3714 = CARTESIAN_POINT ( 'NONE',  ( 0.3346456692913390985, 0.1660481256975885056, 0.3530559997133364547 ) ) ;
#3715 = CARTESIAN_POINT ( 'NONE',  ( 0.6561679790026253567, -0.6046776061558809534, -0.2411417322834644161 ) ) ;
#3716 = CARTESIAN_POINT ( 'NONE',  ( -0.1958661417322836718, 0.3392501089628017219, -0.9501312335958004285 ) ) ;
#3717 = CARTESIAN_POINT ( 'NONE',  ( 0.1049868766404206816, 0.1283753931104748280, 0.1820866141732283561 ) ) ;
#3718 = ORIENTED_EDGE ( 'NONE', *, *, #15170, .T. ) ;
#3719 = CARTESIAN_POINT ( 'NONE',  ( -0.1974969037888706647, 0.3420746716998658843, -0.9580052493438320216 ) ) ;
#3720 = ORIENTED_EDGE ( 'NONE', *, *, #78379, .T. ) ;
#3721 = CARTESIAN_POINT ( 'NONE',  ( -0.8070866141732276899, -0.4536011799217367080, 0.2665933059059888421 ) ) ;
#3722 = CARTESIAN_POINT ( 'NONE',  ( -0.4002624671916004129, -0.3162353388693405765, 0.4822834645669290543 ) ) ;
#3723 = CARTESIAN_POINT ( 'NONE',  ( 0.7767023820430452030, 2.575861430505332611E-15, -0.4118477457932988584 ) ) ;
#3724 = CARTESIAN_POINT ( 'NONE',  ( -0.5511811023622041894, -0.1870078740157480879, -0.4822834645669291653 ) ) ;
#3725 = CARTESIAN_POINT ( 'NONE',  ( -0.2427821522309703550, -0.05778040916215560624, -0.4822834645669293319 ) ) ;
#3726 = CARTESIAN_POINT ( 'NONE',  ( -1.246719160104985846, -0.4281496062992127816, -0.4176697321401328100 ) ) ;
#3727 = CARTESIAN_POINT ( 'NONE',  ( -1.541994750656167090, 0.2952755905511811885, 0.1292274648535926551 ) ) ;
#3728 = CARTESIAN_POINT ( 'NONE',  ( 1.076115485564305141, 0.1283753931104746893, -0.1820866141732285504 ) ) ;
#3729 = LINE ( 'NONE', #15961, #52508 ) ;
#3730 = CARTESIAN_POINT ( 'NONE',  ( 0.2952755905511811885, 0.01200600163628318291, 5.879133660591329580 ) ) ;
#3731 = CARTESIAN_POINT ( 'NONE',  ( 0.6233595800524939223, -0.2845877964562159024, 0.3641732283464567677 ) ) ;
#3732 = CARTESIAN_POINT ( 'NONE',  ( 0.1115485564304470323, 0.2952755905511811885, 0.1292274648535926551 ) ) ;
#3733 = CARTESIAN_POINT ( 'NONE',  ( -0.2230971128608915943, 0.05413385826771666132, 0.4176697321401328100 ) ) ;
#3734 = ORIENTED_EDGE ( 'NONE', *, *, #76855, .F. ) ;
#3735 = CARTESIAN_POINT ( 'NONE',  ( -0.2925321140481932924, 0.2925321140481931814, -1.751968503937007648 ) ) ;
#3736 = DIRECTION ( 'NONE',  ( 0.000000000000000000, 0.000000000000000000, -1.000000000000000000 ) ) ;
#3737 = ORIENTED_EDGE ( 'NONE', *, *, #58775, .T. ) ;
#3738 = CARTESIAN_POINT ( 'NONE',  ( 0.1070741851644054776, -0.3996062992125984925, -1.106955380577427706 ) ) ;
#3739 = CARTESIAN_POINT ( 'NONE',  ( 0.000000000000000000, 1.724409448818897461, 0.000000000000000000 ) ) ;
#3740 = CARTESIAN_POINT ( 'NONE',  ( -0.6496062992125976043, -0.4536011799217367080, 0.2665933059059888421 ) ) ;
#3741 = CARTESIAN_POINT ( 'NONE',  ( -0.7742782152230965886, 0.05413385826771666132, 0.4176697321401328100 ) ) ;
#3742 = CARTESIAN_POINT ( 'NONE',  ( 0.4724409448818898682, 2.892866454678787531E-17, -0.4330708661417322913 ) ) ;
#3743 = CARTESIAN_POINT ( 'NONE',  ( 4.797336870675656522E-17, -0.3917322834645670104, -2.683070866141731958 ) ) ;
#3744 = CARTESIAN_POINT ( 'NONE',  ( 1.620734908136483465, -0.6692913385826771977, 0.1292274648535927661 ) ) ;
#3745 = CARTESIAN_POINT ( 'NONE',  ( 0.4921259842519691285, 0.1660481256975885056, 0.3530559997133364547 ) ) ;
#3746 = CARTESIAN_POINT ( 'NONE',  ( 0.5511811023622055217, -0.1870078740157479769, 0.4822834645669291653 ) ) ;
#3747 = CARTESIAN_POINT ( 'NONE',  ( -0.7480314960629914633, -0.5511811023622047445, 6.969142054262312111E-17 ) ) ;
#3748 = CARTESIAN_POINT ( 'NONE',  ( 0.2690288713910767848, -0.6692913385826773087, -0.1292274648535924053 ) ) ;
#3749 = CARTESIAN_POINT ( 'NONE',  ( -1.157146581871515012E-16, 0.4724409448818898682, -2.438976377952756014 ) ) ;
#3750 = CARTESIAN_POINT ( 'NONE',  ( -0.6167979002624665030, 0.05413385826771666132, 0.4176697321401328100 ) ) ;
#3751 = CARTESIAN_POINT ( 'NONE',  ( 0.3420746716998660508, 0.1974969037888705814, -1.782808398950131101 ) ) ;
#3752 = CARTESIAN_POINT ( 'NONE',  ( 1.272965879265092637, -0.004921259842519576551, 0.3153832671262227771 ) ) ;
#3753 = CARTESIAN_POINT ( 'NONE',  ( 0.1902887139107617975, 0.1771653543307087630, 0.09757992244046791164 ) ) ;
#3754 = CARTESIAN_POINT ( 'NONE',  ( 1.233595800524935227, 0.1283753931104746893, -0.1820866141732285504 ) ) ;
#3755 = CARTESIAN_POINT ( 'NONE',  ( -0.9580052493438311334, -0.4281496062992124485, 0.4176697321401328655 ) ) ;
#3756 = CARTESIAN_POINT ( 'NONE',  ( -0.5249343832020990641, 0.1283753931104748280, 0.1820866141732283561 ) ) ;
#3757 = CARTESIAN_POINT ( 'NONE',  ( -3.184294706754630777, 2.755905511811024056, -0.5314960629921260393 ) ) ;
#3758 = CARTESIAN_POINT ( 'NONE',  ( -1.174540682414697335, -0.3162353388693409650, -0.4822834645669289433 ) ) ;
#3759 = CARTESIAN_POINT ( 'NONE',  ( -0.6167979002624665030, -0.4281496062992127816, -0.4176697321401328100 ) ) ;
#3760 = CARTESIAN_POINT ( 'NONE',  ( 0.1837270341207357105, -0.6046776061558809534, -0.2411417322834644161 ) ) ;
#3762 = CARTESIAN_POINT ( 'NONE',  ( 0.1049643490035304522, -0.3917322834645668994, -2.527539739336271296 ) ) ;
#3761 = CIRCLE ( 'NONE', #13197, 1.122047244094488194 ) ;
#3763 = CARTESIAN_POINT ( 'NONE',  ( -1.854728618660363759, 1.067671560069311854, -0.06860298820093484184 ) ) ;
#3764 = CARTESIAN_POINT ( 'NONE',  ( 0.3674540682414705883, -0.5023911411419708095, 0.1820866141732285504 ) ) ;
#3765 = CARTESIAN_POINT ( 'NONE',  ( 1.036745406824147508, -0.4281496062992127816, -0.4176697321401328100 ) ) ;
#3766 = CARTESIAN_POINT ( 'NONE',  ( 0.4724409448818897017, 0.1265901696524990294, -0.9888451443569553634 ) ) ;
#3767 = CARTESIAN_POINT ( 'NONE',  ( 0.8530183727034128527, -0.4281496062992124485, 0.4176697321401328655 ) ) ;
#3768 = CARTESIAN_POINT ( 'NONE',  ( -1.437007874015747477, -0.4536011799217367080, 0.2665933059059888421 ) ) ;
#3769 = CARTESIAN_POINT ( 'NONE',  ( -1.614173228346456268, -0.6692913385826771977, 8.415575281601705876E-17 ) ) ;
#3770 = CARTESIAN_POINT ( 'NONE',  ( -1.017060367454067249, -0.3162353388693409650, -0.4822834645669289433 ) ) ;
#3771 = CARTESIAN_POINT ( 'NONE',  ( -0.01312335958005186876, -0.004921259842519870586, -0.3153832671262229437 ) ) ;
#3772 = FACE_OUTER_BOUND ( 'NONE', #65740, .T. ) ;
#3773 = CARTESIAN_POINT ( 'NONE',  ( 0.8136482939632553313, 0.1283753931104748280, 0.1820866141732283561 ) ) ;
#3774 = EDGE_CURVE ( 'NONE', #41297, #24318, #70174, .T. ) ;
#3775 = CARTESIAN_POINT ( 'NONE',  ( 8.195543980992789655E-16, -0.1870078740157480879, -0.4822834645669291653 ) ) ;
#3776 = CARTESIAN_POINT ( 'NONE',  ( -0.1998031496062991630, -0.3460692066303959202, -0.2998687664041995160 ) ) ;
#3777 = EDGE_CURVE ( 'NONE', #24500, #32357, #56713, .T. ) ;
#3778 = CARTESIAN_POINT ( 'NONE',  ( -1.292650918635170010, -0.6692913385826771977, 0.1292274648535927661 ) ) ;
#3779 = CARTESIAN_POINT ( 'NONE',  ( 0.3392501089628018329, 0.1958661417322835607, -1.633202099737532942 ) ) ;
#3780 = CARTESIAN_POINT ( 'NONE',  ( 0.8661417322834652488, -0.1870078740157480601, -0.3641732283464567677 ) ) ;
#3781 = CARTESIAN_POINT ( 'NONE',  ( 0.1312335958005257930, 0.2306618581243847221, -0.2411417322834647770 ) ) ;
#3782 = CARTESIAN_POINT ( 'NONE',  ( -0.2624671916010490880, -0.6046776061558807314, 0.2411417322834647770 ) ) ;
#3783 = CARTESIAN_POINT ( 'NONE',  ( -0.2034120734908128059, 0.1771653543307087630, 0.09757992244046791164 ) ) ;
#3784 = LINE ( 'NONE', #16843, #18536 ) ;
#3785 = CARTESIAN_POINT ( 'NONE',  ( -0.3346456692913377662, 0.07958543189024071263, -0.2665933059059888421 ) ) ;
#3786 = CARTESIAN_POINT ( 'NONE',  ( 0.3477690288713918276, -0.6692913385826773087, -0.1292274648535924053 ) ) ;
#3787 = CARTESIAN_POINT ( 'NONE',  ( -1.272965879265091305, -0.3690944881889763329, 0.3153832671262228327 ) ) ;
#3788 = CARTESIAN_POINT ( 'NONE',  ( 0.3460692066303959202, -0.1998031496062991630, -1.441601049868766582 ) ) ;
#3789 = CARTESIAN_POINT ( 'NONE',  ( -1.568241469816272105, -0.3162353388693409650, -0.4822834645669289433 ) ) ;
#3790 = CARTESIAN_POINT ( 'NONE',  ( -2.543486866223389153, 2.716535433070866645, 0.5314960629921260393 ) ) ;
#3791 = ORIENTED_EDGE ( 'NONE', *, *, #67416, .F. ) ;
#3792 = CARTESIAN_POINT ( 'NONE',  ( -1.535433070866141225, 0.1771653543307087630, 0.000000000000000000 ) ) ;
#3793 = CARTESIAN_POINT ( 'NONE',  ( -0.3871391076115479057, -0.3162353388693409650, -0.4822834645669289433 ) ) ;
#3794 = CARTESIAN_POINT ( 'NONE',  ( -1.128608923884513837, 0.2306618581243847221, -0.2411417322834647770 ) ) ;
#3795 = CARTESIAN_POINT ( 'NONE',  ( 0.2867679344610365999, 0.2867679344610365999, -1.639763779527558807 ) ) ;
#3796 = LINE ( 'NONE', #60621, #21602 ) ;
#3797 = EDGE_CURVE ( 'NONE', #65491, #44566, #56560, .T. ) ;
#3798 = CARTESIAN_POINT ( 'NONE',  ( 1.535433070866142558, 0.2952755905511811885, 0.000000000000000000 ) ) ;
#3799 = CARTESIAN_POINT ( 'NONE',  ( 0.6233595800524942554, -0.05778040916215560624, -0.4822834645669293319 ) ) ;
#3800 = CARTESIAN_POINT ( 'NONE',  ( -0.3307086614173228023, -0.3242060844882008741, 0.000000000000000000 ) ) ;
#3801 = CARTESIAN_POINT ( 'NONE',  ( 0.3460692066303958092, 0.1998031496062993018, -2.412729658792650778 ) ) ;
#3802 = EDGE_CURVE ( 'NONE', #17115, #33549, #49990, .T. ) ;
#3803 = CARTESIAN_POINT ( 'NONE',  ( 1.614173228346457378, 0.1771653543307087630, 0.000000000000000000 ) ) ;
#3804 = CARTESIAN_POINT ( 'NONE',  ( 0.2925321140481932369, 0.2925321140481932369, -0.6102362204724409711 ) ) ;
#3805 = ORIENTED_EDGE ( 'NONE', *, *, #36169, .T. ) ;
#3806 = CARTESIAN_POINT ( 'NONE',  ( -0.8923884514435688198, -0.5023911411419708095, 0.1820866141732285504 ) ) ;
#3807 = CARTESIAN_POINT ( 'NONE',  ( 0.3392501089628018884, -0.1958661417322834220, -2.301837270341207553 ) ) ;
#3808 = ORIENTED_EDGE ( 'NONE', *, *, #17740, .F. ) ;
#3809 = CARTESIAN_POINT ( 'NONE',  ( 0.7939632545931766261, -0.05778040916215522460, 0.4822834645669289988 ) ) ;
#3810 = CARTESIAN_POINT ( 'NONE',  ( -0.3608923884514428360, -0.6692913385826773087, -0.1292274648535924053 ) ) ;
#3811 = CARTESIAN_POINT ( 'NONE',  ( -1.305774278215222184, 0.2952755905511811885, 0.1292274648535926551 ) ) ;
#3812 = CARTESIAN_POINT ( 'NONE',  ( 1.207349081364829990, 0.2306618581243848609, 0.2411417322834645549 ) ) ;
#3813 = CARTESIAN_POINT ( 'NONE',  ( -1.213910761154854745, -0.5511811023622046335, 0.09757992244046803654 ) ) ;
#3814 = CARTESIAN_POINT ( 'NONE',  ( 0.4724409448818898682, 2.892866454678787531E-17, -0.5905511811023621549 ) ) ;
#3815 = CARTESIAN_POINT ( 'NONE',  ( 0.1968503937007881344, -0.6692913385826771977, 8.415575281601705876E-17 ) ) ;
#3816 = CARTESIAN_POINT ( 'NONE',  ( -0.7152230971128602510, -0.3162353388693405765, 0.4822834645669290543 ) ) ;
#3817 = CARTESIAN_POINT ( 'NONE',  ( -0.1958661417322836440, 0.3392501089628016664, -1.667959686842832356 ) ) ;
#3818 = CARTESIAN_POINT ( 'NONE',  ( -1.056430446194224881, -0.6692913385826771977, 0.1292274648535927661 ) ) ;
#3819 = CARTESIAN_POINT ( 'NONE',  ( 0.4102808022082889416, 1.299212598425196985, -1.382164990278189398 ) ) ;
#3820 = CARTESIAN_POINT ( 'NONE',  ( 0.9383202099737538715, -0.05778040916215560624, -0.4822834645669293319 ) ) ;
#3821 = CARTESIAN_POINT ( 'NONE',  ( -0.2867679344610365999, 0.2867679344610364889, -2.624015748031495399 ) ) ;
#3822 = CARTESIAN_POINT ( 'NONE',  ( 1.246719160104987623, -0.004921259842519870586, -0.3153832671262229437 ) ) ;
#3823 = ORIENTED_EDGE ( 'NONE', *, *, #26568, .T. ) ;
#3824 = CARTESIAN_POINT ( 'NONE',  ( 0.1049643490035303967, 0.3917322834645670659, -2.824822465388138415 ) ) ;
#3825 = CARTESIAN_POINT ( 'NONE',  ( -0.3871391076115476282, -0.05778040916215522460, 0.4822834645669289988 ) ) ;
#3826 = ORIENTED_EDGE ( 'NONE', *, *, #68575, .T. ) ;
#3827 = VECTOR ( 'NONE', #51170, 39.37007874015748143 ) ;
#3828 = CARTESIAN_POINT ( 'NONE',  ( 0.3083989501312343062, -0.2845877964562159024, 0.3641732283464567677 ) ) ;
#3829 = CARTESIAN_POINT ( 'NONE',  ( -1.673228346456691717, 0.1660481256975883668, -0.3530559997133364547 ) ) ;
#3830 = CARTESIAN_POINT ( 'NONE',  ( 0.6627296587926515548, 0.2952755905511811885, 0.1292274648535926551 ) ) ;
#3831 = CARTESIAN_POINT ( 'NONE',  ( 0.7611548556430451917, -0.6046776061558807314, 0.2411417322834647770 ) ) ;
#3832 = CARTESIAN_POINT ( 'NONE',  ( -0.1443569553805768291, 0.05413385826771666132, 0.4176697321401328100 ) ) ;
#3833 = CARTESIAN_POINT ( 'NONE',  ( -0.3392501089628019995, 0.1958661417322831999, -1.282827714731970215 ) ) ;
#3834 = CARTESIAN_POINT ( 'NONE',  ( -0.9448818897637790704, -0.1870078740157480879, -0.4822834645669291653 ) ) ;
#3835 = CARTESIAN_POINT ( 'NONE',  ( 0.3392501089628018329, 0.1958661417322835607, -2.263123359580052618 ) ) ;
#3836 = CARTESIAN_POINT ( 'NONE',  ( -1.535433070866141225, 0.2952755905511811885, 0.000000000000000000 ) ) ;
#3837 = CARTESIAN_POINT ( 'NONE',  ( -1.076115485564303809, -0.6046776061558809534, -0.2411417322834644161 ) ) ;
#3838 = CARTESIAN_POINT ( 'NONE',  ( 1.115485564304462551, -0.4281496062992127816, -0.4176697321401328100 ) ) ;
#3839 = CARTESIAN_POINT ( 'NONE',  ( 1.587926509186352586, -0.4281496062992127816, -0.4176697321401328100 ) ) ;
#3840 = CARTESIAN_POINT ( 'NONE',  ( -0.3996062992125986035, -0.1070741851644056997, -0.3608923884514435576 ) ) ;
#3841 = CARTESIAN_POINT ( 'NONE',  ( -1.069553805774277722, 0.2952755905511811885, 0.1292274648535926551 ) ) ;
#3842 = CARTESIAN_POINT ( 'NONE',  ( -0.3996062992125984925, -0.1070741851644056858, 0.03477690288713909672 ) ) ;
#3843 = CARTESIAN_POINT ( 'NONE',  ( 0.1968503937007881344, 0.2952755905511811885, 0.000000000000000000 ) ) ;
#3844 = CARTESIAN_POINT ( 'NONE',  ( 0.3460692066303959202, 0.1998031496062993295, -2.178477690288713742 ) ) ;
#3845 = CARTESIAN_POINT ( 'NONE',  ( -0.4265091863517051496, -0.6692913385826771977, 0.1292274648535927661 ) ) ;
#3846 = CARTESIAN_POINT ( 'NONE',  ( -1.633858267716534529, 0.07958543189024085140, 0.2665933059059887866 ) ) ;
#3847 = CARTESIAN_POINT ( 'NONE',  ( 0.7874015748031503170, -0.1870078740157480601, -0.3641732283464567677 ) ) ;
#3848 = CARTESIAN_POINT ( 'NONE',  ( 1.154855643044620184, 0.2306618581243847221, -0.2411417322834647770 ) ) ;
#3849 = CARTESIAN_POINT ( 'NONE',  ( 0.1265901696524990294, -0.4724409448818896462, -0.9494750656167976199 ) ) ;
#3850 = CARTESIAN_POINT ( 'NONE',  ( 0.5905511811023629321, 0.1771653543307087630, 0.000000000000000000 ) ) ;
#3851 = CARTESIAN_POINT ( 'NONE',  ( 0.7349081364829402885, -0.6046776061558809534, -0.2411417322834644161 ) ) ;
#3852 = CARTESIAN_POINT ( 'NONE',  ( -0.1058382717557503072, 0.3949938075777408852, -0.3982939632545932640 ) ) ;
#3853 = CARTESIAN_POINT ( 'NONE',  ( -0.5839895013123351797, 0.2952755905511810774, -0.1292274648535930714 ) ) ;
#3854 = CARTESIAN_POINT ( 'NONE',  ( -0.3492006680983059108, 0.3045572308828553565, -0.01849200668098333403 ) ) ;
#3855 = CARTESIAN_POINT ( 'NONE',  ( 1.345144356955381593, -0.2845877964562161244, -0.3641732283464567121 ) ) ;
#3856 = CARTESIAN_POINT ( 'NONE',  ( -0.7545931758530177724, 0.2952755905511811885, 0.1292274648535926551 ) ) ;
#3857 = CARTESIAN_POINT ( 'NONE',  ( 0.1443569553805781891, -0.4281496062992124485, 0.4176697321401328655 ) ) ;
#3858 = CARTESIAN_POINT ( 'NONE',  ( -1.141732283464566011, 0.2952755905511811885, 0.000000000000000000 ) ) ;
#3859 = CARTESIAN_POINT ( 'NONE',  ( -0.04593175853018302557, -0.6692913385826773087, -0.1292274648535924053 ) ) ;
#3860 = CARTESIAN_POINT ( 'NONE',  ( 0.3412073490813655186, -0.5023911411419708095, -0.1820866141732282451 ) ) ;
#3861 = CARTESIAN_POINT ( 'NONE',  ( -0.4682236582119034263, 1.459426199372924948, -1.019690296884233849 ) ) ;
#3862 = CARTESIAN_POINT ( 'NONE',  ( 0.1312335958005257930, 0.1283753931104746893, -0.1820866141732285504 ) ) ;
#3863 = CARTESIAN_POINT ( 'NONE',  ( 0.6758530183727039509, 0.1771653543307087075, -0.09757992244046823083 ) ) ;
#3864 = CARTESIAN_POINT ( 'NONE',  ( -1.627296587926508442, 0.2306618581243848609, 0.2411417322834645549 ) ) ;
#3865 = EDGE_CURVE ( 'NONE', #29791, #38771, #7201, .T. ) ;
#3866 = CARTESIAN_POINT ( 'NONE',  ( -0.3996062992125986590, 0.1070741851644051723, -1.211942257217847541 ) ) ;
#3867 = CARTESIAN_POINT ( 'NONE',  ( 0.7217847769028878924, 0.05413385826771666132, 0.4176697321401328100 ) ) ;
#3868 = CARTESIAN_POINT ( 'NONE',  ( 0.3917322834645670104, -0.1049643490035303411, -1.206036745406823707 ) ) ;
#3869 = CARTESIAN_POINT ( 'NONE',  ( 1.522309711286089939, 0.1283753931104748280, 0.1820866141732283561 ) ) ;
#3870 = CARTESIAN_POINT ( 'NONE',  ( -0.1988659768032651487, 0.3401783215957732143, 1.649893717844496181E-17 ) ) ;
#3871 = CARTESIAN_POINT ( 'NONE',  ( 0.1706036745406830368, -0.004921259842519576551, 0.3153832671262227771 ) ) ;
#3872 = CARTESIAN_POINT ( 'NONE',  ( 0.2296587926509192634, -0.3162353388693405765, 0.4822834645669290543 ) ) ;
#3873 = CARTESIAN_POINT ( 'NONE',  ( 1.456692913385827515, -0.5511811023622047445, 6.969142054262312111E-17 ) ) ;
#3874 = CARTESIAN_POINT ( 'NONE',  ( -1.253280839895012377, -0.08942795157527998196, 0.3641732283464567121 ) ) ;
#3875 = CARTESIAN_POINT ( 'NONE',  ( -1.430446194225721390, -0.4281496062992124485, 0.4176697321401328655 ) ) ;
#3876 = CARTESIAN_POINT ( 'NONE',  ( 0.2624671916010504757, 0.2306618581243848609, 0.2411417322834645549 ) ) ;
#3877 = CARTESIAN_POINT ( 'NONE',  ( 1.351706036745407680, 0.05413385826771666132, 0.4176697321401328100 ) ) ;
#3878 = CARTESIAN_POINT ( 'NONE',  ( 0.1265901696524989184, 0.4724409448818898127, -0.2276902887139107545 ) ) ;
#3879 = CARTESIAN_POINT ( 'NONE',  ( 0.04593175853018440641, 0.2952755905511810774, -0.1292274648535930714 ) ) ;
#3880 = CARTESIAN_POINT ( 'NONE',  ( 1.318897637795276356, -0.5400638737290844871, 0.3530559997133364547 ) ) ;
#3881 = CARTESIAN_POINT ( 'NONE',  ( 0.9383202099737538715, -0.05778040916215560624, -0.4822834645669293319 ) ) ;
#3882 = CARTESIAN_POINT ( 'NONE',  ( 0.000000000000000000, 2.755905511811024056, 0.000000000000000000 ) ) ;
#3883 = CARTESIAN_POINT ( 'NONE',  ( 0.8530183727034128527, -0.3690944881889763329, 0.3153832671262228327 ) ) ;
#3884 = CARTESIAN_POINT ( 'NONE',  ( 1.528871391076116026, 0.2952755905511811885, 0.1292274648535926551 ) ) ;
#3885 = CARTESIAN_POINT ( 'NONE',  ( -0.01312335958005186876, -0.3690944881889763329, 0.3153832671262228327 ) ) ;
#3886 = CARTESIAN_POINT ( 'NONE',  ( 0.2887139107611556010, 0.2306618581243847221, -0.2411417322834647770 ) ) ;
#3887 = CARTESIAN_POINT ( 'NONE',  ( 0.7874015748031503170, -0.1870078740157479769, 0.4822834645669291653 ) ) ;
#3888 = CARTESIAN_POINT ( 'NONE',  ( -0.5249343832020990641, 0.2306618581243848609, 0.2411417322834645549 ) ) ;
#3889 = CARTESIAN_POINT ( 'NONE',  ( 0.1049643490035303967, 0.3917322834645670659, -2.194901205545618961 ) ) ;
#3890 = CARTESIAN_POINT ( 'NONE',  ( -0.07217847769028813698, -0.2845877964562161244, -0.3641732283464567121 ) ) ;
#3891 = CARTESIAN_POINT ( 'NONE',  ( 0.6430446194225728496, 0.05413385826771666132, 0.4176697321401328100 ) ) ;
#3892 = CARTESIAN_POINT ( 'NONE',  ( 1.089238845144357759, -0.004921259842519870586, -0.3153832671262229437 ) ) ;
#3893 = EDGE_CURVE ( 'NONE', #60217, #66675, #29271, .T. ) ;
#3894 = CARTESIAN_POINT ( 'NONE',  ( 0.000000000000000000, 0.000000000000000000, 0.1574803149606299191 ) ) ;
#3896 = CARTESIAN_POINT ( 'NONE',  ( -0.1070741851644057135, 0.3996062992125985480, -1.108923884514435798 ) ) ;
#3895 = DIRECTION ( 'NONE',  ( 0.000000000000000000, -1.000000000000000000, 0.000000000000000000 ) ) ;
#3897 = CARTESIAN_POINT ( 'NONE',  ( 2.130163876374006282, 1.668131542012052826, -0.4562955581495580781 ) ) ;
#3898 = CARTESIAN_POINT ( 'NONE',  ( -1.371391076115484609, -0.6692913385826771977, 0.1292274648535927661 ) ) ;
#3899 = CARTESIAN_POINT ( 'NONE',  ( -0.4855643044619415427, -0.4281496062992124485, 0.4176697321401328655 ) ) ;
#3900 = CARTESIAN_POINT ( 'NONE',  ( 0.1070741851644054915, -0.3996062992125986035, -2.919947506561679784 ) ) ;
#3901 = CARTESIAN_POINT ( 'NONE',  ( -9.674558042662121740E-17, 0.3949938075777409963, -2.204724409448819422 ) ) ;
#3902 = ORIENTED_EDGE ( 'NONE', *, *, #31743, .F. ) ;
#3903 = CARTESIAN_POINT ( 'NONE',  ( 0.2624671916010504757, 0.1283753931104748280, 0.1820866141732283561 ) ) ;
#3904 = CARTESIAN_POINT ( 'NONE',  ( -0.3392501089628019995, 0.1958661417322832277, -0.8057742782152230721 ) ) ;
#3905 = CARTESIAN_POINT ( 'NONE',  ( 1.062992125984252745, -0.6692913385826771977, 8.415575281601705876E-17 ) ) ;
#3906 = CARTESIAN_POINT ( 'NONE',  ( 0.4724409448818896462, 0.1265901696524990294, -2.329396325459317296 ) ) ;
#3907 = PLANE ( 'NONE',  #56060 ) ;
#3908 = CARTESIAN_POINT ( 'NONE',  ( 0.5314960629921371416, 2.729659904327171205, -3.210901138312280523 ) ) ;
#3909 = CARTESIAN_POINT ( 'NONE',  ( 1.574803149606299746, -0.1870078740157480879, -0.4822834645669291653 ) ) ;
#3910 = CARTESIAN_POINT ( 'NONE',  ( 1.391076115485564868, -0.5023911411419708095, 0.1820866141732285504 ) ) ;
#3911 = CARTESIAN_POINT ( 'NONE',  ( 0.2362204724409456558, -0.1870078740157479769, 0.4822834645669291653 ) ) ;
#3912 = CARTESIAN_POINT ( 'NONE',  ( 0.1958661417322834497, 0.3392501089628018329, -0.3818704479976884336 ) ) ;
#3913 = CARTESIAN_POINT ( 'NONE',  ( 0.05249343832021075018, -0.6046776061558807314, 0.2411417322834647770 ) ) ;
#3914 = CARTESIAN_POINT ( 'NONE',  ( -0.9186351706036736120, 0.1283753931104748280, 0.1820866141732283561 ) ) ;
#3915 = CARTESIAN_POINT ( 'NONE',  ( 0.3543307086614179147, 0.2952755905511811885, 0.000000000000000000 ) ) ;
#3916 = CARTESIAN_POINT ( 'NONE',  ( -0.02624671916010428221, -0.6046776061558807314, 0.2411417322834647770 ) ) ;
#3917 = CARTESIAN_POINT ( 'NONE',  ( 1.220472440944881942, 0.8346805926620878280, -0.5309055118110238558 ) ) ;
#3918 = CARTESIAN_POINT ( 'NONE',  ( 0.3996062992125986035, 0.1070741851644054776, -2.801837270341207553 ) ) ;
#3919 = CARTESIAN_POINT ( 'NONE',  ( 0.3917322834645670104, 0.1049643490035304660, -1.696213541503623912 ) ) ;
#3920 = CARTESIAN_POINT ( 'NONE',  ( 0.7939632545931766261, -0.3162353388693409650, -0.4822834645669289433 ) ) ;
#3921 = CARTESIAN_POINT ( 'NONE',  ( -0.1706036745406816491, -0.4281496062992124485, 0.4176697321401328655 ) ) ;
#3922 = CARTESIAN_POINT ( 'NONE',  ( -1.174540682414697335, -0.05778040916215522460, 0.4822834645669289988 ) ) ;
#3923 = VECTOR ( 'NONE', #23902, 39.37007874015748143 ) ;
#3924 = EDGE_CURVE ( 'NONE', #65725, #23851, #35905, .T. ) ;
#3925 = CARTESIAN_POINT ( 'NONE',  ( 1.102362204724410155, -0.1870078740157479769, 0.4822834645669291653 ) ) ;
#3926 = CARTESIAN_POINT ( 'NONE',  ( 0.6496062992125991586, -0.5400638737290845981, -0.3530559997133363437 ) ) ;
#3927 = CARTESIAN_POINT ( 'NONE',  ( -0.1049643490035302024, -0.3917322834645671215, -0.9442257217847768169 ) ) ;
#3928 = CARTESIAN_POINT ( 'NONE',  ( -0.5643044619422565855, 0.05413385826771626580, -0.4176697321401330321 ) ) ;
#3929 = CARTESIAN_POINT ( 'NONE',  ( 0.2624671916010504757, 0.2306618581243848609, 0.2411417322834645549 ) ) ;
#3930 = CARTESIAN_POINT ( 'NONE',  ( -0.2493438320209966919, -0.4281496062992124485, 0.4176697321401328655 ) ) ;
#3931 = EDGE_CURVE ( 'NONE', #8463, #50964, #10215, .T. ) ;
#3932 = CARTESIAN_POINT ( 'NONE',  ( 0.1771653543307093182, -0.4536011799217368745, -0.2665933059059886201 ) ) ;
#3933 = CARTESIAN_POINT ( 'NONE',  ( 1.679790026246720025, 0.1283753931104748280, 0.1820866141732283561 ) ) ;
#3934 = DIRECTION ( 'NONE',  ( -0.000000000000000000, -1.000000000000000000, 0.000000000000000000 ) ) ;
#3935 = CARTESIAN_POINT ( 'NONE',  ( 0.2296587926509192634, -0.05778040916215560624, -0.4822834645669293319 ) ) ;
#3936 = FILL_AREA_STYLE_COLOUR ( '', #47970 ) ;
#3937 = CARTESIAN_POINT ( 'NONE',  ( -1.561679790026246017, -0.4281496062992127816, -0.4176697321401328100 ) ) ;
#3938 = CARTESIAN_POINT ( 'NONE',  ( 0.1049643490035303689, 0.3917322834645670104, -2.347769028871391050 ) ) ;
#3939 = VERTEX_POINT ( 'NONE', #23651 ) ;
#3940 = ORIENTED_EDGE ( 'NONE', *, *, #47038, .T. ) ;
#3941 = CARTESIAN_POINT ( 'NONE',  ( 0.5052493438320218022, -0.6692913385826773087, -0.1292274648535924053 ) ) ;
#3942 = CARTESIAN_POINT ( 'NONE',  ( 0.4330708661417329575, -0.5511811023622047445, 6.969142054262312111E-17 ) ) ;
#3944 = DIRECTION ( 'NONE',  ( -1.000000000000000000, -3.083952846180990774E-16, 0.000000000000000000 ) ) ;
#3943 = FACE_OUTER_BOUND ( 'NONE', #54517, .T. ) ;
#3945 = CARTESIAN_POINT ( 'NONE',  ( -0.3917322834645671215, 0.1049643490035301469, -0.9048556430446195176 ) ) ;
#3946 = CARTESIAN_POINT ( 'NONE',  ( 0.1265901696524990294, -0.4724409448818896462, -0.004593175853018378711 ) ) ;
#3947 = CARTESIAN_POINT ( 'NONE',  ( 0.1998031496062992463, 0.3460692066303959202, -2.268372703412073310 ) ) ;
#3948 = CARTESIAN_POINT ( 'NONE',  ( 0.8661417322834652488, -0.1870078740157480879, -0.4822834645669291653 ) ) ;
#3949 = CARTESIAN_POINT ( 'NONE',  ( -0.6824146981627288167, 0.2306618581243848609, 0.2411417322834645549 ) ) ;
#3950 = CARTESIAN_POINT ( 'NONE',  ( -0.7086614173228339419, -0.1870078740157480879, -0.4822834645669291653 ) ) ;
#3951 = CARTESIAN_POINT ( 'NONE',  ( 0.4921259842519691285, 0.1660481256975885056, 0.3530559997133364547 ) ) ;
#3952 = CARTESIAN_POINT ( 'NONE',  ( 1.437007874015748810, 0.1660481256975885056, 0.3530559997133364547 ) ) ;
#3953 = CARTESIAN_POINT ( 'NONE',  ( 1.193875086542981023, 0.004960608223779470680, 0.3437734562760185741 ) ) ;
#3954 = CARTESIAN_POINT ( 'NONE',  ( 1.259842519685040019, -0.1870078740157480601, -0.3641732283464567677 ) ) ;
#3955 = DIRECTION ( 'NONE',  ( 0.000000000000000000, 1.000000000000000000, -8.673617379884024625E-16 ) ) ;
#3956 = CARTESIAN_POINT ( 'NONE',  ( -1.332020997375327642, -0.08942795157527998196, 0.3641732283464567121 ) ) ;
#3957 = CARTESIAN_POINT ( 'NONE',  ( -0.3917322834645671215, 0.1049643490035301469, -0.02493438320209968861 ) ) ;
#3958 = CARTESIAN_POINT ( 'NONE',  ( 0.3280839895013130669, -0.4281496062992127816, -0.4176697321401328100 ) ) ;
#3960 = CARTESIAN_POINT ( 'NONE',  ( 0.4606732211678803424, 1.778019097314518016, -0.5309055118110237448 ) ) ;
#3959 = CARTESIAN_POINT ( 'NONE',  ( 1.148293963254593875, -0.6692913385826771977, 0.1292274648535927661 ) ) ;
#3961 = CARTESIAN_POINT ( 'NONE',  ( -1.036745406824146176, -0.004921259842519870586, -0.3153832671262229437 ) ) ;
#3962 = CARTESIAN_POINT ( 'NONE',  ( 0.4396325459317593221, 0.2952755905511810774, -0.1292274648535930714 ) ) ;
#3963 = CARTESIAN_POINT ( 'NONE',  ( 1.122047244094488860, 0.07958543189024085140, 0.2665933059059887866 ) ) ;
#3964 = CARTESIAN_POINT ( 'NONE',  ( -0.3917322834645669549, -7.196005306013483243E-17, -1.694206406002937593 ) ) ;
#3965 = CARTESIAN_POINT ( 'NONE',  ( -1.312335958005248715, -0.5023911411419708095, -0.1820866141732282451 ) ) ;
#3966 = CARTESIAN_POINT ( 'NONE',  ( 1.279527559055118724, -0.5400638737290845981, -0.3530559997133363437 ) ) ;
#3967 = CARTESIAN_POINT ( 'NONE',  ( 0.2909691264735233540, 1.813546053633808830, 0.1157836905918017273 ) ) ;
#3968 = CARTESIAN_POINT ( 'NONE',  ( -0.2755905511811018171, 0.1771653543307087630, 0.000000000000000000 ) ) ;
#3969 = CARTESIAN_POINT ( 'NONE',  ( -0.3346456692913377662, -0.5400638737290844871, 0.3530559997133364547 ) ) ;
#3970 = CARTESIAN_POINT ( 'NONE',  ( -1.555118110236219930, -0.4536011799217368745, -0.2665933059059886201 ) ) ;
#3971 = CARTESIAN_POINT ( 'NONE',  ( -0.6561679790026240244, -0.6046776061558807314, 0.2411417322834647770 ) ) ;
#3972 = CARTESIAN_POINT ( 'NONE',  ( -1.443569553805773564, 0.1283753931104746893, -0.1820866141732285504 ) ) ;
#3973 = CARTESIAN_POINT ( 'NONE',  ( -0.1049643490035302301, -0.3917322834645671770, -0.5413578984590045051 ) ) ;
#3974 = LINE ( 'NONE', #61633, #3699 ) ;
#3975 = CARTESIAN_POINT ( 'NONE',  ( 1.535433070866142335, -0.6692913385826771977, 8.415575281601705876E-17 ) ) ;
#3976 = CARTESIAN_POINT ( 'NONE',  ( -0.4724409448818899238, 0.1265901696524986686, -2.156824146981627166 ) ) ;
#3977 = CARTESIAN_POINT ( 'NONE',  ( -1.056430446194224881, 0.2952755905511810774, -0.1292274648535930714 ) ) ;
#3978 = CARTESIAN_POINT ( 'NONE',  ( -1.148293963254592542, 0.1771653543307087630, 0.09757992244046791164 ) ) ;
#3979 = CARTESIAN_POINT ( 'NONE',  ( -0.5380577427821514602, -0.3690944881889765550, -0.3153832671262227771 ) ) ;
#3980 = CARTESIAN_POINT ( 'NONE',  ( -1.633858267716534529, 0.1660481256975885056, 0.3530559997133364547 ) ) ;
#3981 = CARTESIAN_POINT ( 'NONE',  ( 0.1837270341207357105, -0.6046776061558809534, -0.2411417322834644161 ) ) ;
#3982 = CARTESIAN_POINT ( 'NONE',  ( 0.2690288713910767848, 0.1771653543307087630, 0.09757992244046791164 ) ) ;
#3983 = CARTESIAN_POINT ( 'NONE',  ( -1.220472440944881054, 0.1771653543307087630, 0.000000000000000000 ) ) ;
#3984 = CARTESIAN_POINT ( 'NONE',  ( -1.541994750656167090, 0.2952755905511811885, 0.1292274648535926551 ) ) ;
#3985 = CARTESIAN_POINT ( 'NONE',  ( 1.213910761154856299, -0.5511811023622048555, -0.09757992244046775898 ) ) ;
#3986 = CARTESIAN_POINT ( 'NONE',  ( 1.286089238845145033, -0.6046776061558809534, -0.2411417322834644161 ) ) ;
#3987 = CARTESIAN_POINT ( 'NONE',  ( 0.4725553370316598056, 1.494684982616659275, 2.165615670503216794 ) ) ;
#3988 = CARTESIAN_POINT ( 'NONE',  ( 0.2755905511811031494, 0.1771653543307087630, 0.000000000000000000 ) ) ;
#3989 = CARTESIAN_POINT ( 'NONE',  ( 1.056430446194226658, 0.2952755905511811885, 0.1292274648535926551 ) ) ;
#3990 = CARTESIAN_POINT ( 'NONE',  ( 0.06873123812453012238, 8.471767977567108961E-16, -0.4445507791589058955 ) ) ;
#3991 = CARTESIAN_POINT ( 'NONE',  ( 1.135170603674541256, 0.1771653543307087630, 0.09757992244046791164 ) ) ;
#3992 = ORIENTED_EDGE ( 'NONE', *, *, #78629, .F. ) ;
#3993 = CARTESIAN_POINT ( 'NONE',  ( -1.187664041994749731, -0.3162353388693405765, 0.4822834645669290543 ) ) ;
#3994 = CARTESIAN_POINT ( 'NONE',  ( -0.8202099737532799750, 0.2952755905511810774, -0.1292274648535930714 ) ) ;
#3995 = CARTESIAN_POINT ( 'NONE',  ( -0.05905511811023545637, -0.5400638737290845981, -0.3530559997133363437 ) ) ;
#3996 = CARTESIAN_POINT ( 'NONE',  ( 4.893765752498283924E-17, -0.3996062992125986035, -0.07874015748031498729 ) ) ;
#3997 = CARTESIAN_POINT ( 'NONE',  ( -0.1070741851644051862, -0.3996062992125986590, -2.353674540682414662 ) ) ;
#3998 = CARTESIAN_POINT ( 'NONE',  ( 1.036745406824147508, -0.4281496062992127816, -0.4176697321401328100 ) ) ;
#3999 = CARTESIAN_POINT ( 'NONE',  ( 1.587926509186352142, -0.004921259842519576551, 0.3153832671262227771 ) ) ;
#4000 = CARTESIAN_POINT ( 'NONE',  ( -0.09842519685039295696, -0.5400638737290844871, 0.3530559997133364547 ) ) ;
#4001 = CARTESIAN_POINT ( 'NONE',  ( 0.9055118110236227702, -0.6692913385826771977, 8.415575281601705876E-17 ) ) ;
#4002 = CARTESIAN_POINT ( 'NONE',  ( -0.2925321140481932924, 0.2925321140481931814, -1.751968503937007648 ) ) ;
#4003 = CARTESIAN_POINT ( 'NONE',  ( 0.2891555358219910499, -0.2891555358219909944, -0.8858267716535433989 ) ) ;
#4004 = CARTESIAN_POINT ( 'NONE',  ( 0.3460692066303959757, -0.1998031496062991907, -2.309711286089239035 ) ) ;
#4005 = CARTESIAN_POINT ( 'NONE',  ( -0.4724409448818890911, 0.1265901696525001952, -0.6627296587926508886 ) ) ;
#4006 = CARTESIAN_POINT ( 'NONE',  ( -0.2867679344610364334, -0.2867679344610367109, -0.05118110236220467513 ) ) ;
#4007 = CARTESIAN_POINT ( 'NONE',  ( -0.2887139107611542133, 0.1283753931104748280, 0.1820866141732283561 ) ) ;
#4008 = CARTESIAN_POINT ( 'NONE',  ( -0.6233595800524928121, -0.05778040916215522460, 0.4822834645669289988 ) ) ;
#4009 = CARTESIAN_POINT ( 'NONE',  ( 0.8202099737532813073, 0.2952755905511811885, 0.1292274648535926551 ) ) ;
#4010 = CARTESIAN_POINT ( 'NONE',  ( -0.1974969037888704149, -0.3420746716998661063, -2.347112860892388575 ) ) ;
#4011 = CARTESIAN_POINT ( 'NONE',  ( -0.6036745406824141069, -0.5023911411419708095, -0.1820866141732282451 ) ) ;
#4012 = CARTESIAN_POINT ( 'NONE',  ( -1.371391076115484609, -0.6692913385826771977, 0.1292274648535927661 ) ) ;
#4013 = CARTESIAN_POINT ( 'NONE',  ( 1.351706036745407458, -0.4281496062992127816, -0.4176697321401328100 ) ) ;
#4014 = CARTESIAN_POINT ( 'NONE',  ( -0.1265901696524986964, -0.4724409448818899238, -2.276902887139107268 ) ) ;
#4015 = CARTESIAN_POINT ( 'NONE',  ( 0.1998031496062994405, -0.3460692066303958092, -1.666666666666666741 ) ) ;
#4016 = DIRECTION ( 'NONE',  ( -0.000000000000000000, 1.000000000000000000, -0.000000000000000000 ) ) ;
#4017 = EDGE_CURVE ( 'NONE', #77098, #48423, #4300, .T. ) ;
#4018 = CARTESIAN_POINT ( 'NONE',  ( 0.9448818897637802916, -0.1870078740157479769, 0.4822834645669291653 ) ) ;
#4019 = CARTESIAN_POINT ( 'NONE',  ( 1.437007874015748810, 0.07958543189024085140, 0.2665933059059887866 ) ) ;
#4021 = CARTESIAN_POINT ( 'NONE',  ( -1.410761154855641575, -0.3162353388693409650, -0.4822834645669289433 ) ) ;
#4020 = CARTESIAN_POINT ( 'NONE',  ( 1.692913385826772421, 0.2952755905511811885, 0.000000000000000000 ) ) ;
#4022 = CARTESIAN_POINT ( 'NONE',  ( -0.3917322834645669549, -7.196005306013483243E-17, -2.796568610727347082 ) ) ;
#4023 = DIRECTION ( 'NONE',  ( 0.000000000000000000, 0.000000000000000000, 1.000000000000000000 ) ) ;
#4024 = CARTESIAN_POINT ( 'NONE',  ( 0.8530183727034128527, -0.4281496062992124485, 0.4176697321401328655 ) ) ;
#4025 = CARTESIAN_POINT ( 'NONE',  ( -1.489501312335957062, -0.3162353388693409650, -0.4822834645669289433 ) ) ;
#4026 = CARTESIAN_POINT ( 'NONE',  ( -0.6167979002624665030, 0.05413385826771666132, 0.4176697321401328100 ) ) ;
#4027 = CARTESIAN_POINT ( 'NONE',  ( -0.4461942257217840213, 0.2306618581243848609, 0.2411417322834645549 ) ) ;
#4028 = CARTESIAN_POINT ( 'NONE',  ( -1.489501312335957062, -0.05778040916215522460, 0.4822834645669289988 ) ) ;
#4029 = CARTESIAN_POINT ( 'NONE',  ( -0.3917322834645670104, -7.196005306013484475E-17, -0.1240157480314961758 ) ) ;
#4030 = CARTESIAN_POINT ( 'NONE',  ( 0.06561679790026316017, 0.05413385826771626580, -0.4176697321401330321 ) ) ;
#4031 = CARTESIAN_POINT ( 'NONE',  ( 0.2867679344610365999, -0.2867679344610365444, -2.137795275590551380 ) ) ;
#4032 = CARTESIAN_POINT ( 'NONE',  ( -1.614173228346455824, 0.1771653543307087630, 0.000000000000000000 ) ) ;
#4033 = ORIENTED_EDGE ( 'NONE', *, *, #62252, .T. ) ;
#4034 = CARTESIAN_POINT ( 'NONE',  ( -0.3949938075777411628, 0.1058382717557497937, -2.867454068241469756 ) ) ;
#4035 = ORIENTED_EDGE ( 'NONE', *, *, #46544, .F. ) ;
#4036 = CARTESIAN_POINT ( 'NONE',  ( -0.06561679790026180015, 0.009842519685039467087, 0.3409548833797002021 ) ) ;
#4037 = CARTESIAN_POINT ( 'NONE',  ( -1.555118110236219930, 0.1660481256975885056, 0.3530559997133364547 ) ) ;
#4038 = CARTESIAN_POINT ( 'NONE',  ( 0.1070741851644054915, -0.3996062992125986035, -1.030183727034120533 ) ) ;
#4039 = CARTESIAN_POINT ( 'NONE',  ( 1.633858267716535639, -0.4536011799217367080, 0.2665933059059888421 ) ) ;
#4040 = CARTESIAN_POINT ( 'NONE',  ( -0.5314960629921324786, 2.716535433070866645, 1.854472803289050509 ) ) ;
#4041 = DIRECTION ( 'NONE',  ( 0.000000000000000000, -1.000000000000000000, -1.408710688920637755E-15 ) ) ;
#4042 = CARTESIAN_POINT ( 'NONE',  ( 0.9285414500055708675, 0.000000000000000000, 0.6299212598425202314 ) ) ;
#4043 = CARTESIAN_POINT ( 'NONE',  ( -0.3392501089628017219, -0.1958661417322836718, -0.6095800524934383846 ) ) ;
#4044 = CARTESIAN_POINT ( 'NONE',  ( -0.1509186351706028884, -0.2845877964562161244, -0.3641732283464567121 ) ) ;
#4045 = CARTESIAN_POINT ( 'NONE',  ( -1.049868766404198794, 0.1283753931104746893, -0.1820866141732285504 ) ) ;
#4046 = CARTESIAN_POINT ( 'NONE',  ( -1.601049868766403650, 0.2306618581243847221, -0.2411417322834647770 ) ) ;
#4047 = CARTESIAN_POINT ( 'NONE',  ( 0.6889763779527563470, 0.1660481256975883668, -0.3530559997133364547 ) ) ;
#4048 = CARTESIAN_POINT ( 'NONE',  ( -1.371391076115484609, -0.6692913385826771977, 0.1292274648535927661 ) ) ;
#4049 = CARTESIAN_POINT ( 'NONE',  ( 0.1049643490035303689, 0.3917322834645670104, -0.3005249343832020470 ) ) ;
#4050 = EDGE_LOOP ( 'NONE', ( #80768, #13992, #26789, #62532, #23547, #82750, #11274, #56192, #18075, #78345, #74104, #51839, #74536, #66950 ) ) ;
#4051 = CARTESIAN_POINT ( 'NONE',  ( -1.233595800524933894, -0.6046776061558809534, -0.2411417322834644161 ) ) ;
#4052 = CARTESIAN_POINT ( 'NONE',  ( -0.4724409448818899238, 0.1265901696524986686, -1.765091863517059823 ) ) ;
#4053 = CARTESIAN_POINT ( 'NONE',  ( 1.595398199321655275, 1.034147571970761126, -0.1559797534342494130 ) ) ;
#4054 = CARTESIAN_POINT ( 'NONE',  ( -0.1341536278048670039, 1.050682278017461835, 0.2827841492639485144 ) ) ;
#4055 = CARTESIAN_POINT ( 'NONE',  ( -0.8070866141732276899, 0.1660481256975883668, -0.3530559997133364547 ) ) ;
#4056 = CARTESIAN_POINT ( 'NONE',  ( 1.423884514435696413, -0.3162353388693409650, -0.4822834645669289433 ) ) ;
#4058 = CARTESIAN_POINT ( 'NONE',  ( 0.4091458600556404646, -0.2362204724409448231, -1.994750656167979086 ) ) ;
#4057 = CARTESIAN_POINT ( 'NONE',  ( -1.535433070866141225, 0.2952755905511811885, 0.000000000000000000 ) ) ;
#4059 = CARTESIAN_POINT ( 'NONE',  ( 1.594488188976378673, -0.5400638737290845981, -0.3530559997133363437 ) ) ;
#4060 = CARTESIAN_POINT ( 'NONE',  ( -0.6758530183727028406, -0.6692913385826773087, -0.1292274648535924053 ) ) ;
#4061 = CARTESIAN_POINT ( 'NONE',  ( -0.1049643490035306742, 0.3917322834645668994, -0.4015554873677671943 ) ) ;
#4062 = CARTESIAN_POINT ( 'NONE',  ( 0.02624671916010564918, 0.1283753931104748280, 0.1820866141732283561 ) ) ;
#4063 = CARTESIAN_POINT ( 'NONE',  ( -0.2867679344610364334, -0.2867679344610367109, -0.6161417322834645827 ) ) ;
#4064 = CARTESIAN_POINT ( 'NONE',  ( 0.1115485564304470323, 0.1771653543307087630, 0.09757992244046791164 ) ) ;
#4065 = CARTESIAN_POINT ( 'NONE',  ( 0.4724409448818904789, -0.1870078740157479769, 0.3641732283464567677 ) ) ;
#4066 = CARTESIAN_POINT ( 'NONE',  ( 0.5249343832021003964, 0.2306618581243847221, -0.2411417322834647770 ) ) ;
#4067 = CARTESIAN_POINT ( 'NONE',  ( -0.2493438320209966919, -0.3690944881889763329, 0.3153832671262228327 ) ) ;
#4068 = CARTESIAN_POINT ( 'NONE',  ( 0.1958661417322834775, 0.3392501089628018884, -2.341207349081364963 ) ) ;
#4069 = CARTESIAN_POINT ( 'NONE',  ( -1.594488188976377119, 0.1660481256975883668, -0.3530559997133364547 ) ) ;
#4070 = CARTESIAN_POINT ( 'NONE',  ( -1.010498687664041384, 0.05413385826771666132, 0.4176697321401328100 ) ) ;
#4071 = CARTESIAN_POINT ( 'NONE',  ( -0.4724409448818899238, 0.1265901696524986686, -0.5820209973753280863 ) ) ;
#4072 = CARTESIAN_POINT ( 'NONE',  ( 0.1312335958005255154, -0.6046776061558807314, 0.2411417322834647770 ) ) ;
#4073 = CARTESIAN_POINT ( 'NONE',  ( -0.4396325459317577122, -0.6692913385826773087, -0.1292274648535924053 ) ) ;
#4074 = CARTESIAN_POINT ( 'NONE',  ( 1.535433070866142558, 0.1771653543307087630, 0.000000000000000000 ) ) ;
#4075 = CARTESIAN_POINT ( 'NONE',  ( -0.03280839895013062252, -0.5511811023622046335, 0.09757992244046803654 ) ) ;
#4076 = CARTESIAN_POINT ( 'NONE',  ( -0.04593175853018302557, -0.6692913385826773087, -0.1292274648535924053 ) ) ;
#4077 = CARTESIAN_POINT ( 'NONE',  ( -0.6758530183727028406, 0.2952755905511811885, 0.1292274648535926551 ) ) ;
#4078 = CARTESIAN_POINT ( 'NONE',  ( 3.197598479107677694, 2.742783273398275767, -0.5314960629921260393 ) ) ;
#4079 = DIRECTION ( 'NONE',  ( -0.000000000000000000, -1.000000000000000000, -0.000000000000000000 ) ) ;
#4080 = CARTESIAN_POINT ( 'NONE',  ( 0.1968503937007881344, -0.6692913385826771977, 8.415575281601705876E-17 ) ) ;
#4081 = EDGE_LOOP ( 'NONE', ( #47562, #17698, #57169 ) ) ;
#4082 = CARTESIAN_POINT ( 'NONE',  ( 0.1070741851644053388, 0.3996062992125986035, -2.117454068241469756 ) ) ;
#4083 = CARTESIAN_POINT ( 'NONE',  ( 0.3307086614173228023, -0.3242060844882008741, 0.000000000000000000 ) ) ;
#4084 = CARTESIAN_POINT ( 'NONE',  ( -0.6364829396325453192, -0.2845877964562159024, 0.3641732283464567677 ) ) ;
#4085 = CARTESIAN_POINT ( 'NONE',  ( -0.7152230971128602510, -0.05778040916215560624, -0.4822834645669293319 ) ) ;
#4086 = CARTESIAN_POINT ( 'NONE',  ( 1.332020997375329197, -0.3162353388693405765, 0.4822834645669290543 ) ) ;
#4087 = CARTESIAN_POINT ( 'NONE',  ( 1.187664041994751285, -0.05778040916215522460, 0.4822834645669289988 ) ) ;
#4088 = CARTESIAN_POINT ( 'NONE',  ( -1.607611548556429737, 0.2952755905511810774, -0.1292274648535930714 ) ) ;
#4089 = CARTESIAN_POINT ( 'NONE',  ( -1.181102362204723644, -0.1870078740157480601, -0.3641732283464567677 ) ) ;
#4090 = CARTESIAN_POINT ( 'NONE',  ( 0.1998031496062992463, 0.3460692066303959202, -0.06364829396325462352 ) ) ;
#4091 = CARTESIAN_POINT ( 'NONE',  ( 0.2925321140481932369, -0.2925321140481932369, -0.4133858267716534196 ) ) ;
#4092 = CARTESIAN_POINT ( 'NONE',  ( 0.3917322834645670659, -0.1049643490035303273, -2.785452386647981449 ) ) ;
#4093 = CARTESIAN_POINT ( 'NONE',  ( 1.587926509186352586, -0.3690944881889765550, -0.3153832671262227771 ) ) ;
#4094 = CARTESIAN_POINT ( 'NONE',  ( 1.148293963254593653, 0.1771653543307087075, -0.09757992244046823083 ) ) ;
#4095 = AXIS2_PLACEMENT_3D ( 'NONE', #22085, #78520, #66295 ) ;
#4096 = CARTESIAN_POINT ( 'NONE',  ( 0.4002624671916016896, -0.3162353388693409650, -0.4822834645669289433 ) ) ;
#4097 = CARTESIAN_POINT ( 'NONE',  ( -1.679790026246718693, 0.2306618581243847221, -0.2411417322834647770 ) ) ;
#4098 = CARTESIAN_POINT ( 'NONE',  ( 0.9251968503937015864, -0.5400638737290844871, 0.3530559997133364547 ) ) ;
#4099 = CARTESIAN_POINT ( 'NONE',  ( -0.3949938075777411073, 0.1058382717557497660, -0.8969816272965878134 ) ) ;
#4100 = CARTESIAN_POINT ( 'NONE',  ( 1.253280839895013710, -0.08942795157528024563, -0.3641732283464568787 ) ) ;
#4101 =( BOUNDED_SURFACE ( )  B_SPLINE_SURFACE ( 1, 2, ( 
 ( #66159, #27848, #53509, #6814, #58577, #517, #78378, #79217, #46782, #14822, #13559, #58148, #8086, #39215, #64900, #26600, #26170, #52252, #32911, #942, #71634, #13986, #39642, #20709, #1358, #46362, #72055, #79632, #10572, #74134, #21950, #15652, #3010, #16896, #28677, #74551, #67821, #41308, #42126, #66994, #23591, #54338, #60661, #80048, #23180, #29087, #22367, #66574, #36229, #68237, #16065, #48850, #80868, #10158, #48026, #9738, #53919, #54757, #42535, #72884, #34584, #8908, #2600, #9326, #34996, #61898, #4239, #73726, #16479, #41711, #35824, #47609, #55157, #73304, #29903, #55567, #67403, #48435, #81275, #35409, #15233, #40893, #3424, #61073, #80463, #60252, #22772, #61490, #3838, #28258, #29498, #6295, #63958, #17712, #82503, #31970, #57631, #56400, #68632, #43340, #18119, #12623, #31572, #5880, #18927, #63136, #18527, #30737, #43752, #70269, #24006, #24412, #38282, #30316, #11808, #44576, #62308, #42938, #31553, #37872, #37463, #24819, #49262, #55984, #69458, #74964, #5068, #82098, #5475, #17310, #10972, #50897, #50082, #57210, #31137, #69863, #4645, #56804, #50486, #76190, #82911, #36631, #44170, #25232, #81695, #49674, #75364, #12214, #69041, #63546, #76597, #11391, #75778, #37048, #62730, #71113, #64376, #77429, #7133, #40374, #27322, #52565, #46679, #20182, #25645, #8393, #33236, #6713, #1258, #32806, #72372, #13045, #52982, #78274, #77011, #51308, #19343, #14306, #7982, #65226, #34059, #58898, #33646, #837, #78695, #59722, #71953, #45832, #39966, #44993, #14721, #19764, #21018, #66056, #59308, #70692, #412, #7564, #13456, #26495, #65653, #71531, #38698, #32382, #26906, #52147, #39112, #58046, #26068, #51727, #45417, #13879, #64794, #1665, #39538, #20606, #58473, #77853, #46258, #67300, #79525, #47088, #23077, #9223, #16373, #28157, #47917, #47504, #53812, #2498, #15546, #21840, #80763, #60146, #36125, #10472, #21433, #48745, #73622, #2077, #9634, #3732, #72778, #55055, #3317, #48330, #22259, #27742, #28981, #41611, #42427, #74444, #34896, #53407, #60966, #68127, #79115, #15128, #73196, #40784, #60558, #28572, #35304, #22671, #61383, #66469, #66893, #16790, #8804, #34480, #54648, #80358, #42020, #74027, #2908, #29396, #41205, #54229, #67714, #10050, #79946, #15964, #35713, #75680, #24312, #18021, #12520, #49982, #30216, #43655, #18830, #4138, #44476, #76502, #55878, #11711, #70167, #61798, #68940, #81174, #81590, #30636, #25131, #29803, #18432, #31450, #69357, #31037, #43242, #56301, #82807, #36532, #36949, #50801, #42838, #37366, #57113, #74863, #55464, #44074, #50391, #63038, #5376, #23491, #68531, #81998, #49157, #17611, #11290, #56705, #17205, #10872, #63444, #62626, #69766, #82404, #24723, #62208, #76088, #12111, #37769, #5780, #4546, #23907, #49572, #75268, #4969, #59207, #78595, #6193, #308, #25543, #52046, #65550, #78172, #1155, #44887, #1568, #39434, #70586, #64276, #51621, #7881, #77326, #39859, #33127, #6611, #7457, #32282, #72271, #19655, #25963, #45317, #71853, #77751, #71012, #31871, #27222, #33545, #64693, #14202, #46157, #58797, #13356, #58368, #19236, #20084, #52883, #38181, #83222, #57531, #51209, #57942, #39009, #20919, #46573, #7032, #65121, #32701, #26806, #12940, #20503, #38598, #26388, #63856, #45734, #76906, #730, #71430, #52464, #13777, #34800, #14619, #41519, #54130, #54965, #9947, #47406, #48651, #73522, #80672, #8292, #27640, #40684, #59622, #73095, #41106, #47821, #35207, #73935, #79014, #79421, #29303, #1977, #40273, #79845, #15871, #54547, #22162, #21741, #9536, #67617, #2810, #67204, #22985, #53714, #46986, #65956, #60043, #53302, #66370, #15447, #33960, #16278, #60869, #35620, #9129, #21334, #72680, #3222, #15028, #28887, #66794, #61283, #8707, #41923, #80262, #34378, #2399, #28056, #22578, #48239, #3635, #60459, #28469, #107, #49481, #19458, #531, #38398, #69971, #64077, #42332, #13164, #68441, #45109, #70815, #25761, #68030, #49064, #31668, #62114, #75174, #6415, #12325, #10375, #36032, #76707, #18637, #4457, #6830, #61706, #4046, #29711, #63658, #42746, #51423, #5998, #37983, #55785, #55374 ),
 ( #38814, #58163, #57329, #83023, #25346, #17111, #64492, #32499, #10781, #19040, #44281, #44687, #81080, #57745, #23396, #77125, #26184, #74762, #51008, #74347, #70383, #16692, #36441, #12738, #32084, #30122, #81492, #23808, #20301, #33762, #8923, #77553, #34600, #66587, #45950, #1779, #60265, #2615, #59015, #71232, #71648, #20722, #15247, #51846, #8511, #21545, #65765, #21138, #33352, #46373, #72896, #26613, #27022, #40906, #32924, #14426, #47206, #64915, #45534, #34177, #40493, #40077, #27438, #19886, #58590, #72067, #13576, #7684, #1371, #8097, #39230, #7252, #53522, #52683, #59841, #59423, #72484, #958, #53099, #78809, #46793, #2194, #52266, #14833, #27862, #77971, #13999, #39656, #65347, #78391, #66172, #79230, #42138, #55580, #68251, #74564, #35009, #49275, #29511, #60674, #54350, #41722, #81290, #67415, #29916, #23193, #80062, #80881, #22380, #62320, #9749, #16077, #35421, #61912, #67833, #61086, #21962, #74978, #23606, #54771, #4254, #36243, #48864, #3437, #48447, #9339, #10172, #17323, #28271, #73317, #47622, #41325, #48039, #67006, #3851, #29100, #42952, #15664, #68646, #55172, #79645, #53933, #3022, #16910, #10586, #35837, #36644, #61505, #10984, #80475, #28689, #73741, #42548, #22787, #74147, #16492, #25663, #82112, #31987, #57647, #12638, #55996, #62745, #44185, #75791, #5490, #18943, #82516, #24018, #81708, #5897, #31151, #18133, #19360, #49686, #75379, #17727, #76204, #56413, #38298, #18542, #50501, #69471, #43354, #38715, #69877, #24426, #69055, #51324, #11824, #44591, #30750, #12230, #50095, #43766, #5081, #37477, #63149, #10, #56818, #4657, #13061, #11404, #77027, #37887, #30330, #63562, #6310, #37061, #45009, #31569, #50912, #24832, #57226, #82927, #25248, #70709, #76613, #70285, #63974, #39982, #47106, #58062, #77447, #7149, #26084, #39554, #7581, #14324, #1681, #40390, #45434, #45849, #79132, #51744, #6729, #46274, #65672, #21035, #71969, #71548, #59325, #34076, #52582, #7999, #72795, #20198, #13472, #15145, #26511, #19781, #32822, #13896, #21449, #66073, #33662, #2094, #58915, #64393, #32399, #27339, #1274, #71129, #20622, #14738, #428, #39129, #64810, #58489, #854, #52165, #8409, #27759, #77869, #52998, #65243, #78711, #33253, #46695, #26922, #59740, #53423, #78291, #72388, #48764, #35323, #36145, #23510, #54666, #3336, #80377, #74882, #29000, #9242, #22690, #81193, #66486, #49178, #55484, #34914, #74046, #40801, #8821, #47938, #60163, #60577, #9654, #4157, #34498, #80781, #10491, #48349, #10069, #22278, #60986, #61817, #15564, #15983, #29822, #21858, #16393, #2515, #53831, #28174, #23097, #29414, #42040, #67734, #79545, #47522, #35733, #73214, #79965, #73641, #61401, #41224, #66911, #42447, #41630, #74463, #3750, #55073, #2928, #16810, #68147, #28592, #54248, #67319, #18452, #57133, #51228, #70187, #38199, #57549, #68551, #62648, #4566, #31059, #44496, #82830, #63468, #23927, #63874, #44094, #49594, #43263, #30657, #12541, #56321, #18850, #12133, #68960, #69788, #11310, #17227, #82020, #4990, #24333, #50820, #56727, #50003, #10892, #6213, #31889, #43675, #76521, #25152, #37790, #75700, #36969, #83240, #25561, #42858, #36552, #75288, #82424, #18041, #69378, #31471, #11731, #62228, #30237, #5801, #37387, #63058, #55901, #81612, #17631, #5396, #24743, #50411, #76111, #7476, #39452, #58387, #32300, #27656, #58816, #71030, #38616, #14635, #748, #7900, #19676, #65140, #39027, #45335, #77345, #7051, #13374, #72289, #51640, #76926, #1993, #12959, #40291, #33147, #19254, #1173, #78611, #64294, #46593, #78190, #39879, #13795, #44906, #20521, #26824, #33976, #65972, #26409, #70604, #52482, #59637, #6628, #57960, #64711, #328, #52063, #20101, #46173, #14219, #52898, #25982, #77769, #8309, #32720, #45752, #71869, #65566, #33561, #59223, #71447, #1584, #27239, #20934, #54562, #61719, #9144, #2414, #4057, #15462, #8722, #21757, #34815, #68044, #54978, #80278, #74362, #47835, #53321, #36047, #60886, #34393, #28900, #60474, #16705, #40700, #80685, #22591, #21350, #79031, #47003, #41937, #35635, #9552, #72697, #3236, #61296, #28486, #22999 ) ),
 .UNSPECIFIED., .F., .F., .F. ) 
 B_SPLINE_SURFACE_WITH_KNOTS ( ( 2, 2 ),
 ( 3, 2, 2, 2, 2, 2, 2, 2, 2, 2, 2, 2, 2, 2, 2, 2, 2, 2, 2, 2, 2, 2, 2, 2, 2, 2, 2, 2, 2, 2, 2, 2, 2, 2, 2, 2, 2, 2, 2, 2, 2, 2, 2, 2, 2, 2, 2, 2, 2, 2, 2, 2, 2, 2, 2, 2, 2, 2, 2, 2, 2, 2, 2, 2, 2, 2, 2, 2, 2, 2, 2, 2, 2, 2, 2, 2, 2, 2, 2, 2, 2, 2, 2, 2, 2, 2, 2, 2, 2, 2, 2, 2, 2, 2, 2, 2, 2, 2, 2, 2, 2, 2, 2, 2, 2, 2, 2, 2, 2, 2, 2, 2, 2, 2, 2, 2, 2, 2, 2, 2, 2, 2, 2, 2, 2, 2, 2, 2, 2, 2, 2, 2, 2, 2, 2, 2, 2, 2, 2, 2, 2, 2, 2, 2, 2, 2, 2, 2, 2, 2, 2, 2, 2, 2, 2, 2, 2, 2, 2, 2, 2, 2, 2, 2, 2, 2, 2, 2, 2, 2, 2, 2, 2, 2, 2, 2, 2, 2, 2, 2, 2, 2, 2, 2, 2, 2, 2, 2, 2, 2, 2, 2, 2, 2, 2, 2, 2, 2, 2, 2, 2, 2, 2, 2, 2, 2, 2, 2, 2, 2, 2, 2, 2, 2, 2, 2, 2, 2, 2, 2, 2, 2, 2, 2, 2, 2, 2, 2, 2, 2, 2, 2, 2, 2, 2, 2, 2, 2, 2, 2, 2, 2, 2, 2, 2, 2, 2, 2, 2, 2, 2, 2, 2, 2, 2, 3 ),
 ( 0.000000000000000000, 1.000000000000000000 ),
 ( 0.000000000000000000, 0.003787878787878787984, 0.007575757575757575968, 0.01136363636363636395, 0.01515151515151515194, 0.01893939393939393992, 0.02272727272727272790, 0.02651515151515151589, 0.03030303030303030387, 0.03409090909090908839, 0.03787878787878787984, 0.04166666666666666435, 0.04545454545454545581, 0.04924242424242424032, 0.05303030303030303177, 0.05681818181818181629, 0.06060606060606060774, 0.06439393939393939226, 0.06818181818181817677, 0.07196969696969697516, 0.07575757575757575968, 0.07954545454545454419, 0.08333333333333332871, 0.08712121212121212710, 0.09090909090909091161, 0.09469696969696969613, 0.09848484848484848064, 0.1022727272727272790, 0.1060606060606060635, 0.1098484848484848481, 0.1136363636363636326, 0.1174242424242424310, 0.1212121212121212155, 0.1250000000000000000, 0.1287878787878787845, 0.1325757575757575690, 0.1363636363636363535, 0.1401515151515151381, 0.1439393939393939503, 0.1477272727272727348, 0.1515151515151515194, 0.1553030303030303039, 0.1590909090909090884, 0.1628787878787878729, 0.1666666666666666574, 0.1704545454545454419, 0.1742424242424242542, 0.1780303030303030387, 0.1818181818181818232, 0.1856060606060606077, 0.1893939393939393923, 0.1931818181818181768, 0.1969696969696969613, 0.2007575757575757458, 0.2045454545454545581, 0.2083333333333333426, 0.2121212121212121271, 0.2159090909090909116, 0.2196969696969696961, 0.2234848484848484806, 0.2272727272727272652, 0.2310606060606060497, 0.2348484848484848619, 0.2386363636363636465, 0.2424242424242424310, 0.2462121212121212155, 0.2500000000000000000, 0.2537878787878787845, 0.2575757575757575690, 0.2613636363636363535, 0.2651515151515151381, 0.2689393939393939226, 0.2727272727272727071, 0.2765151515151514916, 0.2803030303030302761, 0.2840909090909091161, 0.2878787878787879007, 0.2916666666666666852, 0.2954545454545454697, 0.2992424242424242542, 0.3030303030303030387, 0.3068181818181818232, 0.3106060606060606077, 0.3143939393939393923, 0.3181818181818181768, 0.3219696969696969613, 0.3257575757575757458, 0.3295454545454545303, 0.3333333333333333148, 0.3371212121212120993, 0.3409090909090908839, 0.3446969696969697239, 0.3484848484848485084, 0.3522727272727272929, 0.3560606060606060774, 0.3598484848484848619, 0.3636363636363636465, 0.3674242424242424310, 0.3712121212121212155, 0.3750000000000000000, 0.3787878787878787845, 0.3825757575757575690, 0.3863636363636363535, 0.3901515151515151381, 0.3939393939393939226, 0.3977272727272727071, 0.4015151515151514916, 0.4053030303030302761, 0.4090909090909091161, 0.4128787878787879007, 0.4166666666666666852, 0.4204545454545454697, 0.4242424242424242542, 0.4280303030303030387, 0.4318181818181818232, 0.4356060606060606077, 0.4393939393939393923, 0.4431818181818181768, 0.4469696969696969613, 0.4507575757575757458, 0.4545454545454545303, 0.4583333333333333148, 0.4621212121212120993, 0.4659090909090908839, 0.4696969696969697239, 0.4734848484848485084, 0.4772727272727272929, 0.4810606060606060774, 0.4848484848484848619, 0.4886363636363636465, 0.4924242424242424310, 0.4962121212121212155, 0.5000000000000000000, 0.5037878787878787845, 0.5075757575757575690, 0.5113636363636363535, 0.5151515151515151381, 0.5189393939393939226, 0.5227272727272727071, 0.5265151515151514916, 0.5303030303030302761, 0.5340909090909090606, 0.5378787878787878451, 0.5416666666666666297, 0.5454545454545454142, 0.5492424242424241987, 0.5530303030303029832, 0.5568181818181817677, 0.5606060606060605522, 0.5643939393939394478, 0.5681818181818182323, 0.5719696969696970168, 0.5757575757575758013, 0.5795454545454545858, 0.5833333333333333703, 0.5871212121212121549, 0.5909090909090909394, 0.5946969696969697239, 0.5984848484848485084, 0.6022727272727272929, 0.6060606060606060774, 0.6098484848484848619, 0.6136363636363636465, 0.6174242424242424310, 0.6212121212121212155, 0.6250000000000000000, 0.6287878787878787845, 0.6325757575757575690, 0.6363636363636363535, 0.6401515151515151381, 0.6439393939393939226, 0.6477272727272727071, 0.6515151515151514916, 0.6553030303030302761, 0.6590909090909090606, 0.6628787878787878451, 0.6666666666666666297, 0.6704545454545454142, 0.6742424242424241987, 0.6780303030303029832, 0.6818181818181817677, 0.6856060606060605522, 0.6893939393939394478, 0.6931818181818182323, 0.6969696969696970168, 0.7007575757575758013, 0.7045454545454545858, 0.7083333333333333703, 0.7121212121212121549, 0.7159090909090909394, 0.7196969696969697239, 0.7234848484848485084, 0.7272727272727272929, 0.7310606060606060774, 0.7348484848484848619, 0.7386363636363636465, 0.7424242424242424310, 0.7462121212121212155, 0.7500000000000000000, 0.7537878787878787845, 0.7575757575757575690, 0.7613636363636363535, 0.7651515151515151381, 0.7689393939393939226, 0.7727272727272727071, 0.7765151515151514916, 0.7803030303030302761, 0.7840909090909090606, 0.7878787878787878451, 0.7916666666666666297, 0.7954545454545454142, 0.7992424242424241987, 0.8030303030303029832, 0.8068181818181817677, 0.8106060606060605522, 0.8143939393939394478, 0.8181818181818182323, 0.8219696969696970168, 0.8257575757575758013, 0.8295454545454545858, 0.8333333333333333703, 0.8371212121212121549, 0.8409090909090909394, 0.8446969696969697239, 0.8484848484848485084, 0.8522727272727272929, 0.8560606060606060774, 0.8598484848484848619, 0.8636363636363636465, 0.8674242424242424310, 0.8712121212121212155, 0.8750000000000000000, 0.8787878787878787845, 0.8825757575757575690, 0.8863636363636363535, 0.8901515151515151381, 0.8939393939393939226, 0.8977272727272727071, 0.9015151515151514916, 0.9053030303030302761, 0.9090909090909090606, 0.9128787878787878451, 0.9166666666666666297, 0.9204545454545454142, 0.9242424242424241987, 0.9280303030303029832, 0.9318181818181817677, 0.9356060606060605522, 0.9393939393939394478, 0.9431818181818182323, 0.9469696969696970168, 0.9507575757575758013, 0.9545454545454545858, 0.9583333333333333703, 0.9621212121212121549, 0.9659090909090909394 ),
 .UNSPECIFIED. ) 
 GEOMETRIC_REPRESENTATION_ITEM ( )  RATIONAL_B_SPLINE_SURFACE ( (
 ( 1.000000000000000000, 0.9659258262890683122, 1.000000000000000000, 0.9659258262890683122, 1.000000000000000000, 0.9659258262890683122, 1.000000000000000000, 0.9659258262890683122, 1.000000000000000000, 0.9659258262890683122, 1.000000000000000000, 0.9659258262890683122, 1.000000000000000000, 0.9659258262890683122, 1.000000000000000000, 0.9659258262890683122, 1.000000000000000000, 0.9659258262890683122, 1.000000000000000000, 0.9659258262890683122, 1.000000000000000000, 0.9659258262890683122, 1.000000000000000000, 0.9659258262890683122, 1.000000000000000000, 0.9659258262890683122, 1.000000000000000000, 0.9659258262890683122, 1.000000000000000000, 0.9659258262890683122, 1.000000000000000000, 0.9659258262890683122, 1.000000000000000000, 0.9659258262890683122, 1.000000000000000000, 0.9659258262890683122, 1.000000000000000000, 0.9659258262890683122, 1.000000000000000000, 0.9659258262890683122, 1.000000000000000000, 0.9659258262890683122, 1.000000000000000000, 0.9659258262890683122, 1.000000000000000000, 0.9659258262890683122, 1.000000000000000000, 0.9659258262890683122, 1.000000000000000000, 0.9659258262890683122, 1.000000000000000000, 0.9659258262890683122, 1.000000000000000000, 0.9659258262890683122, 1.000000000000000000, 0.9659258262890683122, 1.000000000000000000, 0.9659258262890683122, 1.000000000000000000, 0.9659258262890683122, 1.000000000000000000, 0.9659258262890683122, 1.000000000000000000, 0.9659258262890683122, 1.000000000000000000, 0.9659258262890683122, 1.000000000000000000, 0.9659258262890683122, 1.000000000000000000, 0.9659258262890683122, 1.000000000000000000, 0.9659258262890683122, 1.000000000000000000, 0.9659258262890683122, 1.000000000000000000, 0.9659258262890683122, 1.000000000000000000, 0.9659258262890683122, 1.000000000000000000, 0.9659258262890683122, 1.000000000000000000, 0.9659258262890683122, 1.000000000000000000, 0.9659258262890683122, 1.000000000000000000, 0.9659258262890683122, 1.000000000000000000, 0.9659258262890683122, 1.000000000000000000, 0.9659258262890683122, 1.000000000000000000, 0.9659258262890683122, 1.000000000000000000, 0.9659258262890683122, 1.000000000000000000, 0.9659258262890683122, 1.000000000000000000, 0.9659258262890683122, 1.000000000000000000, 0.9659258262890683122, 1.000000000000000000, 0.9659258262890683122, 1.000000000000000000, 0.9659258262890683122, 1.000000000000000000, 0.9659258262890683122, 1.000000000000000000, 0.9659258262890683122, 1.000000000000000000, 0.9659258262890683122, 1.000000000000000000, 0.9659258262890683122, 1.000000000000000000, 0.9659258262890683122, 1.000000000000000000, 0.9659258262890683122, 1.000000000000000000, 0.9659258262890683122, 1.000000000000000000, 0.9659258262890683122, 1.000000000000000000, 0.9659258262890683122, 1.000000000000000000, 0.9659258262890683122, 1.000000000000000000, 0.9659258262890683122, 1.000000000000000000, 0.9659258262890683122, 1.000000000000000000, 0.9659258262890683122, 1.000000000000000000, 0.9659258262890683122, 1.000000000000000000, 0.9659258262890683122, 1.000000000000000000, 0.9659258262890683122, 1.000000000000000000, 0.9659258262890683122, 1.000000000000000000, 0.9659258262890683122, 1.000000000000000000, 0.9659258262890683122, 1.000000000000000000, 0.9659258262890683122, 1.000000000000000000, 0.9659258262890683122, 1.000000000000000000, 0.9659258262890683122, 1.000000000000000000, 0.9659258262890683122, 1.000000000000000000, 0.9659258262890683122, 1.000000000000000000, 0.9659258262890683122, 1.000000000000000000, 0.9659258262890683122, 1.000000000000000000, 0.9659258262890683122, 1.000000000000000000, 0.9659258262890683122, 1.000000000000000000, 0.9659258262890683122, 1.000000000000000000, 0.9659258262890683122, 1.000000000000000000, 0.9659258262890683122, 1.000000000000000000, 0.9659258262890683122, 1.000000000000000000, 0.9659258262890683122, 1.000000000000000000, 0.9659258262890683122, 1.000000000000000000, 0.9659258262890683122, 1.000000000000000000, 0.9659258262890683122, 1.000000000000000000, 0.9659258262890683122, 1.000000000000000000, 0.9659258262890683122, 1.000000000000000000, 0.9659258262890683122, 1.000000000000000000, 0.9659258262890683122, 1.000000000000000000, 0.9659258262890683122, 1.000000000000000000, 0.9659258262890683122, 1.000000000000000000, 0.9659258262890683122, 1.000000000000000000, 0.9659258262890683122, 1.000000000000000000, 0.9659258262890683122, 1.000000000000000000, 0.9659258262890683122, 1.000000000000000000, 0.9659258262890683122, 1.000000000000000000, 0.9659258262890683122, 1.000000000000000000, 0.9659258262890683122, 1.000000000000000000, 0.9659258262890683122, 1.000000000000000000, 0.9659258262890683122, 1.000000000000000000, 0.9659258262890683122, 1.000000000000000000, 0.9659258262890683122, 1.000000000000000000, 0.9659258262890683122, 1.000000000000000000, 0.9659258262890683122, 1.000000000000000000, 0.9659258262890683122, 1.000000000000000000, 0.9659258262890683122, 1.000000000000000000, 0.9659258262890683122, 1.000000000000000000, 0.9659258262890683122, 1.000000000000000000, 0.9659258262890683122, 1.000000000000000000, 0.9659258262890683122, 1.000000000000000000, 0.9659258262890683122, 1.000000000000000000, 0.9659258262890683122, 1.000000000000000000, 0.9659258262890683122, 1.000000000000000000, 0.9659258262890683122, 1.000000000000000000, 0.9659258262890683122, 1.000000000000000000, 0.9659258262890683122, 1.000000000000000000, 0.9659258262890683122, 1.000000000000000000, 0.9659258262890683122, 1.000000000000000000, 0.9659258262890683122, 1.000000000000000000, 0.9659258262890683122, 1.000000000000000000, 0.9659258262890683122, 1.000000000000000000, 0.9659258262890683122, 1.000000000000000000, 0.9659258262890683122, 1.000000000000000000, 0.9659258262890683122, 1.000000000000000000, 0.9659258262890683122, 1.000000000000000000, 0.9659258262890683122, 1.000000000000000000, 0.9659258262890683122, 1.000000000000000000, 0.9659258262890683122, 1.000000000000000000, 0.9659258262890683122, 1.000000000000000000, 0.9659258262890683122, 1.000000000000000000, 0.9659258262890683122, 1.000000000000000000, 0.9659258262890683122, 1.000000000000000000, 0.9659258262890683122, 1.000000000000000000, 0.9659258262890683122, 1.000000000000000000, 0.9659258262890683122, 1.000000000000000000, 0.9659258262890683122, 1.000000000000000000, 0.9659258262890683122, 1.000000000000000000, 0.9659258262890683122, 1.000000000000000000, 0.9659258262890683122, 1.000000000000000000, 0.9659258262890683122, 1.000000000000000000, 0.9659258262890683122, 1.000000000000000000, 0.9659258262890683122, 1.000000000000000000, 0.9659258262890683122, 1.000000000000000000, 0.9659258262890683122, 1.000000000000000000, 0.9659258262890683122, 1.000000000000000000, 0.9659258262890683122, 1.000000000000000000, 0.9659258262890683122, 1.000000000000000000, 0.9659258262890683122, 1.000000000000000000, 0.9659258262890683122, 1.000000000000000000, 0.9659258262890683122, 1.000000000000000000, 0.9659258262890683122, 1.000000000000000000, 0.9659258262890683122, 1.000000000000000000, 0.9659258262890683122, 1.000000000000000000, 0.9659258262890683122, 1.000000000000000000, 0.9659258262890683122, 1.000000000000000000, 0.9659258262890683122, 1.000000000000000000, 0.9659258262890683122, 1.000000000000000000, 0.9659258262890683122, 1.000000000000000000, 0.9659258262890683122, 1.000000000000000000, 0.9659258262890683122, 1.000000000000000000, 0.9659258262890683122, 1.000000000000000000, 0.9659258262890683122, 1.000000000000000000, 0.9659258262890683122, 1.000000000000000000, 0.9659258262890683122, 1.000000000000000000, 0.9659258262890683122, 1.000000000000000000, 0.9659258262890683122, 1.000000000000000000, 0.9659258262890683122, 1.000000000000000000, 0.9659258262890683122, 1.000000000000000000, 0.9659258262890683122, 1.000000000000000000, 0.9659258262890683122, 1.000000000000000000, 0.9659258262890683122, 1.000000000000000000, 0.9659258262890683122, 1.000000000000000000, 0.9659258262890683122, 1.000000000000000000, 0.9659258262890683122, 1.000000000000000000, 0.9659258262890683122, 1.000000000000000000, 0.9659258262890683122, 1.000000000000000000, 0.9659258262890683122, 1.000000000000000000, 0.9659258262890683122, 1.000000000000000000, 0.9659258262890683122, 1.000000000000000000, 0.9659258262890683122, 1.000000000000000000, 0.9659258262890683122, 1.000000000000000000, 0.9659258262890683122, 1.000000000000000000, 0.9659258262890683122, 1.000000000000000000, 0.9659258262890683122, 1.000000000000000000, 0.9659258262890683122, 1.000000000000000000, 0.9659258262890683122, 1.000000000000000000, 0.9659258262890683122, 1.000000000000000000, 0.9659258262890683122, 1.000000000000000000, 0.9659258262890683122, 1.000000000000000000, 0.9659258262890683122, 1.000000000000000000, 0.9659258262890683122, 1.000000000000000000, 0.9659258262890683122, 1.000000000000000000, 0.9659258262890683122, 1.000000000000000000, 0.9659258262890683122, 1.000000000000000000, 0.9659258262890683122, 1.000000000000000000, 0.9659258262890683122, 1.000000000000000000, 0.9659258262890683122, 1.000000000000000000, 0.9659258262890683122, 1.000000000000000000, 0.9659258262890683122, 1.000000000000000000, 0.9659258262890683122, 1.000000000000000000, 0.9659258262890683122, 1.000000000000000000, 0.9659258262890683122, 1.000000000000000000, 0.9659258262890683122, 1.000000000000000000, 0.9659258262890683122, 1.000000000000000000, 0.9659258262890683122, 1.000000000000000000, 0.9659258262890683122, 1.000000000000000000, 0.9659258262890683122, 1.000000000000000000, 0.9659258262890683122, 1.000000000000000000, 0.9659258262890683122, 1.000000000000000000, 0.9659258262890683122, 1.000000000000000000, 0.9659258262890683122, 1.000000000000000000, 0.9659258262890683122, 1.000000000000000000, 0.9659258262890683122, 1.000000000000000000, 0.9659258262890683122, 1.000000000000000000, 0.9659258262890683122, 1.000000000000000000, 0.9659258262890683122, 1.000000000000000000, 0.9659258262890683122, 1.000000000000000000, 0.9659258262890683122, 1.000000000000000000, 0.9659258262890683122, 1.000000000000000000, 0.9659258262890683122, 1.000000000000000000, 0.9659258262890683122, 1.000000000000000000, 0.9659258262890683122, 1.000000000000000000, 0.9659258262890683122, 1.000000000000000000, 0.9659258262890683122, 1.000000000000000000, 0.9659258262890683122, 1.000000000000000000, 0.9659258262890683122, 1.000000000000000000, 0.9659258262890683122, 1.000000000000000000, 0.9659258262890683122, 1.000000000000000000, 0.9659258262890683122, 1.000000000000000000, 0.9659258262890683122, 1.000000000000000000, 0.9659258262890683122, 1.000000000000000000, 0.9659258262890683122, 1.000000000000000000, 0.9659258262890683122, 1.000000000000000000, 0.9659258262890683122, 1.000000000000000000, 0.9659258262890683122, 1.000000000000000000, 0.9659258262890683122, 1.000000000000000000, 0.9659258262890683122, 1.000000000000000000, 0.9659258262890683122, 1.000000000000000000, 0.9659258262890683122, 1.000000000000000000, 0.9659258262890683122, 1.000000000000000000, 0.9659258262890683122, 1.000000000000000000, 0.9659258262890683122, 1.000000000000000000, 0.9659258262890683122, 1.000000000000000000, 0.9659258262890683122, 1.000000000000000000, 0.9659258262890683122, 1.000000000000000000, 0.9659258262890683122, 1.000000000000000000, 0.9659258262890683122, 1.000000000000000000, 0.9659258262890683122, 1.000000000000000000, 0.9659258262890683122, 1.000000000000000000, 0.9659258262890683122, 1.000000000000000000, 0.9659258262890683122, 1.000000000000000000, 0.9659258262890683122, 1.000000000000000000),
 ( 1.000000000000000000, 0.9659258262890683122, 1.000000000000000000, 0.9659258262890683122, 1.000000000000000000, 0.9659258262890683122, 1.000000000000000000, 0.9659258262890683122, 1.000000000000000000, 0.9659258262890683122, 1.000000000000000000, 0.9659258262890683122, 1.000000000000000000, 0.9659258262890683122, 1.000000000000000000, 0.9659258262890683122, 1.000000000000000000, 0.9659258262890683122, 1.000000000000000000, 0.9659258262890683122, 1.000000000000000000, 0.9659258262890683122, 1.000000000000000000, 0.9659258262890683122, 1.000000000000000000, 0.9659258262890683122, 1.000000000000000000, 0.9659258262890683122, 1.000000000000000000, 0.9659258262890683122, 1.000000000000000000, 0.9659258262890683122, 1.000000000000000000, 0.9659258262890683122, 1.000000000000000000, 0.9659258262890683122, 1.000000000000000000, 0.9659258262890683122, 1.000000000000000000, 0.9659258262890683122, 1.000000000000000000, 0.9659258262890683122, 1.000000000000000000, 0.9659258262890683122, 1.000000000000000000, 0.9659258262890683122, 1.000000000000000000, 0.9659258262890683122, 1.000000000000000000, 0.9659258262890683122, 1.000000000000000000, 0.9659258262890683122, 1.000000000000000000, 0.9659258262890683122, 1.000000000000000000, 0.9659258262890683122, 1.000000000000000000, 0.9659258262890683122, 1.000000000000000000, 0.9659258262890683122, 1.000000000000000000, 0.9659258262890683122, 1.000000000000000000, 0.9659258262890683122, 1.000000000000000000, 0.9659258262890683122, 1.000000000000000000, 0.9659258262890683122, 1.000000000000000000, 0.9659258262890683122, 1.000000000000000000, 0.9659258262890683122, 1.000000000000000000, 0.9659258262890683122, 1.000000000000000000, 0.9659258262890683122, 1.000000000000000000, 0.9659258262890683122, 1.000000000000000000, 0.9659258262890683122, 1.000000000000000000, 0.9659258262890683122, 1.000000000000000000, 0.9659258262890683122, 1.000000000000000000, 0.9659258262890683122, 1.000000000000000000, 0.9659258262890683122, 1.000000000000000000, 0.9659258262890683122, 1.000000000000000000, 0.9659258262890683122, 1.000000000000000000, 0.9659258262890683122, 1.000000000000000000, 0.9659258262890683122, 1.000000000000000000, 0.9659258262890683122, 1.000000000000000000, 0.9659258262890683122, 1.000000000000000000, 0.9659258262890683122, 1.000000000000000000, 0.9659258262890683122, 1.000000000000000000, 0.9659258262890683122, 1.000000000000000000, 0.9659258262890683122, 1.000000000000000000, 0.9659258262890683122, 1.000000000000000000, 0.9659258262890683122, 1.000000000000000000, 0.9659258262890683122, 1.000000000000000000, 0.9659258262890683122, 1.000000000000000000, 0.9659258262890683122, 1.000000000000000000, 0.9659258262890683122, 1.000000000000000000, 0.9659258262890683122, 1.000000000000000000, 0.9659258262890683122, 1.000000000000000000, 0.9659258262890683122, 1.000000000000000000, 0.9659258262890683122, 1.000000000000000000, 0.9659258262890683122, 1.000000000000000000, 0.9659258262890683122, 1.000000000000000000, 0.9659258262890683122, 1.000000000000000000, 0.9659258262890683122, 1.000000000000000000, 0.9659258262890683122, 1.000000000000000000, 0.9659258262890683122, 1.000000000000000000, 0.9659258262890683122, 1.000000000000000000, 0.9659258262890683122, 1.000000000000000000, 0.9659258262890683122, 1.000000000000000000, 0.9659258262890683122, 1.000000000000000000, 0.9659258262890683122, 1.000000000000000000, 0.9659258262890683122, 1.000000000000000000, 0.9659258262890683122, 1.000000000000000000, 0.9659258262890683122, 1.000000000000000000, 0.9659258262890683122, 1.000000000000000000, 0.9659258262890683122, 1.000000000000000000, 0.9659258262890683122, 1.000000000000000000, 0.9659258262890683122, 1.000000000000000000, 0.9659258262890683122, 1.000000000000000000, 0.9659258262890683122, 1.000000000000000000, 0.9659258262890683122, 1.000000000000000000, 0.9659258262890683122, 1.000000000000000000, 0.9659258262890683122, 1.000000000000000000, 0.9659258262890683122, 1.000000000000000000, 0.9659258262890683122, 1.000000000000000000, 0.9659258262890683122, 1.000000000000000000, 0.9659258262890683122, 1.000000000000000000, 0.9659258262890683122, 1.000000000000000000, 0.9659258262890683122, 1.000000000000000000, 0.9659258262890683122, 1.000000000000000000, 0.9659258262890683122, 1.000000000000000000, 0.9659258262890683122, 1.000000000000000000, 0.9659258262890683122, 1.000000000000000000, 0.9659258262890683122, 1.000000000000000000, 0.9659258262890683122, 1.000000000000000000, 0.9659258262890683122, 1.000000000000000000, 0.9659258262890683122, 1.000000000000000000, 0.9659258262890683122, 1.000000000000000000, 0.9659258262890683122, 1.000000000000000000, 0.9659258262890683122, 1.000000000000000000, 0.9659258262890683122, 1.000000000000000000, 0.9659258262890683122, 1.000000000000000000, 0.9659258262890683122, 1.000000000000000000, 0.9659258262890683122, 1.000000000000000000, 0.9659258262890683122, 1.000000000000000000, 0.9659258262890683122, 1.000000000000000000, 0.9659258262890683122, 1.000000000000000000, 0.9659258262890683122, 1.000000000000000000, 0.9659258262890683122, 1.000000000000000000, 0.9659258262890683122, 1.000000000000000000, 0.9659258262890683122, 1.000000000000000000, 0.9659258262890683122, 1.000000000000000000, 0.9659258262890683122, 1.000000000000000000, 0.9659258262890683122, 1.000000000000000000, 0.9659258262890683122, 1.000000000000000000, 0.9659258262890683122, 1.000000000000000000, 0.9659258262890683122, 1.000000000000000000, 0.9659258262890683122, 1.000000000000000000, 0.9659258262890683122, 1.000000000000000000, 0.9659258262890683122, 1.000000000000000000, 0.9659258262890683122, 1.000000000000000000, 0.9659258262890683122, 1.000000000000000000, 0.9659258262890683122, 1.000000000000000000, 0.9659258262890683122, 1.000000000000000000, 0.9659258262890683122, 1.000000000000000000, 0.9659258262890683122, 1.000000000000000000, 0.9659258262890683122, 1.000000000000000000, 0.9659258262890683122, 1.000000000000000000, 0.9659258262890683122, 1.000000000000000000, 0.9659258262890683122, 1.000000000000000000, 0.9659258262890683122, 1.000000000000000000, 0.9659258262890683122, 1.000000000000000000, 0.9659258262890683122, 1.000000000000000000, 0.9659258262890683122, 1.000000000000000000, 0.9659258262890683122, 1.000000000000000000, 0.9659258262890683122, 1.000000000000000000, 0.9659258262890683122, 1.000000000000000000, 0.9659258262890683122, 1.000000000000000000, 0.9659258262890683122, 1.000000000000000000, 0.9659258262890683122, 1.000000000000000000, 0.9659258262890683122, 1.000000000000000000, 0.9659258262890683122, 1.000000000000000000, 0.9659258262890683122, 1.000000000000000000, 0.9659258262890683122, 1.000000000000000000, 0.9659258262890683122, 1.000000000000000000, 0.9659258262890683122, 1.000000000000000000, 0.9659258262890683122, 1.000000000000000000, 0.9659258262890683122, 1.000000000000000000, 0.9659258262890683122, 1.000000000000000000, 0.9659258262890683122, 1.000000000000000000, 0.9659258262890683122, 1.000000000000000000, 0.9659258262890683122, 1.000000000000000000, 0.9659258262890683122, 1.000000000000000000, 0.9659258262890683122, 1.000000000000000000, 0.9659258262890683122, 1.000000000000000000, 0.9659258262890683122, 1.000000000000000000, 0.9659258262890683122, 1.000000000000000000, 0.9659258262890683122, 1.000000000000000000, 0.9659258262890683122, 1.000000000000000000, 0.9659258262890683122, 1.000000000000000000, 0.9659258262890683122, 1.000000000000000000, 0.9659258262890683122, 1.000000000000000000, 0.9659258262890683122, 1.000000000000000000, 0.9659258262890683122, 1.000000000000000000, 0.9659258262890683122, 1.000000000000000000, 0.9659258262890683122, 1.000000000000000000, 0.9659258262890683122, 1.000000000000000000, 0.9659258262890683122, 1.000000000000000000, 0.9659258262890683122, 1.000000000000000000, 0.9659258262890683122, 1.000000000000000000, 0.9659258262890683122, 1.000000000000000000, 0.9659258262890683122, 1.000000000000000000, 0.9659258262890683122, 1.000000000000000000, 0.9659258262890683122, 1.000000000000000000, 0.9659258262890683122, 1.000000000000000000, 0.9659258262890683122, 1.000000000000000000, 0.9659258262890683122, 1.000000000000000000, 0.9659258262890683122, 1.000000000000000000, 0.9659258262890683122, 1.000000000000000000, 0.9659258262890683122, 1.000000000000000000, 0.9659258262890683122, 1.000000000000000000, 0.9659258262890683122, 1.000000000000000000, 0.9659258262890683122, 1.000000000000000000, 0.9659258262890683122, 1.000000000000000000, 0.9659258262890683122, 1.000000000000000000, 0.9659258262890683122, 1.000000000000000000, 0.9659258262890683122, 1.000000000000000000, 0.9659258262890683122, 1.000000000000000000, 0.9659258262890683122, 1.000000000000000000, 0.9659258262890683122, 1.000000000000000000, 0.9659258262890683122, 1.000000000000000000, 0.9659258262890683122, 1.000000000000000000, 0.9659258262890683122, 1.000000000000000000, 0.9659258262890683122, 1.000000000000000000, 0.9659258262890683122, 1.000000000000000000, 0.9659258262890683122, 1.000000000000000000, 0.9659258262890683122, 1.000000000000000000, 0.9659258262890683122, 1.000000000000000000, 0.9659258262890683122, 1.000000000000000000, 0.9659258262890683122, 1.000000000000000000, 0.9659258262890683122, 1.000000000000000000, 0.9659258262890683122, 1.000000000000000000, 0.9659258262890683122, 1.000000000000000000, 0.9659258262890683122, 1.000000000000000000, 0.9659258262890683122, 1.000000000000000000, 0.9659258262890683122, 1.000000000000000000, 0.9659258262890683122, 1.000000000000000000, 0.9659258262890683122, 1.000000000000000000, 0.9659258262890683122, 1.000000000000000000, 0.9659258262890683122, 1.000000000000000000, 0.9659258262890683122, 1.000000000000000000, 0.9659258262890683122, 1.000000000000000000, 0.9659258262890683122, 1.000000000000000000, 0.9659258262890683122, 1.000000000000000000, 0.9659258262890683122, 1.000000000000000000, 0.9659258262890683122, 1.000000000000000000, 0.9659258262890683122, 1.000000000000000000, 0.9659258262890683122, 1.000000000000000000, 0.9659258262890683122, 1.000000000000000000, 0.9659258262890683122, 1.000000000000000000, 0.9659258262890683122, 1.000000000000000000, 0.9659258262890683122, 1.000000000000000000, 0.9659258262890683122, 1.000000000000000000, 0.9659258262890683122, 1.000000000000000000, 0.9659258262890683122, 1.000000000000000000, 0.9659258262890683122, 1.000000000000000000, 0.9659258262890683122, 1.000000000000000000, 0.9659258262890683122, 1.000000000000000000, 0.9659258262890683122, 1.000000000000000000, 0.9659258262890683122, 1.000000000000000000, 0.9659258262890683122, 1.000000000000000000, 0.9659258262890683122, 1.000000000000000000, 0.9659258262890683122, 1.000000000000000000, 0.9659258262890683122, 1.000000000000000000, 0.9659258262890683122, 1.000000000000000000, 0.9659258262890683122, 1.000000000000000000, 0.9659258262890683122, 1.000000000000000000, 0.9659258262890683122, 1.000000000000000000, 0.9659258262890683122, 1.000000000000000000, 0.9659258262890683122, 1.000000000000000000, 0.9659258262890683122, 1.000000000000000000, 0.9659258262890683122, 1.000000000000000000, 0.9659258262890683122, 1.000000000000000000, 0.9659258262890683122, 1.000000000000000000, 0.9659258262890683122, 1.000000000000000000, 0.9659258262890683122, 1.000000000000000000, 0.9659258262890683122, 1.000000000000000000, 0.9659258262890683122, 1.000000000000000000, 0.9659258262890683122, 1.000000000000000000, 0.9659258262890683122, 1.000000000000000000, 0.9659258262890683122, 1.000000000000000000) ) ) 
 REPRESENTATION_ITEM ( '' )  SURFACE ( )  );
#4102 = EDGE_CURVE ( 'NONE', #59692, #37337, #74231, .T. ) ;
#4103 = CARTESIAN_POINT ( 'NONE',  ( 0.09186351706036827158, 0.05413385826771666132, 0.4176697321401328100 ) ) ;
#4104 = CARTESIAN_POINT ( 'NONE',  ( -0.8923884514435688198, -0.6046776061558807314, 0.2411417322834647770 ) ) ;
#4105 = CARTESIAN_POINT ( 'NONE',  ( 1.246719160104987623, 0.05413385826771626580, -0.4176697321401330321 ) ) ;
#4106 = CARTESIAN_POINT ( 'NONE',  ( -0.3458507752293906723, -0.3458507752293910609, -1.161417322834645383 ) ) ;
#4107 = CARTESIAN_POINT ( 'NONE',  ( 0.1998031496062994405, -0.3460692066303958092, -2.454068241469816058 ) ) ;
#4108 = CARTESIAN_POINT ( 'NONE',  ( 0.3018372703412079971, -0.3690944881889763329, 0.3153832671262228327 ) ) ;
#4109 = ORIENTED_EDGE ( 'NONE', *, *, #79680, .F. ) ;
#4110 = CARTESIAN_POINT ( 'NONE',  ( -0.3917322834645670104, -0.1049643490035307020, -0.8300718092201594400 ) ) ;
#4111 = ORIENTED_EDGE ( 'NONE', *, *, #15570, .T. ) ;
#4112 = EDGE_CURVE ( 'NONE', #40260, #33327, #71513, .T. ) ;
#4113 = CARTESIAN_POINT ( 'NONE',  ( -0.6561679790026240244, -0.6046776061558807314, 0.2411417322834647770 ) ) ;
#4114 = CARTESIAN_POINT ( 'NONE',  ( -0.2493438320209966919, -0.4281496062992124485, 0.4176697321401328655 ) ) ;
#4115 = CARTESIAN_POINT ( 'NONE',  ( -0.2362204724409440182, -0.1870078740157479769, 0.4822834645669291653 ) ) ;
#4116 = CARTESIAN_POINT ( 'NONE',  ( 0.7742782152230979209, 0.05413385826771626580, -0.4176697321401330321 ) ) ;
#4117 = CARTESIAN_POINT ( 'NONE',  ( -1.397637795275589623, -0.5400638737290845981, -0.3530559997133363437 ) ) ;
#4118 = CARTESIAN_POINT ( 'NONE',  ( -0.5643044619422565855, 0.05413385826771626580, -0.4176697321401330321 ) ) ;
#4119 = CARTESIAN_POINT ( 'NONE',  ( 0.5839895013123367340, -0.6692913385826773087, -0.1292274648535924053 ) ) ;
#4120 = CARTESIAN_POINT ( 'NONE',  ( 0.2821522309711292364, -0.6692913385826771977, 0.1292274648535927661 ) ) ;
#4121 = CARTESIAN_POINT ( 'NONE',  ( 0.8398950131233602345, -0.6046776061558807314, 0.2411417322834647770 ) ) ;
#4122 = CARTESIAN_POINT ( 'NONE',  ( -0.2867679344610365999, 0.2867679344610364889, -0.9566929133858265155 ) ) ;
#4123 = CARTESIAN_POINT ( 'NONE',  ( -0.2165354330708654795, 0.07958543189024085140, 0.2665933059059887866 ) ) ;
#4124 = VERTEX_POINT ( 'NONE', #61129 ) ;
#4125 = CARTESIAN_POINT ( 'NONE',  ( -9.674558042662121740E-17, 0.3949938075777409963, -1.259842519685039353 ) ) ;
#4126 = ORIENTED_EDGE ( 'NONE', *, *, #32799, .F. ) ;
#4127 = CARTESIAN_POINT ( 'NONE',  ( -1.089238845144356427, -0.004921259842519576551, 0.3153832671262227771 ) ) ;
#4128 = CARTESIAN_POINT ( 'NONE',  ( -0.5249343832020990641, 0.2306618581243848609, 0.2411417322834645549 ) ) ;
#4129 = DIRECTION ( 'NONE',  ( 0.000000000000000000, -1.000000000000000000, 0.000000000000000000 ) ) ;
#4130 = CARTESIAN_POINT ( 'NONE',  ( -0.8727034120734901146, -0.05778040916215560624, -0.4822834645669293319 ) ) ;
#4131 = CARTESIAN_POINT ( 'NONE',  ( -0.9251968503937002541, 0.1660481256975885056, 0.3530559997133364547 ) ) ;
#4132 = CARTESIAN_POINT ( 'NONE',  ( -1.220472440944881054, -0.6692913385826771977, 8.415575281601705876E-17 ) ) ;
#4133 = CARTESIAN_POINT ( 'NONE',  ( -1.272965879265091305, -0.4281496062992124485, 0.4176697321401328655 ) ) ;
#4134 = CARTESIAN_POINT ( 'NONE',  ( 0.8989501312335964611, 0.1771653543307087630, 0.09757992244046791164 ) ) ;
#4135 = DIRECTION ( 'NONE',  ( 1.047444401652940007E-14, -0.000000000000000000, -1.000000000000000000 ) ) ;
#4136 = CARTESIAN_POINT ( 'NONE',  ( -0.1958661417322834220, -0.3392501089628018884, 0.007217847769028785422 ) ) ;
#4137 = CARTESIAN_POINT ( 'NONE',  ( 0.01968503937007930540, 0.07958543189024085140, 0.2665933059059887866 ) ) ;
#4138 = CARTESIAN_POINT ( 'NONE',  ( -0.2165354330708654795, 0.1660481256975885056, 0.3530559997133364547 ) ) ;
#4139 = CARTESIAN_POINT ( 'NONE',  ( 0.03280839895013198948, -0.6692913385826773087, -0.1292274648535924053 ) ) ;
#4140 = VERTEX_POINT ( 'NONE', #23240 ) ;
#4141 = CARTESIAN_POINT ( 'NONE',  ( -9.787531504996567848E-17, 0.3996062992125986035, -2.204724409448818978 ) ) ;
#4142 = DIRECTION ( 'NONE',  ( -3.491481338843132961E-15, -0.000000000000000000, 1.000000000000000000 ) ) ;
#4143 = ORIENTED_EDGE ( 'NONE', *, *, #24144, .T. ) ;
#4144 = CARTESIAN_POINT ( 'NONE',  ( -0.1070741851644051862, -0.3996062992125986590, -1.408792650918635259 ) ) ;
#4145 = DIRECTION ( 'NONE',  ( 0.000000000000000000, 1.000000000000000000, -0.000000000000000000 ) ) ;
#4146 = CARTESIAN_POINT ( 'NONE',  ( -0.8398950131233589023, -0.5023911411419708095, -0.1820866141732282451 ) ) ;
#4147 = CARTESIAN_POINT ( 'NONE',  ( -0.8989501312335946848, 0.2952755905511810774, -0.1292274648535930714 ) ) ;
#4148 = CARTESIAN_POINT ( 'NONE',  ( 0.1265901696524990294, -0.4724409448818896462, -0.5577427821522309426 ) ) ;
#4149 = CARTESIAN_POINT ( 'NONE',  ( -0.06215213303350786145, 1.066820816534554961, 3.936548056194433265 ) ) ;
#4150 = CARTESIAN_POINT ( 'NONE',  ( 0.2867679344610365999, -0.2867679344610365444, -2.702755905511810663 ) ) ;
#4151 = CARTESIAN_POINT ( 'NONE',  ( 1.391076115485564868, 0.2306618581243847221, -0.2411417322834647770 ) ) ;
#4152 = CARTESIAN_POINT ( 'NONE',  ( 0.4461942257217855201, -0.6046776061558807314, 0.2411417322834647770 ) ) ;
#4153 = CARTESIAN_POINT ( 'NONE',  ( 0.6496062992125991586, -0.5400638737290845981, -0.3530559997133363437 ) ) ;
#4154 = CARTESIAN_POINT ( 'NONE',  ( -0.8398950131233585692, 0.1283753931104748280, 0.1820866141732283561 ) ) ;
#4155 = CARTESIAN_POINT ( 'NONE',  ( 0.1443569553805781891, -0.4281496062992124485, 0.4176697321401328655 ) ) ;
#4156 = CARTESIAN_POINT ( 'NONE',  ( 0.4724409448818897572, -0.1265901696524988906, -2.235564304461942431 ) ) ;
#4157 = CARTESIAN_POINT ( 'NONE',  ( -0.4002624671916004129, -0.05778040916215560624, -0.4822834645669293319 ) ) ;
#4158 = CARTESIAN_POINT ( 'NONE',  ( -0.2891555358219911054, 0.2891555358219909388, -1.986220472440945128 ) ) ;
#4159 = CARTESIAN_POINT ( 'NONE',  ( 1.397637795275591177, -0.4536011799217367080, 0.2665933059059888421 ) ) ;
#4160 = CARTESIAN_POINT ( 'NONE',  ( -0.4593175853018366950, -0.004921259842519576551, 0.3153832671262227771 ) ) ;
#4161 = CARTESIAN_POINT ( 'NONE',  ( 0.9776902887139113929, -0.5511811023622048555, -0.09757992244046775898 ) ) ;
#4162 = CARTESIAN_POINT ( 'NONE',  ( -1.043307086614172707, 0.1660481256975883668, -0.3530559997133364547 ) ) ;
#4163 = AXIS2_PLACEMENT_3D ( 'NONE', #20077, #40268, #21329 ) ;
#4164 = CARTESIAN_POINT ( 'NONE',  ( -1.102362204724408601, -0.1870078740157480601, -0.3641732283464567677 ) ) ;
#4165 = CARTESIAN_POINT ( 'NONE',  ( 0.1467811222005255545, 2.110655687203366066E-15, -0.4118477457932985253 ) ) ;
#4166 = CARTESIAN_POINT ( 'NONE',  ( -1.187664041994750175, -0.05778040916215560624, -0.4822834645669293319 ) ) ;
#4167 = CARTESIAN_POINT ( 'NONE',  ( -0.3608923884514428360, 0.2952755905511811885, 0.1292274648535926551 ) ) ;
#4168 = CARTESIAN_POINT ( 'NONE',  ( 0.3740157480314966754, -0.5400638737290844871, 0.3530559997133364547 ) ) ;
#4169 = CARTESIAN_POINT ( 'NONE',  ( 0.3917322834645669549, 2.398668435337827645E-17, -2.402867823325772090 ) ) ;
#4170 = CARTESIAN_POINT ( 'NONE',  ( 0.2887139107611556010, 0.2306618581243847221, -0.2411417322834647770 ) ) ;
#4171 = CARTESIAN_POINT ( 'NONE',  ( 0.3412073490813655186, -0.5023911411419708095, -0.1820866141732282451 ) ) ;
#4172 = CARTESIAN_POINT ( 'NONE',  ( -1.450131233595799651, -0.5511811023622046335, 0.09757992244046803654 ) ) ;
#4173 = CARTESIAN_POINT ( 'NONE',  ( 0.8727034120734913358, -0.05778040916215522460, 0.4822834645669289988 ) ) ;
#4174 = CARTESIAN_POINT ( 'NONE',  ( -1.417322834645668772, -0.1870078740157479769, 0.3641732283464567677 ) ) ;
#4175 = CARTESIAN_POINT ( 'NONE',  ( 1.207349081364829990, -0.5023911411419708095, -0.1820866141732282451 ) ) ;
#4176 = ADVANCED_FACE ( 'NONE', ( #74192 ), #33900, .T. ) ;
#4177 = CARTESIAN_POINT ( 'NONE',  ( -0.8989501312335946848, 0.2952755905511810774, -0.1292274648535930714 ) ) ;
#4178 = CARTESIAN_POINT ( 'NONE',  ( -0.3346456692913377662, 0.07958543189024071263, -0.2665933059059888421 ) ) ;
#4179 = CARTESIAN_POINT ( 'NONE',  ( 1.034321223653608346, 4.339766966676338660E-16, 0.4118484887281966822 ) ) ;
#4180 = CARTESIAN_POINT ( 'NONE',  ( 0.8530183727034126306, -0.004921259842519870586, -0.3153832671262229437 ) ) ;
#4181 = PRESENTATION_LAYER_ASSIGNMENT (  '', '', ( #27010 ) ) ;
#4182 = CARTESIAN_POINT ( 'NONE',  ( 0.1115485564304470323, 0.2952755905511811885, 0.1292274648535926551 ) ) ;
#4183 = CARTESIAN_POINT ( 'NONE',  ( 0.2925321140481932369, 0.2925321140481932369, -0.5295275590551181688 ) ) ;
#4184 = CARTESIAN_POINT ( 'NONE',  ( -0.3917322834645669549, -0.1049643490035306603, -1.862860892388451761 ) ) ;
#4185 = CARTESIAN_POINT ( 'NONE',  ( 0.5118110236220478892, 0.1771653543307087630, 0.000000000000000000 ) ) ;
#4186 = CARTESIAN_POINT ( 'NONE',  ( 0.1509186351706045259, -0.05778040916215560624, -0.4822834645669293319 ) ) ;
#4187 = CARTESIAN_POINT ( 'NONE',  ( -0.5446194225721777693, -0.05778040916215522460, 0.4822834645669289988 ) ) ;
#4188 = CARTESIAN_POINT ( 'NONE',  ( -0.3477690288713902178, 0.1771653543307087075, -0.09757992244046823083 ) ) ;
#4189 = FACE_OUTER_BOUND ( 'NONE', #46215, .T. ) ;
#4190 = CARTESIAN_POINT ( 'NONE',  ( -0.4396325459317577122, -0.5511811023622048555, -0.09757992244046775898 ) ) ;
#4191 = CARTESIAN_POINT ( 'NONE',  ( -0.1443569553805765515, -0.4281496062992127816, -0.4176697321401328100 ) ) ;
#4192 = CARTESIAN_POINT ( 'NONE',  ( -1.076115485564303809, 0.1283753931104748280, 0.1820866141732283561 ) ) ;
#4193 = CARTESIAN_POINT ( 'NONE',  ( -0.3460692066303957537, -0.1998031496062994405, -1.231627296587926690 ) ) ;
#4194 = CARTESIAN_POINT ( 'NONE',  ( 1.535433070866142335, -0.6692913385826771977, 8.415575281601705876E-17 ) ) ;
#4195 = DIRECTION ( 'NONE',  ( -0.000000000000000000, -1.000000000000000000, -0.000000000000000000 ) ) ;
#4196 = ORIENTED_EDGE ( 'NONE', *, *, #45967, .F. ) ;
#4197 = CARTESIAN_POINT ( 'NONE',  ( -1.345144356955379816, -0.08942795157528024563, -0.3641732283464568787 ) ) ;
#4198 = CARTESIAN_POINT ( 'NONE',  ( -0.6627296587926503335, -0.6692913385826771977, 0.1292274648535927661 ) ) ;
#4199 = CARTESIAN_POINT ( 'NONE',  ( -1.259842519685038686, -0.1870078740157480879, -0.4822834645669291653 ) ) ;
#4200 = CARTESIAN_POINT ( 'NONE',  ( 0.2867679344610365999, -0.2867679344610365444, -1.757874015748031260 ) ) ;
#4201 = CARTESIAN_POINT ( 'NONE',  ( 0.000000000000000000, 2.145669291338582418, -0.3129921259842520787 ) ) ;
#4202 = CARTESIAN_POINT ( 'NONE',  ( 1.318897637795276356, -0.5400638737290844871, 0.3530559997133364547 ) ) ;
#4203 = CARTESIAN_POINT ( 'NONE',  ( 0.4593175853018380828, 0.05413385826771626580, -0.4176697321401330321 ) ) ;
#4204 = CARTESIAN_POINT ( 'NONE',  ( -0.2952755905511810774, -3.179810529374183920E-17, 5.879133660591329580 ) ) ;
#4205 = CARTESIAN_POINT ( 'NONE',  ( -0.1070741851644057135, 0.3996062992125984925, -2.288057742782152015 ) ) ;
#4206 = CARTESIAN_POINT ( 'NONE',  ( 1.469816272965879911, 0.1283753931104746893, -0.1820866141732285504 ) ) ;
#4207 = CARTESIAN_POINT ( 'NONE',  ( 0.1070741851644053527, 0.3996062992125986590, -0.9383202099737533164 ) ) ;
#4208 = VERTEX_POINT ( 'NONE', #74610 ) ;
#4209 = CARTESIAN_POINT ( 'NONE',  ( -0.9383202099737524282, -0.2845877964562161244, -0.3641732283464567121 ) ) ;
#4210 = CARTESIAN_POINT ( 'NONE',  ( -9.594673741351313045E-17, 0.3917322834645670104, -2.669291338582676865 ) ) ;
#4211 = EDGE_LOOP ( 'NONE', ( #5382, #28024, #47075, #2567 ) ) ;
#4212 = CARTESIAN_POINT ( 'NONE',  ( 0.5118110236220478892, 0.2952755905511811885, 0.000000000000000000 ) ) ;
#4213 = CARTESIAN_POINT ( 'NONE',  ( -0.3805774278215216522, -0.4281496062992127816, -0.4176697321401328100 ) ) ;
#4214 = CARTESIAN_POINT ( 'NONE',  ( -0.9776902887139098386, 0.2952755905511810774, -0.1292274648535930714 ) ) ;
#4215 = CARTESIAN_POINT ( 'NONE',  ( 0.8858267716535438430, 0.1660481256975885056, 0.3530559997133364547 ) ) ;
#4216 = CARTESIAN_POINT ( 'NONE',  ( -1.318897637795274802, 0.07958543189024085140, 0.2665933059059887866 ) ) ;
#4217 = FACE_OUTER_BOUND ( 'NONE', #63842, .T. ) ;
#4218 = CARTESIAN_POINT ( 'NONE',  ( -0.1902887139107604098, 0.2952755905511810774, -0.1292274648535930714 ) ) ;
#4219 = CARTESIAN_POINT ( 'NONE',  ( -0.9776902887139098386, 0.2952755905511810774, -0.1292274648535930714 ) ) ;
#4220 = CARTESIAN_POINT ( 'NONE',  ( -0.3392501089628018329, -0.1958661417322836440, -2.179770710464879802 ) ) ;
#4221 = CARTESIAN_POINT ( 'NONE',  ( -1.469816272965878357, 0.2306618581243848609, 0.2411417322834645549 ) ) ;
#4222 = CARTESIAN_POINT ( 'NONE',  ( -0.7426113562971992099, 2.401574803149605586, 0.5309055118110236338 ) ) ;
#4223 = CARTESIAN_POINT ( 'NONE',  ( -0.1958661417322836718, 0.3392501089628017219, 0.1522309711286089495 ) ) ;
#4224 = CARTESIAN_POINT ( 'NONE',  ( 0.9317585301837276734, -0.004921259842519870586, -0.3153832671262229437 ) ) ;
#4225 = EDGE_LOOP ( 'NONE', ( #17684, #71836, #29859, #26567, #54119, #10477, #4938, #19031, #39331, #65925, #4973, #83294, #3190, #37449 ) ) ;
#4226 = CARTESIAN_POINT ( 'NONE',  ( 0.1974969037888706369, -0.3420746716998659953, -0.09186351706036749443 ) ) ;
#4227 = CARTESIAN_POINT ( 'NONE',  ( -0.2362204724409440182, -0.1870078740157479769, 0.4822834645669291653 ) ) ;
#4228 = ORIENTED_EDGE ( 'NONE', *, *, #74315, .F. ) ;
#4229 = CARTESIAN_POINT ( 'NONE',  ( 0.4396325459317590445, -0.5511811023622046335, 0.09757992244046803654 ) ) ;
#4230 = CARTESIAN_POINT ( 'NONE',  ( -1.417322834645668772, -0.1870078740157479769, 0.4822834645669291653 ) ) ;
#4231 = CARTESIAN_POINT ( 'NONE',  ( 0.5052493438320215802, 0.2952755905511811885, 0.1292274648535926551 ) ) ;
#4232 = CARTESIAN_POINT ( 'NONE',  ( 0.5380577427821529035, 0.05413385826771626580, -0.4176697321401330321 ) ) ;
#4233 = CARTESIAN_POINT ( 'NONE',  ( 0.04593175853018440641, 0.2952755905511810774, -0.1292274648535930714 ) ) ;
#4234 = CARTESIAN_POINT ( 'NONE',  ( -0.2867679344610367109, 0.2867679344610365444, -1.118785719981314264 ) ) ;
#4235 = CARTESIAN_POINT ( 'NONE',  ( -0.9383202099737524282, -0.3162353388693409650, -0.4822834645669289433 ) ) ;
#4236 = CARTESIAN_POINT ( 'NONE',  ( 0.1958661417322836440, -0.3392501089628017219, -2.066272965879265122 ) ) ;
#4237 = CARTESIAN_POINT ( 'NONE',  ( 1.253280839895013710, -0.2845877964562159024, 0.3641732283464567677 ) ) ;
#4238 = CARTESIAN_POINT ( 'NONE',  ( -1.148293963254592542, 0.2952755905511811885, 0.1292274648535926551 ) ) ;
#4239 = CARTESIAN_POINT ( 'NONE',  ( 1.259842519685040019, -0.1870078740157480879, -0.4822834645669291653 ) ) ;
#4240 = CARTESIAN_POINT ( 'NONE',  ( 1.364829396325460076, 0.2306618581243848609, 0.2411417322834645549 ) ) ;
#4241 = ADVANCED_FACE ( 'NONE', ( #16954 ), #53093, .F. ) ;
#4242 = CARTESIAN_POINT ( 'NONE',  ( 0.1998031496062992740, 0.3460692066303959757, -0.4593175853018372501 ) ) ;
#4243 = CARTESIAN_POINT ( 'NONE',  ( -0.8858267716535425107, 0.1660481256975883668, -0.3530559997133364547 ) ) ;
#4244 = CARTESIAN_POINT ( 'NONE',  ( 0.1998031496062992463, 0.3460692066303959202, -0.06364829396325459576 ) ) ;
#4245 = EDGE_CURVE ( 'NONE', #44871, #73939, #73410, .T. ) ;
#4246 = CARTESIAN_POINT ( 'NONE',  ( 0.1443569553805781891, -0.4281496062992124485, 0.4176697321401328655 ) ) ;
#4247 = CARTESIAN_POINT ( 'NONE',  ( -0.2925321140481930704, -0.2925321140481933480, -2.106299212598425452 ) ) ;
#4248 = CARTESIAN_POINT ( 'NONE',  ( -0.6824146981627288167, 0.2306618581243848609, 0.2411417322834645549 ) ) ;
#4249 = CARTESIAN_POINT ( 'NONE',  ( 1.607611548556431069, -0.6692913385826773087, -0.1292274648535924053 ) ) ;
#4250 = CARTESIAN_POINT ( 'NONE',  ( 0.5249343832021005074, -0.5023911411419708095, 0.1820866141732285504 ) ) ;
#4251 = CARTESIAN_POINT ( 'NONE',  ( 1.181102362204724976, -0.1870078740157480879, -0.4822834645669291653 ) ) ;
#4252 = CARTESIAN_POINT ( 'NONE',  ( 0.4724409448818896462, 0.1265901696524990294, -1.146325459317585116 ) ) ;
#4253 = CARTESIAN_POINT ( 'NONE',  ( 0.7808398950131241190, -0.08942795157528024563, -0.3641732283464568787 ) ) ;
#4254 = CARTESIAN_POINT ( 'NONE',  ( 0.8267716535433077274, 0.2952755905511811885, 0.000000000000000000 ) ) ;
#4255 = CARTESIAN_POINT ( 'NONE',  ( 0.2891555358219910499, 0.2891555358219910499, -0.6870078740157480324 ) ) ;
#4256 = CARTESIAN_POINT ( 'NONE',  ( -0.7414698162729651543, 0.2952755905511810774, -0.1292274648535930714 ) ) ;
#4257 = CARTESIAN_POINT ( 'NONE',  ( 0.5314960629920847390, 2.755905511811024056, 3.937007874015794773 ) ) ;
#4258 = CARTESIAN_POINT ( 'NONE',  ( 1.437007874015748810, 0.07958543189024085140, 0.2665933059059887866 ) ) ;
#4259 = CARTESIAN_POINT ( 'NONE',  ( -0.4133858267716528645, 0.1660481256975883668, -0.3530559997133364547 ) ) ;
#4260 = CARTESIAN_POINT ( 'NONE',  ( 0.02624671916010564918, 0.2306618581243848609, 0.2411417322834645549 ) ) ;
#4261 = DIRECTION ( 'NONE',  ( 0.000000000000000000, 0.000000000000000000, 1.000000000000000000 ) ) ;
#4262 = CARTESIAN_POINT ( 'NONE',  ( 0.2099737532808405305, 0.2306618581243847221, -0.2411417322834647770 ) ) ;
#4263 = CARTESIAN_POINT ( 'NONE',  ( -0.02624671916010428221, 0.1283753931104746893, -0.1820866141732285504 ) ) ;
#4264 = CARTESIAN_POINT ( 'NONE',  ( -2.869792031447830905, 1.067551433859863952, -0.06782095098395297950 ) ) ;
#4265 = EDGE_CURVE ( 'NONE', #40586, #9070, #17368, .T. ) ;
#4266 = CARTESIAN_POINT ( 'NONE',  ( 0.1049868766404206816, 0.1283753931104748280, 0.1820866141732283561 ) ) ;
#4267 = CARTESIAN_POINT ( 'NONE',  ( 0.8923884514435701520, -0.5023911411419708095, -0.1820866141732282451 ) ) ;
#4268 = CARTESIAN_POINT ( 'NONE',  ( 1.614173228346457378, 1.330640075373405118, 0.1372047244094478369 ) ) ;
#4269 = CARTESIAN_POINT ( 'NONE',  ( -0.1070741851644051862, -0.3996062992125986590, -1.566272965879265344 ) ) ;
#4270 = CARTESIAN_POINT ( 'NONE',  ( 0.2690288713910767848, 0.2952755905511811885, 0.1292274648535926551 ) ) ;
#4271 = EDGE_CURVE ( 'NONE', #27584, #5989, #60717, .T. ) ;
#4272 = CARTESIAN_POINT ( 'NONE',  ( 0.1958661417322836440, -0.3392501089628017219, -1.658792650918635259 ) ) ;
#4273 = CARTESIAN_POINT ( 'NONE',  ( 1.397637795275591177, 0.07958543189024071263, -0.2665933059059888421 ) ) ;
#4274 = CARTESIAN_POINT ( 'NONE',  ( -2.795275590551183242, 1.574803149606300412, -1.327125379919507468E-16 ) ) ;
#4275 = CARTESIAN_POINT ( 'NONE',  ( -0.3740157480314953431, -0.4536011799217368745, -0.2665933059059886201 ) ) ;
#4276 = CARTESIAN_POINT ( 'NONE',  ( -0.05249343832020911260, 0.2306618581243848609, 0.2411417322834645549 ) ) ;
#4277 = CARTESIAN_POINT ( 'NONE',  ( 1.187664041994751285, -0.08942795157527998196, 0.3641732283464567121 ) ) ;
#4278 = CARTESIAN_POINT ( 'NONE',  ( -1.640419947506561060, -0.3690944881889765550, -0.3153832671262227771 ) ) ;
#4279 = CARTESIAN_POINT ( 'NONE',  ( -1.640419947506561060, -0.4281496062992127816, -0.4176697321401328100 ) ) ;
#4280 = CARTESIAN_POINT ( 'NONE',  ( 0.05249343832021075018, -0.6046776061558807314, 0.2411417322834647770 ) ) ;
#4281 = CARTESIAN_POINT ( 'NONE',  ( 1.292650918635171564, -0.6692913385826773087, -0.1292274648535924053 ) ) ;
#4282 = LINE ( 'NONE', #53548, #31642 ) ;
#4283 = CARTESIAN_POINT ( 'NONE',  ( 0.01968503937007930540, 0.1660481256975885056, 0.3530559997133364547 ) ) ;
#4284 = CARTESIAN_POINT ( 'NONE',  ( 1.410761154855643795, -0.05778040916215560624, -0.4822834645669293319 ) ) ;
#4285 = CARTESIAN_POINT ( 'NONE',  ( 0.8005249343832028242, -0.4281496062992127816, -0.4176697321401328100 ) ) ;
#4286 = CARTESIAN_POINT ( 'NONE',  ( -0.5314960629921171575, 2.742784562772121681, -2.516666329989062145 ) ) ;
#4287 = CARTESIAN_POINT ( 'NONE',  ( 0.5971128608923891301, 0.1771653543307087075, -0.09757992244046823083 ) ) ;
#4288 = CARTESIAN_POINT ( 'NONE',  ( 1.430446194225722500, -0.4281496062992127816, -0.4176697321401328100 ) ) ;
#4289 = CARTESIAN_POINT ( 'NONE',  ( 0.2230971128608929543, -0.004921259842519870586, -0.3153832671262229437 ) ) ;
#4290 = CARTESIAN_POINT ( 'NONE',  ( -0.2887139107611542133, -0.6046776061558809534, -0.2411417322834644161 ) ) ;
#4291 = CARTESIAN_POINT ( 'NONE',  ( 0.5446194225721792126, -0.05778040916215560624, -0.4822834645669293319 ) ) ;
#4292 = CARTESIAN_POINT ( 'NONE',  ( -0.5774278215223089816, -0.6046776061558807314, 0.2411417322834647770 ) ) ;
#4293 = CARTESIAN_POINT ( 'NONE',  ( -0.3392501089628017219, -0.1958661417322836995, -2.096476008695224991 ) ) ;
#4294 = CARTESIAN_POINT ( 'NONE',  ( -0.1509186351706028884, -0.08942795157527998196, 0.3641732283464567121 ) ) ;
#4295 = CARTESIAN_POINT ( 'NONE',  ( 0.6758530183727039509, 0.2952755905511810774, -0.1292274648535930714 ) ) ;
#4296 = CARTESIAN_POINT ( 'NONE',  ( 1.167979002624672580, -0.3690944881889763329, 0.3153832671262228327 ) ) ;
#4297 = CARTESIAN_POINT ( 'NONE',  ( 0.1246719160104994284, 0.2952755905511810774, -0.1292274648535930714 ) ) ;
#4298 = CARTESIAN_POINT ( 'NONE',  ( -1.701219675563209410, 1.179744462059445720, 0.3117399229855621900 ) ) ;
#4300 = LINE ( 'NONE', #55218, #80964 ) ;
#4299 = CARTESIAN_POINT ( 'NONE',  ( -0.5314960629921350321, 2.755905511811024056, 2.583694225513478937 ) ) ;
#4301 = DIRECTION ( 'NONE',  ( 1.000000000000000000, 8.805702923740138355E-17, 0.000000000000000000 ) ) ;
#4302 = CARTESIAN_POINT ( 'NONE',  ( -1.410761154855641575, -0.3162353388693409650, -0.4822834645669289433 ) ) ;
#4303 = CARTESIAN_POINT ( 'NONE',  ( -0.5380577427821514602, -0.4281496062992127816, -0.4176697321401328100 ) ) ;
#4304 = CARTESIAN_POINT ( 'NONE',  ( -1.157146581871515012E-16, 0.4724409448818898682, 0.000000000000000000 ) ) ;
#4305 = CARTESIAN_POINT ( 'NONE',  ( -0.3420746716998661618, 0.1974969037888702206, -2.703412073490814027 ) ) ;
#4306 = ORIENTED_EDGE ( 'NONE', *, *, #63106, .F. ) ;
#4307 = CARTESIAN_POINT ( 'NONE',  ( 0.3149606299212606708, -0.1870078740157480601, -0.3641732283464567677 ) ) ;
#4308 = CARTESIAN_POINT ( 'NONE',  ( 0.3917322834645669549, 0.1049643490035304660, -1.219160104986876325 ) ) ;
#4309 = CARTESIAN_POINT ( 'NONE',  ( 0.9383202099737536495, -0.3162353388693405765, 0.4822834645669290543 ) ) ;
#4310 = CARTESIAN_POINT ( 'NONE',  ( 0.2362204724409451007, -0.4091458600556402980, -2.611548556430446144 ) ) ;
#4311 = CARTESIAN_POINT ( 'NONE',  ( -0.4091458600556405756, 0.2362204724409446288, -0.8904199475065617264 ) ) ;
#4312 = CARTESIAN_POINT ( 'NONE',  ( -1.640419947506561060, -0.3690944881889765550, -0.3153832671262227771 ) ) ;
#4313 = CARTESIAN_POINT ( 'NONE',  ( 1.548556430446194954, 0.2306618581243847221, -0.2411417322834647770 ) ) ;
#4314 = CARTESIAN_POINT ( 'NONE',  ( 1.220472440944882386, -0.5511811023622047445, 6.969142054262312111E-17 ) ) ;
#4315 = CARTESIAN_POINT ( 'NONE',  ( 0.4986876640419954376, -0.6046776061558809534, -0.2411417322834644161 ) ) ;
#4316 = CARTESIAN_POINT ( 'NONE',  ( -0.1049643490035306742, 0.3917322834645668994, -0.2440751724071372475 ) ) ;
#4317 = CARTESIAN_POINT ( 'NONE',  ( -0.2559055118110227234, -0.5400638737290844871, 0.3530559997133364547 ) ) ;
#4318 = CARTESIAN_POINT ( 'NONE',  ( -0.9580052493438311334, -0.3690944881889763329, 0.3153832671262228327 ) ) ;
#4319 = CARTESIAN_POINT ( 'NONE',  ( 0.4068241469816279987, -0.4281496062992127816, -0.4176697321401328100 ) ) ;
#4320 = CARTESIAN_POINT ( 'NONE',  ( -0.05905511811023545637, -0.5400638737290845981, -0.3530559997133363437 ) ) ;
#4321 = CARTESIAN_POINT ( 'NONE',  ( -0.1265901696524993347, 0.4724409448818896462, -0.006561679790026246628 ) ) ;
#4322 = CARTESIAN_POINT ( 'NONE',  ( 0.1070741851644053527, 0.3996062992125986590, -2.828083989501312345 ) ) ;
#4323 = CARTESIAN_POINT ( 'NONE',  ( -0.3917322834645670659, -7.196005306013484475E-17, -1.768392019193912423 ) ) ;
#4324 = CARTESIAN_POINT ( 'NONE',  ( 0.6364829396325465405, -0.3162353388693409650, -0.4822834645669289433 ) ) ;
#4325 = CARTESIAN_POINT ( 'NONE',  ( -0.3937007874015740483, -0.1870078740157480879, -0.4822834645669291653 ) ) ;
#4326 = CARTESIAN_POINT ( 'NONE',  ( -1.614173228346455824, 0.2952755905511811885, 0.000000000000000000 ) ) ;
#4327 = CARTESIAN_POINT ( 'NONE',  ( 0.9383202099737536495, -0.3162353388693405765, 0.4822834645669290543 ) ) ;
#4328 = CARTESIAN_POINT ( 'NONE',  ( 0.5118110236220480003, -0.6692913385826771977, 8.415575281601705876E-17 ) ) ;
#4329 = CARTESIAN_POINT ( 'NONE',  ( -0.2867679344610365999, 0.2867679344610364889, -0.8917322834645667884 ) ) ;
#4330 = CARTESIAN_POINT ( 'NONE',  ( -0.5314960629921254842, -0.5400638737290845981, -0.3530559997133363437 ) ) ;
#4331 = CARTESIAN_POINT ( 'NONE',  ( 0.09186351706036827158, 0.05413385826771666132, 0.4176697321401328100 ) ) ;
#4332 = CARTESIAN_POINT ( 'NONE',  ( -0.4199475065616791736, -0.6046776061558807314, 0.2411417322834647770 ) ) ;
#4333 = CARTESIAN_POINT ( 'NONE',  ( 0.3937007874015754361, -0.1870078740157479769, 0.3641732283464567677 ) ) ;
#4334 = CARTESIAN_POINT ( 'NONE',  ( -1.587926509186350810, -0.4281496062992124485, 0.4176697321401328655 ) ) ;
#4335 = CARTESIAN_POINT ( 'NONE',  ( -1.313877454013331780, 0.2755905511811023723, 0.7983292792091805090 ) ) ;
#4336 = CARTESIAN_POINT ( 'NONE',  ( 0.4921259842519691285, 0.1660481256975885056, 0.3530559997133364547 ) ) ;
#4337 = CIRCLE ( 'NONE', #36587, 2.165354330708661568 ) ;
#4338 = CARTESIAN_POINT ( 'NONE',  ( 1.482939632545932307, 0.05413385826771626580, -0.4176697321401330321 ) ) ;
#4339 = CARTESIAN_POINT ( 'NONE',  ( 0.3917322834645669549, 0.1049643490035304660, -2.321522309711285814 ) ) ;
#4340 = ORIENTED_EDGE ( 'NONE', *, *, #63554, .F. ) ;
#4341 = ORIENTED_EDGE ( 'NONE', *, *, #41805, .F. ) ;
#4342 = CARTESIAN_POINT ( 'NONE',  ( 0.5708661417322842269, 0.1660481256975885056, 0.3530559997133364547 ) ) ;
#4343 = CARTESIAN_POINT ( 'NONE',  ( 0.3280839895013130669, -0.004921259842519576551, 0.3153832671262227771 ) ) ;
#4345 = DIRECTION ( 'NONE',  ( 0.000000000000000000, -1.000000000000000000, 1.408710688920637755E-15 ) ) ;
#4344 = CARTESIAN_POINT ( 'NONE',  ( -1.024573275495623381, 1.664102502641003678, 0.4574570760746348719 ) ) ;
#4346 = CARTESIAN_POINT ( 'NONE',  ( 0.2867679344610365999, -0.2867679344610365444, -0.6555118110236222151 ) ) ;
#4347 = DIRECTION ( 'NONE',  ( -3.096699300667737957E-16, 1.000000000000000000, -0.000000000000000000 ) ) ;
#4348 = CARTESIAN_POINT ( 'NONE',  ( 0.4498537592782897998, 0.000000000000000000, -2.118110236220472675 ) ) ;
#4349 = CARTESIAN_POINT ( 'NONE',  ( -0.3460692066303957537, -0.1998031496062994405, -2.491469816272966042 ) ) ;
#4350 = CARTESIAN_POINT ( 'NONE',  ( 0.6561679790026253567, 0.2306618581243848609, 0.2411417322834645549 ) ) ;
#4351 = CARTESIAN_POINT ( 'NONE',  ( -0.8858267716535425107, -0.5400638737290844871, 0.3530559997133364547 ) ) ;
#4352 = CARTESIAN_POINT ( 'NONE',  ( -0.8727034120734901146, -0.05778040916215560624, -0.4822834645669293319 ) ) ;
#4353 = CARTESIAN_POINT ( 'NONE',  ( 0.6036745406824153282, -0.6046776061558807314, 0.2411417322834647770 ) ) ;
#4354 = CARTESIAN_POINT ( 'NONE',  ( 1.174540682414699111, -0.05778040916215560624, -0.4822834645669293319 ) ) ;
#4355 = CARTESIAN_POINT ( 'NONE',  ( 1.246719160104987623, -0.004921259842519870586, -0.3153832671262229437 ) ) ;
#4356 = APPLICATION_PROTOCOL_DEFINITION ( 'draft international standard', 'automotive_design', 1998, #15402 ) ;
#4357 = CARTESIAN_POINT ( 'NONE',  ( 1.128608923884515169, -0.5023911411419708095, -0.1820866141732282451 ) ) ;
#4358 = CARTESIAN_POINT ( 'NONE',  ( -0.8858267716535425107, -0.5400638737290844871, 0.3530559997133364547 ) ) ;
#4359 = CARTESIAN_POINT ( 'NONE',  ( 0.2925321140481932369, -0.2925321140481931814, -0.3326771653543306728 ) ) ;
#4360 = CARTESIAN_POINT ( 'NONE',  ( 1.627296587926509996, -0.6046776061558807314, 0.2411417322834647770 ) ) ;
#4361 = DIRECTION ( 'NONE',  ( 0.000000000000000000, 0.000000000000000000, 1.000000000000000000 ) ) ;
#4362 = CARTESIAN_POINT ( 'NONE',  ( -0.3608923884514428360, 0.2952755905511811885, 0.1292274648535926551 ) ) ;
#4364 = CARTESIAN_POINT ( 'NONE',  ( -0.7345763322112005556, 1.945772888393059175, 0.5309055118110236338 ) ) ;
#4363 = CARTESIAN_POINT ( 'NONE',  ( 1.089238845144357759, 0.05413385826771626580, -0.4176697321401330321 ) ) ;
#4365 = CARTESIAN_POINT ( 'NONE',  ( -1.135170603674539924, -0.5511811023622046335, 0.09757992244046803654 ) ) ;
#4366 = CARTESIAN_POINT ( 'NONE',  ( 0.3871391076115493490, -0.3162353388693405765, 0.4822834645669290543 ) ) ;
#4367 = CARTESIAN_POINT ( 'NONE',  ( 0.7152230971128614723, -0.2845877964562161244, -0.3641732283464567121 ) ) ;
#4368 = CARTESIAN_POINT ( 'NONE',  ( -9.594673741351310580E-17, 0.3917322834645669549, -1.812316642223410046 ) ) ;
#4369 = CARTESIAN_POINT ( 'NONE',  ( -1.253280839895012377, -0.08942795157527998196, 0.3641732283464567121 ) ) ;
#4370 = CARTESIAN_POINT ( 'NONE',  ( 1.364829396325460076, 0.2306618581243848609, 0.2411417322834645549 ) ) ;
#4371 = ADVANCED_FACE ( 'NONE', ( #22007, #80105 ), #73783, .T. ) ;
#4372 = LINE ( 'NONE', #30040, #53186 ) ;
#4373 = CARTESIAN_POINT ( 'NONE',  ( -0.2427821522309703550, -0.08942795157528024563, -0.3641732283464568787 ) ) ;
#4374 = CARTESIAN_POINT ( 'NONE',  ( -0.2887139107611542133, 0.2306618581243848609, 0.2411417322834645549 ) ) ;
#4375 = CARTESIAN_POINT ( 'NONE',  ( -1.338582677165353729, -0.1870078740157479769, 0.3641732283464567677 ) ) ;
#4376 = CARTESIAN_POINT ( 'NONE',  ( -0.5118110236220466680, -0.6692913385826771977, 8.415575281601705876E-17 ) ) ;
#4377 = CARTESIAN_POINT ( 'NONE',  ( 1.384514435695538559, 0.2952755905511810774, -0.1292274648535930714 ) ) ;
#4378 = CARTESIAN_POINT ( 'NONE',  ( -0.3917322834645670659, -7.196005306013484475E-17, -0.5085494995088732928 ) ) ;
#4379 = CARTESIAN_POINT ( 'NONE',  ( -0.8661417322834640276, -0.1870078740157479769, 0.3641732283464567677 ) ) ;
#4380 = CARTESIAN_POINT ( 'NONE',  ( -0.4581164262379261443, 1.664773289199195538, -1.024290093949186131 ) ) ;
#4381 = CARTESIAN_POINT ( 'NONE',  ( 1.423884514435696191, -0.05778040916215522460, 0.4822834645669289988 ) ) ;
#4382 = CARTESIAN_POINT ( 'NONE',  ( -0.2362204724409447953, -0.4091458600556404646, -1.874671916010498762 ) ) ;
#4383 = CARTESIAN_POINT ( 'NONE',  ( -1.043307086614172707, 0.1660481256975883668, -0.3530559997133364547 ) ) ;
#4384 = CARTESIAN_POINT ( 'NONE',  ( -0.9251968503937002541, -0.4536011799217368745, -0.2665933059059886201 ) ) ;
#4385 = CARTESIAN_POINT ( 'NONE',  ( -0.4855643044619415427, -0.3690944881889763329, 0.3153832671262228327 ) ) ;
#4386 = EDGE_CURVE ( 'NONE', #15857, #38086, #25224, .T. ) ;
#4387 = CARTESIAN_POINT ( 'NONE',  ( -0.5118110236220466680, 0.2066929133858268208, 0.000000000000000000 ) ) ;
#4388 = CARTESIAN_POINT ( 'NONE',  ( 0.1509186351706045259, -0.05778040916215560624, -0.4822834645669293319 ) ) ;
#4389 = CARTESIAN_POINT ( 'NONE',  ( 0.1115485564304470323, 0.1771653543307087630, 0.09757992244046791164 ) ) ;
#4390 = CARTESIAN_POINT ( 'NONE',  ( -1.305774278215222184, -0.5511811023622048555, -0.09757992244046775898 ) ) ;
#4391 = CARTESIAN_POINT ( 'NONE',  ( -1.364829396325458521, 0.2306618581243847221, -0.2411417322834647770 ) ) ;
#4392 = CARTESIAN_POINT ( 'NONE',  ( 1.404199475065617264, -0.3690944881889763329, 0.3153832671262228327 ) ) ;
#4393 = CARTESIAN_POINT ( 'NONE',  ( 1.161417322834646493, -0.5400638737290844871, 0.3530559997133364547 ) ) ;
#4394 = CARTESIAN_POINT ( 'NONE',  ( 0.000000000000000000, 0.000000000000000000, 0.000000000000000000 ) ) ;
#4395 = CARTESIAN_POINT ( 'NONE',  ( 0.2952755905511819101, 0.07958543189024071263, -0.2665933059059888421 ) ) ;
#4396 = CARTESIAN_POINT ( 'NONE',  ( 0.8005249343832028242, -0.4281496062992127816, -0.4176697321401328100 ) ) ;
#4397 = EDGE_CURVE ( 'NONE', #61855, #58782, #63453, .T. ) ;
#4398 = CARTESIAN_POINT ( 'NONE',  ( 0.9973753280839902091, 0.1283753931104746893, -0.1820866141732285504 ) ) ;
#4399 = EDGE_LOOP ( 'NONE', ( #74766, #18773, #7781, #26371, #1245, #28539, #69012, #59812, #71586, #59665 ) ) ;
#4400 = CARTESIAN_POINT ( 'NONE',  ( -1.122047244094487306, 0.1660481256975883668, -0.3530559997133364547 ) ) ;
#4401 = CARTESIAN_POINT ( 'NONE',  ( -1.082677165354329896, -0.5400638737290845981, -0.3530559997133363437 ) ) ;
#4402 = CARTESIAN_POINT ( 'NONE',  ( -0.2230971128608915943, -0.4281496062992127816, -0.4176697321401328100 ) ) ;
#4403 = CARTESIAN_POINT ( 'NONE',  ( 0.3460692066303959757, -0.1998031496062991907, -0.1049868766404199599 ) ) ;
#4404 = CARTESIAN_POINT ( 'NONE',  ( 0.3996062992125985480, 2.446882876249141654E-17, -2.399606299212598604 ) ) ;
#4405 = CARTESIAN_POINT ( 'NONE',  ( 0.7086614173228352742, -0.1870078740157480879, -0.4822834645669291653 ) ) ;
#4406 = CARTESIAN_POINT ( 'NONE',  ( 1.437007874015748810, 0.07958543189024085140, 0.2665933059059887866 ) ) ;
#4407 = CARTESIAN_POINT ( 'NONE',  ( 0.1377952755905518800, 0.1660481256975883668, -0.3530559997133364547 ) ) ;
#4408 = CARTESIAN_POINT ( 'NONE',  ( 0.7939632545931766261, -0.05778040916215522460, 0.4822834645669289988 ) ) ;
#4409 = CARTESIAN_POINT ( 'NONE',  ( -0.2925321140481930704, -0.2925321140481933480, -1.791338582677165059 ) ) ;
#4410 = CARTESIAN_POINT ( 'NONE',  ( -0.3949938075777409963, -7.255918531996591613E-17, -1.299212598425196985 ) ) ;
#4411 = CARTESIAN_POINT ( 'NONE',  ( 0.2925321140481932369, 0.2925321140481932369, -2.657480314960630530 ) ) ;
#4412 = CARTESIAN_POINT ( 'NONE',  ( 0.4724409448818892576, 0.1265901696524997788, -0.5971128608923885750 ) ) ;
#4413 = CARTESIAN_POINT ( 'NONE',  ( 4.797336870675656522E-17, -0.3917322834645670104, -0.7007874015748030150 ) ) ;
#4414 = CARTESIAN_POINT ( 'NONE',  ( -0.3215223097112853146, -0.2845877964562159024, 0.3641732283464567677 ) ) ;
#4415 = CARTESIAN_POINT ( 'NONE',  ( -0.5577427821522301654, -0.05778040916215560624, -0.4822834645669293319 ) ) ;
#4416 = CARTESIAN_POINT ( 'NONE',  ( 0.4855643044619428750, 0.05413385826771666132, 0.4176697321401328100 ) ) ;
#4417 = CARTESIAN_POINT ( 'NONE',  ( -0.1974969037888706924, 0.3420746716998658843, -1.979658792650919041 ) ) ;
#4418 = EDGE_CURVE ( 'NONE', #39102, #22351, #4337, .T. ) ;
#4419 =( BOUNDED_CURVE ( )  B_SPLINE_CURVE ( 1, ( #14614, #1561 ),
 .UNSPECIFIED., .F., .F. ) 
 B_SPLINE_CURVE_WITH_KNOTS ( ( 2, 2 ),
 ( 3.469446951953614189E-18, 0.001999999999999998307 ),
 .UNSPECIFIED. ) 
 CURVE ( )  GEOMETRIC_REPRESENTATION_ITEM ( )  RATIONAL_B_SPLINE_CURVE ( ( 0.9875488213027523443, 0.9875488213027523443 ) ) 
 REPRESENTATION_ITEM ( '' )  );
#4420 = CARTESIAN_POINT ( 'NONE',  ( -1.423884514435694859, -0.05778040916215560624, -0.4822834645669293319 ) ) ;
#4421 = CARTESIAN_POINT ( 'NONE',  ( 1.095800524934383846, -0.3162353388693405765, 0.4822834645669290543 ) ) ;
#4422 = CARTESIAN_POINT ( 'NONE',  ( -0.4091458600556405756, 0.2362204724409446288, -2.545931758530183497 ) ) ;
#4423 = B_SPLINE_CURVE_WITH_KNOTS ( 'NONE', 3,
 ( #50920, #70293, #12645, #38307 ),
 .UNSPECIFIED., .F., .F.,
 ( 4, 4 ),
 ( 0.02954100249761015817, 0.02979193122353610695 ),
 .UNSPECIFIED. ) ;
#4424 = CARTESIAN_POINT ( 'NONE',  ( -0.3996062992125987146, 0.1070741851644051862, -1.765091863517059823 ) ) ;
#4425 = CARTESIAN_POINT ( 'NONE',  ( 0.6299212598425235621, 1.724409448818898127, -0.9285414500055687581 ) ) ;
#4426 = CARTESIAN_POINT ( 'NONE',  ( 1.030183727034121421, -0.3162353388693409650, -0.4822834645669289433 ) ) ;
#4427 = CARTESIAN_POINT ( 'NONE',  ( 0.5183727034120741983, 0.2952755905511810774, -0.1292274648535930714 ) ) ;
#4428 = EDGE_CURVE ( 'NONE', #59522, #59098, #41765, .T. ) ;
#4429 = CARTESIAN_POINT ( 'NONE',  ( 1.391076115485564868, -0.5023911411419708095, 0.1820866141732285504 ) ) ;
#4431 = CARTESIAN_POINT ( 'NONE',  ( -1.548556430446193399, -0.6046776061558809534, -0.2411417322834644161 ) ) ;
#4430 = CARTESIAN_POINT ( 'NONE',  ( -1.620734908136482577, 0.1771653543307087630, 0.09757992244046791164 ) ) ;
#4432 = CARTESIAN_POINT ( 'NONE',  ( -0.3392501089628019995, 0.1958661417322832277, 0.2040682414698161695 ) ) ;
#4433 = CARTESIAN_POINT ( 'NONE',  ( 0.7808398950131241190, -0.05778040916215560624, -0.4822834645669293319 ) ) ;
#4434 = AXIS2_PLACEMENT_3D ( 'NONE', #45455, #876, #27360 ) ;
#4435 = CARTESIAN_POINT ( 'NONE',  ( 1.515748031496063408, 0.07958543189024085140, 0.2665933059059887866 ) ) ;
#4436 = CARTESIAN_POINT ( 'NONE',  ( -0.7020997375328076329, -0.3162353388693409650, -0.4822834645669289433 ) ) ;
#4437 = CARTESIAN_POINT ( 'NONE',  ( -0.5971128608923877978, 0.2952755905511811885, 0.1292274648535926551 ) ) ;
#4438 = CARTESIAN_POINT ( 'NONE',  ( 1.404199475065617264, -0.4281496062992124485, 0.4176697321401328655 ) ) ;
#4439 = CARTESIAN_POINT ( 'NONE',  ( -0.3917322834645671215, 0.1049643490035301469, -0.1174540682414699083 ) ) ;
#4440 = CARTESIAN_POINT ( 'NONE',  ( 0.3018372703412079971, -0.4281496062992124485, 0.4176697321401328655 ) ) ;
#4441 = CARTESIAN_POINT ( 'NONE',  ( -0.3917322834645669549, -0.1049643490035306603, -2.400262467191600635 ) ) ;
#4442 = EDGE_CURVE ( 'NONE', #72462, #7970, #61715, .T. ) ;
#4443 = CARTESIAN_POINT ( 'NONE',  ( -1.502624671916009680, -0.2845877964562159024, 0.3641732283464567677 ) ) ;
#4444 = VERTEX_POINT ( 'NONE', #29554 ) ;
#4445 = CARTESIAN_POINT ( 'NONE',  ( -0.2891555358219908833, -0.2891555358219912164, -2.893700787401575436 ) ) ;
#4446 = VERTEX_POINT ( 'NONE', #80924 ) ;
#4447 = CARTESIAN_POINT ( 'NONE',  ( -1.614173228346457378, 1.606230626554505658, -0.1372047244094477536 ) ) ;
#4448 = CARTESIAN_POINT ( 'NONE',  ( 1.207349081364829990, -0.5023911411419708095, -0.1820866141732282451 ) ) ;
#4449 = CARTESIAN_POINT ( 'NONE',  ( 0.3460692066303959757, -0.1998031496062991907, -1.049868766404199460 ) ) ;
#4450 = CARTESIAN_POINT ( 'NONE',  ( 1.555118110236221041, 0.07958543189024071263, -0.2665933059059888421 ) ) ;
#4451 = CARTESIAN_POINT ( 'NONE',  ( -0.4724409448818896462, -0.1265901696524993070, -0.7526246719160104570 ) ) ;
#4452 = FACE_OUTER_BOUND ( 'NONE', #4211, .T. ) ;
#4453 = PLANE ( 'NONE',  #33840 ) ;
#4454 = CARTESIAN_POINT ( 'NONE',  ( 0.3917322834645670104, 2.398668435337828261E-17, -0.3602362204724410266 ) ) ;
#4455 = CARTESIAN_POINT ( 'NONE',  ( -0.3477690288713902178, 0.1771653543307087075, -0.09757992244046823083 ) ) ;
#4456 = CARTESIAN_POINT ( 'NONE',  ( -1.122047244094487306, -0.4536011799217367080, 0.2665933059059888421 ) ) ;
#4457 = CARTESIAN_POINT ( 'NONE',  ( -1.581364829396324945, -0.05778040916215560624, -0.4822834645669293319 ) ) ;
#4458 = CARTESIAN_POINT ( 'NONE',  ( 0.5577427821522314977, -0.3162353388693409650, -0.4822834645669289433 ) ) ;
#4459 = CARTESIAN_POINT ( 'NONE',  ( -1.194225721784776262, -0.4281496062992124485, 0.4176697321401328655 ) ) ;
#4460 = CARTESIAN_POINT ( 'NONE',  ( -0.3392501089628019995, 0.1958661417322832277, -0.1758530183727033402 ) ) ;
#4461 = VERTEX_POINT ( 'NONE', #42182 ) ;
#4462 = CARTESIAN_POINT ( 'NONE',  ( 1.548556430446194954, -0.6046776061558807314, 0.2411417322834647770 ) ) ;
#4463 = DIRECTION ( 'NONE',  ( 0.7071067811865489050, -0.000000000000000000, -0.7071067811865460184 ) ) ;
#4464 = CARTESIAN_POINT ( 'NONE',  ( -1.157146581871515012E-16, 0.4724409448818898682, -1.732283464566929165 ) ) ;
#4465 = DIRECTION ( 'NONE',  ( -0.000000000000000000, 1.000000000000000000, -0.000000000000000000 ) ) ;
#4466 = CARTESIAN_POINT ( 'NONE',  ( 0.4849061582275019378, 1.967896864084105024, 0.4921425059946345493 ) ) ;
#4467 = CARTESIAN_POINT ( 'NONE',  ( -0.5511811023622038563, -0.1870078740157479769, 0.4822834645669291653 ) ) ;
#4468 = CARTESIAN_POINT ( 'NONE',  ( 1.292650918635171564, -0.6692913385826773087, -0.1292274648535924053 ) ) ;
#4469 = CARTESIAN_POINT ( 'NONE',  ( 0.1181102362204724532, -0.09842519685039369248, 5.158493410915829266E-18 ) ) ;
#4470 = CARTESIAN_POINT ( 'NONE',  ( -0.8792650918635160906, 0.05413385826771626580, -0.4176697321401330321 ) ) ;
#4471 = CARTESIAN_POINT ( 'NONE',  ( 0.3392501089628018329, 0.1958661417322835052, -0.3687470884176359265 ) ) ;
#4472 = CARTESIAN_POINT ( 'NONE',  ( -0.1246719160104980823, 0.1771653543307087630, 0.09757992244046791164 ) ) ;
#4473 = CARTESIAN_POINT ( 'NONE',  ( -0.1049643490035307020, 0.3917322834645669549, -0.2486876640419948270 ) ) ;
#4474 = CARTESIAN_POINT ( 'NONE',  ( -0.2296587926509179312, -0.08942795157527998196, 0.3641732283464567121 ) ) ;
#4475 = CARTESIAN_POINT ( 'NONE',  ( 0.4986876640419954376, 0.1283753931104748280, 0.1820866141732283561 ) ) ;
#4476 = CARTESIAN_POINT ( 'NONE',  ( 0.6824146981627303710, 0.2306618581243847221, -0.2411417322834647770 ) ) ;
#4477 = CARTESIAN_POINT ( 'NONE',  ( -0.8858267716535425107, -0.4536011799217367080, 0.2665933059059888421 ) ) ;
#4478 = CARTESIAN_POINT ( 'NONE',  ( 0.2867679344610365999, -0.2867679344610365444, -2.295275590551181022 ) ) ;
#4479 = CARTESIAN_POINT ( 'NONE',  ( 1.423884514435696191, -0.05778040916215522460, 0.4822834645669289988 ) ) ;
#4480 = CARTESIAN_POINT ( 'NONE',  ( -0.9645669291338575535, 0.1660481256975883668, -0.3530559997133364547 ) ) ;
#4481 = CARTESIAN_POINT ( 'NONE',  ( -0.2362204724409447953, -0.4091458600556404646, -0.7723097112860892732 ) ) ;
#4482 = CARTESIAN_POINT ( 'NONE',  ( -0.1246719160104980823, 0.2952755905511811885, 0.1292274648535926551 ) ) ;
#4483 = B_SPLINE_CURVE_WITH_KNOTS ( 'NONE', 3,
 ( #44127, #70221, #12577, #38234, #63912, #6248, #51680, #38654 ),
 .UNSPECIFIED., .F., .F.,
 ( 4, 2, 2, 4 ),
 ( 0.05229140441945555329, 0.05473522118133025000, 0.05595712956226760182, 0.05717903794320495364 ),
 .UNSPECIFIED. ) ;
#4484 = EDGE_CURVE ( 'NONE', #65458, #3121, #22831, .T. ) ;
#4485 = CARTESIAN_POINT ( 'NONE',  ( -0.3543307086614165824, 0.2952755905511811885, 0.000000000000000000 ) ) ;
#4486 = CARTESIAN_POINT ( 'NONE',  ( 1.056430446194226658, 0.1771653543307087630, 0.09757992244046791164 ) ) ;
#4487 = CARTESIAN_POINT ( 'NONE',  ( 0.1312335958005255154, -0.5023911411419708095, 0.1820866141732285504 ) ) ;
#4488 = CARTESIAN_POINT ( 'NONE',  ( -0.4002624671916004129, -0.05778040916215560624, -0.4822834645669293319 ) ) ;
#4489 = CARTESIAN_POINT ( 'NONE',  ( -0.7742782152230962556, -0.4281496062992127816, -0.4176697321401328100 ) ) ;
#4490 = CARTESIAN_POINT ( 'NONE',  ( 3.184294706754630777, 2.755905511811024056, -0.5314960629921260393 ) ) ;
#4491 = CARTESIAN_POINT ( 'NONE',  ( 1.653543307086614789, -0.1870078740157479769, 0.3641732283464567677 ) ) ;
#4492 = AXIS2_PLACEMENT_3D ( 'NONE', #21782, #66834, #67655 ) ;
#4493 = CARTESIAN_POINT ( 'NONE',  ( 0.1902887139107617975, -0.6692913385826773087, -0.1292274648535924053 ) ) ;
#4494 = ORIENTED_EDGE ( 'NONE', *, *, #64155, .T. ) ;
#4495 = CARTESIAN_POINT ( 'NONE',  ( 0.1998031496062992463, 0.3460692066303959202, -1.795931758530183719 ) ) ;
#4496 = CARTESIAN_POINT ( 'NONE',  ( 1.286089238845145033, 0.2306618581243848609, 0.2411417322834645549 ) ) ;
#4497 = CARTESIAN_POINT ( 'NONE',  ( -0.6955380577427815458, -0.3690944881889765550, -0.3153832671262227771 ) ) ;
#4498 = CARTESIAN_POINT ( 'NONE',  ( -0.7545931758530177724, 0.2952755905511811885, 0.1292274648535926551 ) ) ;
#4499 = CARTESIAN_POINT ( 'NONE',  ( 1.325459317585302665, -0.4281496062992124485, 0.4176697321401328655 ) ) ;
#4500 = CARTESIAN_POINT ( 'NONE',  ( 1.076115485564305141, 0.2306618581243847221, -0.2411417322834647770 ) ) ;
#4501 = FACE_OUTER_BOUND ( 'NONE', #77542, .T. ) ;
#4502 = CARTESIAN_POINT ( 'NONE',  ( -1.194225721784776262, -0.004921259842519870586, -0.3153832671262229437 ) ) ;
#4503 = CARTESIAN_POINT ( 'NONE',  ( -9.787531504996566615E-17, 0.3996062992125985480, -0.2342519685039370358 ) ) ;
#4504 = CARTESIAN_POINT ( 'NONE',  ( -0.3460692066303960868, 0.1998031496062990242, -0.4986876640419947715 ) ) ;
#4505 = CARTESIAN_POINT ( 'NONE',  ( 0.3949938075777409963, 2.418639510665530435E-17, 0.03937007874015741732 ) ) ;
#4506 = CARTESIAN_POINT ( 'NONE',  ( 0.7677165354330716118, -0.4536011799217367080, 0.2665933059059888421 ) ) ;
#4507 = CARTESIAN_POINT ( 'NONE',  ( 0.6692913385826777528, 0.2952755905511811885, 0.000000000000000000 ) ) ;
#4508 = CARTESIAN_POINT ( 'NONE',  ( 1.561679790026247350, -0.4281496062992124485, 0.4176697321401328655 ) ) ;
#4509 = CARTESIAN_POINT ( 'NONE',  ( 0.1974969037888704704, 0.3420746716998660508, -1.008530183727033958 ) ) ;
#4510 = CARTESIAN_POINT ( 'NONE',  ( 0.6889763779527566800, -0.4536011799217367080, 0.2665933059059888421 ) ) ;
#4511 = CARTESIAN_POINT ( 'NONE',  ( -0.2690288713910754526, -0.6692913385826771977, 0.1292274648535927661 ) ) ;
#4512 = CARTESIAN_POINT ( 'NONE',  ( -0.6889763779527552368, 0.1660481256975885056, 0.3530559997133364547 ) ) ;
#4513 = CARTESIAN_POINT ( 'NONE',  ( 1.332020997375329197, -0.3162353388693405765, 0.4822834645669290543 ) ) ;
#4514 = CARTESIAN_POINT ( 'NONE',  ( -0.1265901696524986964, -0.4724409448818899238, -1.332020997375328086 ) ) ;
#4515 = CARTESIAN_POINT ( 'NONE',  ( -0.3996062992125985480, -0.1070741851644057135, -2.250656167979002475 ) ) ;
#4516 = CARTESIAN_POINT ( 'NONE',  ( -0.1049868766404193215, 0.1283753931104746893, -0.1820866141732285504 ) ) ;
#4517 = ORIENTED_EDGE ( 'NONE', *, *, #74844, .F. ) ;
#4518 = CARTESIAN_POINT ( 'NONE',  ( -0.3392501089628017219, -0.1958661417322836995, -0.9941138039708155016 ) ) ;
#4519 = ORIENTED_EDGE ( 'NONE', *, *, #38868, .F. ) ;
#4520 = CARTESIAN_POINT ( 'NONE',  ( -0.6627296587926503335, -0.6692913385826771977, 0.1292274648535927661 ) ) ;
#4521 = CARTESIAN_POINT ( 'NONE',  ( -0.1574803149606292529, -0.1870078740157480879, -0.4822834645669291653 ) ) ;
#4522 = CARTESIAN_POINT ( 'NONE',  ( -0.5249343832020990641, 0.2306618581243848609, 0.2411417322834645549 ) ) ;
#4523 = CARTESIAN_POINT ( 'NONE',  ( 0.5774278215223104249, 0.2306618581243848609, 0.2411417322834645549 ) ) ;
#4524 = CARTESIAN_POINT ( 'NONE',  ( -0.6233595800524928121, -0.3162353388693409650, -0.4822834645669289433 ) ) ;
#4525 = CARTESIAN_POINT ( 'NONE',  ( -1.430446194225720724, 0.05413385826771626580, -0.4176697321401330321 ) ) ;
#4526 = CARTESIAN_POINT ( 'NONE',  ( -0.7414698162729651543, 0.2952755905511810774, -0.1292274648535930714 ) ) ;
#4527 = CARTESIAN_POINT ( 'NONE',  ( 0.7545931758530188826, -0.6692913385826771977, 0.1292274648535927661 ) ) ;
#4528 = CARTESIAN_POINT ( 'NONE',  ( 0.4002624671916016896, -0.3162353388693409650, -0.4822834645669289433 ) ) ;
#4529 = CARTESIAN_POINT ( 'NONE',  ( 0.1958661417322834775, 0.3392501089628018884, -1.081364829396325389 ) ) ;
#4530 = CARTESIAN_POINT ( 'NONE',  ( -0.2952755905511803003, -0.4536011799217368745, -0.2665933059059886201 ) ) ;
#4531 = VERTEX_POINT ( 'NONE', #67048 ) ;
#4532 = CARTESIAN_POINT ( 'NONE',  ( 0.1974969037888706369, -0.3420746716998659953, -1.351706036745407014 ) ) ;
#4533 = ORIENTED_EDGE ( 'NONE', *, *, #25905, .F. ) ;
#4534 = CARTESIAN_POINT ( 'NONE',  ( -1.299212598425196097, -0.5511811023622047445, 6.969142054262312111E-17 ) ) ;
#4535 = CARTESIAN_POINT ( 'NONE',  ( -0.4330708661417315697, -0.6692913385826771977, 8.415575281601705876E-17 ) ) ;
#4536 = CARTESIAN_POINT ( 'NONE',  ( 2.795275590551181466, 2.362204724409448620, 0.000000000000000000 ) ) ;
#4537 = CARTESIAN_POINT ( 'NONE',  ( -0.7086614173228339419, -0.1870078740157480879, -0.4822834645669291653 ) ) ;
#4538 = CARTESIAN_POINT ( 'NONE',  ( -0.6364829396325453192, -0.3162353388693405765, 0.4822834645669290543 ) ) ;
#4539 = PLANE ( 'NONE',  #70052 ) ;
#4540 = CARTESIAN_POINT ( 'NONE',  ( -1.660104986876639543, -0.05778040916215560624, -0.4822834645669293319 ) ) ;
#4541 = CARTESIAN_POINT ( 'NONE',  ( 0.9776902887139113929, -0.5511811023622048555, -0.09757992244046775898 ) ) ;
#4542 = CARTESIAN_POINT ( 'NONE',  ( -0.1265901696524986964, -0.4724409448818899238, -1.017060367454068137 ) ) ;
#4543 = CARTESIAN_POINT ( 'NONE',  ( 0.3392501089628018884, -0.1958661417322834220, -0.03215223097112869521 ) ) ;
#4544 = CARTESIAN_POINT ( 'NONE',  ( -0.07874015748031421014, -0.1870078740157480601, -0.3641732283464567677 ) ) ;
#4545 = VECTOR ( 'NONE', #15434, 39.37007874015748143 ) ;
#4546 = CARTESIAN_POINT ( 'NONE',  ( -0.5511811023622038563, -0.1870078740157479769, 0.4822834645669291653 ) ) ;
#4547 = FACE_OUTER_BOUND ( 'NONE', #79584, .T. ) ;
#4548 = CARTESIAN_POINT ( 'NONE',  ( -0.2755905511811015396, -0.6692913385826771977, 8.415575281601705876E-17 ) ) ;
#4549 = VERTEX_POINT ( 'NONE', #61959 ) ;
#4550 = CARTESIAN_POINT ( 'NONE',  ( -0.2925321140481930704, -0.2925321140481933480, -2.106299212598425452 ) ) ;
#4551 = DIRECTION ( 'NONE',  ( 0.000000000000000000, 0.000000000000000000, 1.000000000000000000 ) ) ;
#4552 = ORIENTED_EDGE ( 'NONE', *, *, #29199, .T. ) ;
#4553 = CARTESIAN_POINT ( 'NONE',  ( -0.3996062992125984925, -0.1070741851644056858, -1.697506561679789971 ) ) ;
#4554 = CARTESIAN_POINT ( 'NONE',  ( 1.586052503253845281, 0.4724409448818907564, -0.1653254495020589354 ) ) ;
#4555 = CARTESIAN_POINT ( 'NONE',  ( -0.8464566929133852113, -0.4536011799217368745, -0.2665933059059886201 ) ) ;
#4556 = CARTESIAN_POINT ( 'NONE',  ( -0.7808398950131225646, -0.05778040916215522460, 0.4822834645669289988 ) ) ;
#4557 = CARTESIAN_POINT ( 'NONE',  ( -0.3458507752293906723, -0.3458507752293910609, -0.3740157480314960092 ) ) ;
#4558 = DIRECTION ( 'NONE',  ( -1.000000000000000000, 0.000000000000000000, 0.000000000000000000 ) ) ;
#4559 = CARTESIAN_POINT ( 'NONE',  ( 0.3917322834645670104, -0.1049643490035303411, -2.873359580052493811 ) ) ;
#4560 = CARTESIAN_POINT ( 'NONE',  ( 1.227034120734908917, 0.2952755905511810774, -0.1292274648535930714 ) ) ;
#4561 = CARTESIAN_POINT ( 'NONE',  ( 0.3346456692913390985, 0.1660481256975885056, 0.3530559997133364547 ) ) ;
#4562 = CARTESIAN_POINT ( 'NONE',  ( 0.6167979002624679463, 0.05413385826771626580, -0.4176697321401330321 ) ) ;
#4563 = CARTESIAN_POINT ( 'NONE',  ( -0.6561679790026240244, 0.1283753931104746893, -0.1820866141732285504 ) ) ;
#4564 = CARTESIAN_POINT ( 'NONE',  ( -0.1640419947506555343, -0.3162353388693405765, 0.4822834645669290543 ) ) ;
#4565 = CARTESIAN_POINT ( 'NONE',  ( 0.2362204724409451007, -0.4091458600556402980, -2.530839895013123453 ) ) ;
#4566 = CARTESIAN_POINT ( 'NONE',  ( -0.7217847769028863381, 0.05413385826771626580, -0.4176697321401330321 ) ) ;
#4567 = AXIS2_PLACEMENT_3D ( 'NONE', #22833, #22009, #68296 ) ;
#4568 = CARTESIAN_POINT ( 'NONE',  ( -0.3949938075777411073, 0.1058382717557497660, -2.314304461942256808 ) ) ;
#4569 = CARTESIAN_POINT ( 'NONE',  ( 1.181102362204724976, -0.1870078740157480601, -0.3641732283464567677 ) ) ;
#4570 = CARTESIAN_POINT ( 'NONE',  ( -0.4396325459317579898, 0.1771653543307087630, 0.09757992244046791164 ) ) ;
#4571 = CARTESIAN_POINT ( 'NONE',  ( 1.325459317585302665, -0.3690944881889763329, 0.3153832671262228327 ) ) ;
#4572 = CARTESIAN_POINT ( 'NONE',  ( -1.509186351706035767, 0.05413385826771626580, -0.4176697321401330321 ) ) ;
#4573 = CARTESIAN_POINT ( 'NONE',  ( -1.128608923884513837, 0.1283753931104746893, -0.1820866141732285504 ) ) ;
#4574 = CARTESIAN_POINT ( 'NONE',  ( 0.1471411879992355343, 1.702998256715020864E-15, -0.4281989832122452544 ) ) ;
#4575 = CARTESIAN_POINT ( 'NONE',  ( 0.3412073490813655186, -0.5023911411419708095, -0.1820866141732282451 ) ) ;
#4576 = CARTESIAN_POINT ( 'NONE',  ( -0.3083989501312330295, -0.3162353388693409650, -0.4822834645669289433 ) ) ;
#4577 = DIRECTION ( 'NONE',  ( 0.000000000000000000, 1.000000000000000000, 0.000000000000000000 ) ) ;
#4578 = CARTESIAN_POINT ( 'NONE',  ( 0.06561679790026316017, -0.3690944881889763329, 0.3153832671262228327 ) ) ;
#4579 = CARTESIAN_POINT ( 'NONE',  ( -1.706036745406823485, 0.1283753931104748280, 0.1820866141732283561 ) ) ;
#4580 = CARTESIAN_POINT ( 'NONE',  ( 0.9448818897637802916, -0.1870078740157480879, -0.4822834645669291653 ) ) ;
#4581 = FACE_OUTER_BOUND ( 'NONE', #14274, .T. ) ;
#4582 = CARTESIAN_POINT ( 'NONE',  ( 1.391076115485564868, -0.5023911411419708095, 0.1820866141732285504 ) ) ;
#4583 = CARTESIAN_POINT ( 'NONE',  ( -0.7480314960629914633, 0.2952755905511811885, 0.000000000000000000 ) ) ;
#4584 = CARTESIAN_POINT ( 'NONE',  ( -0.4855643044619415427, -0.004921259842519870586, -0.3153832671262229437 ) ) ;
#4585 = CARTESIAN_POINT ( 'NONE',  ( 4.893765752498283924E-17, -0.3996062992125986035, -2.755905511811023612 ) ) ;
#4586 = CARTESIAN_POINT ( 'NONE',  ( 0.03937007874015806264, 0.1771653543307087630, 0.000000000000000000 ) ) ;
#4587 = CARTESIAN_POINT ( 'NONE',  ( -0.2952755905511803003, -0.5400638737290845981, -0.3530559997133363437 ) ) ;
#4588 = CARTESIAN_POINT ( 'NONE',  ( -0.3996062992125986590, 0.1070741851644051723, -0.5820209973753280863 ) ) ;
#4589 = CARTESIAN_POINT ( 'NONE',  ( 0.3917322834645670104, 2.398668435337828261E-17, -2.092519685039370358 ) ) ;
#4590 = CARTESIAN_POINT ( 'NONE',  ( 0.7808398950131240079, -0.2845877964562159024, 0.3641732283464567677 ) ) ;
#4591 = CARTESIAN_POINT ( 'NONE',  ( -0.2165354330708654795, 0.1660481256975885056, 0.3530559997133364547 ) ) ;
#4592 = CARTESIAN_POINT ( 'NONE',  ( -0.5314960629921250401, 0.1660481256975885056, 0.3530559997133364547 ) ) ;
#4593 = CARTESIAN_POINT ( 'NONE',  ( -0.6496062992125976043, 0.07958543189024071263, -0.2665933059059888421 ) ) ;
#4594 = CARTESIAN_POINT ( 'NONE',  ( -3.908320185825792326, 1.537401574803149984, 0.4744094488188970171 ) ) ;
#4595 = CARTESIAN_POINT ( 'NONE',  ( -0.2559055118110227234, -0.4536011799217367080, 0.2665933059059888421 ) ) ;
#4596 = CARTESIAN_POINT ( 'NONE',  ( 0.006561679790026889343, -0.3162353388693409650, -0.4822834645669289433 ) ) ;
#4597 = CARTESIAN_POINT ( 'NONE',  ( -1.115485564304461219, -0.3690944881889763329, 0.3153832671262228327 ) ) ;
#4598 = CARTESIAN_POINT ( 'NONE',  ( -1.496062992125983815, -0.1870078740157479769, 0.4822834645669291653 ) ) ;
#4599 = CARTESIAN_POINT ( 'NONE',  ( 0.4624320255261049062, 8.471767977567108961E-16, -0.4445507791589058955 ) ) ;
#4600 = ORIENTED_EDGE ( 'NONE', *, *, #43269, .F. ) ;
#4601 = CIRCLE ( 'NONE', #44948, 3.937007874015748143 ) ;
#4602 = CARTESIAN_POINT ( 'NONE',  ( -1.640419947506561060, -0.3690944881889765550, -0.3153832671262227771 ) ) ;
#4603 = CARTESIAN_POINT ( 'NONE',  ( -0.4855643044619415427, -0.4281496062992124485, 0.4176697321401328655 ) ) ;
#4604 = CARTESIAN_POINT ( 'NONE',  ( -1.062992125984250968, -0.6692913385826771977, 8.415575281601705876E-17 ) ) ;
#4605 = CARTESIAN_POINT ( 'NONE',  ( -0.2867679344610365999, 0.2867679344610364889, -1.521653543307086354 ) ) ;
#4606 = FACE_OUTER_BOUND ( 'NONE', #8364, .T. ) ;
#4607 = CARTESIAN_POINT ( 'NONE',  ( 1.049868766404200349, 0.2306618581243848609, 0.2411417322834645549 ) ) ;
#4608 = CARTESIAN_POINT ( 'NONE',  ( 0.5905511811023629321, 0.2952755905511811885, 0.000000000000000000 ) ) ;
#4609 = DIRECTION ( 'NONE',  ( 0.000000000000000000, 0.000000000000000000, -1.000000000000000000 ) ) ;
#4610 = CARTESIAN_POINT ( 'NONE',  ( -0.1998031496062991630, -0.3460692066303959202, -2.504593175853018661 ) ) ;
#4611 = CARTESIAN_POINT ( 'NONE',  ( 1.233595800524935227, -0.5023911411419708095, 0.1820866141732285504 ) ) ;
#4612 = CARTESIAN_POINT ( 'NONE',  ( 0.1998031496062992740, 0.3460692066303959757, -0.7742782152230971437 ) ) ;
#4613 = ORIENTED_EDGE ( 'NONE', *, *, #4271, .F. ) ;
#4614 = CARTESIAN_POINT ( 'NONE',  ( -0.9251968503937002541, -0.4536011799217368745, -0.2665933059059886201 ) ) ;
#4616 = CARTESIAN_POINT ( 'NONE',  ( 4.797336870675656522E-17, -0.3917322834645670104, -2.433070866141732402 ) ) ;
#4615 = CIRCLE ( 'NONE', #54371, 1.181102362204724310 ) ;
#4617 = VERTEX_POINT ( 'NONE', #10214 ) ;
#4618 = CARTESIAN_POINT ( 'NONE',  ( 0.3608923884514443348, 0.2952755905511810774, -0.1292274648535930714 ) ) ;
#4619 = CARTESIAN_POINT ( 'NONE',  ( -0.3412073490813641308, -0.6046776061558807314, 0.2411417322834647770 ) ) ;
#4620 = CARTESIAN_POINT ( 'NONE',  ( -0.8989501312335946848, -0.6692913385826771977, 0.1292274648535927661 ) ) ;
#4621 = CARTESIAN_POINT ( 'NONE',  ( 0.9908136482939640111, -0.6692913385826771977, 0.1292274648535927661 ) ) ;
#4622 = CARTESIAN_POINT ( 'NONE',  ( -1.108923884514435132, -0.08942795157528024563, -0.3641732283464568787 ) ) ;
#4623 = DIRECTION ( 'NONE',  ( 1.000000000000000000, 0.000000000000000000, 0.000000000000000000 ) ) ;
#4624 = CARTESIAN_POINT ( 'NONE',  ( -0.006561679790025524116, -0.05778040916215560624, -0.4822834645669293319 ) ) ;
#4625 = CARTESIAN_POINT ( 'NONE',  ( -1.312335958005248715, 0.2306618581243848609, 0.2411417322834645549 ) ) ;
#4626 = CARTESIAN_POINT ( 'NONE',  ( -0.3917322834645668994, -0.1049643490035306742, -1.858248400753593987 ) ) ;
#4627 = CARTESIAN_POINT ( 'NONE',  ( -1.633858267716534529, 0.1660481256975885056, 0.3530559997133364547 ) ) ;
#4628 = CARTESIAN_POINT ( 'NONE',  ( 1.912049360642951330E-20, 1.062992125984252745, -2.874015748031495843 ) ) ;
#4629 = CARTESIAN_POINT ( 'NONE',  ( 0.3392501089628018329, 0.1958661417322835607, 0.03412073490813653104 ) ) ;
#4630 = CARTESIAN_POINT ( 'NONE',  ( 0.7808398950131241190, -0.08942795157528024563, -0.3641732283464568787 ) ) ;
#4631 = ORIENTED_EDGE ( 'NONE', *, *, #45026, .F. ) ;
#4632 = CARTESIAN_POINT ( 'NONE',  ( -0.3420746716998661618, 0.1974969037888702206, -0.1837270341207349611 ) ) ;
#4633 = CARTESIAN_POINT ( 'NONE',  ( -0.8530183727034112984, 0.05413385826771666132, 0.4176697321401328100 ) ) ;
#4634 = ORIENTED_EDGE ( 'NONE', *, *, #66088, .F. ) ;
#4635 = CARTESIAN_POINT ( 'NONE',  ( -0.2034120734908131112, -0.5511811023622048555, -0.09757992244046775898 ) ) ;
#4636 = CARTESIAN_POINT ( 'NONE',  ( -1.660104986876639543, -0.05778040916215560624, -0.4822834645669293319 ) ) ;
#4637 = CARTESIAN_POINT ( 'NONE',  ( 0.3871391076115492380, -0.05778040916215560624, -0.4822834645669293319 ) ) ;
#4638 = CARTESIAN_POINT ( 'NONE',  ( 0.5905511811023629321, -0.6692913385826771977, 8.415575281601705876E-17 ) ) ;
#4639 = CARTESIAN_POINT ( 'NONE',  ( -0.5249343832020990641, -0.6046776061558809534, -0.2411417322834644161 ) ) ;
#4640 = CARTESIAN_POINT ( 'NONE',  ( 4.797336870675656522E-17, -0.3917322834645670659, -1.177840838091550602 ) ) ;
#4641 = CARTESIAN_POINT ( 'NONE',  ( -0.8070866141732276899, 0.1660481256975883668, -0.3530559997133364547 ) ) ;
#4642 = CARTESIAN_POINT ( 'NONE',  ( 0.1049643490035304938, -0.3917322834645669549, -2.847112860892388131 ) ) ;
#4643 = CARTESIAN_POINT ( 'NONE',  ( 1.397637795275591177, -0.4536011799217367080, 0.2665933059059888421 ) ) ;
#4644 = CARTESIAN_POINT ( 'NONE',  ( -0.8595800524934373854, -0.05778040916215522460, 0.4822834645669289988 ) ) ;
#4645 = CARTESIAN_POINT ( 'NONE',  ( 0.8005249343832028242, -0.4281496062992127816, -0.4176697321401328100 ) ) ;
#4646 = CARTESIAN_POINT ( 'NONE',  ( 1.384514435695538559, 0.2952755905511810774, -0.1292274648535930714 ) ) ;
#4647 = CARTESIAN_POINT ( 'NONE',  ( 0.1998031496062992740, 0.3460692066303959757, -0.7742782152230971437 ) ) ;
#4648 = CARTESIAN_POINT ( 'NONE',  ( -1.489501312335957062, -0.3162353388693409650, -0.4822834645669289433 ) ) ;
#4649 = CARTESIAN_POINT ( 'NONE',  ( 0.3460692066303959202, -0.1998031496062991630, -0.1817585301837270351 ) ) ;
#4650 = CARTESIAN_POINT ( 'NONE',  ( 0.3083989501312343062, -0.3162353388693405765, 0.4822834645669290543 ) ) ;
#4651 = CARTESIAN_POINT ( 'NONE',  ( -0.1070741851644051862, -0.3996062992125987146, -2.119422572178477626 ) ) ;
#4652 = CARTESIAN_POINT ( 'NONE',  ( -1.509186351706035767, -0.3690944881889763329, 0.3153832671262228327 ) ) ;
#4653 = CARTESIAN_POINT ( 'NONE',  ( 0.4461942257217856311, 0.1283753931104746893, -0.1820866141732285504 ) ) ;
#4654 = CARTESIAN_POINT ( 'NONE',  ( 0.8398950131233602345, 0.2306618581243847221, -0.2411417322834647770 ) ) ;
#4655 = CARTESIAN_POINT ( 'NONE',  ( 0.4724409448818897572, -0.1265901696524988906, -1.133202099737532720 ) ) ;
#4656 = CARTESIAN_POINT ( 'NONE',  ( 0.8661417322834653598, -0.1870078740157479769, 0.3641732283464567677 ) ) ;
#4657 = CARTESIAN_POINT ( 'NONE',  ( 0.3018372703412079971, -0.4281496062992124485, 0.4176697321401328655 ) ) ;
#4658 = CARTESIAN_POINT ( 'NONE',  ( 0.1058382717557500852, -0.3949938075777408852, -0.7919947506561679784 ) ) ;
#4659 = CARTESIAN_POINT ( 'NONE',  ( -0.8727034120734901146, -0.05778040916215560624, -0.4822834645669293319 ) ) ;
#4660 = DIRECTION ( 'NONE',  ( 1.000000000000000000, -0.000000000000000000, -0.000000000000000000 ) ) ;
#4661 = AXIS2_PLACEMENT_3D ( 'NONE', #39756, #72582, #21233 ) ;
#4662 = CARTESIAN_POINT ( 'NONE',  ( 0.8858267716535438430, -0.4536011799217368745, -0.2665933059059886201 ) ) ;
#4663 = CARTESIAN_POINT ( 'NONE',  ( -0.1377952755905504645, 0.1660481256975885056, 0.3530559997133364547 ) ) ;
#4664 = LINE ( 'NONE', #50100, #18420 ) ;
#4665 = CARTESIAN_POINT ( 'NONE',  ( -0.2755905511811018171, 0.2952755905511811885, 0.000000000000000000 ) ) ;
#4666 = CARTESIAN_POINT ( 'NONE',  ( 0.08530183727034192087, -0.08942795157527998196, 0.3641732283464567121 ) ) ;
#4667 = CARTESIAN_POINT ( 'NONE',  ( -2.554262525012222174, 1.537401574803149984, 0.4744094488188970171 ) ) ;
#4668 = CARTESIAN_POINT ( 'NONE',  ( 0.1181102362204730916, 0.1771653543307087630, 0.000000000000000000 ) ) ;
#4669 = CARTESIAN_POINT ( 'NONE',  ( 0.7808398950131240079, -0.2845877964562159024, 0.3641732283464567677 ) ) ;
#4670 = DIRECTION ( 'NONE',  ( -1.224646799147349509E-16, 0.000000000000000000, -1.000000000000000000 ) ) ;
#4671 = CARTESIAN_POINT ( 'NONE',  ( 4.893765752498283308E-17, -0.3996062992125985480, -1.572834645669291431 ) ) ;
#4672 = CARTESIAN_POINT ( 'NONE',  ( 0.3740157480314966754, -0.5400638737290844871, 0.3530559997133364547 ) ) ;
#4673 = ADVANCED_FACE ( 'NONE', ( #68294 ), #15109, .F. ) ;
#4674 = CARTESIAN_POINT ( 'NONE',  ( 0.1049643490035303689, 0.3917322834645670104, -1.402887139107611647 ) ) ;
#4675 = CARTESIAN_POINT ( 'NONE',  ( 1.056430446194226658, 0.1771653543307087630, 0.09757992244046791164 ) ) ;
#4676 = CARTESIAN_POINT ( 'NONE',  ( 0.4330708661417321248, 1.968503937007873850, 0.000000000000000000 ) ) ;
#4677 = CARTESIAN_POINT ( 'NONE',  ( -0.4461942257217840213, 0.1283753931104748280, 0.1820866141732283561 ) ) ;
#4678 = VECTOR ( 'NONE', #82708, 39.37007874015748143 ) ;
#4679 = CARTESIAN_POINT ( 'NONE',  ( -0.2427821522309703550, -0.08942795157528024563, -0.3641732283464568787 ) ) ;
#4680 = CARTESIAN_POINT ( 'NONE',  ( -0.4068241469816264999, -0.4281496062992124485, 0.4176697321401328655 ) ) ;
#4681 = CARTESIAN_POINT ( 'NONE',  ( 0.8661417322834653598, -0.1870078740157479769, 0.3641732283464567677 ) ) ;
#4682 = CARTESIAN_POINT ( 'NONE',  ( -1.679790026246718693, 0.1283753931104746893, -0.1820866141732285504 ) ) ;
#4683 = CARTESIAN_POINT ( 'NONE',  ( 1.299212598425197429, 0.1771653543307087630, 0.000000000000000000 ) ) ;
#4684 = CARTESIAN_POINT ( 'NONE',  ( 0.07874015748031558404, -0.1870078740157479769, 0.4822834645669291653 ) ) ;
#4685 = CARTESIAN_POINT ( 'NONE',  ( 1.128608923884515169, -0.6046776061558809534, -0.2411417322834644161 ) ) ;
#4686 = CARTESIAN_POINT ( 'NONE',  ( 0.3635331417845804602, 1.231226750417219851, -2.000933467513867470 ) ) ;
#4687 = CARTESIAN_POINT ( 'NONE',  ( 5.463695987328526437E-16, -0.1870078740157479769, 0.4822834645669291653 ) ) ;
#4688 = CARTESIAN_POINT ( 'NONE',  ( 1.482939632545932307, -0.4281496062992124485, 0.4176697321401328655 ) ) ;
#4689 = CARTESIAN_POINT ( 'NONE',  ( 0.7414698162729663755, 0.2952755905511811885, 0.1292274648535926551 ) ) ;
#4690 = CARTESIAN_POINT ( 'NONE',  ( 0.4709442531824356015, 0.03757601356358734185, -1.929133858267717549 ) ) ;
#4691 = CARTESIAN_POINT ( 'NONE',  ( 0.9908136482939640111, -0.5511811023622046335, 0.09757992244046803654 ) ) ;
#4692 = CARTESIAN_POINT ( 'NONE',  ( 1.102362204724410155, -0.1870078740157480879, -0.4822834645669291653 ) ) ;
#4693 = CARTESIAN_POINT ( 'NONE',  ( -0.006561679790025524116, -0.2845877964562159024, 0.3641732283464567677 ) ) ;
#4694 = CARTESIAN_POINT ( 'NONE',  ( -0.3412073490813641308, 0.2306618581243847221, -0.2411417322834647770 ) ) ;
#4695 = CARTESIAN_POINT ( 'NONE',  ( 0.2559055118110243332, -0.5400638737290845981, -0.3530559997133363437 ) ) ;
#4696 = CARTESIAN_POINT ( 'NONE',  ( -0.7086614173228339419, -0.1870078740157479769, 0.4822834645669291653 ) ) ;
#4697 = EDGE_CURVE ( 'NONE', #75845, #16450, #47346, .T. ) ;
#4698 = CARTESIAN_POINT ( 'NONE',  ( -0.09186351706036689768, -0.004921259842519870586, -0.3153832671262229437 ) ) ;
#4699 = CARTESIAN_POINT ( 'NONE',  ( 0.8858267716535438430, -0.5400638737290845981, -0.3530559997133363437 ) ) ;
#4700 = CARTESIAN_POINT ( 'NONE',  ( 0.9514435695538062676, -0.2845877964562161244, -0.3641732283464567121 ) ) ;
#4701 = CARTESIAN_POINT ( 'NONE',  ( 0.1968503937007881344, -0.6692913385826771977, 8.415575281601705876E-17 ) ) ;
#4702 = CARTESIAN_POINT ( 'NONE',  ( -1.667080261987974543, 1.152314991887330997, 0.2771243236687696010 ) ) ;
#4704 = CARTESIAN_POINT ( 'NONE',  ( 0.1998031496062992740, 0.3460692066303959757, -1.089238845144356871 ) ) ;
#4703 = CARTESIAN_POINT ( 'NONE',  ( -1.062992125984250968, 0.2952755905511811885, 0.000000000000000000 ) ) ;
#4705 = DIRECTION ( 'NONE',  ( 1.049727191138618079E-16, -0.5150380749100549327, 0.8571673007021117785 ) ) ;
#4706 = CARTESIAN_POINT ( 'NONE',  ( 0.3917322834645669549, 0.1049643490035304660, -2.164041994750655729 ) ) ;
#4707 = CARTESIAN_POINT ( 'NONE',  ( -1.187664041994749731, -0.3162353388693405765, 0.4822834645669290543 ) ) ;
#4708 = CARTESIAN_POINT ( 'NONE',  ( -0.2952755905511804668, 0.1660481256975885056, 0.3530559997133364547 ) ) ;
#4709 = CARTESIAN_POINT ( 'NONE',  ( -0.2362204724409447953, -0.4091458600556404646, -0.5380577427821522374 ) ) ;
#4710 = CARTESIAN_POINT ( 'NONE',  ( -0.1058382717557497937, -0.3949938075777411628, -2.906824146981628054 ) ) ;
#4711 = EDGE_LOOP ( 'NONE', ( #70240, #18438, #36585, #7340 ) ) ;
#4712 = CARTESIAN_POINT ( 'NONE',  ( 0.1640419947506569498, -0.2845877964562161244, -0.3641732283464567121 ) ) ;
#4713 = CARTESIAN_POINT ( 'NONE',  ( 0.1049643490035303689, 0.3917322834645670104, -1.402887139107611647 ) ) ;
#4714 = CARTESIAN_POINT ( 'NONE',  ( 0.7283464566929140904, -0.5400638737290845981, -0.3530559997133363437 ) ) ;
#4715 = CARTESIAN_POINT ( 'NONE',  ( 0.4091458600556403535, 0.2362204724409449896, -2.650918635170603554 ) ) ;
#4716 = CARTESIAN_POINT ( 'NONE',  ( 0.9548908091195654757, -4.927456884911482678E-16, 0.4445507791589062840 ) ) ;
#4717 = CARTESIAN_POINT ( 'NONE',  ( -1.660104986876639543, -0.08942795157528024563, -0.3641732283464568787 ) ) ;
#4718 = CARTESIAN_POINT ( 'NONE',  ( 1.036745406824147731, 0.05413385826771666132, 0.4176697321401328100 ) ) ;
#4719 = CARTESIAN_POINT ( 'NONE',  ( 1.259842519685040019, -0.1870078740157479769, 0.3641732283464567677 ) ) ;
#4720 = CARTESIAN_POINT ( 'NONE',  ( 0.1443569553805781891, 0.05413385826771626580, -0.4176697321401330321 ) ) ;
#4721 = CARTESIAN_POINT ( 'NONE',  ( 0.3917322834645668994, -0.1049643490035303134, -0.6640226789688171705 ) ) ;
#4722 = CARTESIAN_POINT ( 'NONE',  ( -0.2296587926509179312, -0.05778040916215522460, 0.4822834645669289988 ) ) ;
#4723 = CARTESIAN_POINT ( 'NONE',  ( -0.9448818897637790704, -0.1870078740157479769, 0.3641732283464567677 ) ) ;
#4724 = ADVANCED_FACE ( 'NONE', ( #54394 ), #29146, .T. ) ;
#4725 = CARTESIAN_POINT ( 'NONE',  ( 0.5839895013123367340, -0.6692913385826773087, -0.1292274648535924053 ) ) ;
#4726 = CARTESIAN_POINT ( 'NONE',  ( -0.6692913385826764205, -0.6692913385826771977, 8.415575281601705876E-17 ) ) ;
#4727 = CARTESIAN_POINT ( 'NONE',  ( -1.586052503253848167, 1.023622047244095556, 0.1653254495020564929 ) ) ;
#4728 = LINE ( 'NONE', #37953, #11362 ) ;
#4729 = ORIENTED_EDGE ( 'NONE', *, *, #31019, .T. ) ;
#4730 = CARTESIAN_POINT ( 'NONE',  ( 0.2867679344610366554, -0.2867679344610365999, -1.984927452264778847 ) ) ;
#4731 = CARTESIAN_POINT ( 'NONE',  ( 0.4658792650918641698, -0.05778040916215560624, -0.4822834645669293319 ) ) ;
#4732 = VECTOR ( 'NONE', #8701, 39.37007874015748143 ) ;
#4733 = CARTESIAN_POINT ( 'NONE',  ( -0.4461942257217840213, 0.2306618581243848609, 0.2411417322834645549 ) ) ;
#4734 = CARTESIAN_POINT ( 'NONE',  ( -1.581364829396324945, -0.05778040916215560624, -0.4822834645669293319 ) ) ;
#4736 = CARTESIAN_POINT ( 'NONE',  ( 0.9120734908136489683, -0.6692913385826771977, 0.1292274648535927661 ) ) ;
#4735 = VECTOR ( 'NONE', #36418, 39.37007874015748143 ) ;
#4737 = CARTESIAN_POINT ( 'NONE',  ( 0.3018372703412079971, 0.05413385826771626580, -0.4176697321401330321 ) ) ;
#4738 = CARTESIAN_POINT ( 'NONE',  ( 0.1958661417322836440, -0.3392501089628017219, -1.436351706036745446 ) ) ;
#4739 = CARTESIAN_POINT ( 'NONE',  ( -0.8792650918635160906, 0.05413385826771626580, -0.4176697321401330321 ) ) ;
#4740 = CARTESIAN_POINT ( 'NONE',  ( 0.03937007874015833325, -0.6692913385826771977, 8.415575281601705876E-17 ) ) ;
#4741 = CARTESIAN_POINT ( 'NONE',  ( -0.5249343832020990641, 0.2306618581243848609, 0.2411417322834645549 ) ) ;
#4742 = CARTESIAN_POINT ( 'NONE',  ( 0.1246719160104994284, 0.1771653543307087075, -0.09757992244046823083 ) ) ;
#4743 = CARTESIAN_POINT ( 'NONE',  ( -1.601049868766403650, -0.6046776061558807314, 0.2411417322834647770 ) ) ;
#4744 = CARTESIAN_POINT ( 'NONE',  ( -0.2524666497344155158, -0.1533018367440332486, 5.791491733107224427 ) ) ;
#4745 = CARTESIAN_POINT ( 'NONE',  ( 0.3543307086614179147, 0.2952755905511811885, 0.000000000000000000 ) ) ;
#4746 = CARTESIAN_POINT ( 'NONE',  ( 3.911381074053594809, 1.694895442417441167, -0.4486550326265806854 ) ) ;
#4747 = CARTESIAN_POINT ( 'NONE',  ( -1.594488188976377119, 0.1660481256975883668, -0.3530559997133364547 ) ) ;
#4748 = CARTESIAN_POINT ( 'NONE',  ( -0.1049643490035307020, 0.3917322834645669549, -2.675853018372703396 ) ) ;
#4749 = VERTEX_POINT ( 'NONE', #38345 ) ;
#4750 = EDGE_LOOP ( 'NONE', ( #33633, #26354, #54234, #43979 ) ) ;
#4751 = CARTESIAN_POINT ( 'NONE',  ( 0.8333333333333340365, -0.6692913385826771977, 0.1292274648535927661 ) ) ;
#4752 = CARTESIAN_POINT ( 'NONE',  ( 0.3083989501312343062, -0.2845877964562159024, 0.3641732283464567677 ) ) ;
#4754 = DIRECTION ( 'NONE',  ( 0.000000000000000000, -1.000000000000000000, -0.000000000000000000 ) ) ;
#4753 = CARTESIAN_POINT ( 'NONE',  ( -1.031215834252966479, 1.709707895510313325, 0.4423016570855548002 ) ) ;
#4755 = CARTESIAN_POINT ( 'NONE',  ( -0.2867679344610364334, -0.2867679344610367109, -0.6161417322834646937 ) ) ;
#4756 = CARTESIAN_POINT ( 'NONE',  ( -0.3458507752293906723, -0.3458507752293910609, 0.1791338582677165503 ) ) ;
#4757 = CARTESIAN_POINT ( 'NONE',  ( 3.937007874015748143, 1.724409448818897905, 0.4359958488159722534 ) ) ;
#4758 = CARTESIAN_POINT ( 'NONE',  ( 0.3996062992125985480, 2.446882876249141654E-17, -2.557086614173228689 ) ) ;
#4759 = CARTESIAN_POINT ( 'NONE',  ( 0.5577427821522314977, -0.3162353388693409650, -0.4822834645669289433 ) ) ;
#4760 = CARTESIAN_POINT ( 'NONE',  ( -1.358267716535432434, -0.5400638737290844871, 0.3530559997133364547 ) ) ;
#4761 = CARTESIAN_POINT ( 'NONE',  ( -1.279527559055116948, -0.5400638737290844871, 0.3530559997133364547 ) ) ;
#4762 = CARTESIAN_POINT ( 'NONE',  ( 0.8792650918635177559, -0.4281496062992127816, -0.4176697321401328100 ) ) ;
#4763 = CARTESIAN_POINT ( 'NONE',  ( 1.279527559055118724, 0.1660481256975885056, 0.3530559997133364547 ) ) ;
#4764 = CARTESIAN_POINT ( 'NONE',  ( 1.489501312335958172, -0.2845877964562159024, 0.3641732283464567677 ) ) ;
#4765 = ITEM_DEFINED_TRANSFORMATION ( 'NONE', 'NONE', #71911,  #22098 ) ;
#4766 = CARTESIAN_POINT ( 'NONE',  ( 1.076115485564305141, 0.1283753931104746893, -0.1820866141732285504 ) ) ;
#4767 = CARTESIAN_POINT ( 'NONE',  ( -0.7152230971128602510, -0.3162353388693405765, 0.4822834645669290543 ) ) ;
#4768 = CARTESIAN_POINT ( 'NONE',  ( 0.3996062992125984925, 0.1070741851644054637, -0.3589238845144357426 ) ) ;
#4769 = CARTESIAN_POINT ( 'NONE',  ( 1.404199475065617708, 0.05413385826771626580, -0.4176697321401330321 ) ) ;
#4770 = CARTESIAN_POINT ( 'NONE',  ( -0.2867679344610365999, 0.2867679344610364889, -0.3267716535433070613 ) ) ;
#4771 = CARTESIAN_POINT ( 'NONE',  ( -0.4330708661417315697, -0.6692913385826771977, 8.415575281601705876E-17 ) ) ;
#4773 = FACE_OUTER_BOUND ( 'NONE', #39205, .T. ) ;
#4772 = CARTESIAN_POINT ( 'NONE',  ( 1.299212598425197429, -0.6692913385826771977, 8.415575281601705876E-17 ) ) ;
#4774 = CARTESIAN_POINT ( 'NONE',  ( -1.023622047244094002, -0.1870078740157480601, -0.3641732283464567677 ) ) ;
#4775 = CARTESIAN_POINT ( 'NONE',  ( 0.5183727034120741983, -0.6692913385826771977, 0.1292274648535927661 ) ) ;
#4776 = CARTESIAN_POINT ( 'NONE',  ( 0.8858267716535438430, -0.4536011799217368745, -0.2665933059059886201 ) ) ;
#4777 = CARTESIAN_POINT ( 'NONE',  ( 0.3917322834645668994, 0.1049643490035304522, -1.464547613352018773 ) ) ;
#4778 = CARTESIAN_POINT ( 'NONE',  ( -1.240157480314959759, 0.07958543189024085140, 0.2665933059059887866 ) ) ;
#4779 = CARTESIAN_POINT ( 'NONE',  ( 1.049868766404200349, 0.2306618581243848609, 0.2411417322834645549 ) ) ;
#4780 = DIRECTION ( 'NONE',  ( -0.000000000000000000, -1.000000000000000000, -0.000000000000000000 ) ) ;
#4781 = CARTESIAN_POINT ( 'NONE',  ( -0.5118110236220466680, -0.5511811023622047445, 6.969142054262312111E-17 ) ) ;
#4782 = CARTESIAN_POINT ( 'NONE',  ( -0.2427821522309703550, -0.05778040916215560624, -0.4822834645669293319 ) ) ;
#4783 = CARTESIAN_POINT ( 'NONE',  ( -1.292650918635170010, 0.1771653543307087075, -0.09757992244046823083 ) ) ;
#4784 = CARTESIAN_POINT ( 'NONE',  ( -0.8792650918635160906, 0.05413385826771626580, -0.4176697321401330321 ) ) ;
#4785 = CARTESIAN_POINT ( 'NONE',  ( 1.476377952755906442, -0.5400638737290844871, 0.3530559997133364547 ) ) ;
#4786 = CARTESIAN_POINT ( 'NONE',  ( 0.3917322834645670659, 2.398668435337828261E-17, -0.7447699719498183102 ) ) ;
#4787 = CARTESIAN_POINT ( 'NONE',  ( -0.9908136482939626788, 0.1771653543307087630, 0.09757992244046791164 ) ) ;
#4788 = CARTESIAN_POINT ( 'NONE',  ( 2.630268417803937719, 1.724409448818898127, 0.4359958488159723644 ) ) ;
#4789 = CARTESIAN_POINT ( 'NONE',  ( 1.292650918635171564, 0.2952755905511811885, 0.1292274648535926551 ) ) ;
#4790 = CARTESIAN_POINT ( 'NONE',  ( 0.2362204724409451007, -0.4091458600556402980, -2.058398950131233640 ) ) ;
#4791 = CARTESIAN_POINT ( 'NONE',  ( -1.377952755905511140, 0.2952755905511811885, 0.000000000000000000 ) ) ;
#4792 = CARTESIAN_POINT ( 'NONE',  ( -1.443569553805773564, 0.1283753931104746893, -0.1820866141732285504 ) ) ;
#4793 = CARTESIAN_POINT ( 'NONE',  ( -0.8005249343832013809, -0.3690944881889763329, 0.3153832671262228327 ) ) ;
#4794 = CARTESIAN_POINT ( 'NONE',  ( -1.601049868766403650, 0.2306618581243847221, -0.2411417322834647770 ) ) ;
#4795 = CARTESIAN_POINT ( 'NONE',  ( -0.1837270341207340729, 0.2306618581243847221, -0.2411417322834647770 ) ) ;
#4796 = CARTESIAN_POINT ( 'NONE',  ( 0.1640419947506569498, -0.2845877964562161244, -0.3641732283464567121 ) ) ;
#4797 = CARTESIAN_POINT ( 'NONE',  ( -1.089238845144356427, -0.004921259842519576551, 0.3153832671262227771 ) ) ;
#4798 = CARTESIAN_POINT ( 'NONE',  ( -1.627296587926508442, -0.6046776061558809534, -0.2411417322834644161 ) ) ;
#4799 = CARTESIAN_POINT ( 'NONE',  ( 1.371391076115485719, -0.5511811023622048555, -0.09757992244046775898 ) ) ;
#4800 = CARTESIAN_POINT ( 'NONE',  ( 1.148293963254593875, -0.6692913385826771977, 0.1292274648535927661 ) ) ;
#4801 = CARTESIAN_POINT ( 'NONE',  ( 0.1179898944395467303, 1.077592634160696505, 1.863899027365439443 ) ) ;
#4802 = CARTESIAN_POINT ( 'NONE',  ( 0.3871391076115493490, -0.2845877964562159024, 0.3641732283464567677 ) ) ;
#4803 = CARTESIAN_POINT ( 'NONE',  ( 0.5118110236220480003, -0.6692913385826771977, 8.415575281601705876E-17 ) ) ;
#4804 = ADVANCED_FACE ( 'NONE', ( #77070 ), #316, .F. ) ;
#4805 = CARTESIAN_POINT ( 'NONE',  ( 0.9448818897637802916, -0.1870078740157479769, 0.3641732283464567677 ) ) ;
#4806 = VERTEX_POINT ( 'NONE', #44633 ) ;
#4807 = CARTESIAN_POINT ( 'NONE',  ( -1.279527559055116948, 0.1660481256975883668, -0.3530559997133364547 ) ) ;
#4808 = EDGE_CURVE ( 'NONE', #31839, #73164, #12686, .T. ) ;
#4809 = CARTESIAN_POINT ( 'NONE',  ( -0.7939632545931750718, -0.05778040916215560624, -0.4822834645669293319 ) ) ;
#4810 = CARTESIAN_POINT ( 'NONE',  ( -0.2755905511811018171, 0.2952755905511811885, 0.000000000000000000 ) ) ;
#4811 = CARTESIAN_POINT ( 'NONE',  ( 0.1070741851644054915, -0.3996062992125985480, -0.08530183727034119923 ) ) ;
#4812 = CARTESIAN_POINT ( 'NONE',  ( 0.3996062992125985480, 2.446882876249141654E-17, -2.557086614173228689 ) ) ;
#4813 = CARTESIAN_POINT ( 'NONE',  ( 0.3215223097112867578, -0.05778040916215522460, 0.4822834645669289988 ) ) ;
#4814 = CARTESIAN_POINT ( 'NONE',  ( 1.607611548556431069, 0.1771653543307087630, 0.09757992244046791164 ) ) ;
#4815 = CARTESIAN_POINT ( 'NONE',  ( 0.2230971128608932319, -0.4281496062992124485, 0.4176697321401328655 ) ) ;
#4816 = CARTESIAN_POINT ( 'NONE',  ( 0.9645669291338588858, 0.1660481256975885056, 0.3530559997133364547 ) ) ;
#4817 = CARTESIAN_POINT ( 'NONE',  ( -0.3460692066303960868, 0.1998031496062990242, -2.388451443569553856 ) ) ;
#4818 = CARTESIAN_POINT ( 'NONE',  ( -0.3949938075777411628, 0.1058382717557497937, -1.450131233595800762 ) ) ;
#4819 = CARTESIAN_POINT ( 'NONE',  ( 0.1070741851644054915, -0.3996062992125986035, -2.919947506561679784 ) ) ;
#4820 = CARTESIAN_POINT ( 'NONE',  ( -0.5314960629921196000, 2.729664732663033888, -1.840814918237481113 ) ) ;
#4821 = CARTESIAN_POINT ( 'NONE',  ( -0.3392501089628017219, -0.1958661417322836718, -0.5170603674540682482 ) ) ;
#4822 = CARTESIAN_POINT ( 'NONE',  ( -0.5380577427821514602, -0.3690944881889765550, -0.3153832671262227771 ) ) ;
#4823 = CARTESIAN_POINT ( 'NONE',  ( -0.8464566929133852113, -0.5400638737290845981, -0.3530559997133363437 ) ) ;
#4824 = CARTESIAN_POINT ( 'NONE',  ( 0.2952755905511816326, -0.5400638737290844871, 0.3530559997133364547 ) ) ;
#4825 = CARTESIAN_POINT ( 'NONE',  ( 0.1058382717557500852, -0.3949938075777408852, -2.524278215223097366 ) ) ;
#4826 = CARTESIAN_POINT ( 'NONE',  ( 0.9317585301837276734, 0.05413385826771626580, -0.4176697321401330321 ) ) ;
#4827 = ADVANCED_FACE ( 'NONE', ( #44227 ), #70330, .T. ) ;
#4828 = CARTESIAN_POINT ( 'NONE',  ( 1.496062992125984703, -0.1870078740157480879, -0.4822834645669291653 ) ) ;
#4829 = CARTESIAN_POINT ( 'NONE',  ( 1.167979002624672580, 0.05413385826771626580, -0.4176697321401330321 ) ) ;
#4830 = CARTESIAN_POINT ( 'NONE',  ( -0.3458507752293909498, 0.3458507752293907833, -2.539370078740157410 ) ) ;
#4831 = CARTESIAN_POINT ( 'NONE',  ( 0.3996062992125986035, 0.1070741851644054776, -2.171916010498687211 ) ) ;
#4832 = DIRECTION ( 'NONE',  ( 1.000000000000000000, -0.000000000000000000, -0.000000000000000000 ) ) ;
#4833 = VECTOR ( 'NONE', #62107, 39.37007874015748143 ) ;
#4834 = AXIS2_PLACEMENT_3D ( 'NONE', #13381, #39034, #29524 ) ;
#4835 = ADVANCED_FACE ( 'NONE', ( #64019 ), #6360, .F. ) ;
#4836 = CARTESIAN_POINT ( 'NONE',  ( 0.8595800524934390507, -0.05778040916215560624, -0.4822834645669293319 ) ) ;
#4837 = CARTESIAN_POINT ( 'NONE',  ( 0.7020997375328090762, -0.05778040916215560624, -0.4822834645669293319 ) ) ;
#4838 = CARTESIAN_POINT ( 'NONE',  ( 1.194225721784777594, -0.3690944881889765550, -0.3153832671262227771 ) ) ;
#4840 = CARTESIAN_POINT ( 'NONE',  ( 1.581364829396326277, -0.05778040916215522460, 0.4822834645669289988 ) ) ;
#4839 = CARTESIAN_POINT ( 'NONE',  ( 1.653543307086614789, -0.1870078740157479769, 0.4822834645669291653 ) ) ;
#4841 = CARTESIAN_POINT ( 'NONE',  ( -0.2867679344610366554, 0.2867679344610365444, -2.619403256396638735 ) ) ;
#4842 = DIRECTION ( 'NONE',  ( -0.000000000000000000, 1.000000000000000000, -0.000000000000000000 ) ) ;
#4843 = CARTESIAN_POINT ( 'NONE',  ( 0.6824146981627303710, -0.6046776061558807314, 0.2411417322834647770 ) ) ;
#4844 = CARTESIAN_POINT ( 'NONE',  ( 1.450131233595801428, -0.5511811023622048555, -0.09757992244046775898 ) ) ;
#4845 = CARTESIAN_POINT ( 'NONE',  ( -0.3215223097112853146, -0.3162353388693405765, 0.4822834645669290543 ) ) ;
#4846 = CARTESIAN_POINT ( 'NONE',  ( -0.4527559055118102749, 0.1660481256975885056, 0.3530559997133364547 ) ) ;
#4847 = CARTESIAN_POINT ( 'NONE',  ( -1.627296587926508442, 0.2306618581243848609, 0.2411417322834645549 ) ) ;
#4848 = CARTESIAN_POINT ( 'NONE',  ( 4.797336870675656522E-17, -0.3917322834645670104, -0.3208661417322835607 ) ) ;
#4849 = CARTESIAN_POINT ( 'NONE',  ( -0.1049643490035307020, 0.3917322834645669549, -1.573490813648293907 ) ) ;
#4850 = CARTESIAN_POINT ( 'NONE',  ( -0.3392501089628019995, 0.1958661417322832277, -2.223097112860892288 ) ) ;
#4851 = CARTESIAN_POINT ( 'NONE',  ( 1.574803149606299746, -0.1870078740157480879, -0.4822834645669291653 ) ) ;
#4852 = ORIENTED_EDGE ( 'NONE', *, *, #13917, .T. ) ;
#4853 = CARTESIAN_POINT ( 'NONE',  ( 0.1974969037888704704, 0.3420746716998660508, -2.821522309711286258 ) ) ;
#4854 = ORIENTED_EDGE ( 'NONE', *, *, #63459, .F. ) ;
#4855 = CARTESIAN_POINT ( 'NONE',  ( 0.000000000000000000, 0.04488074079120789317, 0.000000000000000000 ) ) ;
#4856 = AXIS2_PLACEMENT_3D ( 'NONE', #56095, #4345, #75067 ) ;
#4857 = CARTESIAN_POINT ( 'NONE',  ( 1.548556430446194954, -0.5023911411419708095, 0.1820866141732285504 ) ) ;
#4858 = CARTESIAN_POINT ( 'NONE',  ( 0.1998031496062994405, -0.3460692066303958092, -1.351706036745406792 ) ) ;
#4859 = LINE ( 'NONE', #68024, #26333 ) ;
#4860 = CARTESIAN_POINT ( 'NONE',  ( 1.141392835773559211, 0.3937007874015748254, 1.318558190104271333 ) ) ;
#4861 = CARTESIAN_POINT ( 'NONE',  ( -0.4724409448818898682, -8.678599364036362592E-17, -0.9035433070866141225 ) ) ;
#4862 = CARTESIAN_POINT ( 'NONE',  ( 0.4556364816766638737, 1.768811104025900249, 0.5309055118110234117 ) ) ;
#4863 = CARTESIAN_POINT ( 'NONE',  ( -0.2867679344610365999, 0.2867679344610364889, -0.4192913385826772532 ) ) ;
#4864 = CARTESIAN_POINT ( 'NONE',  ( -0.5446194225721777693, -0.08942795157527998196, 0.3641732283464567121 ) ) ;
#4865 = CARTESIAN_POINT ( 'NONE',  ( -1.318897637795274802, -0.4536011799217368745, -0.2665933059059886201 ) ) ;
#4866 = EDGE_CURVE ( 'NONE', #23166, #80344, #43250, .T. ) ;
#4867 = CARTESIAN_POINT ( 'NONE',  ( 0.6036745406824153282, -0.6046776061558807314, 0.2411417322834647770 ) ) ;
#4868 = CARTESIAN_POINT ( 'NONE',  ( -1.161417322834644716, 0.1660481256975885056, 0.3530559997133364547 ) ) ;
#4869 = CARTESIAN_POINT ( 'NONE',  ( 0.1049643490035303689, 0.3917322834645670104, -0.1430446194225721002 ) ) ;
#4870 = ORIENTED_EDGE ( 'NONE', *, *, #2252, .F. ) ;
#4871 = CARTESIAN_POINT ( 'NONE',  ( 1.351706036745407458, -0.4281496062992127816, -0.4176697321401328100 ) ) ;
#4872 = CARTESIAN_POINT ( 'NONE',  ( 0.3499960723095487114, -0.3045081538226084295, -0.01928741089222630808 ) ) ;
#4873 = LENGTH_MEASURE_WITH_UNIT ( LENGTH_MEASURE( 0.02539999999999999897 ), #76000 );
#4874 = CARTESIAN_POINT ( 'NONE',  ( -0.1265901696524986964, -0.4724409448818899238, -1.489501312335957950 ) ) ;
#4875 = FACE_OUTER_BOUND ( 'NONE', #5056, .T. ) ;
#4876 = CARTESIAN_POINT ( 'NONE',  ( -0.5708661417322825615, -0.4536011799217367080, 0.2665933059059888421 ) ) ;
#4877 = CARTESIAN_POINT ( 'NONE',  ( -0.4724409448818899238, 0.1265901696524986964, -0.9776902887139107268 ) ) ;
#4878 = CARTESIAN_POINT ( 'NONE',  ( -0.9645669291338575535, 0.1660481256975883668, -0.3530559997133364547 ) ) ;
#4879 = CARTESIAN_POINT ( 'NONE',  ( 1.148293963254593875, -0.6692913385826771977, 0.1292274648535927661 ) ) ;
#4880 = VERTEX_POINT ( 'NONE', #69917 ) ;
#4882 = CARTESIAN_POINT ( 'NONE',  ( 0.6758530183727039509, 0.2066929133858267098, -0.1054918080437494132 ) ) ;
#4881 = CARTESIAN_POINT ( 'NONE',  ( 0.7545931758530189937, 0.2952755905511810219, -0.1292274648535930437 ) ) ;
#4883 = CARTESIAN_POINT ( 'NONE',  ( 1.666666666666667185, 0.05413385826771666132, 0.4176697321401328100 ) ) ;
#4884 = CARTESIAN_POINT ( 'NONE',  ( -1.030183727034119867, -0.05778040916215560624, -0.4822834645669293319 ) ) ;
#4885 = CARTESIAN_POINT ( 'NONE',  ( -0.1958661417322836440, 0.3392501089628016664, -0.5655974821184234225 ) ) ;
#4886 = CARTESIAN_POINT ( 'NONE',  ( 0.1312335958005255154, -0.5023911411419708095, 0.1820866141732285504 ) ) ;
#4887 = CARTESIAN_POINT ( 'NONE',  ( -0.1958661417322836718, 0.3392501089628017219, -1.042650918635170676 ) ) ;
#4888 = CARTESIAN_POINT ( 'NONE',  ( -0.2034120734908128059, 0.1771653543307087630, 0.09757992244046791164 ) ) ;
#4889 = CARTESIAN_POINT ( 'NONE',  ( 0.4199475065616803948, -0.5023911411419708095, -0.1820866141732282451 ) ) ;
#4890 = CARTESIAN_POINT ( 'NONE',  ( 0.6496062992125991586, 0.1660481256975885056, 0.3530559997133364547 ) ) ;
#4891 = CARTESIAN_POINT ( 'NONE',  ( -0.9120734908136475250, -0.5511811023622048555, -0.09757992244046775898 ) ) ;
#4892 = CARTESIAN_POINT ( 'NONE',  ( 0.1958661417322836440, -0.3392501089628017219, -2.288713910761154935 ) ) ;
#4893 = CARTESIAN_POINT ( 'NONE',  ( 1.410761154855643795, -0.3162353388693405765, 0.4822834645669290543 ) ) ;
#4894 = EDGE_CURVE ( 'NONE', #21217, #49832, #69102, .T. ) ;
#4895 = CIRCLE ( 'NONE', #53246, 0.2952755905511810774 ) ;
#4896 = CARTESIAN_POINT ( 'NONE',  ( -0.9711286089238838626, 0.2306618581243847221, -0.2411417322834647770 ) ) ;
#4897 = AXIS2_PLACEMENT_3D ( 'NONE', #65315, #53901, #45919 ) ;
#4898 = CARTESIAN_POINT ( 'NONE',  ( -0.4724409448818895907, -0.1265901696524993070, -0.5951443569553805935 ) ) ;
#4899 = AXIS2_PLACEMENT_3D ( 'NONE', #46645, #47054, #52534 ) ;
#4900 = CARTESIAN_POINT ( 'NONE',  ( 0.1640419947506569498, -0.05778040916215522460, 0.4822834645669289988 ) ) ;
#4901 = CARTESIAN_POINT ( 'NONE',  ( -0.6824146981627288167, 0.2306618581243848609, 0.2411417322834645549 ) ) ;
#4902 = CARTESIAN_POINT ( 'NONE',  ( 1.259842519685040019, -0.1870078740157480601, -0.3641732283464567677 ) ) ;
#4903 = CARTESIAN_POINT ( 'NONE',  ( 0.09842519685039434474, -0.4536011799217368745, -0.2665933059059886201 ) ) ;
#4904 = CARTESIAN_POINT ( 'NONE',  ( -0.1049868766404193215, 0.2306618581243847221, -0.2411417322834647770 ) ) ;
#4905 = CARTESIAN_POINT ( 'NONE',  ( -1.056430446194224881, -0.6692913385826771977, 0.1292274648535927661 ) ) ;
#4906 = CARTESIAN_POINT ( 'NONE',  ( 1.614173228346456712, 2.401574803149606474, 0.1372047244094478646 ) ) ;
#4907 = CARTESIAN_POINT ( 'NONE',  ( -1.157146581871515012E-16, 0.4724409448818898682, -0.3149606299212598381 ) ) ;
#4908 = CARTESIAN_POINT ( 'NONE',  ( -0.1246719160104980823, -0.6692913385826773087, -0.1292274648535924053 ) ) ;
#4909 = ORIENTED_EDGE ( 'NONE', *, *, #50636, .F. ) ;
#4910 = CARTESIAN_POINT ( 'NONE',  ( 0.1070741851644054776, -0.3996062992125984925, -1.894356955380577023 ) ) ;
#4911 =( BOUNDED_CURVE ( )  B_SPLINE_CURVE ( 3, ( #22328, #47991, #39286, #67369 ),
 .UNSPECIFIED., .F., .F. ) 
 B_SPLINE_CURVE_WITH_KNOTS ( ( 4, 4 ),
 ( 1.859270518042427600, 2.743397753083149926 ),
 .UNSPECIFIED. ) 
 CURVE ( )  GEOMETRIC_REPRESENTATION_ITEM ( )  RATIONAL_B_SPLINE_CURVE ( ( 1.000000000000000000, 0.9359138408343250504, 0.9359138408343250504, 1.000000000000000000 ) ) 
 REPRESENTATION_ITEM ( '' )  );
#4912 = EDGE_CURVE ( 'NONE', #71641, #53395, #37929, .T. ) ;
#4913 = CARTESIAN_POINT ( 'NONE',  ( 1.312335958005249825, 0.2306618581243847221, -0.2411417322834647770 ) ) ;
#4914 = CARTESIAN_POINT ( 'NONE',  ( -0.5052493438320203589, -0.5511811023622046335, 0.09757992244046803654 ) ) ;
#4915 = AXIS2_PLACEMENT_3D ( 'NONE', #67213, #9546, #29312 ) ;
#4916 = CARTESIAN_POINT ( 'NONE',  ( -0.6167979002624665030, 0.05413385826771666132, 0.4176697321401328100 ) ) ;
#4917 = CARTESIAN_POINT ( 'NONE',  ( 1.161417322834646493, -0.5400638737290844871, 0.3530559997133364547 ) ) ;
#4918 = CARTESIAN_POINT ( 'NONE',  ( 1.082677165354331228, 0.1660481256975883668, -0.3530559997133364547 ) ) ;
#4919 = CARTESIAN_POINT ( 'NONE',  ( -1.574803149606298192, -0.1870078740157480879, -0.4822834645669291653 ) ) ;
#4920 = CARTESIAN_POINT ( 'NONE',  ( -1.207349081364828880, 0.1283753931104746893, -0.1820866141732285504 ) ) ;
#4921 = CARTESIAN_POINT ( 'NONE',  ( -0.3460692066303957537, -0.1998031496062994405, -0.1292650918635170898 ) ) ;
#4922 = CARTESIAN_POINT ( 'NONE',  ( -0.2925321140481932924, 0.2925321140481931814, -0.3346456692913385988 ) ) ;
#4923 = CARTESIAN_POINT ( 'NONE',  ( -0.3949938075777409408, -0.1058382717557502933, -0.3608923884514436686 ) ) ;
#4924 = CARTESIAN_POINT ( 'NONE',  ( 0.1656725442894022571, 1.091696002692744250, 2.847499275411782715 ) ) ;
#4925 = CARTESIAN_POINT ( 'NONE',  ( -3.912791665790199769, 1.724409448818897905, 0.4359958488159718093 ) ) ;
#4926 = CARTESIAN_POINT ( 'NONE',  ( 0.6364829396325465405, -0.08942795157527998196, 0.3641732283464567121 ) ) ;
#4927 = CARTESIAN_POINT ( 'NONE',  ( 0.3346456692913390985, 0.1660481256975885056, 0.3530559997133364547 ) ) ;
#4928 = CARTESIAN_POINT ( 'NONE',  ( 0.2378425880835043915, -0.1752652180395700143, 0.1496354662858539464 ) ) ;
#4929 = CARTESIAN_POINT ( 'NONE',  ( -0.1974969037888706924, 0.3420746716998658843, -0.8772965879265093303 ) ) ;
#4930 = CARTESIAN_POINT ( 'NONE',  ( 0.8530183727034128527, -0.3690944881889763329, 0.3153832671262228327 ) ) ;
#4931 = CARTESIAN_POINT ( 'NONE',  ( -0.4199475065616791736, -0.6046776061558807314, 0.2411417322834647770 ) ) ;
#4932 = CARTESIAN_POINT ( 'NONE',  ( -0.7086614173228339419, -0.1870078740157479769, 0.4822834645669291653 ) ) ;
#4933 = CARTESIAN_POINT ( 'NONE',  ( 1.187664041994751285, -0.05778040916215522460, 0.4822834645669289988 ) ) ;
#4934 = B_SPLINE_CURVE_WITH_KNOTS ( 'NONE', 3,
 ( #32380, #7980, #44991, #52145 ),
 .UNSPECIFIED., .F., .F.,
 ( 4, 4 ),
 ( 0.1307222445546316614, 0.1321409493595269991 ),
 .UNSPECIFIED. ) ;
#4935 = CARTESIAN_POINT ( 'NONE',  ( 0.4091458600556403535, 0.2362204724409449896, -1.233595800524934338 ) ) ;
#4936 = CARTESIAN_POINT ( 'NONE',  ( 0.2925321140481932369, 0.2925321140481932369, -2.185039370078739829 ) ) ;
#4937 = CARTESIAN_POINT ( 'NONE',  ( -0.2559055118110230564, 0.07958543189024071263, -0.2665933059059888421 ) ) ;
#4938 = ORIENTED_EDGE ( 'NONE', *, *, #80939, .F. ) ;
#4939 = CARTESIAN_POINT ( 'NONE',  ( -0.3917322834645670104, -0.1049643490035307020, -0.6725914942595296875 ) ) ;
#4940 = ORIENTED_EDGE ( 'NONE', *, *, #8497, .F. ) ;
#4941 = CARTESIAN_POINT ( 'NONE',  ( -0.6889763779527552368, -0.5400638737290845981, -0.3530559997133363437 ) ) ;
#4942 = CARTESIAN_POINT ( 'NONE',  ( -0.2887139107611542133, -0.6046776061558809534, -0.2411417322834644161 ) ) ;
#4943 = CARTESIAN_POINT ( 'NONE',  ( -0.2690288713910754526, -0.6692913385826771977, 0.1292274648535927661 ) ) ;
#4944 = CARTESIAN_POINT ( 'NONE',  ( 0.5708661417322842269, 0.1660481256975885056, 0.3530559997133364547 ) ) ;
#4945 = CARTESIAN_POINT ( 'NONE',  ( -0.5052493438320203589, 0.2952755905511810774, -0.1292274648535930714 ) ) ;
#4946 = CARTESIAN_POINT ( 'NONE',  ( -1.469816272965878357, 0.2306618581243848609, 0.2411417322834645549 ) ) ;
#4947 = CARTESIAN_POINT ( 'NONE',  ( -0.8202099737532801971, -0.6692913385826771977, 0.1292274648535927661 ) ) ;
#4948 = CARTESIAN_POINT ( 'NONE',  ( 0.8136482939632553313, 0.2306618581243848609, 0.2411417322834645549 ) ) ;
#4949 = CARTESIAN_POINT ( 'NONE',  ( 0.3392501089628018329, 0.1958661417322835607, -0.9107611548556429071 ) ) ;
#4950 = CARTESIAN_POINT ( 'NONE',  ( -0.5708661417322825615, -0.4536011799217367080, 0.2665933059059888421 ) ) ;
#4951 = ORIENTED_EDGE ( 'NONE', *, *, #71288, .F. ) ;
#4952 = CARTESIAN_POINT ( 'NONE',  ( 4.837279021331060870E-17, -0.3949938075777409963, -1.338582677165354173 ) ) ;
#4953 = AXIS2_PLACEMENT_3D ( 'NONE', #39750, #27536, #65446 ) ;
#4954 = EDGE_LOOP ( 'NONE', ( #61444, #23136, #36130, #74334 ) ) ;
#4955 = CARTESIAN_POINT ( 'NONE',  ( -1.423884514435694859, -0.2845877964562159024, 0.3641732283464567677 ) ) ;
#4956 = AXIS2_PLACEMENT_3D ( 'NONE', #30902, #44748, #12384 ) ;
#4957 = CARTESIAN_POINT ( 'NONE',  ( -1.049868766404198794, -0.6046776061558807314, 0.2411417322834647770 ) ) ;
#4958 = CARTESIAN_POINT ( 'NONE',  ( -0.9580052493438311334, 0.05413385826771626580, -0.4176697321401330321 ) ) ;
#4959 = CARTESIAN_POINT ( 'NONE',  ( -0.3149606299212459048, 2.559055118110236560, -3.924389226575469625 ) ) ;
#4960 = CARTESIAN_POINT ( 'NONE',  ( -0.9055118110236215490, 0.2952755905511811885, 0.000000000000000000 ) ) ;
#4961 = CARTESIAN_POINT ( 'NONE',  ( -0.7020997375328076329, -0.3162353388693409650, -0.4822834645669289433 ) ) ;
#4962 = CARTESIAN_POINT ( 'NONE',  ( 2.543486866223389153, 2.716535433070866645, -0.5314960629921260393 ) ) ;
#4963 = EDGE_CURVE ( 'NONE', #3706, #81247, #78485, .T. ) ;
#4964 = CARTESIAN_POINT ( 'NONE',  ( -0.4422811034547447506, 1.709755814870675072, -3.912091310349552931 ) ) ;
#4965 = CARTESIAN_POINT ( 'NONE',  ( 0.6430446194225729606, -0.3690944881889765550, -0.3153832671262227771 ) ) ;
#4966 = CARTESIAN_POINT ( 'NONE',  ( -0.6299212598425059095, 2.165354330708661568, -3.937007874015764131 ) ) ;
#4967 = CARTESIAN_POINT ( 'NONE',  ( 0.3917322834645670104, -0.1049643490035303411, -0.03871391076115493490 ) ) ;
#4968 = CARTESIAN_POINT ( 'NONE',  ( 0.1771653543307093182, 0.07958543189024085140, 0.2665933059059887866 ) ) ;
#4969 = CARTESIAN_POINT ( 'NONE',  ( -0.5774278215223089816, -0.6046776061558807314, 0.2411417322834647770 ) ) ;
#4970 = EDGE_CURVE ( 'NONE', #14187, #15098, #5125, .T. ) ;
#4971 = CARTESIAN_POINT ( 'NONE',  ( 3.908320185825792770, 1.506033013147133115, 0.4744094488188977388 ) ) ;
#4972 = CARTESIAN_POINT ( 'NONE',  ( -0.09842519685039295696, -0.5400638737290844871, 0.3530559997133364547 ) ) ;
#4973 = ORIENTED_EDGE ( 'NONE', *, *, #14716, .T. ) ;
#4974 = CARTESIAN_POINT ( 'NONE',  ( -9.787531504996567848E-17, 0.3996062992125986035, -2.047244094488188892 ) ) ;
#4975 = CARTESIAN_POINT ( 'NONE',  ( -0.8398950131233585692, 0.1539470093639523085, 0.1968503937007873850 ) ) ;
#4976 = VERTEX_POINT ( 'NONE', #50140 ) ;
#4977 = CARTESIAN_POINT ( 'NONE',  ( 0.2925321140481932369, -0.2925321140481931814, -1.750000000000000222 ) ) ;
#4978 = CARTESIAN_POINT ( 'NONE',  ( 1.555118110236221041, -0.5400638737290844871, 0.3530559997133364547 ) ) ;
#4979 = CARTESIAN_POINT ( 'NONE',  ( -1.338582677165353729, -0.1870078740157480601, -0.3641732283464567677 ) ) ;
#4980 = CARTESIAN_POINT ( 'NONE',  ( -0.8727034120734901146, -0.05778040916215560624, -0.4822834645669293319 ) ) ;
#4981 = CARTESIAN_POINT ( 'NONE',  ( -1.157146581871515012E-16, 0.4724409448818898682, -0.4724409448818898127 ) ) ;
#4982 = CARTESIAN_POINT ( 'NONE',  ( -0.4323474733757479704, 1.341489562532706792, 3.913201052770269861 ) ) ;
#4983 = CARTESIAN_POINT ( 'NONE',  ( 0.1049643490035304938, -0.3917322834645669549, -0.07742782152230966164 ) ) ;
#4984 = CARTESIAN_POINT ( 'NONE',  ( 1.450131233595801428, -0.6692913385826773087, -0.1292274648535924053 ) ) ;
#4985 = CARTESIAN_POINT ( 'NONE',  ( 0.2493438320209980519, -0.4281496062992127816, -0.4176697321401328100 ) ) ;
#4986 = CARTESIAN_POINT ( 'NONE',  ( 0.3740157480314966754, -0.5400638737290844871, 0.3530559997133364547 ) ) ;
#4987 = CARTESIAN_POINT ( 'NONE',  ( -1.246719160104985846, -0.3690944881889765550, -0.3153832671262227771 ) ) ;
#4988 = CARTESIAN_POINT ( 'NONE',  ( -0.4790026246719154557, -0.3162353388693405765, 0.4822834645669290543 ) ) ;
#4989 = CARTESIAN_POINT ( 'NONE',  ( -0.3458507752293906723, -0.3458507752293910609, -2.498031496062992574 ) ) ;
#4990 = CARTESIAN_POINT ( 'NONE',  ( -0.8530183727034112984, -0.4281496062992127816, -0.4176697321401328100 ) ) ;
#4991 = CARTESIAN_POINT ( 'NONE',  ( -0.1058382717557503072, 0.3949938075777408852, -2.445538057742782101 ) ) ;
#4992 = CARTESIAN_POINT ( 'NONE',  ( 1.410761154855643795, -0.2845877964562159024, 0.3641732283464567677 ) ) ;
#4993 = CARTESIAN_POINT ( 'NONE',  ( -0.2099737532808391705, -0.5023911411419708095, -0.1820866141732282451 ) ) ;
#4994 = CARTESIAN_POINT ( 'NONE',  ( 1.095800524934383846, -0.08942795157528024563, -0.3641732283464568787 ) ) ;
#4995 = CARTESIAN_POINT ( 'NONE',  ( -1.443569553805773564, -0.6046776061558807314, 0.2411417322834647770 ) ) ;
#4996 = CARTESIAN_POINT ( 'NONE',  ( -1.240157480314959759, -0.4536011799217368745, -0.2665933059059886201 ) ) ;
#4997 = CARTESIAN_POINT ( 'NONE',  ( 0.9348729704079946634, -8.644661201599092366E-16, -0.4445507791589066171 ) ) ;
#4998 = CARTESIAN_POINT ( 'NONE',  ( 0.4133858267716541968, 0.07958543189024085140, 0.2665933059059887866 ) ) ;
#4999 = CARTESIAN_POINT ( 'NONE',  ( -0.4986876640419939388, 0.2306618581243847221, -0.2411417322834647770 ) ) ;
#5000 = CARTESIAN_POINT ( 'NONE',  ( -2.170146923806675510, 1.537401574803149984, 0.4744094488188970171 ) ) ;
#5001 = CARTESIAN_POINT ( 'NONE',  ( -0.05249343832020911260, 0.1283753931104748280, 0.1820866141732283561 ) ) ;
#5002 = CARTESIAN_POINT ( 'NONE',  ( -1.732283464566928277, -0.1870078740157479769, 0.3641732283464567677 ) ) ;
#5003 = CARTESIAN_POINT ( 'NONE',  ( 0.6036745406824154392, 0.2306618581243847221, -0.2411417322834647770 ) ) ;
#5004 = DIRECTION ( 'NONE',  ( 0.000000000000000000, -1.000000000000000000, 0.000000000000000000 ) ) ;
#5005 = CARTESIAN_POINT ( 'NONE',  ( 1.423884514435696191, -0.08942795157527998196, 0.3641732283464567121 ) ) ;
#5006 = CARTESIAN_POINT ( 'NONE',  ( -1.115485564304461219, -0.4281496062992124485, 0.4176697321401328655 ) ) ;
#5007 = CARTESIAN_POINT ( 'NONE',  ( -0.08530183727034056085, -0.2845877964562159024, 0.3641732283464567677 ) ) ;
#5008 = CARTESIAN_POINT ( 'NONE',  ( 0.000000000000000000, 0.04921259842519689481, -0.08523872084492506440 ) ) ;
#5009 = CARTESIAN_POINT ( 'NONE',  ( 0.3215223097112867578, -0.08942795157527998196, 0.3641732283464567121 ) ) ;
#5010 = CARTESIAN_POINT ( 'NONE',  ( -1.332020997375327642, -0.3162353388693409650, -0.4822834645669289433 ) ) ;
#5011 = CARTESIAN_POINT ( 'NONE',  ( -0.4068241469816264999, -0.4281496062992124485, 0.4176697321401328655 ) ) ;
#5012 = CARTESIAN_POINT ( 'NONE',  ( -0.1998031496062991630, -0.3460692066303959202, -0.6148293963254594097 ) ) ;
#5013 = VECTOR ( 'NONE', #6228, 39.37007874015748143 ) ;
#5014 = CARTESIAN_POINT ( 'NONE',  ( 0.3917322834645669549, 0.1049643490035304660, -2.256561679790026531 ) ) ;
#5015 = CARTESIAN_POINT ( 'NONE',  ( 0.4527559055118117182, -0.4536011799217367080, 0.2665933059059888421 ) ) ;
#5017 = PRESENTATION_LAYER_ASSIGNMENT (  '', '', ( #30554 ) ) ;
#5016 = CARTESIAN_POINT ( 'NONE',  ( -0.3215223097112853146, -0.05778040916215560624, -0.4822834645669293319 ) ) ;
#5018 = CARTESIAN_POINT ( 'NONE',  ( -0.7152230971128602510, -0.3162353388693405765, 0.4822834645669290543 ) ) ;
#5019 = CARTESIAN_POINT ( 'NONE',  ( -0.7545931758530176614, -0.5511811023622048555, -0.09757992244046775898 ) ) ;
#5020 = CARTESIAN_POINT ( 'NONE',  ( -3.935120607642087709, 1.078895829074301593, -0.1227907875732516252 ) ) ;
#5021 = CARTESIAN_POINT ( 'NONE',  ( -0.07874015748031421014, -0.1870078740157479769, 0.4822834645669291653 ) ) ;
#5022 = CARTESIAN_POINT ( 'NONE',  ( -1.102362204724408601, -0.1870078740157479769, 0.3641732283464567677 ) ) ;
#5023 = CARTESIAN_POINT ( 'NONE',  ( -1.587926509186350810, 0.05413385826771626580, -0.4176697321401330321 ) ) ;
#5024 = CARTESIAN_POINT ( 'NONE',  ( -0.4724409448818917001, 0.1265901696524956710, -2.629265091863517867 ) ) ;
#5025 = VERTEX_POINT ( 'NONE', #56043 ) ;
#5026 = CARTESIAN_POINT ( 'NONE',  ( -1.548556430446193399, 0.1283753931104748280, 0.1820866141732283561 ) ) ;
#5027 = CARTESIAN_POINT ( 'NONE',  ( -1.233595800524933894, 0.2306618581243848609, 0.2411417322834645549 ) ) ;
#5028 = CARTESIAN_POINT ( 'NONE',  ( -0.7152230971128602510, -0.05778040916215560624, -0.4822834645669293319 ) ) ;
#5029 = CARTESIAN_POINT ( 'NONE',  ( -1.417322834645668772, -0.1870078740157480879, -0.4822834645669291653 ) ) ;
#5030 = CARTESIAN_POINT ( 'NONE',  ( -0.1049643490035302024, -0.3917322834645671215, -1.574146981627296604 ) ) ;
#5031 = CARTESIAN_POINT ( 'NONE',  ( 0.000000000000000000, 0.03937007874015747977, 0.000000000000000000 ) ) ;
#5032 = CARTESIAN_POINT ( 'NONE',  ( 1.076115485564305141, 0.2306618581243847221, -0.2411417322834647770 ) ) ;
#5033 = CARTESIAN_POINT ( 'NONE',  ( 0.5511811023622055217, -0.1870078740157479769, 0.4822834645669291653 ) ) ;
#5034 = DIRECTION ( 'NONE',  ( 0.000000000000000000, -0.000000000000000000, 1.000000000000000000 ) ) ;
#5035 = CARTESIAN_POINT ( 'NONE',  ( -0.3460692066303957537, -0.1998031496062994405, -2.491469816272966042 ) ) ;
#5036 = CARTESIAN_POINT ( 'NONE',  ( 1.128608923884514947, 0.1283753931104748280, 0.1820866141732283561 ) ) ;
#5037 = CARTESIAN_POINT ( 'NONE',  ( 0.3996062992125986590, -0.1070741851644053111, -1.056430446194225992 ) ) ;
#5038 = VERTEX_POINT ( 'NONE', #75837 ) ;
#5039 = CARTESIAN_POINT ( 'NONE',  ( -0.7414698162729651543, -0.5511811023622046335, 0.09757992244046803654 ) ) ;
#5040 = CARTESIAN_POINT ( 'NONE',  ( 0.2867679344610365999, 0.2867679344610365999, -2.492125984251968518 ) ) ;
#5041 = EDGE_LOOP ( 'NONE', ( #59399, #1348, #43449, #26373 ) ) ;
#5042 = CARTESIAN_POINT ( 'NONE',  ( 0.4658792650918640033, -0.3162353388693405765, 0.4822834645669290543 ) ) ;
#5043 = CARTESIAN_POINT ( 'NONE',  ( -0.7414698162729651543, 0.2952755905511810774, -0.1292274648535930714 ) ) ;
#5044 = CARTESIAN_POINT ( 'NONE',  ( -1.043307086614172041, -0.5400638737290844871, 0.3530559997133364547 ) ) ;
#5045 = CARTESIAN_POINT ( 'NONE',  ( 0.9514435695538062676, -0.3162353388693409650, -0.4822834645669289433 ) ) ;
#5046 = CARTESIAN_POINT ( 'NONE',  ( 1.666666666666667185, 0.05413385826771666132, 0.4176697321401328100 ) ) ;
#5047 = CARTESIAN_POINT ( 'NONE',  ( -6.686372609646914991E-25, 1.062992125984252745, 1.850393700787401619 ) ) ;
#5048 = CARTESIAN_POINT ( 'NONE',  ( -0.2099737532808391705, 0.2306618581243848609, 0.2411417322834645549 ) ) ;
#5049 = CARTESIAN_POINT ( 'NONE',  ( -1.377952755905511140, -0.6692913385826771977, 8.415575281601705876E-17 ) ) ;
#5050 = CARTESIAN_POINT ( 'NONE',  ( 0.5314960629921294810, 2.559055118110236560, -0.9881811337016621621 ) ) ;
#5051 = CARTESIAN_POINT ( 'NONE',  ( 1.601049868766404982, -0.6046776061558809534, -0.2411417322834644161 ) ) ;
#5052 = CARTESIAN_POINT ( 'NONE',  ( 0.3917322834645669549, 0.1049643490035304660, -2.729002624671915900 ) ) ;
#5053 = CARTESIAN_POINT ( 'NONE',  ( 0.8136482939632553313, -0.5023911411419708095, -0.1820866141732282451 ) ) ;
#5054 = VERTEX_POINT ( 'NONE', #31612 ) ;
#5055 = CARTESIAN_POINT ( 'NONE',  ( -0.3420746716998661618, 0.1974969037888702206, -0.3412073490813648524 ) ) ;
#5056 = EDGE_LOOP ( 'NONE', ( #31226, #15117, #67513, #8693 ) ) ;
#5057 = CARTESIAN_POINT ( 'NONE',  ( 0.1181102362204730916, -0.5511811023622047445, 6.969142054262312111E-17 ) ) ;
#5058 = CARTESIAN_POINT ( 'NONE',  ( -1.489501312335957062, -0.3162353388693409650, -0.4822834645669289433 ) ) ;
#5059 = CARTESIAN_POINT ( 'NONE',  ( 0.5577427821522314977, -0.3162353388693409650, -0.4822834645669289433 ) ) ;
#5060 = CARTESIAN_POINT ( 'NONE',  ( 0.5314960629921264834, 0.1660481256975883668, -0.3530559997133364547 ) ) ;
#5061 = ADVANCED_FACE ( 'NONE', ( #82971 ), #81751, .F. ) ;
#5062 = CARTESIAN_POINT ( 'NONE',  ( -0.5708661417322828946, 0.1660481256975883668, -0.3530559997133364547 ) ) ;
#5063 = CARTESIAN_POINT ( 'NONE',  ( 0.2867679344610366554, 0.2867679344610366554, -1.236895956201786717 ) ) ;
#5064 = CARTESIAN_POINT ( 'NONE',  ( -1.240157480314959759, -0.5400638737290845981, -0.3530559997133363437 ) ) ;
#5065 = CARTESIAN_POINT ( 'NONE',  ( -0.2867679344610364334, -0.2867679344610367109, -2.505905511811023612 ) ) ;
#5066 = CARTESIAN_POINT ( 'NONE',  ( 1.476377952755906220, 0.07958543189024071263, -0.2665933059059888421 ) ) ;
#5067 = CARTESIAN_POINT ( 'NONE',  ( -0.9973753280839886548, 0.2306618581243848609, 0.2411417322834645549 ) ) ;
#5068 = CARTESIAN_POINT ( 'NONE',  ( 0.8661417322834653598, -0.1870078740157479769, 0.4822834645669291653 ) ) ;
#5069 = CARTESIAN_POINT ( 'NONE',  ( 1.345144356955381593, -0.05778040916215522460, 0.4822834645669289988 ) ) ;
#5070 = CARTESIAN_POINT ( 'NONE',  ( 4.893765752498283924E-17, -0.3996062992125986035, -0.7086614173228346081 ) ) ;
#5071 = CARTESIAN_POINT ( 'NONE',  ( -1.535433070866141225, 0.2952755905511811885, 0.000000000000000000 ) ) ;
#5072 = CARTESIAN_POINT ( 'NONE',  ( -0.2925321140481932369, 0.2925321140481931259, -0.2539370078740156855 ) ) ;
#5073 = CARTESIAN_POINT ( 'NONE',  ( 0.4461942257217855201, -0.6046776061558807314, 0.2411417322834647770 ) ) ;
#5074 = CARTESIAN_POINT ( 'NONE',  ( -9.787531504996567848E-17, 0.3996062992125986035, -2.204724409448818978 ) ) ;
#5075 = CARTESIAN_POINT ( 'NONE',  ( 0.3917322834645670104, -0.1049643490035303411, -1.770997375328083656 ) ) ;
#5076 = CARTESIAN_POINT ( 'NONE',  ( -1.515748031496062076, -0.4536011799217367080, 0.2665933059059888421 ) ) ;
#5077 = CARTESIAN_POINT ( 'NONE',  ( 0.4133858267716541968, 0.07958543189024085140, 0.2665933059059887866 ) ) ;
#5078 = CARTESIAN_POINT ( 'NONE',  ( 0.7742782152230978099, -0.4281496062992124485, 0.4176697321401328655 ) ) ;
#5079 = CARTESIAN_POINT ( 'NONE',  ( 0.4091458600556404646, -0.2362204724409448231, -1.284120734908136496 ) ) ;
#5080 = CARTESIAN_POINT ( 'NONE',  ( 0.6692913385826778638, -0.5511811023622047445, 6.969142054262312111E-17 ) ) ;
#5081 = CARTESIAN_POINT ( 'NONE',  ( 0.3346456692913390985, 0.1660481256975885056, 0.3530559997133364547 ) ) ;
#5082 = CARTESIAN_POINT ( 'NONE',  ( 0.3949938075777409963, 2.418639510665530743E-17, -0.9822834645669292764 ) ) ;
#5083 = CARTESIAN_POINT ( 'NONE',  ( -0.8005249343832013809, -0.4281496062992124485, 0.4176697321401328655 ) ) ;
#5084 = FACE_OUTER_BOUND ( 'NONE', #51511, .T. ) ;
#5085 = DIMENSIONAL_EXPONENTS ( 1.000000000000000000, 0.000000000000000000, 0.000000000000000000, 0.000000000000000000, 0.000000000000000000, 0.000000000000000000, 0.000000000000000000 ) ;
#5086 = CARTESIAN_POINT ( 'NONE',  ( 0.8989501312335963501, -0.5511811023622048555, -0.09757992244046775898 ) ) ;
#5087 = CARTESIAN_POINT ( 'NONE',  ( -0.1509186351706028884, -0.05778040916215522460, 0.4822834645669289988 ) ) ;
#5088 = CARTESIAN_POINT ( 'NONE',  ( -1.115485564304461219, 0.05413385826771626580, -0.4176697321401330321 ) ) ;
#5089 = CARTESIAN_POINT ( 'NONE',  ( -0.1509186351706028884, -0.05778040916215522460, 0.4822834645669289988 ) ) ;
#5090 = CARTESIAN_POINT ( 'NONE',  ( 0.05905511811023709395, -0.4536011799217367080, 0.2665933059059888421 ) ) ;
#5091 = CARTESIAN_POINT ( 'NONE',  ( -2.565212732165802478, 1.469708627452555261, 0.4698506773045482698 ) ) ;
#5092 = CARTESIAN_POINT ( 'NONE',  ( -0.4593175853018366950, 0.05413385826771666132, 0.4176697321401328100 ) ) ;
#5093 = CARTESIAN_POINT ( 'NONE',  ( 0.6102362204724416372, -0.4536011799217367080, 0.2665933059059888421 ) ) ;
#5094 = CARTESIAN_POINT ( 'NONE',  ( 1.604771003085129433, 1.320215725944020813, 0.1466069496707751441 ) ) ;
#5095 = CARTESIAN_POINT ( 'NONE',  ( -0.3996062992125984925, -0.1070741851644056858, -1.854986876640420057 ) ) ;
#5096 = CARTESIAN_POINT ( 'NONE',  ( 0.3346456692913393205, -0.5400638737290845981, -0.3530559997133363437 ) ) ;
#5097 =( BOUNDED_CURVE ( )  B_SPLINE_CURVE ( 2, ( #2336, #73030, #14139, #47340, #40212, #8230, #65053, #78951, #14965, #53652, #21269, #9064, #65486 ),
 .UNSPECIFIED., .F., .F. ) 
 B_SPLINE_CURVE_WITH_KNOTS ( ( 3, 2, 2, 2, 2, 2, 3 ),
 ( 0.1740332660251417696, 0.1742424242424242542, 0.1780303030303030387, 0.1818181818181818232, 0.1856060606060606077, 0.1893939393939393923, 0.1896030976112218769 ),
 .UNSPECIFIED. ) 
 CURVE ( )  GEOMETRIC_REPRESENTATION_ITEM ( )  RATIONAL_B_SPLINE_CURVE ( ( 0.9964447847208424136, 0.9981185001348094055, 1.000000000000000000, 0.9659258262890683122, 1.000000000000000000, 0.9659258262890683122, 1.000000000000000000, 0.9659258262890683122, 1.000000000000000000, 0.9659258262890683122, 1.000000000000000000, 0.9981185001348095165, 0.9964447847208426357 ) ) 
 REPRESENTATION_ITEM ( '' )  );
#5098 = CARTESIAN_POINT ( 'NONE',  ( 1.338582677165355062, -0.1870078740157479769, 0.3641732283464567677 ) ) ;
#5099 = DIRECTION ( 'NONE',  ( -1.000000000000000000, -3.469446951953613696E-16, 0.000000000000000000 ) ) ;
#5100 = CARTESIAN_POINT ( 'NONE',  ( -0.3280839895013117347, -0.3690944881889763329, 0.3153832671262228327 ) ) ;
#5101 = CARTESIAN_POINT ( 'NONE',  ( -0.9383202099737524282, -0.08942795157527998196, 0.3641732283464567121 ) ) ;
#5102 = CARTESIAN_POINT ( 'NONE',  ( -0.3412073490813641308, 0.2306618581243847221, -0.2411417322834647770 ) ) ;
#5103 = CARTESIAN_POINT ( 'NONE',  ( 0.2034120734908142214, 0.2952755905511810774, -0.1292274648535930714 ) ) ;
#5104 = CARTESIAN_POINT ( 'NONE',  ( 1.108923884514436686, -0.2845877964562161244, -0.3641732283464567121 ) ) ;
#5105 = CARTESIAN_POINT ( 'NONE',  ( 0.4436778669133205066, 1.368715629171030512, -1.030622242485704110 ) ) ;
#5106 = CARTESIAN_POINT ( 'NONE',  ( 1.548556430446194954, -0.5023911411419708095, 0.1820866141732285504 ) ) ;
#5107 = CARTESIAN_POINT ( 'NONE',  ( 0.7283464566929143125, 0.1660481256975885056, 0.3530559997133364547 ) ) ;
#5108 = DIRECTION ( 'NONE',  ( -0.000000000000000000, -1.000000000000000000, -0.000000000000000000 ) ) ;
#5109 = CARTESIAN_POINT ( 'NONE',  ( 0.1246719160104994284, -0.6692913385826771977, 0.1292274648535927661 ) ) ;
#5110 = CARTESIAN_POINT ( 'NONE',  ( 0.2867679344610365999, 0.2867679344610365999, -0.8523622047244096001 ) ) ;
#5111 = CARTESIAN_POINT ( 'NONE',  ( 0.9842519685039378130, -0.6692913385826771977, 8.415575281601705876E-17 ) ) ;
#5112 = CARTESIAN_POINT ( 'NONE',  ( 0.6036745406824154392, 0.2306618581243847221, -0.2411417322834647770 ) ) ;
#5113 = CARTESIAN_POINT ( 'NONE',  ( -0.4256046601534574925, 1.327241662710675119, -3.913942542435401961 ) ) ;
#5114 = CARTESIAN_POINT ( 'NONE',  ( 0.3346456692913393205, -0.4536011799217368745, -0.2665933059059886201 ) ) ;
#5115 = CARTESIAN_POINT ( 'NONE',  ( 1.305774278215223960, -0.6692913385826771977, 0.1292274648535927661 ) ) ;
#5116 = CARTESIAN_POINT ( 'NONE',  ( 0.2952755905511816326, -0.4536011799217367080, 0.2665933059059888421 ) ) ;
#5117 = CARTESIAN_POINT ( 'NONE',  ( -0.4527559055118102749, -0.5400638737290845981, -0.3530559997133363437 ) ) ;
#5118 = CARTESIAN_POINT ( 'NONE',  ( 0.4330708661417329575, -0.6692913385826771977, 8.415575281601705876E-17 ) ) ;
#5119 = CARTESIAN_POINT ( 'NONE',  ( -0.6102362204724400829, -0.5400638737290845981, -0.3530559997133363437 ) ) ;
#5120 = CARTESIAN_POINT ( 'NONE',  ( -0.2624671916010490880, 0.1283753931104746893, -0.1820866141732285504 ) ) ;
#5121 = CARTESIAN_POINT ( 'NONE',  ( 0.4461942257217855201, -0.6046776061558807314, 0.2411417322834647770 ) ) ;
#5122 = CARTESIAN_POINT ( 'NONE',  ( 0.9383202099737538715, -0.08942795157528024563, -0.3641732283464568787 ) ) ;
#5123 = CARTESIAN_POINT ( 'NONE',  ( -0.2624671916010490880, -0.6046776061558807314, 0.2411417322834647770 ) ) ;
#5124 = SURFACE_STYLE_FILL_AREA ( #25706 ) ;
#5126 = CARTESIAN_POINT ( 'NONE',  ( 0.1998031496062994405, -0.3460692066303958092, -1.036745406824147064 ) ) ;
#5125 = LINE ( 'NONE', #24062, #9694 ) ;
#5127 = CARTESIAN_POINT ( 'NONE',  ( 1.541994750656168645, 0.2952755905511810774, -0.1292274648535930714 ) ) ;
#5128 = PLANE ( 'NONE',  #31473 ) ;
#5129 = VECTOR ( 'NONE', #11670, 39.37007874015748143 ) ;
#5130 = CARTESIAN_POINT ( 'NONE',  ( -1.167979002624671470, 0.05413385826771666132, 0.4176697321401328100 ) ) ;
#5131 = CARTESIAN_POINT ( 'NONE',  ( -0.9120734908136475250, 0.2952755905511811885, 0.1292274648535926551 ) ) ;
#5132 = CARTESIAN_POINT ( 'NONE',  ( -0.4724409448818898682, -8.678599364036362592E-17, -0.5118110236220472231 ) ) ;
#5133 = CARTESIAN_POINT ( 'NONE',  ( -0.3949938075777409963, -7.255918531996591613E-17, -2.559055118110236560 ) ) ;
#5134 = ORIENTED_EDGE ( 'NONE', *, *, #64537, .T. ) ;
#5135 = CARTESIAN_POINT ( 'NONE',  ( 0.3280839895013130669, -0.3690944881889765550, -0.3153832671262227771 ) ) ;
#5136 = CARTESIAN_POINT ( 'NONE',  ( 0.3917322834645670104, -0.1049643490035303411, -1.363517060367453793 ) ) ;
#5137 = CARTESIAN_POINT ( 'NONE',  ( 0.7020997375328090762, -0.05778040916215560624, -0.4822834645669293319 ) ) ;
#5138 = CARTESIAN_POINT ( 'NONE',  ( -0.4091458600556402980, -0.2362204724409451284, -2.414698162729658648 ) ) ;
#5139 = CARTESIAN_POINT ( 'NONE',  ( 0.9776902887139113929, 0.2952755905511811885, 0.1292274648535926551 ) ) ;
#5140 = CARTESIAN_POINT ( 'NONE',  ( -1.673228346456691717, 0.07958543189024071263, -0.2665933059059888421 ) ) ;
#5141 = CARTESIAN_POINT ( 'NONE',  ( 1.253280839895013710, -0.05778040916215560624, -0.4822834645669293319 ) ) ;
#5142 = CARTESIAN_POINT ( 'NONE',  ( 1.292650918635171564, 0.1771653543307087630, 0.09757992244046791164 ) ) ;
#5143 = CARTESIAN_POINT ( 'NONE',  ( 0.05249343832021075018, -0.6046776061558807314, 0.2411417322834647770 ) ) ;
#5144 = CARTESIAN_POINT ( 'NONE',  ( -0.2867679344610364334, -0.2867679344610368219, -0.7690095556092370055 ) ) ;
#5145 = CARTESIAN_POINT ( 'NONE',  ( -0.5052493438320203589, 0.2952755905511810774, -0.1292274648535930714 ) ) ;
#5146 = CARTESIAN_POINT ( 'NONE',  ( -1.233595800524933894, 0.1283753931104748280, 0.1820866141732283561 ) ) ;
#5147 = ADVANCED_FACE ( 'NONE', ( #18584 ), #53, .F. ) ;
#5148 = CARTESIAN_POINT ( 'NONE',  ( -0.4265091863517051496, 0.2952755905511810774, -0.1292274648535930714 ) ) ;
#5149 = CARTESIAN_POINT ( 'NONE',  ( 1.601049868766404982, -0.6046776061558809534, -0.2411417322834644161 ) ) ;
#5150 = DIRECTION ( 'NONE',  ( 1.000000000000000000, 0.000000000000000000, -1.692413147294446216E-16 ) ) ;
#5151 = ORIENTED_EDGE ( 'NONE', *, *, #174, .T. ) ;
#5152 = CARTESIAN_POINT ( 'NONE',  ( -0.3392501089628017219, -0.1958661417322836995, -2.096476008695224991 ) ) ;
#5153 = CARTESIAN_POINT ( 'NONE',  ( 0.3674540682414705883, -0.6046776061558807314, 0.2411417322834647770 ) ) ;
#5154 = ORIENTED_EDGE ( 'NONE', *, *, #20936, .T. ) ;
#5155 = CARTESIAN_POINT ( 'NONE',  ( -0.2690288713910754526, 0.2952755905511810774, -0.1292274648535930714 ) ) ;
#5156 = CARTESIAN_POINT ( 'NONE',  ( -1.561679790026246017, -0.4281496062992127816, -0.4176697321401328100 ) ) ;
#5157 = CARTESIAN_POINT ( 'NONE',  ( 0.6167979002624678353, -0.4281496062992124485, 0.4176697321401328655 ) ) ;
#5158 = EDGE_CURVE ( 'NONE', #80251, #12202, #35238, .T. ) ;
#5159 = CARTESIAN_POINT ( 'NONE',  ( 0.09842519685039434474, 0.1660481256975885056, 0.3530559997133364547 ) ) ;
#5160 = CARTESIAN_POINT ( 'NONE',  ( -0.1049643490035307020, 0.3917322834645669549, -1.351049868766404538 ) ) ;
#5161 = CARTESIAN_POINT ( 'NONE',  ( -0.8070866141732276899, -0.5400638737290844871, 0.3530559997133364547 ) ) ;
#5162 = CARTESIAN_POINT ( 'NONE',  ( 0.08530183727034192087, -0.05778040916215522460, 0.4822834645669289988 ) ) ;
#5163 = CARTESIAN_POINT ( 'NONE',  ( -0.2559055118110227234, -0.5400638737290844871, 0.3530559997133364547 ) ) ;
#5164 = CARTESIAN_POINT ( 'NONE',  ( 0.3805774278215230400, -0.3690944881889763329, 0.3153832671262228327 ) ) ;
#5165 = CARTESIAN_POINT ( 'NONE',  ( -0.2490413359174502850, -0.1587297840844698882, 5.622433025490734870 ) ) ;
#5166 = CARTESIAN_POINT ( 'NONE',  ( -0.2887139107611542133, 0.2306618581243848609, 0.2411417322834645549 ) ) ;
#5167 = DIRECTION ( 'NONE',  ( 0.000000000000000000, 0.000000000000000000, -1.000000000000000000 ) ) ;
#5168 = CARTESIAN_POINT ( 'NONE',  ( -1.568241469816272105, -0.3162353388693409650, -0.4822834645669289433 ) ) ;
#5169 = CARTESIAN_POINT ( 'NONE',  ( 0.3917322834645670104, 2.398668435337828261E-17, -2.944881889763779181 ) ) ;
#5170 = VERTEX_POINT ( 'NONE', #18179 ) ;
#5171 = EDGE_LOOP ( 'NONE', ( #79814, #50362, #35809, #23877 ) ) ;
#5172 = CARTESIAN_POINT ( 'NONE',  ( 0.9055118110236227702, 0.2952755905511811885, 0.000000000000000000 ) ) ;
#5173 = CARTESIAN_POINT ( 'NONE',  ( 0.3018372703412079971, -0.3690944881889763329, 0.3153832671262228327 ) ) ;
#5175 = CARTESIAN_POINT ( 'NONE',  ( 2.795275590551181910, 1.568468489416428469, 0.000000000000000000 ) ) ;
#5174 = DIRECTION ( 'NONE',  ( -1.000000000000000000, -0.000000000000000000, -0.000000000000000000 ) ) ;
#5176 = CARTESIAN_POINT ( 'NONE',  ( -0.1049643490035302024, -0.3917322834645671215, -1.259186351706037099 ) ) ;
#5177 = CARTESIAN_POINT ( 'NONE',  ( 0.2362204724409451007, -0.4091458600556402980, 0.1463254593175852825 ) ) ;
#5178 = DIRECTION ( 'NONE',  ( -0.7071067811865437980, 0.000000000000000000, 0.7071067811865512365 ) ) ;
#5179 = CARTESIAN_POINT ( 'NONE',  ( -0.3420746716998662729, 0.1974969037888702206, 0.2119422572178478181 ) ) ;
#5180 = CARTESIAN_POINT ( 'NONE',  ( 0.5314960629921264834, 0.1660481256975883668, -0.3530559997133364547 ) ) ;
#5181 = CARTESIAN_POINT ( 'NONE',  ( -1.299212598425196097, 0.2952755905511811885, 0.000000000000000000 ) ) ;
#5182 = CARTESIAN_POINT ( 'NONE',  ( -1.030183727034119867, -0.05778040916215560624, -0.4822834645669293319 ) ) ;
#5183 = CARTESIAN_POINT ( 'NONE',  ( 0.4461942257217855201, -0.6046776061558807314, 0.2411417322834647770 ) ) ;
#5184 = CARTESIAN_POINT ( 'NONE',  ( 1.154855643044620184, 0.2306618581243847221, -0.2411417322834647770 ) ) ;
#5185 = CARTESIAN_POINT ( 'NONE',  ( 1.227034120734908917, 0.1771653543307087075, -0.09757992244046823083 ) ) ;
#5186 = CARTESIAN_POINT ( 'NONE',  ( 1.292650918635171564, -0.5511811023622048555, -0.09757992244046775898 ) ) ;
#5187 = CARTESIAN_POINT ( 'NONE',  ( -0.6561679790026240244, 0.2306618581243847221, -0.2411417322834647770 ) ) ;
#5188 = CARTESIAN_POINT ( 'NONE',  ( 0.1070741851644053388, 0.3996062992125986035, -0.5426509186351704539 ) ) ;
#5189 = CARTESIAN_POINT ( 'NONE',  ( 1.548556430446194954, 0.2306618581243847221, -0.2411417322834647770 ) ) ;
#5190 = CARTESIAN_POINT ( 'NONE',  ( 0.1958661417322836440, -0.3392501089628017219, -0.3989501312335957950 ) ) ;
#5191 = CARTESIAN_POINT ( 'NONE',  ( -0.2493438320209966919, -0.4281496062992124485, 0.4176697321401328655 ) ) ;
#5193 = CARTESIAN_POINT ( 'NONE',  ( -0.4744094488189045666, 1.537401574803149984, 2.170146923806632877 ) ) ;
#5192 = CARTESIAN_POINT ( 'NONE',  ( 0.9973753280839902091, -0.6046776061558807314, 0.2411417322834647770 ) ) ;
#5194 = CARTESIAN_POINT ( 'NONE',  ( -1.561679790026246017, -0.004921259842519576551, 0.3153832671262227771 ) ) ;
#5195 = CARTESIAN_POINT ( 'NONE',  ( 0.2493438320209980519, 0.05413385826771666132, 0.4176697321401328100 ) ) ;
#5196 = CARTESIAN_POINT ( 'NONE',  ( 0.7939632545931766261, -0.08942795157527998196, 0.3641732283464567121 ) ) ;
#5197 = B_SPLINE_CURVE_WITH_KNOTS ( 'NONE', 3,
 ( #46124, #52851, #2366, #20888, #46539, #33926, #78562, #26773, #52013, #14588, #34345, #71819, #58760, #46953, #73062, #60010, #1946, #59589, #65924, #7847, #8261, #27608, #53269, #78979, #21300, #72645, #53681, #9095, #20048, #21708, #14995, #40652, #66336, #34768, #60427, #2778, #45700, #71396 ),
 .UNSPECIFIED., .F., .F.,
 ( 4, 2, 2, 2, 2, 2, 2, 2, 2, 2, 2, 2, 2, 2, 2, 2, 2, 2, 4 ),
 ( 2.754675881573757960E-16, 0.003207193274590246918, 0.004810789911885232466, 0.006414386549180218881, 0.007216184867827709487, 0.008017983186475202695, 0.009621579823770182172, 0.01042337814241767538, 0.01122517646106516512, 0.01282877309836014459, 0.01363057141700763954, 0.01443236973565512754, 0.01603596637295011049, 0.01763956301024508996, 0.01924315964754007291, 0.02084675628483505239, 0.02245035292213002839, 0.02405394955942500787, 0.02565754619671998388 ),
 .UNSPECIFIED. ) ;
#5198 = CARTESIAN_POINT ( 'NONE',  ( -1.587926509186350810, -0.3690944881889763329, 0.3153832671262228327 ) ) ;
#5199 = CARTESIAN_POINT ( 'NONE',  ( 0.8005249343832028242, -0.4281496062992127816, -0.4176697321401328100 ) ) ;
#5200 = CARTESIAN_POINT ( 'NONE',  ( 0.000000000000000000, 2.165354330708661568, 0.000000000000000000 ) ) ;
#5201 = CARTESIAN_POINT ( 'NONE',  ( -0.4921259842519677963, -0.4536011799217367080, 0.2665933059059888421 ) ) ;
#5202 = CARTESIAN_POINT ( 'NONE',  ( -0.4199475065616791736, 0.2306618581243847221, -0.2411417322834647770 ) ) ;
#5203 = CARTESIAN_POINT ( 'NONE',  ( 1.555118110236221041, 0.1660481256975883668, -0.3530559997133364547 ) ) ;
#5204 = CARTESIAN_POINT ( 'NONE',  ( -1.128608923884513837, -0.6046776061558807314, 0.2411417322834647770 ) ) ;
#5205 = CARTESIAN_POINT ( 'NONE',  ( 1.325459317585302665, -0.4281496062992124485, 0.4176697321401328655 ) ) ;
#5206 = CARTESIAN_POINT ( 'NONE',  ( -0.3392501089628019995, 0.1958661417322831999, -0.9678670848107107094 ) ) ;
#5207 = CARTESIAN_POINT ( 'NONE',  ( -0.9842519685039360366, 0.1771653543307087630, 0.000000000000000000 ) ) ;
#5208 = CARTESIAN_POINT ( 'NONE',  ( 1.115258233734506055, 1.079260963165236342, 0.1241637467760029201 ) ) ;
#5209 = CARTESIAN_POINT ( 'NONE',  ( 1.338582677165355062, -0.1870078740157480879, -0.4822834645669291653 ) ) ;
#5210 = CARTESIAN_POINT ( 'NONE',  ( -0.4091458600556402980, -0.2362204724409451284, -2.019028871391076230 ) ) ;
#5211 = CARTESIAN_POINT ( 'NONE',  ( 0.4744094488188841385, 1.506018186285911442, 3.908320185825793658 ) ) ;
#5212 = CARTESIAN_POINT ( 'NONE',  ( -1.417322834645668772, -0.1870078740157480601, -0.3641732283464567677 ) ) ;
#5213 = CARTESIAN_POINT ( 'NONE',  ( -0.9120734908136475250, 0.1771653543307087630, 0.09757992244046791164 ) ) ;
#5214 = CARTESIAN_POINT ( 'NONE',  ( 1.601049868766404982, -0.5023911411419708095, -0.1820866141732282451 ) ) ;
#5215 = CARTESIAN_POINT ( 'NONE',  ( -0.3871391076115476282, -0.05778040916215522460, 0.4822834645669289988 ) ) ;
#5216 = CARTESIAN_POINT ( 'NONE',  ( 0.1706036745406830368, -0.3690944881889765550, -0.3153832671262227771 ) ) ;
#5217 = CARTESIAN_POINT ( 'NONE',  ( -1.181102362204723644, -0.1870078740157480601, -0.3641732283464567677 ) ) ;
#5218 = CARTESIAN_POINT ( 'NONE',  ( 1.450131233595801428, 0.1771653543307087630, 0.09757992244046791164 ) ) ;
#5219 = CARTESIAN_POINT ( 'NONE',  ( 1.082677165354331228, 0.1660481256975883668, -0.3530559997133364547 ) ) ;
#5220 = CARTESIAN_POINT ( 'NONE',  ( 1.522309711286089939, -0.6046776061558809534, -0.2411417322834644161 ) ) ;
#5221 = CARTESIAN_POINT ( 'NONE',  ( 0.4921259842519691285, -0.4536011799217368745, -0.2665933059059886201 ) ) ;
#5222 = EDGE_CURVE ( 'NONE', #4446, #39863, #37318, .T. ) ;
#5223 = CARTESIAN_POINT ( 'NONE',  ( 0.6561679790026253567, -0.6046776061558809534, -0.2411417322834644161 ) ) ;
#5224 = CARTESIAN_POINT ( 'NONE',  ( 0.8005249343832027131, -0.004921259842519576551, 0.3153832671262227771 ) ) ;
#5225 = EDGE_LOOP ( 'NONE', ( #25021, #51193, #5134, #58563 ) ) ;
#5226 = CARTESIAN_POINT ( 'NONE',  ( -1.213910761154854745, -0.6692913385826771977, 0.1292274648535927661 ) ) ;
#5227 = CARTESIAN_POINT ( 'NONE',  ( -1.450131233595799651, 0.2952755905511810774, -0.1292274648535930714 ) ) ;
#5228 = CARTESIAN_POINT ( 'NONE',  ( -0.07874015748031421014, -0.1870078740157480879, -0.4822834645669291653 ) ) ;
#5229 = CARTESIAN_POINT ( 'NONE',  ( 0.000000000000000000, 0.07874015748031502893, 0.000000000000000000 ) ) ;
#5230 = CARTESIAN_POINT ( 'NONE',  ( 0.1998031496062992463, 0.3460692066303959202, -2.740813648293963567 ) ) ;
#5231 = CARTESIAN_POINT ( 'NONE',  ( 0.4855643044619428750, 0.05413385826771666132, 0.4176697321401328100 ) ) ;
#5232 = CARTESIAN_POINT ( 'NONE',  ( 1.207349081364829990, -0.5023911411419708095, -0.1820866141732282451 ) ) ;
#5233 = CARTESIAN_POINT ( 'NONE',  ( 0.07874015748031558404, -0.1870078740157479769, 0.4822834645669291653 ) ) ;
#5234 = CARTESIAN_POINT ( 'NONE',  ( 0.2821522309711292364, -0.6692913385826771977, 0.1292274648535927661 ) ) ;
#5235 = CARTESIAN_POINT ( 'NONE',  ( 0.1070741851644053527, 0.3996062992125986590, -2.040682414698162361 ) ) ;
#5236 = CARTESIAN_POINT ( 'NONE',  ( 0.1058382717557500713, -0.3949938075777409408, -1.660104986876640654 ) ) ;
#5237 = CARTESIAN_POINT ( 'NONE',  ( -0.4024773509250166303, 1.285781980195177532, 1.047418557759479008 ) ) ;
#5238 = PLANE ( 'NONE',  #54701 ) ;
#5239 = CARTESIAN_POINT ( 'NONE',  ( -0.1958661417322836718, 0.3392501089628017219, -0.4776902887139107268 ) ) ;
#5240 = CARTESIAN_POINT ( 'NONE',  ( -0.4724409448818890911, -0.1870078740157479769, 0.3641732283464567677 ) ) ;
#5241 = CARTESIAN_POINT ( 'NONE',  ( -0.5511811023622041894, -0.1870078740157480879, -0.4822834645669291653 ) ) ;
#5242 = CARTESIAN_POINT ( 'NONE',  ( 0.5511811023622054106, -0.1870078740157480879, -0.4822834645669291653 ) ) ;
#5243 = CARTESIAN_POINT ( 'NONE',  ( 0.3949938075777409408, -0.1058382717557499186, -2.708005249343832244 ) ) ;
#5244 = CARTESIAN_POINT ( 'NONE',  ( 0.9251968503937015864, 0.1660481256975883668, -0.3530559997133364547 ) ) ;
#5245 = CARTESIAN_POINT ( 'NONE',  ( -1.482939632545930975, 0.05413385826771666132, 0.4176697321401328100 ) ) ;
#5246 = CARTESIAN_POINT ( 'NONE',  ( 0.8989501312335963501, -0.6692913385826773087, -0.1292274648535924053 ) ) ;
#5247 = CARTESIAN_POINT ( 'NONE',  ( 0.2362204724409451007, -0.4091458600556402980, -2.926509186351706315 ) ) ;
#5248 = CARTESIAN_POINT ( 'NONE',  ( -9.787531504996567848E-17, 0.3996062992125986035, -2.204724409448818978 ) ) ;
#5249 = CARTESIAN_POINT ( 'NONE',  ( -0.7478466213799872531, 2.204724409448818978, 0.5309055118110236338 ) ) ;
#5250 = CARTESIAN_POINT ( 'NONE',  ( 1.017060367454068581, -0.05778040916215560624, -0.4822834645669293319 ) ) ;
#5251 = CARTESIAN_POINT ( 'NONE',  ( 0.4199475065616803948, -0.6046776061558809534, -0.2411417322834644161 ) ) ;
#5252 = CARTESIAN_POINT ( 'NONE',  ( 1.030183727034121421, -0.2845877964562161244, -0.3641732283464567121 ) ) ;
#5254 = CARTESIAN_POINT ( 'NONE',  ( 1.292650918635171564, 0.2952755905511811885, 0.1292274648535926551 ) ) ;
#5253 = CARTESIAN_POINT ( 'NONE',  ( 1.601049868766404982, -0.6046776061558809534, -0.2411417322834644161 ) ) ;
#5255 = CARTESIAN_POINT ( 'NONE',  ( 0.1049643490035304938, -0.3917322834645669549, -0.1699475065616798397 ) ) ;
#5256 = SURFACE_SIDE_STYLE ('',( #44356 ) ) ;
#5257 = CARTESIAN_POINT ( 'NONE',  ( 0.9908136482939640111, -0.6692913385826771977, 0.1292274648535927661 ) ) ;
#5258 = CARTESIAN_POINT ( 'NONE',  ( 1.561679790026247350, -0.004921259842519870586, -0.3153832671262229437 ) ) ;
#5259 = CARTESIAN_POINT ( 'NONE',  ( -0.3740157480314953431, -0.5400638737290845981, -0.3530559997133363437 ) ) ;
#5260 = CARTESIAN_POINT ( 'NONE',  ( -1.023622047244094002, -0.1870078740157480879, -0.4822834645669291653 ) ) ;
#5261 = CARTESIAN_POINT ( 'NONE',  ( 1.003937007874016185, 0.1660481256975883668, -0.3530559997133364547 ) ) ;
#5262 = CARTESIAN_POINT ( 'NONE',  ( -0.1049643490035302024, -0.3917322834645671215, -0.6292650918635172008 ) ) ;
#5263 = CARTESIAN_POINT ( 'NONE',  ( 0.3392501089628018329, 0.1958661417322835607, -1.540682414698162805 ) ) ;
#5264 = CARTESIAN_POINT ( 'NONE',  ( 0.3917322834645670104, -0.1049643490035303411, -2.780839895013122565 ) ) ;
#5265 = CARTESIAN_POINT ( 'NONE',  ( -1.535433070866141225, -0.5511811023622047445, 6.969142054262312111E-17 ) ) ;
#5266 = ORIENTED_EDGE ( 'NONE', *, *, #64961, .F. ) ;
#5267 = CARTESIAN_POINT ( 'NONE',  ( 0.3420746716998659953, 0.1974969037888705536, -2.808398950131233640 ) ) ;
#5268 = ORIENTED_EDGE ( 'NONE', *, *, #46085, .F. ) ;
#5269 = CARTESIAN_POINT ( 'NONE',  ( -0.7330049731600569718, 2.221336660396575624, -0.5178675056770626339 ) ) ;
#5270 = CARTESIAN_POINT ( 'NONE',  ( 1.528871391076116026, -0.5511811023622048555, -0.09757992244046775898 ) ) ;
#5271 = CARTESIAN_POINT ( 'NONE',  ( -0.3460692066303960868, 0.1998031496062990242, -1.443569553805774230 ) ) ;
#5272 = CARTESIAN_POINT ( 'NONE',  ( 1.522309711286089939, 0.1283753931104748280, 0.1820866141732283561 ) ) ;
#5273 = CARTESIAN_POINT ( 'NONE',  ( 3.264097702071373064, 2.755905511811024056, -0.5314960629921260393 ) ) ;
#5274 = B_SPLINE_CURVE_WITH_KNOTS ( 'NONE', 3,
 ( #19374, #45024, #11838, #70725, #82944, #17745, #36664 ),
 .UNSPECIFIED., .F., .F.,
 ( 4, 3, 4 ),
 ( 5.204170427930421283E-18, 0.001246230184515548971, 0.002492489877932633786 ),
 .UNSPECIFIED. ) ;
#5275 = DIRECTION ( 'NONE',  ( 0.000000000000000000, 0.000000000000000000, 1.000000000000000000 ) ) ;
#5276 = CARTESIAN_POINT ( 'NONE',  ( -0.1224964469087656410, 1.944119274041657519, 0.2884380004297487088 ) ) ;
#5277 = CARTESIAN_POINT ( 'NONE',  ( 0.1958661417322834775, 0.3392501089628018884, -0.5439632545931759600 ) ) ;
#5278 =( BOUNDED_CURVE ( )  B_SPLINE_CURVE ( 2, ( #67497, #9832, #61167, #3518, #22870, #48531, #16576, #6401, #17813, #69144, #76694, #69558, #50587 ),
 .UNSPECIFIED., .F., .F. ) 
 B_SPLINE_CURVE_WITH_KNOTS ( ( 3, 2, 2, 2, 2, 2, 3 ),
 ( 0.3624999999999999889, 0.3666666666666666408, 0.3708333333333333481, 0.3750000000000000000, 0.3791666666666666519, 0.3833333333333333592, 0.3875000000000000111 ),
 .UNSPECIFIED. ) 
 CURVE ( )  GEOMETRIC_REPRESENTATION_ITEM ( )  RATIONAL_B_SPLINE_CURVE ( ( 1.000000000000000000, 0.9659258262890683122, 1.000000000000000000, 0.9659258262890683122, 1.000000000000000000, 0.9659258262890683122, 1.000000000000000000, 0.9659258262890683122, 1.000000000000000000, 0.9659258262890683122, 1.000000000000000000, 0.9659258262890683122, 1.000000000000000000 ) ) 
 REPRESENTATION_ITEM ( '' )  );
#5279 = CARTESIAN_POINT ( 'NONE',  ( -0.6561679790026240244, 0.1283753931104746893, -0.1820866141732285504 ) ) ;
#5280 = CARTESIAN_POINT ( 'NONE',  ( -1.325459317585300889, -0.3690944881889765550, -0.3153832671262227771 ) ) ;
#5281 = CARTESIAN_POINT ( 'NONE',  ( -1.108923884514435132, -0.05778040916215560624, -0.4822834645669293319 ) ) ;
#5282 = CARTESIAN_POINT ( 'NONE',  ( -0.006561679790025524116, -0.3162353388693405765, 0.4822834645669290543 ) ) ;
#5283 = CARTESIAN_POINT ( 'NONE',  ( -1.167979002624671470, 0.05413385826771666132, 0.4176697321401328100 ) ) ;
#5284 = ORIENTED_EDGE ( 'NONE', *, *, #20936, .F. ) ;
#5285 = EDGE_CURVE ( 'NONE', #1651, #39863, #70298, .T. ) ;
#5286 = CARTESIAN_POINT ( 'NONE',  ( 1.358267716535433323, -0.5400638737290845981, -0.3530559997133363437 ) ) ;
#5287 = PLANE ( 'NONE',  #33955 ) ;
#5288 = DIRECTION ( 'NONE',  ( -0.9988019536772235751, 0.000000000000000000, 0.04893523608364114263 ) ) ;
#5289 = CARTESIAN_POINT ( 'NONE',  ( -0.4724409448818895907, -0.1265901696524993070, -1.935695538057742526 ) ) ;
#5290 = DIRECTION ( 'NONE',  ( 0.000000000000000000, -1.000000000000000000, 0.000000000000000000 ) ) ;
#5291 = CARTESIAN_POINT ( 'NONE',  ( -0.4330708661417315697, -0.5511811023622047445, 6.969142054262312111E-17 ) ) ;
#5292 = EDGE_CURVE ( 'NONE', #18339, #58371, #78937, .T. ) ;
#5293 = CARTESIAN_POINT ( 'NONE',  ( -1.233595800524933894, -0.6046776061558809534, -0.2411417322834644161 ) ) ;
#5294 = CARTESIAN_POINT ( 'NONE',  ( 1.062992125984252745, 0.2952755905511811885, 0.000000000000000000 ) ) ;
#5295 = ORIENTED_EDGE ( 'NONE', *, *, #11474, .F. ) ;
#5297 = CARTESIAN_POINT ( 'NONE',  ( 0.2362204724409451007, -0.4091458600556402980, -2.688320209973753538 ) ) ;
#5296 = DIRECTION ( 'NONE',  ( 0.000000000000000000, 1.000000000000000000, -0.000000000000000000 ) ) ;
#5298 = CONICAL_SURFACE ( 'NONE', #34865, 0.1190944881889763746, 0.8726646259971682085 ) ;
#5299 = CARTESIAN_POINT ( 'NONE',  ( -0.5314960629921371416, 2.755905511811024056, 3.184294706754628557 ) ) ;
#5300 = CARTESIAN_POINT ( 'NONE',  ( -1.082677165354329896, 0.1660481256975885056, 0.3530559997133364547 ) ) ;
#5301 = CARTESIAN_POINT ( 'NONE',  ( -0.1958661417322834497, -0.3392501089628018884, -0.4606106054780034764 ) ) ;
#5302 = CARTESIAN_POINT ( 'NONE',  ( -0.1509186351706028884, -0.08942795157527998196, 0.3641732283464567121 ) ) ;
#5303 = CARTESIAN_POINT ( 'NONE',  ( -9.594673741351313045E-17, 0.3917322834645670104, -0.7145669291338584417 ) ) ;
#5304 = CARTESIAN_POINT ( 'NONE',  ( -0.5774278215223089816, -0.5023911411419708095, 0.1820866141732285504 ) ) ;
#5305 = CARTESIAN_POINT ( 'NONE',  ( 0.6102362204724416372, -0.4536011799217367080, 0.2665933059059888421 ) ) ;
#5306 = CARTESIAN_POINT ( 'NONE',  ( 0.7086614173228352742, -0.1870078740157480879, -0.4822834645669291653 ) ) ;
#5307 = CARTESIAN_POINT ( 'NONE',  ( -0.5446194225721777693, -0.08942795157527998196, 0.3641732283464567121 ) ) ;
#5308 = CARTESIAN_POINT ( 'NONE',  ( -0.1958661417322834220, -0.3392501089628018884, -2.734908136482939511 ) ) ;
#5309 = CARTESIAN_POINT ( 'NONE',  ( 1.036745406824147508, -0.4281496062992127816, -0.4176697321401328100 ) ) ;
#5310 = EDGE_CURVE ( 'NONE', #63414, #42276, #8047, .T. ) ;
#5311 = CARTESIAN_POINT ( 'NONE',  ( -1.115485564304461219, 0.05413385826771626580, -0.4176697321401330321 ) ) ;
#5312 = CARTESIAN_POINT ( 'NONE',  ( 5.785732909357575061E-17, -0.4724409448818898682, -0.9429133858267716439 ) ) ;
#5313 = CARTESIAN_POINT ( 'NONE',  ( -0.07874015748031421014, -0.1870078740157480879, -0.4822834645669291653 ) ) ;
#5314 = CARTESIAN_POINT ( 'NONE',  ( -0.4593175853018364174, -0.4281496062992127816, -0.4176697321401328100 ) ) ;
#5315 = CARTESIAN_POINT ( 'NONE',  ( 1.220472440944882608, 0.1771653543307087630, 0.000000000000000000 ) ) ;
#5316 = CARTESIAN_POINT ( 'NONE',  ( 0.04593175853018440641, 0.1771653543307087075, -0.09757992244046823083 ) ) ;
#5317 = CARTESIAN_POINT ( 'NONE',  ( -0.03280839895013062252, -0.6692913385826771977, 0.1292274648535927661 ) ) ;
#5318 = CARTESIAN_POINT ( 'NONE',  ( -1.181102362204723644, -0.1870078740157479769, 0.4822834645669291653 ) ) ;
#5319 = CARTESIAN_POINT ( 'NONE',  ( -0.7535225988626923499, 2.401574803149606474, 0.4915354330708645025 ) ) ;
#5320 = CARTESIAN_POINT ( 'NONE',  ( 1.541994750656168645, 0.1771653543307087075, -0.09757992244046823083 ) ) ;
#5321 = CARTESIAN_POINT ( 'NONE',  ( -0.1181102362204717315, -0.6692913385826771977, 8.415575281601705876E-17 ) ) ;
#5322 = CARTESIAN_POINT ( 'NONE',  ( -1.305774278215222184, -0.6692913385826773087, -0.1292274648535924053 ) ) ;
#5323 = ORIENTED_EDGE ( 'NONE', *, *, #31050, .F. ) ;
#5324 = CARTESIAN_POINT ( 'NONE',  ( -0.3460692066303957537, -0.1998031496062994405, -2.019028871391076230 ) ) ;
#5325 = CARTESIAN_POINT ( 'NONE',  ( 1.023622047244095112, -0.1870078740157480879, -0.4822834645669291653 ) ) ;
#5326 = CARTESIAN_POINT ( 'NONE',  ( -0.7217847769028863381, -0.004921259842519870586, -0.3153832671262229437 ) ) ;
#5327 = CARTESIAN_POINT ( 'NONE',  ( -0.6627296587926503335, -0.6692913385826771977, 0.1292274648535927661 ) ) ;
#5328 = CARTESIAN_POINT ( 'NONE',  ( 1.181102362204725198, -0.1870078740157479769, 0.4822834645669291653 ) ) ;
#5329 = CARTESIAN_POINT ( 'NONE',  ( 1.095800524934383846, -0.05778040916215560624, -0.4822834645669293319 ) ) ;
#5330 = CYLINDRICAL_SURFACE ( 'NONE', #2210, 0.1771653543307085410 ) ;
#5331 = CARTESIAN_POINT ( 'NONE',  ( -0.9317585301837263412, -0.004921259842519576551, 0.3153832671262227771 ) ) ;
#5332 = CARTESIAN_POINT ( 'NONE',  ( -0.1998031496062991630, -0.3460692066303959202, -0.6148293963254594097 ) ) ;
#5333 = CARTESIAN_POINT ( 'NONE',  ( 4.893765752498283924E-17, -0.3996062992125986035, -1.023622047244094446 ) ) ;
#5334 = CARTESIAN_POINT ( 'NONE',  ( 0.3420746716998659953, 0.1974969037888705536, -0.1312335958005249881 ) ) ;
#5335 = CARTESIAN_POINT ( 'NONE',  ( 0.2422408962274362754, 1.129482473309794788, -1.586876790830786588 ) ) ;
#5336 = CARTESIAN_POINT ( 'NONE',  ( 1.095800524934383846, -0.08942795157528024563, -0.3641732283464568787 ) ) ;
#5337 = CARTESIAN_POINT ( 'NONE',  ( 0.5577427821522314977, -0.2845877964562161244, -0.3641732283464567121 ) ) ;
#5338 = CARTESIAN_POINT ( 'NONE',  ( 0.6167979002624678353, -0.4281496062992124485, 0.4176697321401328655 ) ) ;
#5339 = CARTESIAN_POINT ( 'NONE',  ( 1.594488188976378673, 0.1660481256975885056, 0.3530559997133364547 ) ) ;
#5340 = CARTESIAN_POINT ( 'NONE',  ( -0.3949938075777409963, -7.255918531996591613E-17, -1.375984251968503713 ) ) ;
#5341 = CARTESIAN_POINT ( 'NONE',  ( 0.8858267716535438430, 0.07958543189024085140, 0.2665933059059887866 ) ) ;
#5342 = CARTESIAN_POINT ( 'NONE',  ( -0.1115485564304453947, -0.6692913385826771977, 0.1292274648535927661 ) ) ;
#5343 = CARTESIAN_POINT ( 'NONE',  ( -1.062992125984250968, -0.6692913385826771977, 8.415575281601705876E-17 ) ) ;
#5344 = CARTESIAN_POINT ( 'NONE',  ( 1.463254593175853824, -0.6692913385826771977, 0.1292274648535927661 ) ) ;
#5345 = CARTESIAN_POINT ( 'NONE',  ( -0.2362204724409447953, -0.4091458600556404646, -1.482939632545931863 ) ) ;
#5346 = CARTESIAN_POINT ( 'NONE',  ( 0.1070741851644053666, 0.3996062992125986035, -2.670603674540682260 ) ) ;
#5347 = CARTESIAN_POINT ( 'NONE',  ( 0.04593175853018440641, 0.1771653543307087075, -0.09757992244046823083 ) ) ;
#5348 = ORIENTED_EDGE ( 'NONE', *, *, #39869, .F. ) ;
#5349 = ORIENTED_EDGE ( 'NONE', *, *, #50488, .F. ) ;
#5350 = CARTESIAN_POINT ( 'NONE',  ( -0.9251968503937002541, 0.1660481256975885056, 0.3530559997133364547 ) ) ;
#5351 = CARTESIAN_POINT ( 'NONE',  ( -0.4593175853018364174, -0.4281496062992127816, -0.4176697321401328100 ) ) ;
#5352 = CARTESIAN_POINT ( 'NONE',  ( -0.2624671916010490880, -0.6046776061558807314, 0.2411417322834647770 ) ) ;
#5353 = CARTESIAN_POINT ( 'NONE',  ( 0.5380577427821529035, -0.4281496062992124485, 0.4176697321401328655 ) ) ;
#5354 = CARTESIAN_POINT ( 'NONE',  ( -0.2755905511811015396, -0.6692913385826771977, 8.415575281601705876E-17 ) ) ;
#5355 = CARTESIAN_POINT ( 'NONE',  ( -1.338582677165353729, -0.1870078740157479769, 0.4822834645669291653 ) ) ;
#5356 = CARTESIAN_POINT ( 'NONE',  ( -0.9908136482939626788, -0.6692913385826773087, -0.1292274648535924053 ) ) ;
#5357 = CARTESIAN_POINT ( 'NONE',  ( 0.9317585301837276734, -0.4281496062992124485, 0.4176697321401328655 ) ) ;
#5358 = EDGE_CURVE ( 'NONE', #35363, #59927, #28223, .T. ) ;
#5359 = CARTESIAN_POINT ( 'NONE',  ( 0.1049643490035303689, 0.3917322834645670104, -1.245406824146981561 ) ) ;
#5360 = CARTESIAN_POINT ( 'NONE',  ( -0.3871391076115476282, -0.08942795157527998196, 0.3641732283464567121 ) ) ;
#5361 = VERTEX_POINT ( 'NONE', #32445 ) ;
#5362 = CARTESIAN_POINT ( 'NONE',  ( -0.3420746716998659953, -0.1974969037888706647, -1.312335958005249159 ) ) ;
#5363 = ORIENTED_EDGE ( 'NONE', *, *, #18680, .T. ) ;
#5364 = CARTESIAN_POINT ( 'NONE',  ( -1.187664041994750175, -0.08942795157528024563, -0.3641732283464568787 ) ) ;
#5365 = CARTESIAN_POINT ( 'NONE',  ( -1.154855643044618851, 0.2306618581243848609, 0.2411417322834645549 ) ) ;
#5366 = CARTESIAN_POINT ( 'NONE',  ( -1.030183727034119867, -0.3162353388693405765, 0.4822834645669290543 ) ) ;
#5367 = CARTESIAN_POINT ( 'NONE',  ( -0.3996062992125986035, -0.1070741851644056997, -0.04593175853018373334 ) ) ;
#5368 = CARTESIAN_POINT ( 'NONE',  ( -0.6233595800524928121, -0.05778040916215522460, 0.4822834645669289988 ) ) ;
#5369 = CARTESIAN_POINT ( 'NONE',  ( -0.8267716535433065062, -0.6692913385826771977, 8.415575281601705876E-17 ) ) ;
#5370 = DIRECTION ( 'NONE',  ( -0.000000000000000000, -1.000000000000000000, -0.000000000000000000 ) ) ;
#5371 = DIRECTION ( 'NONE',  ( 0.000000000000000000, 0.4999999999999998335, -0.8660254037844385966 ) ) ;
#5372 = CARTESIAN_POINT ( 'NONE',  ( 0.5314960629921267055, -0.4536011799217367080, 0.2665933059059888421 ) ) ;
#5373 = LINE ( 'NONE', #6190, #36365 ) ;
#5374 = CARTESIAN_POINT ( 'NONE',  ( -0.1049643490035302024, -0.3917322834645671215, 0.0006561679790025351077 ) ) ;
#5375 = CARTESIAN_POINT ( 'NONE',  ( -0.1443569553805768291, -0.004921259842519576551, 0.3153832671262227771 ) ) ;
#5376 = CARTESIAN_POINT ( 'NONE',  ( -0.4199475065616791736, -0.6046776061558807314, 0.2411417322834647770 ) ) ;
#5377 = CARTESIAN_POINT ( 'NONE',  ( 1.410761154855643795, -0.3162353388693405765, 0.4822834645669290543 ) ) ;
#5378 = CARTESIAN_POINT ( 'NONE',  ( -0.07874015748031421014, -0.1870078740157479769, 0.4822834645669291653 ) ) ;
#5379 = ORIENTED_EDGE ( 'NONE', *, *, #44186, .F. ) ;
#5380 = CARTESIAN_POINT ( 'NONE',  ( -0.3996062992125986035, -0.1070741851644056997, -2.093175853018372834 ) ) ;
#5381 = CARTESIAN_POINT ( 'NONE',  ( -0.8136482939632537770, 0.1539470093639521697, -0.1968503937007875793 ) ) ;
#5382 = ORIENTED_EDGE ( 'NONE', *, *, #53323, .T. ) ;
#5383 = CARTESIAN_POINT ( 'NONE',  ( 0.3996062992125985480, 2.446882876249141654E-17, -1.612204724409448842 ) ) ;
#5384 = CARTESIAN_POINT ( 'NONE',  ( -1.646051170424378096, 0.000000000000000000, -0.3464511005275205946 ) ) ;
#5385 = CARTESIAN_POINT ( 'NONE',  ( -0.9317585301837263412, -0.004921259842519576551, 0.3153832671262227771 ) ) ;
#5386 = CARTESIAN_POINT ( 'NONE',  ( -1.213910761154854745, 0.2952755905511810774, -0.1292274648535930714 ) ) ;
#5387 = CARTESIAN_POINT ( 'NONE',  ( 0.3458507752293908943, 0.3458507752293908943, -0.6102362204724409711 ) ) ;
#5388 = CARTESIAN_POINT ( 'NONE',  ( -0.1528522289550877378, 1.087215528301579193, 3.934144666135135360 ) ) ;
#5389 = CARTESIAN_POINT ( 'NONE',  ( -0.3392501089628017219, -0.1958661417322836718, -2.814304461942257252 ) ) ;
#5390 = CARTESIAN_POINT ( 'NONE',  ( 1.187664041994751285, -0.05778040916215522460, 0.4822834645669289988 ) ) ;
#5391 = CARTESIAN_POINT ( 'NONE',  ( 0.2952755905511816326, -0.5400638737290844871, 0.3530559997133364547 ) ) ;
#5392 = CARTESIAN_POINT ( 'NONE',  ( 0.1706036745406830368, -0.4281496062992127816, -0.4176697321401328100 ) ) ;
#5393 = CARTESIAN_POINT ( 'NONE',  ( -1.023622047244093558, -0.1870078740157479769, 0.3641732283464567677 ) ) ;
#5394 = CARTESIAN_POINT ( 'NONE',  ( -0.4199475065616791736, 0.2306618581243847221, -0.2411417322834647770 ) ) ;
#5395 = CARTESIAN_POINT ( 'NONE',  ( -0.2925321140481930149, -0.2925321140481933480, 0.1791338582677164948 ) ) ;
#5396 = CARTESIAN_POINT ( 'NONE',  ( -1.062992125984250968, 0.2952755905511811885, 0.000000000000000000 ) ) ;
#5397 = CARTESIAN_POINT ( 'NONE',  ( -0.1974969037888706924, 0.3420746716998658843, -2.137139107611548905 ) ) ;
#5398 = CARTESIAN_POINT ( 'NONE',  ( 1.227034120734908917, -0.5511811023622046335, 0.09757992244046803654 ) ) ;
#5399 = CARTESIAN_POINT ( 'NONE',  ( -0.3674540682414692561, -0.5023911411419708095, -0.1820866141732282451 ) ) ;
#5400 = CARTESIAN_POINT ( 'NONE',  ( 1.082677165354331228, 0.07958543189024071263, -0.2665933059059888421 ) ) ;
#5401 = CARTESIAN_POINT ( 'NONE',  ( -1.594488188976377563, -0.5400638737290844871, 0.3530559997133364547 ) ) ;
#5402 = CARTESIAN_POINT ( 'NONE',  ( -1.036745406824146176, -0.3690944881889763329, 0.3153832671262228327 ) ) ;
#5403 = CARTESIAN_POINT ( 'NONE',  ( 0.4849061582275022153, 1.726086921369708538, 0.4921425059946342717 ) ) ;
#5404 = CARTESIAN_POINT ( 'NONE',  ( 0.5446194225721792126, -0.2845877964562159024, 0.3641732283464567677 ) ) ;
#5405 = CARTESIAN_POINT ( 'NONE',  ( -0.6955380577427815458, 0.05413385826771666132, 0.4176697321401328100 ) ) ;
#5406 =( BOUNDED_SURFACE ( )  B_SPLINE_SURFACE ( 1, 2, ( 
 ( #56545, #77162, #58199, #12361, #64529, #64117, #6034, #5622, #11952, #6866, #24965, #19076, #37607, #31706, #5214, #57366, #83061, #25382, #13202, #76746, #71265, #82246, #50231, #63282, #32122, #31288, #57780, #56953, #567, #82650, #144, #25799, #32535, #51460, #51883, #19922, #45572, #13612, #50637, #76341, #70006, #65383, #14459, #7718, #40528, #72929, #52718, #40111, #39692, #64948, #46407, #47239, #1403, #71683, #59875, #60296, #21577, #14866, #46826, #53965, #53554, #27475, #34632, #8958, #15280, #33386, #40941, #66207, #21171, #72518, #59049, #66620, #2646, #8546, #20335, #15699, #28303, #78844, #72101, #53133, #59462, #2229, #47655, #34212, #27059, #78429, #79677, #992, #21994, #73351, #7288, #65798, #26647, #27894, #20757, #32958, #45987, #79262, #58625, #52301, #78007, #8132, #14035, #33797, #1813, #22413, #61538, #4691, #41752, #74180, #67447, #16941, #49308, #29135, #16527, #16108, #41356, #22821, #23638, #61117, #48070, #36275, #36677, #81324, #74598, #23226, #30365, #29949, #3883, #11021, #68679, #75009, #9781, #17356, #42582, #80913, #48896, #35452, #42984, #62353, #68283, #80093, #75416, #56032, #55205, #48479, #29543, #35872, #61947, #24049, #10618, #3469, #54802, #81740, #60705, #49720, #67037, #9369, #73772, #80506, #35040, #3054, #28720, #54383, #42171, #67866, #10203, #4287, #55613, #37506, #82547, #18973, #11853, #58095, #77058, #70744, #11439, #5928, #37095, #31600, #69504, #25694, #460, #24460, #24866, #26116, #13096, #82145, #51777, #43800, #37916, #50126, #51355, #6760, #38331, #43391, #6348, #38749, #50534, #19391, #57260, #18572, #18167, #30781, #45043, #63181, #82959, #5114, #76238, #17760, #44215, #69905, #12259, #57679, #25277, #69091, #62780, #56442, #64426, #44622, #75826, #5519, #32432, #50945, #63593, #76642, #70317, #64007, #31185, #12672, #56849, #32019, #41, #13504, #40837, #34532, #72830, #888, #39588, #59773, #2128, #66522, #39160, #65277, #52619, #15180, #26546, #45466, #13931, #58949, #78745, #71580, #60197, #53456, #47139, #71164, #65703, #64845, #8033, #45882, #27796, #2548, #52199, #1307, #28206, #8854, #58523, #77482, #20234, #14359, #77903, #79164, #19817, #14769, #7183, #66106, #32854, #26956, #21481, #33696, #78325, #7616, #33288, #20656, #46309, #59357, #72003, #40016, #1716, #27371, #53032, #21070, #34112, #46728, #72420, #40425, #8442, #4595, #3370, #73249, #42073, #79998, #49209, #34947, #67768, #74497, #36176, #10104, #61019, #3785, #16844, #29853, #60610, #74081, #17259, #54282, #29034, #22312, #29448, #61849, #41662, #54705, #28624, #53865, #35357, #4190, #73674, #2959, #48799, #74913, #10522, #55107, #35768, #42887, #42478, #16427, #23540, #81224, #55516, #47975, #68582, #80816, #61438, #23131, #16016, #10923, #68183, #36580, #67353, #62259, #79577, #21893, #47556, #15598, #41258, #9686, #66944, #9276, #80411, #22723, #48382, #13722, #12464, #18775, #65061, #30266, #70113, #32644, #6557, #70528, #70957, #20447, #7399, #65493, #76448, #50748, #19598, #44830, #674, #39799, #6138, #76848, #51153, #64638, #64223, #32229, #26750, #82752, #58309, #19181, #44418, #12883, #6975, #77269, #57887, #38126, #31813, #20025, #25906, #55930, #13302, #25487, #63800, #57473, #46100, #45676, #77695, #254, #83167, #1099, #25074, #38543, #45261, #51566, #26328, #38954, #51990, #71372, #71793, #39376, #33067, #58737, #52405, #78114, #14146, #46932, #15815, #46514, #78958, #60404, #2755, #47349, #73038, #41049, #52827, #66313, #33903, #53660, #9073, #20864, #28414, #8652, #66734, #21686, #72216, #65901, #59567, #34744, #2344, #34323, #8237, #54074, #53243, #14972, #72624, #15387, #21277, #79789, #14567, #1923, #59985, #40219, #28000, #79367, #40631, #22105, #47765, #73463, #41464, #35153, #67149, #59154, #9478, #27586, #7825, #33492, #27165, #1511, #78539, #966, #77133, #40085, #59022, #52690, #76714, #71239, #19047, #13583, #51430, #7692, #65772, #6422, #6837, #8104, #78398, #64085, #33770, #25769, #19894, #32091, #33359, #72074, #20308, #25353, #71655, #20730, #32507, #1378, #39237, #539, #114 ),
 ( #44694, #83030, #58170, #70391, #64922, #19466, #46381, #57752, #7260, #45958, #65354, #32932, #26192, #58597, #14007, #27029, #45116, #45541, #14433, #70824, #51853, #13171, #26620, #51015, #38821, #77560, #64499, #12746, #52274, #38405, #77978, #39664, #54358, #54778, #16084, #9346, #41333, #48454, #48047, #21969, #29108, #3444, #67423, #59849, #41729, #35017, #15672, #67013, #34185, #9756, #80481, #60681, #14840, #10179, #35428, #73325, #66596, #47631, #53940, #80070, #42145, #3030, #21552, #2201, #61093, #78816, #22794, #16501, #74154, #66181, #47213, #67840, #59431, #1786, #21145, #72903, #34607, #8930, #27446, #53107, #46800, #72491, #79652, #40500, #2622, #15255, #73748, #28696, #8518, #22387, #27869, #53529, #79237, #40914, #60272, #28278, #68812, #64147, #49445, #76773, #30505, #75139, #17890, #62910, #82679, #75551, #38461, #57399, #51074, #17484, #69636, #43115, #11982, #49851, #6063, #6481, #4826, #5244, #32151, #19105, #62492, #81457, #24182, #18298, #56167, #31734, #70449, #18703, #23774, #70036, #44753, #30908, #83090, #37636, #82276, #81870, #11158, #25411, #43527, #63313, #36817, #56575, #69226, #24594, #50262, #75960, #38047, #5651, #11573, #37232, #43942, #31317, #56982, #24996, #50671, #76370, #12807, #44345, #12390, #63723, #40139, #46016, #64980, #7747, #78456, #33822, #38879, #78034, #21196, #58227, #7316, #594, #33412, #65824, #45599, #32985, #32565, #57807, #39294, #8157, #77616, #64558, #52748, #53160, #14485, #59074, #39718, #46850, #46436, #20364, #27503, #1842, #59488, #26250, #78871, #1429, #14064, #65409, #51909, #72545, #14892, #27085, #13229, #8571, #40552, #58653, #66233, #71710, #173, #25827, #51486, #77189, #1020, #19521, #20781, #19949, #45174, #6895, #72127, #70880, #71293, #13641, #26673, #52328, #54833, #10234, #15307, #54412, #80943, #34662, #67065, #60325, #9810, #42200, #22023, #9397, #8989, #34241, #15728, #16556, #53995, #40970, #29164, #29574, #74210, #67476, #16137, #23258, #22850, #80123, #3913, #61570, #67896, #2674, #35901, #35482, #73801, #41783, #28333, #55237, #48928, #61146, #72956, #68312, #74628, #48102, #41384, #22442, #28750, #80538, #16972, #3498, #79707, #47683, #42612, #53579, #59903, #2255, #27920, #66652, #73378, #79288, #21606, #35068, #47266, #60734, #3086, #48510, #43017, #61980, #30396, #75451, #11886, #4722, #50976, #69937, #63626, #4317, #82178, #29982, #24494, #62385, #18605, #76674, #17386, #17789, #19006, #5963, #75040, #44655, #36710, #30810, #68711, #44248, #82991, #31218, #36304, #82579, #31633, #43424, #12293, #50161, #11470, #11052, #23668, #37949, #56062, #75857, #81356, #69121, #10649, #37127, #62811, #81771, #24898, #5145, #55645, #18199, #24081, #49340, #49751, #25312, #50567, #56886, #56475, #43834, #57293, #69536, #37538, #63214, #5554, #76271, #51388, #52235, #38782, #1750, #33323, #46342, #1340, #77938, #8069, #45077, #45501, #59392, #77093, #77517, #78360, #52654, #13968, #39625, #58985, #75, #7219, #6796, #20268, #26991, #19425, #20691, #32890, #72036, #65314, #70780, #13131, #32467, #14392, #26582, #58559, #64459, #40050, #51812, #39197, #71198, #7653, #19852, #65736, #25728, #58129, #925, #496, #45918, #71616, #13541, #64880, #33731, #27407, #53068, #21104, #78779, #64041, #70351, #26151, #12706, #38365, #6380, #32052, #57712, #35390, #10139, #35803, #3818, #60231, #54739, #53900, #16460, #22347, #80028, #29068, #27829, #34147, #80444, #46762, #2163, #48007, #21930, #2581, #2992, #61470, #22754, #80849, #8478, #66140, #34978, #28240, #16046, #55138, #21515, #8889, #66556, #73706, #79613, #47591, #42105, #14804, #41692, #34566, #59808, #73285, #67385, #9308, #15633, #53489, #9719, #41290, #79199, #67802, #72455, #40462, #60642, #47174, #61055, #72865, #28658, #15214, #29479, #3405, #48414, #74114, #54317, #40874, #66975, #81677, #12195, #4221, #30298, #31119, #5457, #50065, #75760, #69439, #36211, #43322, #42919, #56382, #37445, #29885, #56786, #69022, #11792, #18102, #55548, #49243, #68614, #63119, #62712, #11373, #74946, #82486, #4627, #75346, #23988, #43735 ) ),
 .UNSPECIFIED., .F., .F., .F. ) 
 B_SPLINE_SURFACE_WITH_KNOTS ( ( 2, 2 ),
 ( 3, 2, 2, 2, 2, 2, 2, 2, 2, 2, 2, 2, 2, 2, 2, 2, 2, 2, 2, 2, 2, 2, 2, 2, 2, 2, 2, 2, 2, 2, 2, 2, 2, 2, 2, 2, 2, 2, 2, 2, 2, 2, 2, 2, 2, 2, 2, 2, 2, 2, 2, 2, 2, 2, 2, 2, 2, 2, 2, 2, 2, 2, 2, 2, 2, 2, 2, 2, 2, 2, 2, 2, 2, 2, 2, 2, 2, 2, 2, 2, 2, 2, 2, 2, 2, 2, 2, 2, 2, 2, 2, 2, 2, 2, 2, 2, 2, 2, 2, 2, 2, 2, 2, 2, 2, 2, 2, 2, 2, 2, 2, 2, 2, 2, 2, 2, 2, 2, 2, 2, 2, 2, 2, 2, 2, 2, 2, 2, 2, 2, 2, 2, 2, 2, 2, 2, 2, 2, 2, 2, 2, 2, 2, 2, 2, 2, 2, 2, 2, 2, 2, 2, 2, 2, 2, 2, 2, 2, 2, 2, 2, 2, 2, 2, 2, 2, 2, 2, 2, 2, 2, 2, 2, 2, 2, 2, 2, 2, 2, 2, 2, 2, 2, 2, 2, 2, 2, 2, 2, 2, 2, 2, 2, 2, 2, 2, 2, 2, 2, 2, 2, 2, 2, 2, 2, 2, 2, 2, 2, 2, 2, 2, 2, 2, 2, 2, 2, 2, 2, 2, 2, 2, 2, 2, 2, 2, 2, 2, 2, 2, 2, 2, 2, 2, 2, 2, 2, 2, 2, 2, 2, 2, 2, 2, 2, 2, 2, 2, 2, 2, 2, 2, 2, 2, 2, 3 ),
 ( 0.000000000000000000, 1.000000000000000000 ),
 ( 0.000000000000000000, 0.003787878787878787984, 0.007575757575757575968, 0.01136363636363636395, 0.01515151515151515194, 0.01893939393939393992, 0.02272727272727272790, 0.02651515151515151589, 0.03030303030303030387, 0.03409090909090908839, 0.03787878787878787984, 0.04166666666666666435, 0.04545454545454545581, 0.04924242424242424032, 0.05303030303030303177, 0.05681818181818181629, 0.06060606060606060774, 0.06439393939393939226, 0.06818181818181817677, 0.07196969696969697516, 0.07575757575757575968, 0.07954545454545454419, 0.08333333333333332871, 0.08712121212121212710, 0.09090909090909091161, 0.09469696969696969613, 0.09848484848484848064, 0.1022727272727272790, 0.1060606060606060635, 0.1098484848484848481, 0.1136363636363636326, 0.1174242424242424310, 0.1212121212121212155, 0.1250000000000000000, 0.1287878787878787845, 0.1325757575757575690, 0.1363636363636363535, 0.1401515151515151381, 0.1439393939393939503, 0.1477272727272727348, 0.1515151515151515194, 0.1553030303030303039, 0.1590909090909090884, 0.1628787878787878729, 0.1666666666666666574, 0.1704545454545454419, 0.1742424242424242542, 0.1780303030303030387, 0.1818181818181818232, 0.1856060606060606077, 0.1893939393939393923, 0.1931818181818181768, 0.1969696969696969613, 0.2007575757575757458, 0.2045454545454545581, 0.2083333333333333426, 0.2121212121212121271, 0.2159090909090909116, 0.2196969696969696961, 0.2234848484848484806, 0.2272727272727272652, 0.2310606060606060497, 0.2348484848484848619, 0.2386363636363636465, 0.2424242424242424310, 0.2462121212121212155, 0.2500000000000000000, 0.2537878787878787845, 0.2575757575757575690, 0.2613636363636363535, 0.2651515151515151381, 0.2689393939393939226, 0.2727272727272727071, 0.2765151515151514916, 0.2803030303030302761, 0.2840909090909091161, 0.2878787878787879007, 0.2916666666666666852, 0.2954545454545454697, 0.2992424242424242542, 0.3030303030303030387, 0.3068181818181818232, 0.3106060606060606077, 0.3143939393939393923, 0.3181818181818181768, 0.3219696969696969613, 0.3257575757575757458, 0.3295454545454545303, 0.3333333333333333148, 0.3371212121212120993, 0.3409090909090908839, 0.3446969696969697239, 0.3484848484848485084, 0.3522727272727272929, 0.3560606060606060774, 0.3598484848484848619, 0.3636363636363636465, 0.3674242424242424310, 0.3712121212121212155, 0.3750000000000000000, 0.3787878787878787845, 0.3825757575757575690, 0.3863636363636363535, 0.3901515151515151381, 0.3939393939393939226, 0.3977272727272727071, 0.4015151515151514916, 0.4053030303030302761, 0.4090909090909091161, 0.4128787878787879007, 0.4166666666666666852, 0.4204545454545454697, 0.4242424242424242542, 0.4280303030303030387, 0.4318181818181818232, 0.4356060606060606077, 0.4393939393939393923, 0.4431818181818181768, 0.4469696969696969613, 0.4507575757575757458, 0.4545454545454545303, 0.4583333333333333148, 0.4621212121212120993, 0.4659090909090908839, 0.4696969696969697239, 0.4734848484848485084, 0.4772727272727272929, 0.4810606060606060774, 0.4848484848484848619, 0.4886363636363636465, 0.4924242424242424310, 0.4962121212121212155, 0.5000000000000000000, 0.5037878787878787845, 0.5075757575757575690, 0.5113636363636363535, 0.5151515151515151381, 0.5189393939393939226, 0.5227272727272727071, 0.5265151515151514916, 0.5303030303030302761, 0.5340909090909090606, 0.5378787878787878451, 0.5416666666666666297, 0.5454545454545454142, 0.5492424242424241987, 0.5530303030303029832, 0.5568181818181817677, 0.5606060606060605522, 0.5643939393939394478, 0.5681818181818182323, 0.5719696969696970168, 0.5757575757575758013, 0.5795454545454545858, 0.5833333333333333703, 0.5871212121212121549, 0.5909090909090909394, 0.5946969696969697239, 0.5984848484848485084, 0.6022727272727272929, 0.6060606060606060774, 0.6098484848484848619, 0.6136363636363636465, 0.6174242424242424310, 0.6212121212121212155, 0.6250000000000000000, 0.6287878787878787845, 0.6325757575757575690, 0.6363636363636363535, 0.6401515151515151381, 0.6439393939393939226, 0.6477272727272727071, 0.6515151515151514916, 0.6553030303030302761, 0.6590909090909090606, 0.6628787878787878451, 0.6666666666666666297, 0.6704545454545454142, 0.6742424242424241987, 0.6780303030303029832, 0.6818181818181817677, 0.6856060606060605522, 0.6893939393939394478, 0.6931818181818182323, 0.6969696969696970168, 0.7007575757575758013, 0.7045454545454545858, 0.7083333333333333703, 0.7121212121212121549, 0.7159090909090909394, 0.7196969696969697239, 0.7234848484848485084, 0.7272727272727272929, 0.7310606060606060774, 0.7348484848484848619, 0.7386363636363636465, 0.7424242424242424310, 0.7462121212121212155, 0.7500000000000000000, 0.7537878787878787845, 0.7575757575757575690, 0.7613636363636363535, 0.7651515151515151381, 0.7689393939393939226, 0.7727272727272727071, 0.7765151515151514916, 0.7803030303030302761, 0.7840909090909090606, 0.7878787878787878451, 0.7916666666666666297, 0.7954545454545454142, 0.7992424242424241987, 0.8030303030303029832, 0.8068181818181817677, 0.8106060606060605522, 0.8143939393939394478, 0.8181818181818182323, 0.8219696969696970168, 0.8257575757575758013, 0.8295454545454545858, 0.8333333333333333703, 0.8371212121212121549, 0.8409090909090909394, 0.8446969696969697239, 0.8484848484848485084, 0.8522727272727272929, 0.8560606060606060774, 0.8598484848484848619, 0.8636363636363636465, 0.8674242424242424310, 0.8712121212121212155, 0.8750000000000000000, 0.8787878787878787845, 0.8825757575757575690, 0.8863636363636363535, 0.8901515151515151381, 0.8939393939393939226, 0.8977272727272727071, 0.9015151515151514916, 0.9053030303030302761, 0.9090909090909090606, 0.9128787878787878451, 0.9166666666666666297, 0.9204545454545454142, 0.9242424242424241987, 0.9280303030303029832, 0.9318181818181817677, 0.9356060606060605522, 0.9393939393939394478, 0.9431818181818182323, 0.9469696969696970168, 0.9507575757575758013, 0.9545454545454545858, 0.9583333333333333703, 0.9621212121212121549, 0.9659090909090909394 ),
 .UNSPECIFIED. ) 
 GEOMETRIC_REPRESENTATION_ITEM ( )  RATIONAL_B_SPLINE_SURFACE ( (
 ( 1.000000000000000000, 0.9659258262890683122, 1.000000000000000000, 0.9659258262890683122, 1.000000000000000000, 0.9659258262890683122, 1.000000000000000000, 0.9659258262890683122, 1.000000000000000000, 0.9659258262890683122, 1.000000000000000000, 0.9659258262890683122, 1.000000000000000000, 0.9659258262890683122, 1.000000000000000000, 0.9659258262890683122, 1.000000000000000000, 0.9659258262890683122, 1.000000000000000000, 0.9659258262890683122, 1.000000000000000000, 0.9659258262890683122, 1.000000000000000000, 0.9659258262890683122, 1.000000000000000000, 0.9659258262890683122, 1.000000000000000000, 0.9659258262890683122, 1.000000000000000000, 0.9659258262890683122, 1.000000000000000000, 0.9659258262890683122, 1.000000000000000000, 0.9659258262890683122, 1.000000000000000000, 0.9659258262890683122, 1.000000000000000000, 0.9659258262890683122, 1.000000000000000000, 0.9659258262890683122, 1.000000000000000000, 0.9659258262890683122, 1.000000000000000000, 0.9659258262890683122, 1.000000000000000000, 0.9659258262890683122, 1.000000000000000000, 0.9659258262890683122, 1.000000000000000000, 0.9659258262890683122, 1.000000000000000000, 0.9659258262890683122, 1.000000000000000000, 0.9659258262890683122, 1.000000000000000000, 0.9659258262890683122, 1.000000000000000000, 0.9659258262890683122, 1.000000000000000000, 0.9659258262890683122, 1.000000000000000000, 0.9659258262890683122, 1.000000000000000000, 0.9659258262890683122, 1.000000000000000000, 0.9659258262890683122, 1.000000000000000000, 0.9659258262890683122, 1.000000000000000000, 0.9659258262890683122, 1.000000000000000000, 0.9659258262890683122, 1.000000000000000000, 0.9659258262890683122, 1.000000000000000000, 0.9659258262890683122, 1.000000000000000000, 0.9659258262890683122, 1.000000000000000000, 0.9659258262890683122, 1.000000000000000000, 0.9659258262890683122, 1.000000000000000000, 0.9659258262890683122, 1.000000000000000000, 0.9659258262890683122, 1.000000000000000000, 0.9659258262890683122, 1.000000000000000000, 0.9659258262890683122, 1.000000000000000000, 0.9659258262890683122, 1.000000000000000000, 0.9659258262890683122, 1.000000000000000000, 0.9659258262890683122, 1.000000000000000000, 0.9659258262890683122, 1.000000000000000000, 0.9659258262890683122, 1.000000000000000000, 0.9659258262890683122, 1.000000000000000000, 0.9659258262890683122, 1.000000000000000000, 0.9659258262890683122, 1.000000000000000000, 0.9659258262890683122, 1.000000000000000000, 0.9659258262890683122, 1.000000000000000000, 0.9659258262890683122, 1.000000000000000000, 0.9659258262890683122, 1.000000000000000000, 0.9659258262890683122, 1.000000000000000000, 0.9659258262890683122, 1.000000000000000000, 0.9659258262890683122, 1.000000000000000000, 0.9659258262890683122, 1.000000000000000000, 0.9659258262890683122, 1.000000000000000000, 0.9659258262890683122, 1.000000000000000000, 0.9659258262890683122, 1.000000000000000000, 0.9659258262890683122, 1.000000000000000000, 0.9659258262890683122, 1.000000000000000000, 0.9659258262890683122, 1.000000000000000000, 0.9659258262890683122, 1.000000000000000000, 0.9659258262890683122, 1.000000000000000000, 0.9659258262890683122, 1.000000000000000000, 0.9659258262890683122, 1.000000000000000000, 0.9659258262890683122, 1.000000000000000000, 0.9659258262890683122, 1.000000000000000000, 0.9659258262890683122, 1.000000000000000000, 0.9659258262890683122, 1.000000000000000000, 0.9659258262890683122, 1.000000000000000000, 0.9659258262890683122, 1.000000000000000000, 0.9659258262890683122, 1.000000000000000000, 0.9659258262890683122, 1.000000000000000000, 0.9659258262890683122, 1.000000000000000000, 0.9659258262890683122, 1.000000000000000000, 0.9659258262890683122, 1.000000000000000000, 0.9659258262890683122, 1.000000000000000000, 0.9659258262890683122, 1.000000000000000000, 0.9659258262890683122, 1.000000000000000000, 0.9659258262890683122, 1.000000000000000000, 0.9659258262890683122, 1.000000000000000000, 0.9659258262890683122, 1.000000000000000000, 0.9659258262890683122, 1.000000000000000000, 0.9659258262890683122, 1.000000000000000000, 0.9659258262890683122, 1.000000000000000000, 0.9659258262890683122, 1.000000000000000000, 0.9659258262890683122, 1.000000000000000000, 0.9659258262890683122, 1.000000000000000000, 0.9659258262890683122, 1.000000000000000000, 0.9659258262890683122, 1.000000000000000000, 0.9659258262890683122, 1.000000000000000000, 0.9659258262890683122, 1.000000000000000000, 0.9659258262890683122, 1.000000000000000000, 0.9659258262890683122, 1.000000000000000000, 0.9659258262890683122, 1.000000000000000000, 0.9659258262890683122, 1.000000000000000000, 0.9659258262890683122, 1.000000000000000000, 0.9659258262890683122, 1.000000000000000000, 0.9659258262890683122, 1.000000000000000000, 0.9659258262890683122, 1.000000000000000000, 0.9659258262890683122, 1.000000000000000000, 0.9659258262890683122, 1.000000000000000000, 0.9659258262890683122, 1.000000000000000000, 0.9659258262890683122, 1.000000000000000000, 0.9659258262890683122, 1.000000000000000000, 0.9659258262890683122, 1.000000000000000000, 0.9659258262890683122, 1.000000000000000000, 0.9659258262890683122, 1.000000000000000000, 0.9659258262890683122, 1.000000000000000000, 0.9659258262890683122, 1.000000000000000000, 0.9659258262890683122, 1.000000000000000000, 0.9659258262890683122, 1.000000000000000000, 0.9659258262890683122, 1.000000000000000000, 0.9659258262890683122, 1.000000000000000000, 0.9659258262890683122, 1.000000000000000000, 0.9659258262890683122, 1.000000000000000000, 0.9659258262890683122, 1.000000000000000000, 0.9659258262890683122, 1.000000000000000000, 0.9659258262890683122, 1.000000000000000000, 0.9659258262890683122, 1.000000000000000000, 0.9659258262890683122, 1.000000000000000000, 0.9659258262890683122, 1.000000000000000000, 0.9659258262890683122, 1.000000000000000000, 0.9659258262890683122, 1.000000000000000000, 0.9659258262890683122, 1.000000000000000000, 0.9659258262890683122, 1.000000000000000000, 0.9659258262890683122, 1.000000000000000000, 0.9659258262890683122, 1.000000000000000000, 0.9659258262890683122, 1.000000000000000000, 0.9659258262890683122, 1.000000000000000000, 0.9659258262890683122, 1.000000000000000000, 0.9659258262890683122, 1.000000000000000000, 0.9659258262890683122, 1.000000000000000000, 0.9659258262890683122, 1.000000000000000000, 0.9659258262890683122, 1.000000000000000000, 0.9659258262890683122, 1.000000000000000000, 0.9659258262890683122, 1.000000000000000000, 0.9659258262890683122, 1.000000000000000000, 0.9659258262890683122, 1.000000000000000000, 0.9659258262890683122, 1.000000000000000000, 0.9659258262890683122, 1.000000000000000000, 0.9659258262890683122, 1.000000000000000000, 0.9659258262890683122, 1.000000000000000000, 0.9659258262890683122, 1.000000000000000000, 0.9659258262890683122, 1.000000000000000000, 0.9659258262890683122, 1.000000000000000000, 0.9659258262890683122, 1.000000000000000000, 0.9659258262890683122, 1.000000000000000000, 0.9659258262890683122, 1.000000000000000000, 0.9659258262890683122, 1.000000000000000000, 0.9659258262890683122, 1.000000000000000000, 0.9659258262890683122, 1.000000000000000000, 0.9659258262890683122, 1.000000000000000000, 0.9659258262890683122, 1.000000000000000000, 0.9659258262890683122, 1.000000000000000000, 0.9659258262890683122, 1.000000000000000000, 0.9659258262890683122, 1.000000000000000000, 0.9659258262890683122, 1.000000000000000000, 0.9659258262890683122, 1.000000000000000000, 0.9659258262890683122, 1.000000000000000000, 0.9659258262890683122, 1.000000000000000000, 0.9659258262890683122, 1.000000000000000000, 0.9659258262890683122, 1.000000000000000000, 0.9659258262890683122, 1.000000000000000000, 0.9659258262890683122, 1.000000000000000000, 0.9659258262890683122, 1.000000000000000000, 0.9659258262890683122, 1.000000000000000000, 0.9659258262890683122, 1.000000000000000000, 0.9659258262890683122, 1.000000000000000000, 0.9659258262890683122, 1.000000000000000000, 0.9659258262890683122, 1.000000000000000000, 0.9659258262890683122, 1.000000000000000000, 0.9659258262890683122, 1.000000000000000000, 0.9659258262890683122, 1.000000000000000000, 0.9659258262890683122, 1.000000000000000000, 0.9659258262890683122, 1.000000000000000000, 0.9659258262890683122, 1.000000000000000000, 0.9659258262890683122, 1.000000000000000000, 0.9659258262890683122, 1.000000000000000000, 0.9659258262890683122, 1.000000000000000000, 0.9659258262890683122, 1.000000000000000000, 0.9659258262890683122, 1.000000000000000000, 0.9659258262890683122, 1.000000000000000000, 0.9659258262890683122, 1.000000000000000000, 0.9659258262890683122, 1.000000000000000000, 0.9659258262890683122, 1.000000000000000000, 0.9659258262890683122, 1.000000000000000000, 0.9659258262890683122, 1.000000000000000000, 0.9659258262890683122, 1.000000000000000000, 0.9659258262890683122, 1.000000000000000000, 0.9659258262890683122, 1.000000000000000000, 0.9659258262890683122, 1.000000000000000000, 0.9659258262890683122, 1.000000000000000000, 0.9659258262890683122, 1.000000000000000000, 0.9659258262890683122, 1.000000000000000000, 0.9659258262890683122, 1.000000000000000000, 0.9659258262890683122, 1.000000000000000000, 0.9659258262890683122, 1.000000000000000000, 0.9659258262890683122, 1.000000000000000000, 0.9659258262890683122, 1.000000000000000000, 0.9659258262890683122, 1.000000000000000000, 0.9659258262890683122, 1.000000000000000000, 0.9659258262890683122, 1.000000000000000000, 0.9659258262890683122, 1.000000000000000000, 0.9659258262890683122, 1.000000000000000000, 0.9659258262890683122, 1.000000000000000000, 0.9659258262890683122, 1.000000000000000000, 0.9659258262890683122, 1.000000000000000000, 0.9659258262890683122, 1.000000000000000000, 0.9659258262890683122, 1.000000000000000000, 0.9659258262890683122, 1.000000000000000000, 0.9659258262890683122, 1.000000000000000000, 0.9659258262890683122, 1.000000000000000000, 0.9659258262890683122, 1.000000000000000000, 0.9659258262890683122, 1.000000000000000000, 0.9659258262890683122, 1.000000000000000000, 0.9659258262890683122, 1.000000000000000000, 0.9659258262890683122, 1.000000000000000000, 0.9659258262890683122, 1.000000000000000000, 0.9659258262890683122, 1.000000000000000000, 0.9659258262890683122, 1.000000000000000000, 0.9659258262890683122, 1.000000000000000000, 0.9659258262890683122, 1.000000000000000000, 0.9659258262890683122, 1.000000000000000000, 0.9659258262890683122, 1.000000000000000000, 0.9659258262890683122, 1.000000000000000000, 0.9659258262890683122, 1.000000000000000000, 0.9659258262890683122, 1.000000000000000000, 0.9659258262890683122, 1.000000000000000000, 0.9659258262890683122, 1.000000000000000000, 0.9659258262890683122, 1.000000000000000000, 0.9659258262890683122, 1.000000000000000000, 0.9659258262890683122, 1.000000000000000000, 0.9659258262890683122, 1.000000000000000000, 0.9659258262890683122, 1.000000000000000000, 0.9659258262890683122, 1.000000000000000000, 0.9659258262890683122, 1.000000000000000000, 0.9659258262890683122, 1.000000000000000000, 0.9659258262890683122, 1.000000000000000000, 0.9659258262890683122, 1.000000000000000000, 0.9659258262890683122, 1.000000000000000000, 0.9659258262890683122, 1.000000000000000000, 0.9659258262890683122, 1.000000000000000000, 0.9659258262890683122, 1.000000000000000000, 0.9659258262890683122, 1.000000000000000000, 0.9659258262890683122, 1.000000000000000000, 0.9659258262890683122, 1.000000000000000000, 0.9659258262890683122, 1.000000000000000000, 0.9659258262890683122, 1.000000000000000000),
 ( 1.000000000000000000, 0.9659258262890683122, 1.000000000000000000, 0.9659258262890683122, 1.000000000000000000, 0.9659258262890683122, 1.000000000000000000, 0.9659258262890683122, 1.000000000000000000, 0.9659258262890683122, 1.000000000000000000, 0.9659258262890683122, 1.000000000000000000, 0.9659258262890683122, 1.000000000000000000, 0.9659258262890683122, 1.000000000000000000, 0.9659258262890683122, 1.000000000000000000, 0.9659258262890683122, 1.000000000000000000, 0.9659258262890683122, 1.000000000000000000, 0.9659258262890683122, 1.000000000000000000, 0.9659258262890683122, 1.000000000000000000, 0.9659258262890683122, 1.000000000000000000, 0.9659258262890683122, 1.000000000000000000, 0.9659258262890683122, 1.000000000000000000, 0.9659258262890683122, 1.000000000000000000, 0.9659258262890683122, 1.000000000000000000, 0.9659258262890683122, 1.000000000000000000, 0.9659258262890683122, 1.000000000000000000, 0.9659258262890683122, 1.000000000000000000, 0.9659258262890683122, 1.000000000000000000, 0.9659258262890683122, 1.000000000000000000, 0.9659258262890683122, 1.000000000000000000, 0.9659258262890683122, 1.000000000000000000, 0.9659258262890683122, 1.000000000000000000, 0.9659258262890683122, 1.000000000000000000, 0.9659258262890683122, 1.000000000000000000, 0.9659258262890683122, 1.000000000000000000, 0.9659258262890683122, 1.000000000000000000, 0.9659258262890683122, 1.000000000000000000, 0.9659258262890683122, 1.000000000000000000, 0.9659258262890683122, 1.000000000000000000, 0.9659258262890683122, 1.000000000000000000, 0.9659258262890683122, 1.000000000000000000, 0.9659258262890683122, 1.000000000000000000, 0.9659258262890683122, 1.000000000000000000, 0.9659258262890683122, 1.000000000000000000, 0.9659258262890683122, 1.000000000000000000, 0.9659258262890683122, 1.000000000000000000, 0.9659258262890683122, 1.000000000000000000, 0.9659258262890683122, 1.000000000000000000, 0.9659258262890683122, 1.000000000000000000, 0.9659258262890683122, 1.000000000000000000, 0.9659258262890683122, 1.000000000000000000, 0.9659258262890683122, 1.000000000000000000, 0.9659258262890683122, 1.000000000000000000, 0.9659258262890683122, 1.000000000000000000, 0.9659258262890683122, 1.000000000000000000, 0.9659258262890683122, 1.000000000000000000, 0.9659258262890683122, 1.000000000000000000, 0.9659258262890683122, 1.000000000000000000, 0.9659258262890683122, 1.000000000000000000, 0.9659258262890683122, 1.000000000000000000, 0.9659258262890683122, 1.000000000000000000, 0.9659258262890683122, 1.000000000000000000, 0.9659258262890683122, 1.000000000000000000, 0.9659258262890683122, 1.000000000000000000, 0.9659258262890683122, 1.000000000000000000, 0.9659258262890683122, 1.000000000000000000, 0.9659258262890683122, 1.000000000000000000, 0.9659258262890683122, 1.000000000000000000, 0.9659258262890683122, 1.000000000000000000, 0.9659258262890683122, 1.000000000000000000, 0.9659258262890683122, 1.000000000000000000, 0.9659258262890683122, 1.000000000000000000, 0.9659258262890683122, 1.000000000000000000, 0.9659258262890683122, 1.000000000000000000, 0.9659258262890683122, 1.000000000000000000, 0.9659258262890683122, 1.000000000000000000, 0.9659258262890683122, 1.000000000000000000, 0.9659258262890683122, 1.000000000000000000, 0.9659258262890683122, 1.000000000000000000, 0.9659258262890683122, 1.000000000000000000, 0.9659258262890683122, 1.000000000000000000, 0.9659258262890683122, 1.000000000000000000, 0.9659258262890683122, 1.000000000000000000, 0.9659258262890683122, 1.000000000000000000, 0.9659258262890683122, 1.000000000000000000, 0.9659258262890683122, 1.000000000000000000, 0.9659258262890683122, 1.000000000000000000, 0.9659258262890683122, 1.000000000000000000, 0.9659258262890683122, 1.000000000000000000, 0.9659258262890683122, 1.000000000000000000, 0.9659258262890683122, 1.000000000000000000, 0.9659258262890683122, 1.000000000000000000, 0.9659258262890683122, 1.000000000000000000, 0.9659258262890683122, 1.000000000000000000, 0.9659258262890683122, 1.000000000000000000, 0.9659258262890683122, 1.000000000000000000, 0.9659258262890683122, 1.000000000000000000, 0.9659258262890683122, 1.000000000000000000, 0.9659258262890683122, 1.000000000000000000, 0.9659258262890683122, 1.000000000000000000, 0.9659258262890683122, 1.000000000000000000, 0.9659258262890683122, 1.000000000000000000, 0.9659258262890683122, 1.000000000000000000, 0.9659258262890683122, 1.000000000000000000, 0.9659258262890683122, 1.000000000000000000, 0.9659258262890683122, 1.000000000000000000, 0.9659258262890683122, 1.000000000000000000, 0.9659258262890683122, 1.000000000000000000, 0.9659258262890683122, 1.000000000000000000, 0.9659258262890683122, 1.000000000000000000, 0.9659258262890683122, 1.000000000000000000, 0.9659258262890683122, 1.000000000000000000, 0.9659258262890683122, 1.000000000000000000, 0.9659258262890683122, 1.000000000000000000, 0.9659258262890683122, 1.000000000000000000, 0.9659258262890683122, 1.000000000000000000, 0.9659258262890683122, 1.000000000000000000, 0.9659258262890683122, 1.000000000000000000, 0.9659258262890683122, 1.000000000000000000, 0.9659258262890683122, 1.000000000000000000, 0.9659258262890683122, 1.000000000000000000, 0.9659258262890683122, 1.000000000000000000, 0.9659258262890683122, 1.000000000000000000, 0.9659258262890683122, 1.000000000000000000, 0.9659258262890683122, 1.000000000000000000, 0.9659258262890683122, 1.000000000000000000, 0.9659258262890683122, 1.000000000000000000, 0.9659258262890683122, 1.000000000000000000, 0.9659258262890683122, 1.000000000000000000, 0.9659258262890683122, 1.000000000000000000, 0.9659258262890683122, 1.000000000000000000, 0.9659258262890683122, 1.000000000000000000, 0.9659258262890683122, 1.000000000000000000, 0.9659258262890683122, 1.000000000000000000, 0.9659258262890683122, 1.000000000000000000, 0.9659258262890683122, 1.000000000000000000, 0.9659258262890683122, 1.000000000000000000, 0.9659258262890683122, 1.000000000000000000, 0.9659258262890683122, 1.000000000000000000, 0.9659258262890683122, 1.000000000000000000, 0.9659258262890683122, 1.000000000000000000, 0.9659258262890683122, 1.000000000000000000, 0.9659258262890683122, 1.000000000000000000, 0.9659258262890683122, 1.000000000000000000, 0.9659258262890683122, 1.000000000000000000, 0.9659258262890683122, 1.000000000000000000, 0.9659258262890683122, 1.000000000000000000, 0.9659258262890683122, 1.000000000000000000, 0.9659258262890683122, 1.000000000000000000, 0.9659258262890683122, 1.000000000000000000, 0.9659258262890683122, 1.000000000000000000, 0.9659258262890683122, 1.000000000000000000, 0.9659258262890683122, 1.000000000000000000, 0.9659258262890683122, 1.000000000000000000, 0.9659258262890683122, 1.000000000000000000, 0.9659258262890683122, 1.000000000000000000, 0.9659258262890683122, 1.000000000000000000, 0.9659258262890683122, 1.000000000000000000, 0.9659258262890683122, 1.000000000000000000, 0.9659258262890683122, 1.000000000000000000, 0.9659258262890683122, 1.000000000000000000, 0.9659258262890683122, 1.000000000000000000, 0.9659258262890683122, 1.000000000000000000, 0.9659258262890683122, 1.000000000000000000, 0.9659258262890683122, 1.000000000000000000, 0.9659258262890683122, 1.000000000000000000, 0.9659258262890683122, 1.000000000000000000, 0.9659258262890683122, 1.000000000000000000, 0.9659258262890683122, 1.000000000000000000, 0.9659258262890683122, 1.000000000000000000, 0.9659258262890683122, 1.000000000000000000, 0.9659258262890683122, 1.000000000000000000, 0.9659258262890683122, 1.000000000000000000, 0.9659258262890683122, 1.000000000000000000, 0.9659258262890683122, 1.000000000000000000, 0.9659258262890683122, 1.000000000000000000, 0.9659258262890683122, 1.000000000000000000, 0.9659258262890683122, 1.000000000000000000, 0.9659258262890683122, 1.000000000000000000, 0.9659258262890683122, 1.000000000000000000, 0.9659258262890683122, 1.000000000000000000, 0.9659258262890683122, 1.000000000000000000, 0.9659258262890683122, 1.000000000000000000, 0.9659258262890683122, 1.000000000000000000, 0.9659258262890683122, 1.000000000000000000, 0.9659258262890683122, 1.000000000000000000, 0.9659258262890683122, 1.000000000000000000, 0.9659258262890683122, 1.000000000000000000, 0.9659258262890683122, 1.000000000000000000, 0.9659258262890683122, 1.000000000000000000, 0.9659258262890683122, 1.000000000000000000, 0.9659258262890683122, 1.000000000000000000, 0.9659258262890683122, 1.000000000000000000, 0.9659258262890683122, 1.000000000000000000, 0.9659258262890683122, 1.000000000000000000, 0.9659258262890683122, 1.000000000000000000, 0.9659258262890683122, 1.000000000000000000, 0.9659258262890683122, 1.000000000000000000, 0.9659258262890683122, 1.000000000000000000, 0.9659258262890683122, 1.000000000000000000, 0.9659258262890683122, 1.000000000000000000, 0.9659258262890683122, 1.000000000000000000, 0.9659258262890683122, 1.000000000000000000, 0.9659258262890683122, 1.000000000000000000, 0.9659258262890683122, 1.000000000000000000, 0.9659258262890683122, 1.000000000000000000, 0.9659258262890683122, 1.000000000000000000, 0.9659258262890683122, 1.000000000000000000, 0.9659258262890683122, 1.000000000000000000, 0.9659258262890683122, 1.000000000000000000, 0.9659258262890683122, 1.000000000000000000, 0.9659258262890683122, 1.000000000000000000, 0.9659258262890683122, 1.000000000000000000, 0.9659258262890683122, 1.000000000000000000, 0.9659258262890683122, 1.000000000000000000, 0.9659258262890683122, 1.000000000000000000, 0.9659258262890683122, 1.000000000000000000, 0.9659258262890683122, 1.000000000000000000, 0.9659258262890683122, 1.000000000000000000, 0.9659258262890683122, 1.000000000000000000, 0.9659258262890683122, 1.000000000000000000, 0.9659258262890683122, 1.000000000000000000, 0.9659258262890683122, 1.000000000000000000, 0.9659258262890683122, 1.000000000000000000, 0.9659258262890683122, 1.000000000000000000, 0.9659258262890683122, 1.000000000000000000, 0.9659258262890683122, 1.000000000000000000, 0.9659258262890683122, 1.000000000000000000, 0.9659258262890683122, 1.000000000000000000, 0.9659258262890683122, 1.000000000000000000, 0.9659258262890683122, 1.000000000000000000, 0.9659258262890683122, 1.000000000000000000, 0.9659258262890683122, 1.000000000000000000, 0.9659258262890683122, 1.000000000000000000, 0.9659258262890683122, 1.000000000000000000, 0.9659258262890683122, 1.000000000000000000, 0.9659258262890683122, 1.000000000000000000, 0.9659258262890683122, 1.000000000000000000, 0.9659258262890683122, 1.000000000000000000, 0.9659258262890683122, 1.000000000000000000, 0.9659258262890683122, 1.000000000000000000, 0.9659258262890683122, 1.000000000000000000, 0.9659258262890683122, 1.000000000000000000, 0.9659258262890683122, 1.000000000000000000, 0.9659258262890683122, 1.000000000000000000, 0.9659258262890683122, 1.000000000000000000, 0.9659258262890683122, 1.000000000000000000, 0.9659258262890683122, 1.000000000000000000, 0.9659258262890683122, 1.000000000000000000, 0.9659258262890683122, 1.000000000000000000, 0.9659258262890683122, 1.000000000000000000, 0.9659258262890683122, 1.000000000000000000, 0.9659258262890683122, 1.000000000000000000, 0.9659258262890683122, 1.000000000000000000, 0.9659258262890683122, 1.000000000000000000, 0.9659258262890683122, 1.000000000000000000, 0.9659258262890683122, 1.000000000000000000, 0.9659258262890683122, 1.000000000000000000, 0.9659258262890683122, 1.000000000000000000, 0.9659258262890683122, 1.000000000000000000, 0.9659258262890683122, 1.000000000000000000) ) ) 
 REPRESENTATION_ITEM ( '' )  SURFACE ( )  );
#5407 = CARTESIAN_POINT ( 'NONE',  ( 0.5314960629920991719, 2.729656616209943376, 2.556891461833393553 ) ) ;
#5408 = CARTESIAN_POINT ( 'NONE',  ( -0.1312335958005241554, -0.5023911411419708095, -0.1820866141732282451 ) ) ;
#5409 = CARTESIAN_POINT ( 'NONE',  ( -1.574803149606298636, -0.1870078740157479769, 0.3641732283464567677 ) ) ;
#5410 = CARTESIAN_POINT ( 'NONE',  ( 0.6299212598425204535, -0.1870078740157480879, -0.4822834645669291653 ) ) ;
#5411 = CARTESIAN_POINT ( 'NONE',  ( 0.000000000000000000, 0.000000000000000000, -2.755905511811024056 ) ) ;
#5412 = CARTESIAN_POINT ( 'NONE',  ( 1.417322834645670104, -0.1870078740157479769, 0.3641732283464567677 ) ) ;
#5413 = MECHANICAL_DESIGN_GEOMETRIC_PRESENTATION_REPRESENTATION (  '', ( #56467 ), #14986 ) ;
#5414 = CARTESIAN_POINT ( 'NONE',  ( -0.9580052493438311334, -0.4281496062992124485, 0.4176697321401328655 ) ) ;
#5415 = CARTESIAN_POINT ( 'NONE',  ( -0.3937007874015740483, -0.1870078740157479769, 0.3641732283464567677 ) ) ;
#5416 = FACE_OUTER_BOUND ( 'NONE', #31024, .T. ) ;
#5417 = CARTESIAN_POINT ( 'NONE',  ( 0.3083989501312343062, -0.2845877964562159024, 0.3641732283464567677 ) ) ;
#5418 = CARTESIAN_POINT ( 'NONE',  ( -1.220472440944881054, 0.2952755905511811885, 0.000000000000000000 ) ) ;
#5419 = CARTESIAN_POINT ( 'NONE',  ( -0.4330708661417315697, -0.6692913385826771977, 8.415575281601705876E-17 ) ) ;
#5420 = CARTESIAN_POINT ( 'NONE',  ( 0.3460692066303958092, 0.1998031496062993018, -0.8379265091863516979 ) ) ;
#5421 = CARTESIAN_POINT ( 'NONE',  ( -0.3392501089628017219, -0.1958661417322836718, -2.184383202099737797 ) ) ;
#5422 = CARTESIAN_POINT ( 'NONE',  ( 0.6364829396325465405, -0.08942795157527998196, 0.3641732283464567121 ) ) ;
#5423 = CARTESIAN_POINT ( 'NONE',  ( -0.4724409448818890911, -0.1870078740157480879, -0.4822834645669291653 ) ) ;
#5424 = CARTESIAN_POINT ( 'NONE',  ( -0.8267716535433065062, 0.2952755905511811885, 0.000000000000000000 ) ) ;
#5425 = CARTESIAN_POINT ( 'NONE',  ( -1.003937007874014853, 0.07958543189024085140, 0.2665933059059887866 ) ) ;
#5426 = CARTESIAN_POINT ( 'NONE',  ( 1.150409065943327258, 0.000000000000000000, 0.8265612839971842041 ) ) ;
#5427 = CARTESIAN_POINT ( 'NONE',  ( -0.2165354330708654795, 0.1660481256975885056, 0.3530559997133364547 ) ) ;
#5428 = ADVANCED_FACE ( 'NONE', ( #34125 ), #17812, .F. ) ;
#5429 = CARTESIAN_POINT ( 'NONE',  ( -1.660104986876639543, -0.08942795157528024563, -0.3641732283464568787 ) ) ;
#5430 = CARTESIAN_POINT ( 'NONE',  ( -1.463254593175852492, 0.2952755905511811885, 0.1292274648535926551 ) ) ;
#5431 = CARTESIAN_POINT ( 'NONE',  ( 0.000000000000000000, 1.929133858267716661, 2.362204724409448620 ) ) ;
#5432 = VERTEX_POINT ( 'NONE', #52633 ) ;
#5433 = EDGE_CURVE ( 'NONE', #40470, #7361, #16503, .T. ) ;
#5434 = DIRECTION ( 'NONE',  ( 1.000000000000000000, 0.000000000000000000, 3.455050906509825972E-15 ) ) ;
#5435 = CARTESIAN_POINT ( 'NONE',  ( -1.305774278215222184, -0.6692913385826773087, -0.1292274648535924053 ) ) ;
#5436 = CARTESIAN_POINT ( 'NONE',  ( -0.7086614173228339419, -0.1870078740157480879, -0.4822834645669291653 ) ) ;
#5437 = CARTESIAN_POINT ( 'NONE',  ( 1.502624671916010790, -0.3162353388693409650, -0.4822834645669289433 ) ) ;
#5438 = CARTESIAN_POINT ( 'NONE',  ( -0.2867679344610365999, 0.2867679344610364889, -1.994094488188976610 ) ) ;
#5439 = DIRECTION ( 'NONE',  ( 0.000000000000000000, -1.000000000000000000, 0.000000000000000000 ) ) ;
#5440 = CARTESIAN_POINT ( 'NONE',  ( 0.8989501312335964611, 0.2952755905511811885, 0.1292274648535926551 ) ) ;
#5441 = CARTESIAN_POINT ( 'NONE',  ( 0.3871391076115493490, -0.3162353388693405765, 0.4822834645669290543 ) ) ;
#5442 = LINE ( 'NONE', #24378, #55679 ) ;
#5443 = DIRECTION ( 'NONE',  ( -1.000000000000000000, 0.000000000000000000, 1.692413147294445970E-16 ) ) ;
#5444 = CARTESIAN_POINT ( 'NONE',  ( 1.181102362204724976, -0.1870078740157480601, -0.3641732283464567677 ) ) ;
#5445 = CARTESIAN_POINT ( 'NONE',  ( 4.893765752498283924E-17, -0.3996062992125986035, -0.7086614173228346081 ) ) ;
#5446 = ORIENTED_EDGE ( 'NONE', *, *, #33065, .T. ) ;
#5447 = CARTESIAN_POINT ( 'NONE',  ( -0.3917322834645671215, 0.1049643490035301469, -2.702099737532808632 ) ) ;
#5448 = ORIENTED_EDGE ( 'NONE', *, *, #50835, .F. ) ;
#5449 = CARTESIAN_POINT ( 'NONE',  ( 0.3543307086614179147, 0.2952755905511811885, 0.000000000000000000 ) ) ;
#5450 = CARTESIAN_POINT ( 'NONE',  ( -0.8398950131233589023, -0.6046776061558809534, -0.2411417322834644161 ) ) ;
#5451 = CARTESIAN_POINT ( 'NONE',  ( -1.338582677165353729, -0.1870078740157479769, 0.4822834645669291653 ) ) ;
#5452 = CARTESIAN_POINT ( 'NONE',  ( 0.8727034120734913358, -0.05778040916215522460, 0.4822834645669289988 ) ) ;
#5453 = CARTESIAN_POINT ( 'NONE',  ( 1.548556430446194954, 0.2306618581243847221, -0.2411417322834647770 ) ) ;
#5454 = DIRECTION ( 'NONE',  ( 0.000000000000000000, 0.000000000000000000, 1.000000000000000000 ) ) ;
#5455 = CARTESIAN_POINT ( 'NONE',  ( -0.2493438320209966919, -0.4281496062992124485, 0.4176697321401328655 ) ) ;
#5456 = CARTESIAN_POINT ( 'NONE',  ( -1.430446194225720724, 0.05413385826771626580, -0.4176697321401330321 ) ) ;
#5457 = CARTESIAN_POINT ( 'NONE',  ( -1.489501312335957062, -0.05778040916215522460, 0.4822834645669289988 ) ) ;
#5458 = CARTESIAN_POINT ( 'NONE',  ( 1.640419947506562393, -0.4281496062992124485, 0.4176697321401328655 ) ) ;
#5459 = CARTESIAN_POINT ( 'NONE',  ( 0.3392501089628018884, -0.1958661417322834220, -2.866797900262466836 ) ) ;
#5460 = CARTESIAN_POINT ( 'NONE',  ( 0.8464566929133866546, -0.4536011799217367080, 0.2665933059059888421 ) ) ;
#5461 = ORIENTED_EDGE ( 'NONE', *, *, #20213, .F. ) ;
#5462 = CARTESIAN_POINT ( 'NONE',  ( -0.3949938075777411628, 0.1058382717557497937, -0.3477690288713912170 ) ) ;
#5463 = ORIENTED_EDGE ( 'NONE', *, *, #40392, .T. ) ;
#5464 = CARTESIAN_POINT ( 'NONE',  ( 0.1049868766404206816, -0.5023911411419708095, -0.1820866141732282451 ) ) ;
#5465 = CARTESIAN_POINT ( 'NONE',  ( 2.857004350179362273, 1.081388112195868390, -0.1351566381870096811 ) ) ;
#5466 = CARTESIAN_POINT ( 'NONE',  ( 0.7152230971128614723, -0.3162353388693409650, -0.4822834645669289433 ) ) ;
#5467 = CARTESIAN_POINT ( 'NONE',  ( 0.2624671916010504757, -0.6046776061558809534, -0.2411417322834644161 ) ) ;
#5468 = CARTESIAN_POINT ( 'NONE',  ( -0.7414698162729651543, 0.2952755905511810774, -0.1292274648535930714 ) ) ;
#5469 = ADVANCED_FACE ( 'NONE', ( #473 ), #47200, .F. ) ;
#5470 = CARTESIAN_POINT ( 'NONE',  ( 0.3917322834645670104, 0.1049643490035304660, -1.696213541503623912 ) ) ;
#5471 = CARTESIAN_POINT ( 'NONE',  ( -1.391076115485563314, -0.6046776061558809534, -0.2411417322834644161 ) ) ;
#5472 = CARTESIAN_POINT ( 'NONE',  ( 0.2867679344610365999, -0.2867679344610365444, -2.545275590551181022 ) ) ;
#5473 = CARTESIAN_POINT ( 'NONE',  ( 1.194225721784777594, -0.3690944881889765550, -0.3153832671262227771 ) ) ;
#5474 = CARTESIAN_POINT ( 'NONE',  ( -1.305774278215222184, 0.2952755905511811885, 0.1292274648535926551 ) ) ;
#5475 = CARTESIAN_POINT ( 'NONE',  ( 0.8530183727034128527, -0.4281496062992124485, 0.4176697321401328655 ) ) ;
#5476 = CARTESIAN_POINT ( 'NONE',  ( 1.043307086614173818, 0.1660481256975885056, 0.3530559997133364547 ) ) ;
#5477 = AXIS2_PLACEMENT_3D ( 'NONE', #24719, #17608, #62623 ) ;
#5478 = CARTESIAN_POINT ( 'NONE',  ( -0.3460692066303958092, -0.1998031496062994683, -0.6824146981627295938 ) ) ;
#5479 = CARTESIAN_POINT ( 'NONE',  ( -1.167979002624671470, -0.4281496062992127816, -0.4176697321401328100 ) ) ;
#5480 = CARTESIAN_POINT ( 'NONE',  ( 0.2925321140481932369, -0.2925321140481931814, -0.4901574803149606474 ) ) ;
#5481 = B_SPLINE_CURVE_WITH_KNOTS ( 'NONE', 3,
 ( #21600, #40965, #61140, #60320, #22435, #67059, #2669 ),
 .UNSPECIFIED., .F., .F.,
 ( 4, 3, 4 ),
 ( 0.000000000000000000, 0.001246232571205312112, 0.002492492258783314020 ),
 .UNSPECIFIED. ) ;
#5482 = CARTESIAN_POINT ( 'NONE',  ( -0.2034120734908131112, -0.6692913385826773087, -0.1292274648535924053 ) ) ;
#5483 = CARTESIAN_POINT ( 'NONE',  ( 0.3996062992125986590, -0.1070741851644053111, -2.473753280839894764 ) ) ;
#5484 = CARTESIAN_POINT ( 'NONE',  ( 0.2867679344610365999, 0.2867679344610365999, -1.797244094488188892 ) ) ;
#5485 = CARTESIAN_POINT ( 'NONE',  ( 1.430446194225722500, -0.4281496062992127816, -0.4176697321401328100 ) ) ;
#5486 = CARTESIAN_POINT ( 'NONE',  ( 0.08530183727034192087, -0.08942795157527998196, 0.3641732283464567121 ) ) ;
#5487 = CARTESIAN_POINT ( 'NONE',  ( 1.036745406824147508, -0.4281496062992127816, -0.4176697321401328100 ) ) ;
#5488 = CARTESIAN_POINT ( 'NONE',  ( -0.1265901696524993347, 0.4724409448818895907, -1.185695538057742526 ) ) ;
#5489 = CARTESIAN_POINT ( 'NONE',  ( 0.6627296587926517768, -0.5511811023622048555, -0.09757992244046775898 ) ) ;
#5490 = CARTESIAN_POINT ( 'NONE',  ( 0.5314960629921264834, 0.1660481256975883668, -0.3530559997133364547 ) ) ;
#5491 = CARTESIAN_POINT ( 'NONE',  ( -9.674558042662122972E-17, 0.3949938075777409963, -1.179133858267716661 ) ) ;
#5492 = CARTESIAN_POINT ( 'NONE',  ( -0.9186351706036736120, 0.2306618581243848609, 0.2411417322834645549 ) ) ;
#5493 = FACE_OUTER_BOUND ( 'NONE', #40997, .T. ) ;
#5494 = CARTESIAN_POINT ( 'NONE',  ( 1.049868766404200127, -0.5023911411419708095, -0.1820866141732282451 ) ) ;
#5495 = CARTESIAN_POINT ( 'NONE',  ( 0.4702623840880357786, 1.602034772339061552, -1.018747574612956619 ) ) ;
#5496 = CARTESIAN_POINT ( 'NONE',  ( -0.4593175853018366950, 0.05413385826771666132, 0.4176697321401328100 ) ) ;
#5497 = CARTESIAN_POINT ( 'NONE',  ( 0.2099737532808405305, -0.5023911411419708095, 0.1820866141732285504 ) ) ;
#5498 = CARTESIAN_POINT ( 'NONE',  ( 1.968503937007874072, 0.000000000000000000, 5.701968306260621233 ) ) ;
#5499 = CARTESIAN_POINT ( 'NONE',  ( -0.5249343832020990641, -0.6046776061558809534, -0.2411417322834644161 ) ) ;
#5500 = CARTESIAN_POINT ( 'NONE',  ( 0.8136482939632553313, 0.1283753931104748280, 0.1820866141732283561 ) ) ;
#5501 = CARTESIAN_POINT ( 'NONE',  ( 0.1998031496062994128, -0.3460692066303957537, -1.743438320209973913 ) ) ;
#5502 = CARTESIAN_POINT ( 'NONE',  ( 0.5118110236220480003, -0.6692913385826771977, 8.415575281601705876E-17 ) ) ;
#5503 = CARTESIAN_POINT ( 'NONE',  ( 1.200787401574803681, 0.07958543189024085140, 0.2665933059059887866 ) ) ;
#5504 = CARTESIAN_POINT ( 'NONE',  ( 0.2262115530851599166, 8.471767977567108961E-16, -0.4445507791589058955 ) ) ;
#5505 = CARTESIAN_POINT ( 'NONE',  ( -0.5643044619422565855, -0.004921259842519870586, -0.3153832671262229437 ) ) ;
#5506 = CARTESIAN_POINT ( 'NONE',  ( -0.6758530183727028406, -0.5511811023622048555, -0.09757992244046775898 ) ) ;
#5507 = CARTESIAN_POINT ( 'NONE',  ( -0.1574803149606292529, -0.1870078740157480879, -0.4822834645669291653 ) ) ;
#5508 = CARTESIAN_POINT ( 'NONE',  ( 0.5118110236220478892, 0.2952755905511811885, 0.000000000000000000 ) ) ;
#5509 = CARTESIAN_POINT ( 'NONE',  ( 0.8464566929133866546, -0.4536011799217367080, 0.2665933059059888421 ) ) ;
#5510 = CARTESIAN_POINT ( 'NONE',  ( -1.712598425196849572, 0.07958543189024085140, 0.2665933059059887866 ) ) ;
#5511 = CARTESIAN_POINT ( 'NONE',  ( -1.653543307086613234, -0.1870078740157480879, -0.4822834645669291653 ) ) ;
#5512 = CARTESIAN_POINT ( 'NONE',  ( 0.8136482939632553313, -0.6046776061558809534, -0.2411417322834644161 ) ) ;
#5513 = CARTESIAN_POINT ( 'NONE',  ( -1.604771003085129433, 1.829390573268580455, -0.1466069496707752273 ) ) ;
#5514 = CARTESIAN_POINT ( 'NONE',  ( -0.4330708661417315697, 0.2952755905511811885, 0.000000000000000000 ) ) ;
#5515 = CARTESIAN_POINT ( 'NONE',  ( -0.1958661417322834220, -0.3392501089628018884, -1.095144356955380704 ) ) ;
#5516 = CARTESIAN_POINT ( 'NONE',  ( 0.7611548556430454138, 0.2306618581243847221, -0.2411417322834647770 ) ) ;
#5517 = CARTESIAN_POINT ( 'NONE',  ( 0.5183727034120741983, -0.6692913385826771977, 0.1292274648535927661 ) ) ;
#5518 = LINE ( 'NONE', #6759, #49471 ) ;
#5519 = CARTESIAN_POINT ( 'NONE',  ( 0.2427821522309719648, -0.08942795157527998196, 0.3641732283464567121 ) ) ;
#5520 = CARTESIAN_POINT ( 'NONE',  ( 1.227034120734908917, 0.2952755905511810774, -0.1292274648535930714 ) ) ;
#5521 = EDGE_CURVE ( 'NONE', #50887, #11079, #40322, .T. ) ;
#5522 = CARTESIAN_POINT ( 'NONE',  ( -0.1181102362204717315, 0.1771653543307087630, 0.000000000000000000 ) ) ;
#5523 = CARTESIAN_POINT ( 'NONE',  ( -0.1640419947506553400, -0.05778040916215560624, -0.4822834645669293319 ) ) ;
#5524 = CARTESIAN_POINT ( 'NONE',  ( -1.614173228346456712, 2.401574803149606474, 0.1372047244094477536 ) ) ;
#5525 = CARTESIAN_POINT ( 'NONE',  ( 0.4133858267716541968, -0.5400638737290845981, -0.3530559997133363437 ) ) ;
#5526 = CARTESIAN_POINT ( 'NONE',  ( -0.7611548556430438595, -0.6046776061558809534, -0.2411417322834644161 ) ) ;
#5527 = CARTESIAN_POINT ( 'NONE',  ( -0.5183727034120726440, -0.5511811023622048555, -0.09757992244046775898 ) ) ;
#5528 = VECTOR ( 'NONE', #43648, 39.37007874015748143 ) ;
#5529 = CARTESIAN_POINT ( 'NONE',  ( 0.2624671916010504757, -0.6046776061558809534, -0.2411417322834644161 ) ) ;
#5530 = CARTESIAN_POINT ( 'NONE',  ( -1.377952755905511140, 0.2952755905511811885, 0.000000000000000000 ) ) ;
#5531 = CARTESIAN_POINT ( 'NONE',  ( -0.4658792650918627265, -0.3162353388693409650, -0.4822834645669289433 ) ) ;
#5532 = CARTESIAN_POINT ( 'NONE',  ( 0.4724409448818902568, -0.1265901696524981135, -0.5839895013123360679 ) ) ;
#5534 = CARTESIAN_POINT ( 'NONE',  ( 1.312335958005249825, 0.2306618581243847221, -0.2411417322834647770 ) ) ;
#5533 = CARTESIAN_POINT ( 'NONE',  ( -0.9329488473419921268, -1.146068349578384814E-15, 0.3627985898453523483 ) ) ;
#5535 = CARTESIAN_POINT ( 'NONE',  ( 1.620734908136483465, -0.6692913385826771977, 0.1292274648535927661 ) ) ;
#5536 = CARTESIAN_POINT ( 'NONE',  ( 0.1958661417322836440, -0.3392501089628017219, -2.131233595800524849 ) ) ;
#5537 = PLANE ( 'NONE',  #27442 ) ;
#5538 = CARTESIAN_POINT ( 'NONE',  ( -1.023622047244094002, -0.1870078740157480879, -0.4822834645669291653 ) ) ;
#5539 = CARTESIAN_POINT ( 'NONE',  ( 0.3458507752293908943, -0.3458507752293908943, -0.2559055118110235560 ) ) ;
#5540 = CARTESIAN_POINT ( 'NONE',  ( 0.1058382717557499880, 0.3949938075777411073, -2.670603674540682260 ) ) ;
#5541 = VERTEX_POINT ( 'NONE', #41498 ) ;
#5542 = CARTESIAN_POINT ( 'NONE',  ( 0.2821522309711292364, 0.1771653543307087075, -0.09757992244046823083 ) ) ;
#5543 = CARTESIAN_POINT ( 'NONE',  ( 4.797336870675656522E-17, -0.3917322834645670104, -1.330708661417322691 ) ) ;
#5544 = CARTESIAN_POINT ( 'NONE',  ( 0.6233595800524939223, -0.3162353388693405765, 0.4822834645669290543 ) ) ;
#5545 = CARTESIAN_POINT ( 'NONE',  ( -0.2362204724409451284, 0.4091458600556402425, -2.690288713910760965 ) ) ;
#5546 = DIRECTION ( 'NONE',  ( 1.000000000000000000, 0.000000000000000000, 0.000000000000000000 ) ) ;
#5547 = CARTESIAN_POINT ( 'NONE',  ( -0.5708661417322825615, -0.4536011799217367080, 0.2665933059059888421 ) ) ;
#5549 = AXIS2_PLACEMENT_3D ( 'NONE', #58593, #52269, #962 ) ;
#5548 = CARTESIAN_POINT ( 'NONE',  ( -1.706036745406823485, 0.1283753931104748280, 0.1820866141732283561 ) ) ;
#5550 = CARTESIAN_POINT ( 'NONE',  ( 1.233595800524935227, 0.2306618581243847221, -0.2411417322834647770 ) ) ;
#5551 = CARTESIAN_POINT ( 'NONE',  ( 0.8202099737532813073, 0.1771653543307087630, 0.09757992244046791164 ) ) ;
#5552 = CARTESIAN_POINT ( 'NONE',  ( -0.1771653543307080136, 0.1660481256975883668, -0.3530559997133364547 ) ) ;
#5553 = CARTESIAN_POINT ( 'NONE',  ( -0.3917322834645670659, 0.1049643490035301607, -0.5852825214885022387 ) ) ;
#5554 = CARTESIAN_POINT ( 'NONE',  ( -0.6036745406824141069, -0.6046776061558809534, -0.2411417322834644161 ) ) ;
#5555 = CARTESIAN_POINT ( 'NONE',  ( -1.266404199475064773, -0.2845877964562159024, 0.3641732283464567677 ) ) ;
#5556 = CARTESIAN_POINT ( 'NONE',  ( -0.4527559055118102749, 0.1660481256975885056, 0.3530559997133364547 ) ) ;
#5557 = LINE ( 'NONE', #70354, #7207 ) ;
#5558 = DIRECTION ( 'NONE',  ( 0.000000000000000000, 1.000000000000000000, 0.000000000000000000 ) ) ;
#5559 = ORIENTED_EDGE ( 'NONE', *, *, #30484, .F. ) ;
#5560 = CARTESIAN_POINT ( 'NONE',  ( 0.1958661417322834775, 0.3392501089628018884, -1.873378895834332258 ) ) ;
#5561 = CARTESIAN_POINT ( 'NONE',  ( 0.5118110236220480003, -0.6692913385826771977, 8.415575281601705876E-17 ) ) ;
#5562 = ORIENTED_EDGE ( 'NONE', *, *, #58189, .T. ) ;
#5563 = CARTESIAN_POINT ( 'NONE',  ( -0.3543307086614165824, -0.6692913385826771977, 8.415575281601705876E-17 ) ) ;
#5564 = CARTESIAN_POINT ( 'NONE',  ( -1.305774278215222184, 0.2952755905511811885, 0.1292274648535926551 ) ) ;
#5565 = CARTESIAN_POINT ( 'NONE',  ( 0.5774278215223103139, -0.6046776061558809534, -0.2411417322834644161 ) ) ;
#5566 = CARTESIAN_POINT ( 'NONE',  ( 0.03280839895013198948, -0.6692913385826773087, -0.1292274648535924053 ) ) ;
#5567 = CARTESIAN_POINT ( 'NONE',  ( 0.3917322834645669549, 0.1049643490035304660, -1.469160104986876769 ) ) ;
#5568 = CARTESIAN_POINT ( 'NONE',  ( -0.9055118110236215490, 0.2952755905511811885, 0.000000000000000000 ) ) ;
#5569 = CARTESIAN_POINT ( 'NONE',  ( 0.2887139107611556010, 0.2306618581243847221, -0.2411417322834647770 ) ) ;
#5570 = CARTESIAN_POINT ( 'NONE',  ( -0.4002624671916004129, -0.3162353388693405765, 0.4822834645669290543 ) ) ;
#5571 = CARTESIAN_POINT ( 'NONE',  ( 0.4330708661417329575, 0.1771653543307087630, 0.000000000000000000 ) ) ;
#5572 = CARTESIAN_POINT ( 'NONE',  ( -0.2917302971764580977, -0.04706822171083040879, 5.873170128030149151 ) ) ;
#5573 = CARTESIAN_POINT ( 'NONE',  ( -0.2034120734908131112, -0.6692913385826773087, -0.1292274648535924053 ) ) ;
#5574 = DIRECTION ( 'NONE',  ( 0.000000000000000000, 0.000000000000000000, 1.000000000000000000 ) ) ;
#5575 = CARTESIAN_POINT ( 'NONE',  ( 1.476377952755906220, 0.1660481256975883668, -0.3530559997133364547 ) ) ;
#5576 = CARTESIAN_POINT ( 'NONE',  ( 0.3392501089628018329, 0.1958661417322835607, -2.643044619422571628 ) ) ;
#5577 = VERTEX_POINT ( 'NONE', #67183 ) ;
#5578 = ORIENTED_EDGE ( 'NONE', *, *, #44328, .F. ) ;
#5579 = CARTESIAN_POINT ( 'NONE',  ( 0.4002624671916016896, -0.05778040916215522460, 0.4822834645669289988 ) ) ;
#5580 = CARTESIAN_POINT ( 'NONE',  ( -0.01968503937007793844, -0.4536011799217367080, 0.2665933059059888421 ) ) ;
#5582 = CARTESIAN_POINT ( 'NONE',  ( -0.06804098107080119862, -3.915482057279200494E-15, 0.4118484887281999574 ) ) ;
#5581 = CARTESIAN_POINT ( 'NONE',  ( 1.259842519685040019, -0.1870078740157480601, -0.3641732283464567677 ) ) ;
#5583 = CARTESIAN_POINT ( 'NONE',  ( -0.2867679344610364334, -0.2867679344610367109, -1.088582677165354173 ) ) ;
#5584 = CARTESIAN_POINT ( 'NONE',  ( -0.4724409448818899238, 0.1265901696524986686, 0.04790026246719158304 ) ) ;
#5585 = CARTESIAN_POINT ( 'NONE',  ( -0.3996062992125986590, 0.1070741851644051723, -2.786745406824146620 ) ) ;
#5586 = CARTESIAN_POINT ( 'NONE',  ( 0.3871391076115492380, -0.05778040916215560624, -0.4822834645669293319 ) ) ;
#5587 = CARTESIAN_POINT ( 'NONE',  ( -1.430446194225720724, 0.05413385826771626580, -0.4176697321401330321 ) ) ;
#5588 = CARTESIAN_POINT ( 'NONE',  ( -1.089238845144356427, 0.05413385826771666132, 0.4176697321401328100 ) ) ;
#5589 = CARTESIAN_POINT ( 'NONE',  ( 0.1377952755905518800, -0.5400638737290844871, 0.3530559997133364547 ) ) ;
#5590 = STYLED_ITEM ( 'NONE', ( #2289 ), #33421 ) ;
#5591 = CARTESIAN_POINT ( 'NONE',  ( 0.8792650918635177559, -0.4281496062992127816, -0.4176697321401328100 ) ) ;
#5592 = CARTESIAN_POINT ( 'NONE',  ( 1.456692913385827515, -0.5511811023622047445, 6.969142054262312111E-17 ) ) ;
#5593 = CONTEXT_DEPENDENT_SHAPE_REPRESENTATION ( #77201, #45952 ) ;
#5594 = CARTESIAN_POINT ( 'NONE',  ( 0.6824146981627303710, -0.5023911411419708095, 0.1820866141732285504 ) ) ;
#5595 = CARTESIAN_POINT ( 'NONE',  ( -1.049868766404198794, -0.6046776061558807314, 0.2411417322834647770 ) ) ;
#5596 = CARTESIAN_POINT ( 'NONE',  ( 0.3460692066303959202, -0.1998031496062991630, -0.4967191601049869010 ) ) ;
#5597 = CARTESIAN_POINT ( 'NONE',  ( 1.482939632545932307, -0.4281496062992124485, 0.4176697321401328655 ) ) ;
#5598 = CARTESIAN_POINT ( 'NONE',  ( -9.594673741351313045E-17, 0.3917322834645670104, -0.3070866141732283006 ) ) ;
#5600 = CARTESIAN_POINT ( 'NONE',  ( 3.937007874015748143, 2.755905511811024056, -0.5314960629921260393 ) ) ;
#5599 = CARTESIAN_POINT ( 'NONE',  ( 1.351706036745407680, 0.05413385826771666132, 0.4176697321401328100 ) ) ;
#5601 = CARTESIAN_POINT ( 'NONE',  ( -1.673228346456691717, 0.07958543189024071263, -0.2665933059059888421 ) ) ;
#5602 = CARTESIAN_POINT ( 'NONE',  ( 0.006561679790026889343, -0.3162353388693409650, -0.4822834645669289433 ) ) ;
#5603 = CARTESIAN_POINT ( 'NONE',  ( 0.6692913385826777528, 0.1771653543307087630, 0.000000000000000000 ) ) ;
#5604 = CARTESIAN_POINT ( 'NONE',  ( -1.522309711286088607, 0.1283753931104746893, -0.1820866141732285504 ) ) ;
#5605 = CARTESIAN_POINT ( 'NONE',  ( 1.108923884514436686, -0.3162353388693409650, -0.4822834645669289433 ) ) ;
#5606 = CARTESIAN_POINT ( 'NONE',  ( -0.5314960629921250401, 0.1660481256975885056, 0.3530559997133364547 ) ) ;
#5607 = CARTESIAN_POINT ( 'NONE',  ( -0.5249343832020990641, -0.5023911411419708095, -0.1820866141732282451 ) ) ;
#5608 = CARTESIAN_POINT ( 'NONE',  ( -0.6036745406824141069, 0.2306618581243848609, 0.2411417322834645549 ) ) ;
#5609 = CARTESIAN_POINT ( 'NONE',  ( 1.417322834645670104, -0.1870078740157480879, -0.4822834645669291653 ) ) ;
#5610 = CARTESIAN_POINT ( 'NONE',  ( -1.043307086614172707, 0.1660481256975883668, -0.3530559997133364547 ) ) ;
#5611 = CARTESIAN_POINT ( 'NONE',  ( 1.496062992125985147, -0.1870078740157479769, 0.4822834645669291653 ) ) ;
#5612 = CARTESIAN_POINT ( 'NONE',  ( -0.3392501089628017219, -0.1958661417322836995, -0.9941138039708155016 ) ) ;
#5613 = CARTESIAN_POINT ( 'NONE',  ( -1.292650918635170010, 0.1771653543307087075, -0.09757992244046823083 ) ) ;
#5614 = EDGE_CURVE ( 'NONE', #25547, #69342, #35597, .T. ) ;
#5615 = CARTESIAN_POINT ( 'NONE',  ( 1.116867003146159609, 1.075369016579923676, 0.1087923042922196853 ) ) ;
#5616 = CARTESIAN_POINT ( 'NONE',  ( 0.8858267716535438430, -0.5400638737290845981, -0.3530559997133363437 ) ) ;
#5617 = B_SPLINE_CURVE_WITH_KNOTS ( 'NONE', 3,
 ( #41673, #42085, #67780, #67365, #61034, #29046, #54717, #56767, #82062, #82873, #69419, #37011, #50450, #49634, #81656, #43717, #57595, #76152, #23967, #25197, #6256, #63512, #75327, #56363, #11353, #31933, #25608, #17673, #83285, #30699, #62269, #50863, #24375, #51271, #18492, #38244, #63921, #50046 ),
 .UNSPECIFIED., .F., .F.,
 ( 4, 2, 2, 2, 2, 2, 2, 2, 2, 2, 2, 2, 2, 2, 2, 2, 2, 2, 4 ),
 ( 0.000000000000000000, 0.003207193274590005357, 0.004810789911885009554, 0.006414386549180013317, 0.007216184867827516065, 0.008017983186475018814, 0.009621579823770027781, 0.01042337814241752966, 0.01122517646106503328, 0.01282877309836003878, 0.01363057141700754413, 0.01443236973565504601, 0.01603596637295005151, 0.01763956301024505874, 0.01924315964754006250, 0.02084675628483506973, 0.02245035292213007003, 0.02405394955942507726, 0.02565754619672007755 ),
 .UNSPECIFIED. ) ;
#5618 = CARTESIAN_POINT ( 'NONE',  ( 0.2362204724409449064, 0.4091458600556404646, -2.425853018372703396 ) ) ;
#5619 = CARTESIAN_POINT ( 'NONE',  ( -1.548556430446193399, 0.2306618581243848609, 0.2411417322834645549 ) ) ;
#5620 = CARTESIAN_POINT ( 'NONE',  ( -1.653543307086613234, -0.1870078740157479769, 0.3641732283464567677 ) ) ;
#5621 = CARTESIAN_POINT ( 'NONE',  ( -0.9711286089238838626, -0.5023911411419708095, 0.1820866141732285504 ) ) ;
#5622 = CARTESIAN_POINT ( 'NONE',  ( 1.646981627296588035, -0.2845877964562159024, 0.3641732283464567677 ) ) ;
#5623 = CARTESIAN_POINT ( 'NONE',  ( -0.5577427821522301654, -0.3162353388693405765, 0.4822834645669290543 ) ) ;
#5624 = CARTESIAN_POINT ( 'NONE',  ( -0.04593175853018302557, 0.1771653543307087630, 0.09757992244046791164 ) ) ;
#5625 = CARTESIAN_POINT ( 'NONE',  ( -1.456692913385826182, -0.5511811023622047445, 6.969142054262312111E-17 ) ) ;
#5626 = CARTESIAN_POINT ( 'NONE',  ( 1.522309711286089939, -0.5023911411419708095, -0.1820866141732282451 ) ) ;
#5627 = CARTESIAN_POINT ( 'NONE',  ( 0.8989501312335964611, 0.2952755905511811885, 0.1292274648535926551 ) ) ;
#5628 = CARTESIAN_POINT ( 'NONE',  ( 1.397637795275591177, -0.5400638737290844871, 0.3530559997133364547 ) ) ;
#5629 = CARTESIAN_POINT ( 'NONE',  ( 0.05905511811023709395, -0.4536011799217367080, 0.2665933059059888421 ) ) ;
#5630 = CARTESIAN_POINT ( 'NONE',  ( 0.6430446194225729606, -0.4281496062992127816, -0.4176697321401328100 ) ) ;
#5631 = CARTESIAN_POINT ( 'NONE',  ( 1.148293963254593653, 0.1771653543307087075, -0.09757992244046823083 ) ) ;
#5632 = ORIENTED_EDGE ( 'NONE', *, *, #56851, .T. ) ;
#5633 = CARTESIAN_POINT ( 'NONE',  ( -1.522309711286088607, -0.6046776061558807314, 0.2411417322834647770 ) ) ;
#5634 = CARTESIAN_POINT ( 'NONE',  ( -1.456692913385826182, 0.2952755905511811885, 0.000000000000000000 ) ) ;
#5635 = CARTESIAN_POINT ( 'NONE',  ( -0.3083989501312330295, -0.05778040916215522460, 0.4822834645669289988 ) ) ;
#5636 = CARTESIAN_POINT ( 'NONE',  ( -0.3460692066303960868, 0.1998031496062990242, -0.3412073490813647969 ) ) ;
#5637 = CARTESIAN_POINT ( 'NONE',  ( -0.3996062992125984925, -0.1070741851644056858, -2.642388451443570041 ) ) ;
#5638 = CARTESIAN_POINT ( 'NONE',  ( 0.3608923884514443348, 0.2952755905511810774, -0.1292274648535930714 ) ) ;
#5639 = CARTESIAN_POINT ( 'NONE',  ( 1.292650918635171564, 0.1771653543307087630, 0.09757992244046791164 ) ) ;
#5640 = CARTESIAN_POINT ( 'NONE',  ( 0.1837270341207357105, -0.6046776061558809534, -0.2411417322834644161 ) ) ;
#5641 = CARTESIAN_POINT ( 'NONE',  ( 0.1640419947506569498, -0.05778040916215522460, 0.4822834645669289988 ) ) ;
#5642 = CARTESIAN_POINT ( 'NONE',  ( -0.1070741851644051862, -0.3996062992125987146, -2.276902887139107268 ) ) ;
#5643 = CARTESIAN_POINT ( 'NONE',  ( 0.3420746716998659953, 0.1974969037888705536, -1.548556430446194065 ) ) ;
#5644 = CARTESIAN_POINT ( 'NONE',  ( -0.2386152867011636369, 1.127078383925389504, 1.096469326408681999 ) ) ;
#5645 = CARTESIAN_POINT ( 'NONE',  ( 0.4724409448818898682, 2.892866454678787531E-17, -2.480314960629921295 ) ) ;
#5646 = CARTESIAN_POINT ( 'NONE',  ( 0.1049643490035304799, -0.3917322834645669549, -0.5498687664041993495 ) ) ;
#5647 = CARTESIAN_POINT ( 'NONE',  ( -0.6299212598425188991, -0.1870078740157479769, 0.3641732283464567677 ) ) ;
#5648 = CARTESIAN_POINT ( 'NONE',  ( -0.7414698162729651543, 0.2952755905511810774, -0.1292274648535930714 ) ) ;
#5649 = VECTOR ( 'NONE', #69209, 39.37007874015748143 ) ;
#5650 = CARTESIAN_POINT ( 'NONE',  ( 0.3949938075777408852, 0.1058382717557500435, -2.406167979002624691 ) ) ;
#5651 = CARTESIAN_POINT ( 'NONE',  ( 0.7283464566929143125, 0.1660481256975885056, 0.3530559997133364547 ) ) ;
#5652 = CARTESIAN_POINT ( 'NONE',  ( -1.410761154855641575, -0.3162353388693409650, -0.4822834645669289433 ) ) ;
#5653 = CARTESIAN_POINT ( 'NONE',  ( 0.6758530183727039509, 0.2952755905511810774, -0.1292274648535930714 ) ) ;
#5654 = CARTESIAN_POINT ( 'NONE',  ( -0.4091458600556405756, 0.2362204724409446288, -2.703412073490813583 ) ) ;
#5655 = CARTESIAN_POINT ( 'NONE',  ( 0.3996062992125986590, -0.1070741851644053111, -2.001312335958005395 ) ) ;
#5656 = CARTESIAN_POINT ( 'NONE',  ( 1.594488188976378673, -0.5400638737290845981, -0.3530559997133363437 ) ) ;
#5657 = CARTESIAN_POINT ( 'NONE',  ( 0.7086614173228352742, -0.1870078740157480879, -0.4822834645669291653 ) ) ;
#5658 = CARTESIAN_POINT ( 'NONE',  ( 0.7152230971128614723, -0.3162353388693409650, -0.4822834645669289433 ) ) ;
#5659 = CARTESIAN_POINT ( 'NONE',  ( 0.9776902887139113929, 0.1771653543307087630, 0.09757992244046791164 ) ) ;
#5660 = CARTESIAN_POINT ( 'NONE',  ( 1.377952755905512472, 0.2952755905511811885, 0.000000000000000000 ) ) ;
#5661 = CARTESIAN_POINT ( 'NONE',  ( -0.3917322834645670104, -7.196005306013484475E-17, -0.1240157480314961758 ) ) ;
#5662 = CARTESIAN_POINT ( 'NONE',  ( -0.5314960629921348101, 2.729661060880496759, 2.530077729939674835 ) ) ;
#5663 = CARTESIAN_POINT ( 'NONE',  ( 0.7545931758530189937, 0.2952755905511810774, -0.1292274648535930714 ) ) ;
#5664 = DIRECTION ( 'NONE',  ( 0.000000000000000000, 0.000000000000000000, -1.000000000000000000 ) ) ;
#5665 = CARTESIAN_POINT ( 'NONE',  ( -0.5249343832020990641, -0.6046776061558809534, -0.2411417322834644161 ) ) ;
#5666 = CARTESIAN_POINT ( 'NONE',  ( -1.049868766404198794, 0.2306618581243847221, -0.2411417322834647770 ) ) ;
#5667 = CARTESIAN_POINT ( 'NONE',  ( 0.9776902887139113929, 0.2952755905511811885, 0.1292274648535926551 ) ) ;
#5668 = CARTESIAN_POINT ( 'NONE',  ( -9.594673741351313045E-17, 0.3917322834645670104, -0.7145669291338584417 ) ) ;
#5669 = CARTESIAN_POINT ( 'NONE',  ( 0.3392501089628018884, -0.1958661417322834220, -1.671916010498687655 ) ) ;
#5670 = CARTESIAN_POINT ( 'NONE',  ( 0.3392501089628018329, 0.1958661417322835607, -2.643044619422571628 ) ) ;
#5671 = ORIENTED_EDGE ( 'NONE', *, *, #32566, .T. ) ;
#5672 = CARTESIAN_POINT ( 'NONE',  ( 4.893765752498283924E-17, -0.3996062992125986035, -0.07874015748031498729 ) ) ;
#5673 = VERTEX_POINT ( 'NONE', #9926 ) ;
#5674 = CARTESIAN_POINT ( 'NONE',  ( 1.345144356955381593, -0.2845877964562161244, -0.3641732283464567121 ) ) ;
#5675 = CARTESIAN_POINT ( 'NONE',  ( -0.1070741851644051862, -0.3996062992125987146, -1.332020997375328086 ) ) ;
#5676 = CARTESIAN_POINT ( 'NONE',  ( 1.358267716535433323, 0.07958543189024085140, 0.2665933059059887866 ) ) ;
#5677 = CARTESIAN_POINT ( 'NONE',  ( -0.7759054087898756835, -3.623651218081290895E-15, 0.3791475997938233977 ) ) ;
#5678 = CARTESIAN_POINT ( 'NONE',  ( 0.000000000000000000, 0.4374015748031496176, 0.000000000000000000 ) ) ;
#5679 = CARTESIAN_POINT ( 'NONE',  ( 3.833048050305355326E-17, 1.954428616053095924, 0.3129921259842520787 ) ) ;
#5680 = CARTESIAN_POINT ( 'NONE',  ( 0.3392501089628018884, -0.1958661417322834220, -0.3471128608923885195 ) ) ;
#5681 = CARTESIAN_POINT ( 'NONE',  ( -0.8202099737532799750, 0.1771653543307087075, -0.09757992244046823083 ) ) ;
#5682 = CARTESIAN_POINT ( 'NONE',  ( -1.660104986876639543, -0.08942795157528024563, -0.3641732283464568787 ) ) ;
#5683 = CARTESIAN_POINT ( 'NONE',  ( -1.240157480314959759, -0.5400638737290845981, -0.3530559997133363437 ) ) ;
#5684 = CARTESIAN_POINT ( 'NONE',  ( 0.03280839895013198948, 0.2952755905511811885, 0.1292274648535926551 ) ) ;
#5685 = CARTESIAN_POINT ( 'NONE',  ( -1.653543307086613234, -0.1870078740157479769, 0.4822834645669291653 ) ) ;
#5686 = ORIENTED_EDGE ( 'NONE', *, *, #74381, .F. ) ;
#5687 = CARTESIAN_POINT ( 'NONE',  ( 1.568241469816273437, -0.3162353388693405765, 0.4822834645669290543 ) ) ;
#5688 = CARTESIAN_POINT ( 'NONE',  ( 1.912049360642951330E-20, 1.062992125984252745, -2.874015748031495843 ) ) ;
#5689 = CARTESIAN_POINT ( 'NONE',  ( 0.1265901696524990294, -0.4724409448818896462, -1.975065616797900381 ) ) ;
#5690 = CARTESIAN_POINT ( 'NONE',  ( 0.7086614173228347191, 0.000000000000000000, 0.000000000000000000 ) ) ;
#5691 = CARTESIAN_POINT ( 'NONE',  ( -0.3805774278215216522, -0.004921259842519576551, 0.3153832671262227771 ) ) ;
#5692 = CARTESIAN_POINT ( 'NONE',  ( -1.259842519685038686, -0.1870078740157480879, -0.4822834645669291653 ) ) ;
#5693 = CARTESIAN_POINT ( 'NONE',  ( 1.135170603674541256, -0.6692913385826773087, -0.1292274648535924053 ) ) ;
#5694 = VERTEX_POINT ( 'NONE', #6077 ) ;
#5696 = CARTESIAN_POINT ( 'NONE',  ( -1.614173228346457378, 0.7794589730111965986, 0.1372047244094476981 ) ) ;
#5695 = CARTESIAN_POINT ( 'NONE',  ( 0.7742782152230979209, 0.05413385826771626580, -0.4176697321401330321 ) ) ;
#5697 = CARTESIAN_POINT ( 'NONE',  ( 1.095800524934383846, -0.05778040916215560624, -0.4822834645669293319 ) ) ;
#5698 = CARTESIAN_POINT ( 'NONE',  ( -1.272965879265091305, -0.4281496062992124485, 0.4176697321401328655 ) ) ;
#5699 = CARTESIAN_POINT ( 'NONE',  ( 0.1049643490035304522, -0.3917322834645668994, -0.3228153298874523180 ) ) ;
#5700 = CARTESIAN_POINT ( 'NONE',  ( -0.3018372703412066094, -0.004921259842519576551, 0.3153832671262227771 ) ) ;
#5701 = CARTESIAN_POINT ( 'NONE',  ( -0.3392501089628019995, 0.1958661417322832277, -0.8982939632545933195 ) ) ;
#5702 = CARTESIAN_POINT ( 'NONE',  ( -0.5118110236220466680, 0.1771653543307087630, 0.000000000000000000 ) ) ;
#5703 = CARTESIAN_POINT ( 'NONE',  ( 0.6364829396325465405, -0.08942795157527998196, 0.3641732283464567121 ) ) ;
#5704 = CARTESIAN_POINT ( 'NONE',  ( 0.2296587926509192634, -0.05778040916215560624, -0.4822834645669293319 ) ) ;
#5705 = AXIS2_PLACEMENT_3D ( 'NONE', #56863, #24473, #63605 ) ;
#5706 = CARTESIAN_POINT ( 'NONE',  ( -0.6036745406824141069, -0.5023911411419708095, -0.1820866141732282451 ) ) ;
#5707 = CARTESIAN_POINT ( 'NONE',  ( 0.2867679344610365999, -0.2867679344610365444, -2.925196850393700920 ) ) ;
#5708 = CARTESIAN_POINT ( 'NONE',  ( 1.181102362204724976, -0.1870078740157480879, -0.4822834645669291653 ) ) ;
#5709 = ADVANCED_FACE ( 'NONE', ( #11589 ), #39292, .F. ) ;
#5710 = CARTESIAN_POINT ( 'NONE',  ( -0.8398950131233585692, 0.2306618581243848609, 0.2411417322834645549 ) ) ;
#5711 = CARTESIAN_POINT ( 'NONE',  ( -0.4724409448818899238, 0.1265901696524986686, -1.369422572178477404 ) ) ;
#5712 = CARTESIAN_POINT ( 'NONE',  ( -0.1902887139107604098, -0.6692913385826771977, 0.1292274648535927661 ) ) ;
#5713 = CARTESIAN_POINT ( 'NONE',  ( -0.7283464566929126471, -0.5400638737290844871, 0.3530559997133364547 ) ) ;
#5714 = CARTESIAN_POINT ( 'NONE',  ( 1.364829396325460076, 0.1283753931104748280, 0.1820866141732283561 ) ) ;
#5715 = CARTESIAN_POINT ( 'NONE',  ( 0.1049868766404206816, -0.5023911411419708095, -0.1820866141732282451 ) ) ;
#5716 = CARTESIAN_POINT ( 'NONE',  ( -0.6036745406824141069, 0.2306618581243848609, 0.2411417322834645549 ) ) ;
#5717 = CARTESIAN_POINT ( 'NONE',  ( -1.194225721784776262, -0.4281496062992124485, 0.4176697321401328655 ) ) ;
#5718 = FACE_OUTER_BOUND ( 'NONE', #76006, .T. ) ;
#5719 = CARTESIAN_POINT ( 'NONE',  ( 1.154855643044620184, -0.5023911411419708095, 0.1820866141732285504 ) ) ;
#5720 = CARTESIAN_POINT ( 'NONE',  ( -0.1443569553805765515, -0.4281496062992127816, -0.4176697321401328100 ) ) ;
#5721 = CARTESIAN_POINT ( 'NONE',  ( -1.122047244094487306, -0.5400638737290844871, 0.3530559997133364547 ) ) ;
#5722 = ORIENTED_EDGE ( 'NONE', *, *, #11555, .F. ) ;
#5723 = CARTESIAN_POINT ( 'NONE',  ( -0.3996062992125984925, -0.1070741851644056858, -2.012467191601049699 ) ) ;
#5724 = CARTESIAN_POINT ( 'NONE',  ( 1.128608923884514947, 0.2306618581243848609, 0.2411417322834645549 ) ) ;
#5725 = CARTESIAN_POINT ( 'NONE',  ( -0.6889763779527552368, -0.4536011799217368745, -0.2665933059059886201 ) ) ;
#5726 = CARTESIAN_POINT ( 'NONE',  ( -0.3460692066303957537, -0.1998031496062994405, -1.546587926509186639 ) ) ;
#5727 = CARTESIAN_POINT ( 'NONE',  ( -1.003937007874015297, -0.5400638737290845981, -0.3530559997133363437 ) ) ;
#5728 = CARTESIAN_POINT ( 'NONE',  ( 1.259842519685040019, -0.1870078740157480879, -0.4822834645669291653 ) ) ;
#5729 = CARTESIAN_POINT ( 'NONE',  ( 1.115485564304462551, -0.4281496062992127816, -0.4176697321401328100 ) ) ;
#5730 = CARTESIAN_POINT ( 'NONE',  ( 1.515748031496063186, -0.5400638737290845981, -0.3530559997133363437 ) ) ;
#5731 = CARTESIAN_POINT ( 'NONE',  ( -0.9711286089238838626, -0.5023911411419708095, 0.1820866141732285504 ) ) ;
#5732 = CARTESIAN_POINT ( 'NONE',  ( 0.2925321140481931814, -0.2925321140481931259, -0.4901574803149605919 ) ) ;
#5733 = CARTESIAN_POINT ( 'NONE',  ( 0.3996062992125986035, 0.1070741851644054776, -1.069553805774278166 ) ) ;
#5734 = CARTESIAN_POINT ( 'NONE',  ( 0.3949938075777409963, 2.418639510665530435E-17, -0.4330708661417323468 ) ) ;
#5735 = CARTESIAN_POINT ( 'NONE',  ( 0.2639696576368102954, 1.142922413699645645, 2.800935327256448559 ) ) ;
#5736 = CARTESIAN_POINT ( 'NONE',  ( 1.351706036745407680, -0.004921259842519576551, 0.3153832671262227771 ) ) ;
#5737 = ADVANCED_FACE ( 'NONE', ( #75153 ), #31239, .F. ) ;
#5738 = CARTESIAN_POINT ( 'NONE',  ( 0.8464566929133865436, 0.07958543189024071263, -0.2665933059059888421 ) ) ;
#5739 = CARTESIAN_POINT ( 'NONE',  ( 0.4921259842519691285, 0.1660481256975885056, 0.3530559997133364547 ) ) ;
#5740 = CARTESIAN_POINT ( 'NONE',  ( 1.555118110236221041, -0.5400638737290844871, 0.3530559997133364547 ) ) ;
#5741 = CARTESIAN_POINT ( 'NONE',  ( -0.1058382717557503072, 0.3949938075777408852, -1.500656167979002253 ) ) ;
#5742 = CARTESIAN_POINT ( 'NONE',  ( 0.9580052493438327987, -0.3690944881889765550, -0.3153832671262227771 ) ) ;
#5743 = CARTESIAN_POINT ( 'NONE',  ( -0.3412073490813641308, 0.2306618581243847221, -0.2411417322834647770 ) ) ;
#5744 = CARTESIAN_POINT ( 'NONE',  ( -1.253280839895012377, -0.3162353388693409650, -0.4822834645669289433 ) ) ;
#5745 = CARTESIAN_POINT ( 'NONE',  ( 1.404199475065617708, 0.05413385826771626580, -0.4176697321401330321 ) ) ;
#5746 = CARTESIAN_POINT ( 'NONE',  ( 0.3458507752293908943, 0.3458507752293908943, -1.555118110236220597 ) ) ;
#5747 = CARTESIAN_POINT ( 'NONE',  ( -0.1070741851644057135, 0.3996062992125985480, -2.683727034120734878 ) ) ;
#5748 = CARTESIAN_POINT ( 'NONE',  ( 0.07874015748031558404, -0.1870078740157480601, -0.3641732283464567677 ) ) ;
#5749 =( BOUNDED_CURVE ( )  B_SPLINE_CURVE ( 2, ( #64966, #19936, #72114, #14881, #33810, #52732, #59062, #66221, #65812, #65397, #40541, #21184, #53146 ),
 .UNSPECIFIED., .F., .F. ) 
 B_SPLINE_CURVE_WITH_KNOTS ( ( 3, 2, 2, 2, 2, 2, 3 ),
 ( 0.5035787205705963832, 0.5037878787878788955, 0.5075757575757575690, 0.5113636363636364646, 0.5151515151515151381, 0.5189393939393940336, 0.5191485521566765460 ),
 .UNSPECIFIED. ) 
 CURVE ( )  GEOMETRIC_REPRESENTATION_ITEM ( )  RATIONAL_B_SPLINE_CURVE ( ( 0.9964447847208420805, 0.9981185001348091834, 1.000000000000000000, 0.9659258262890683122, 1.000000000000000000, 0.9659258262890683122, 1.000000000000000000, 0.9659258262890683122, 1.000000000000000000, 0.9659258262890683122, 1.000000000000000000, 0.9981185001348090724, 0.9964447847208418585 ) ) 
 REPRESENTATION_ITEM ( '' )  );
#5750 = ORIENTED_EDGE ( 'NONE', *, *, #47538, .T. ) ;
#5751 = VERTEX_POINT ( 'NONE', #24608 ) ;
#5752 = CIRCLE ( 'NONE', #66284, 3.937007874015748143 ) ;
#5753 = CARTESIAN_POINT ( 'NONE',  ( -0.8398950131233589023, -0.6046776061558809534, -0.2411417322834644161 ) ) ;
#5754 = CARTESIAN_POINT ( 'NONE',  ( -0.4724409448818890911, -0.1870078740157480879, -0.4822834645669291653 ) ) ;
#5756 = CARTESIAN_POINT ( 'NONE',  ( -0.8136482939632537770, 0.2306618581243847221, -0.2411417322834647770 ) ) ;
#5755 = CARTESIAN_POINT ( 'NONE',  ( -0.7414698162729651543, -0.5511811023622046335, 0.09757992244046803654 ) ) ;
#5757 = CARTESIAN_POINT ( 'NONE',  ( 0.2690288713910767848, 0.2952755905511811885, 0.1292274648535926551 ) ) ;
#5758 = CARTESIAN_POINT ( 'NONE',  ( -0.5511811023622038563, -0.1870078740157479769, 0.4822834645669291653 ) ) ;
#5759 = CARTESIAN_POINT ( 'NONE',  ( -1.450131233595799651, 0.2952755905511810774, -0.1292274648535930714 ) ) ;
#5760 = CARTESIAN_POINT ( 'NONE',  ( -0.8070866141732276899, -0.5400638737290844871, 0.3530559997133364547 ) ) ;
#5761 = CARTESIAN_POINT ( 'NONE',  ( 0.7939632545931766261, -0.05778040916215522460, 0.4822834645669289988 ) ) ;
#5762 = ADVANCED_FACE ( 'NONE', ( #62093 ), #63407, .F. ) ;
#5763 = CARTESIAN_POINT ( 'NONE',  ( -0.3917322834645671215, 0.1049643490035301469, -1.442257217847769057 ) ) ;
#5764 = CARTESIAN_POINT ( 'NONE',  ( -0.4724409448818890911, -0.1870078740157480601, -0.3641732283464567677 ) ) ;
#5765 = ORIENTED_EDGE ( 'NONE', *, *, #70822, .F. ) ;
#5766 = CARTESIAN_POINT ( 'NONE',  ( 0.3949938075777409963, 2.418639510665530435E-17, -1.535433070866141447 ) ) ;
#5767 = ORIENTED_EDGE ( 'NONE', *, *, #27454, .T. ) ;
#5768 = CARTESIAN_POINT ( 'NONE',  ( -1.253280839895012377, -0.08942795157527998196, 0.3641732283464567121 ) ) ;
#5769 = CARTESIAN_POINT ( 'NONE',  ( -0.9973753280839886548, 0.2306618581243848609, 0.2411417322834645549 ) ) ;
#5770 = CARTESIAN_POINT ( 'NONE',  ( -0.9251968503937002541, -0.5400638737290845981, -0.3530559997133363437 ) ) ;
#5771 = CARTESIAN_POINT ( 'NONE',  ( 0.2925321140481932369, 0.2925321140481932369, -0.2952755905511811330 ) ) ;
#5772 = CARTESIAN_POINT ( 'NONE',  ( -1.200787401574802349, 0.1660481256975883668, -0.3530559997133364547 ) ) ;
#5773 = CARTESIAN_POINT ( 'NONE',  ( -0.8202099737532801971, -0.6692913385826771977, 0.1292274648535927661 ) ) ;
#5774 = CARTESIAN_POINT ( 'NONE',  ( -1.574803149606298192, -0.1870078740157480879, -0.4822834645669291653 ) ) ;
#5775 = FACE_OUTER_BOUND ( 'NONE', #69430, .T. ) ;
#5776 = CARTESIAN_POINT ( 'NONE',  ( 0.3412073490813655186, -0.5023911411419708095, -0.1820866141732282451 ) ) ;
#5777 = PLANE ( 'NONE',  #79402 ) ;
#5778 = CARTESIAN_POINT ( 'NONE',  ( 0.1049643490035303689, 0.3917322834645670104, 0.07939632545931750440 ) ) ;
#5779 = CARTESIAN_POINT ( 'NONE',  ( 0.1968503937007881344, 0.1771653543307087630, 0.000000000000000000 ) ) ;
#5780 = CARTESIAN_POINT ( 'NONE',  ( -0.5446194225721777693, -0.05778040916215522460, 0.4822834645669289988 ) ) ;
#5781 = CARTESIAN_POINT ( 'NONE',  ( 1.200787401574803681, -0.5400638737290845981, -0.3530559997133363437 ) ) ;
#5782 = CARTESIAN_POINT ( 'NONE',  ( -0.5314960629921250401, 0.1660481256975885056, 0.3530559997133364547 ) ) ;
#5783 = ORIENTED_EDGE ( 'NONE', *, *, #78238, .F. ) ;
#5784 = CARTESIAN_POINT ( 'NONE',  ( 0.3996062992125986590, -0.1070741851644053111, -2.158792650918635037 ) ) ;
#5785 = DIRECTION ( 'NONE',  ( 1.000000000000000000, 0.000000000000000000, 0.000000000000000000 ) ) ;
#5786 = ORIENTED_EDGE ( 'NONE', *, *, #51527, .T. ) ;
#5787 = CARTESIAN_POINT ( 'NONE',  ( 0.1070741851644053388, 0.3996062992125986035, -1.645013123359579943 ) ) ;
#5788 = CARTESIAN_POINT ( 'NONE',  ( -0.7217847769028863381, -0.4281496062992124485, 0.4176697321401328655 ) ) ;
#5789 = CARTESIAN_POINT ( 'NONE',  ( 1.253280839895013710, -0.3162353388693405765, 0.4822834645669290543 ) ) ;
#5790 = CARTESIAN_POINT ( 'NONE',  ( -1.076115485564303809, 0.1283753931104748280, 0.1820866141732283561 ) ) ;
#5791 = CARTESIAN_POINT ( 'NONE',  ( -1.423884514435694859, -0.3162353388693405765, 0.4822834645669290543 ) ) ;
#5792 = CARTESIAN_POINT ( 'NONE',  ( 0.1265901696524989462, 0.4724409448818897572, -0.9383202099737533164 ) ) ;
#5793 = DIRECTION ( 'NONE',  ( 0.000000000000000000, 1.000000000000000000, 0.000000000000000000 ) ) ;
#5794 = CARTESIAN_POINT ( 'NONE',  ( 0.1049643490035304938, -0.3917322834645669549, 0.08005249343832024356 ) ) ;
#5795 = CARTESIAN_POINT ( 'NONE',  ( 1.482939632545932307, -0.4281496062992124485, 0.4176697321401328655 ) ) ;
#5796 = CARTESIAN_POINT ( 'NONE',  ( -0.1958661417322836718, 0.3392501089628017219, -2.145013123359580387 ) ) ;
#5797 = CARTESIAN_POINT ( 'NONE',  ( 0.05249343832021075018, -0.6046776061558807314, 0.2411417322834647770 ) ) ;
#5798 = CARTESIAN_POINT ( 'NONE',  ( -0.9055118110236215490, -0.5511811023622047445, 6.969142054262312111E-17 ) ) ;
#5799 = CARTESIAN_POINT ( 'NONE',  ( -0.2427821522309703550, -0.05778040916215560624, -0.4822834645669293319 ) ) ;
#5800 = CARTESIAN_POINT ( 'NONE',  ( 0.2362204724409449064, 0.4091458600556404646, -2.583333333333333481 ) ) ;
#5801 = CARTESIAN_POINT ( 'NONE',  ( -1.023622047244094002, -0.1870078740157480879, -0.4822834645669291653 ) ) ;
#5802 = CARTESIAN_POINT ( 'NONE',  ( -0.7480314960629914633, 0.2952755905511811885, 0.000000000000000000 ) ) ;
#5803 = CARTESIAN_POINT ( 'NONE',  ( -0.1974969037888706924, 0.3420746716998658843, -2.294619422572178102 ) ) ;
#5804 = CARTESIAN_POINT ( 'NONE',  ( 0.6824146981627303710, 0.1283753931104746893, -0.1820866141732285504 ) ) ;
#5805 = CARTESIAN_POINT ( 'NONE',  ( -0.1902887139107604098, -0.5511811023622046335, 0.09757992244046803654 ) ) ;
#5806 = AXIS2_PLACEMENT_3D ( 'NONE', #82537, #44206, #38321 ) ;
#5807 = CARTESIAN_POINT ( 'NONE',  ( 0.7545931758530189937, 0.1771653543307087075, -0.09757992244046823083 ) ) ;
#5808 = CARTESIAN_POINT ( 'NONE',  ( -1.640419947506561060, -0.4281496062992127816, -0.4176697321401328100 ) ) ;
#5809 = CARTESIAN_POINT ( 'NONE',  ( 1.345144356955381593, -0.3162353388693409650, -0.4822834645669289433 ) ) ;
#5810 = CARTESIAN_POINT ( 'NONE',  ( 0.6364829396325465405, -0.2845877964562161244, -0.3641732283464567121 ) ) ;
#5811 = CARTESIAN_POINT ( 'NONE',  ( -0.8005249343832011588, 0.05413385826771626580, -0.4176697321401330321 ) ) ;
#5812 = CARTESIAN_POINT ( 'NONE',  ( 1.246719160104987623, -0.4281496062992124485, 0.4176697321401328655 ) ) ;
#5813 = CARTESIAN_POINT ( 'NONE',  ( 1.090429162302623212, 1.606403293320555813E-17, -0.3627985898453514602 ) ) ;
#5814 = CARTESIAN_POINT ( 'NONE',  ( -0.1246719160104980823, -0.5511811023622048555, -0.09757992244046775898 ) ) ;
#5815 = CARTESIAN_POINT ( 'NONE',  ( 0.1771653543307093182, -0.5400638737290845981, -0.3530559997133363437 ) ) ;
#5816 = CARTESIAN_POINT ( 'NONE',  ( 0.2142011206082509167, 0.2032823926810629067, 0.1316721176867485521 ) ) ;
#5817 = AXIS2_PLACEMENT_3D ( 'NONE', #26960, #54287, #8037 ) ;
#5818 = CARTESIAN_POINT ( 'NONE',  ( 1.318897637795276356, 0.07958543189024071263, -0.2665933059059888421 ) ) ;
#5819 = CARTESIAN_POINT ( 'NONE',  ( -1.279527559055116948, -0.5400638737290844871, 0.3530559997133364547 ) ) ;
#5820 = CARTESIAN_POINT ( 'NONE',  ( -0.4527559055118102749, -0.4536011799217368745, -0.2665933059059886201 ) ) ;
#5821 = CARTESIAN_POINT ( 'NONE',  ( 0.5314960629921349211, 2.716535433070866645, -2.543486866223387377 ) ) ;
#5822 = CARTESIAN_POINT ( 'NONE',  ( -1.141732283464566011, -0.6692913385826771977, 8.415575281601705876E-17 ) ) ;
#5823 = CARTESIAN_POINT ( 'NONE',  ( -0.4855643044619415427, 0.05413385826771626580, -0.4176697321401330321 ) ) ;
#5824 = CARTESIAN_POINT ( 'NONE',  ( 0.3996062992125984925, 0.1070741851644054637, -0.6738845144356955252 ) ) ;
#5825 = CARTESIAN_POINT ( 'NONE',  ( -0.3917322834645671215, 0.1049643490035301469, -2.322178477690288734 ) ) ;
#5826 = CARTESIAN_POINT ( 'NONE',  ( 0.6561679790026253567, 0.1283753931104748280, 0.1820866141732283561 ) ) ;
#5827 = CARTESIAN_POINT ( 'NONE',  ( -0.3543307086614165824, 0.2952755905511811885, 0.000000000000000000 ) ) ;
#5828 = CARTESIAN_POINT ( 'NONE',  ( -0.4986876640419939388, 0.2306618581243847221, -0.2411417322834647770 ) ) ;
#5829 = CARTESIAN_POINT ( 'NONE',  ( -0.6692913385826764205, 0.1771653543307087630, 0.000000000000000000 ) ) ;
#5830 = FACE_OUTER_BOUND ( 'NONE', #54401, .T. ) ;
#5831 = CARTESIAN_POINT ( 'NONE',  ( 0.01312335958005323398, -0.4281496062992127816, -0.4176697321401328100 ) ) ;
#5832 = DIRECTION ( 'NONE',  ( 3.386413887818972582E-16, -0.7071067811865514585, 0.7071067811865435759 ) ) ;
#5833 = CARTESIAN_POINT ( 'NONE',  ( 1.404199475065617264, -0.4281496062992124485, 0.4176697321401328655 ) ) ;
#5834 = CARTESIAN_POINT ( 'NONE',  ( 0.4724409448818905899, -0.1265901696524973641, -0.7414698162729659314 ) ) ;
#5835 = CARTESIAN_POINT ( 'NONE',  ( -0.1049643490035302301, -0.3917322834645671770, -2.116161048065303696 ) ) ;
#5836 = ORIENTED_EDGE ( 'NONE', *, *, #82874, .F. ) ;
#5837 = LINE ( 'NONE', #64334, #33788 ) ;
#5838 = CARTESIAN_POINT ( 'NONE',  ( -1.463254593175852492, -0.6692913385826773087, -0.1292274648535924053 ) ) ;
#5839 = CARTESIAN_POINT ( 'NONE',  ( -0.6955380577427815458, -0.4281496062992127816, -0.4176697321401328100 ) ) ;
#5840 = CARTESIAN_POINT ( 'NONE',  ( -1.614173228346455824, 0.2952755905511811885, 0.000000000000000000 ) ) ;
#5841 = CARTESIAN_POINT ( 'NONE',  ( 0.1958661417322836440, -0.3392501089628017219, -2.066272965879265122 ) ) ;
#5842 = FACE_OUTER_BOUND ( 'NONE', #35715, .T. ) ;
#5843 = CARTESIAN_POINT ( 'NONE',  ( 0.8464566929133866546, -0.5400638737290844871, 0.3530559997133364547 ) ) ;
#5844 = CARTESIAN_POINT ( 'NONE',  ( 0.03280839895013198948, -0.6692913385826773087, -0.1292274648535924053 ) ) ;
#5845 = DIRECTION ( 'NONE',  ( 0.000000000000000000, 0.000000000000000000, -1.000000000000000000 ) ) ;
#5846 = CARTESIAN_POINT ( 'NONE',  ( -0.6496062992125976043, 0.1660481256975883391, -0.3530559997133364547 ) ) ;
#5847 = CARTESIAN_POINT ( 'NONE',  ( 1.292650918635171564, 0.1771653543307087630, 0.09757992244046791164 ) ) ;
#5848 = CARTESIAN_POINT ( 'NONE',  ( 4.893765752498283924E-17, -0.3996062992125986035, -1.181102362204724310 ) ) ;
#5849 = ORIENTED_EDGE ( 'NONE', *, *, #24051, .T. ) ;
#5850 = CARTESIAN_POINT ( 'NONE',  ( 0.1958661417322836440, -0.3392501089628017219, -2.761154855643044304 ) ) ;
#5851 = ORIENTED_EDGE ( 'NONE', *, *, #79270, .T. ) ;
#5852 = CARTESIAN_POINT ( 'NONE',  ( 0.5249343832021003964, 0.2306618581243847221, -0.2411417322834647770 ) ) ;
#5853 = CARTESIAN_POINT ( 'NONE',  ( -0.8070866141732276899, -0.5400638737290844871, 0.3530559997133364547 ) ) ;
#5854 = CARTESIAN_POINT ( 'NONE',  ( -1.384514435695537005, -0.6692913385826773087, -0.1292274648535924053 ) ) ;
#5855 = CARTESIAN_POINT ( 'NONE',  ( 0.4921259842519691285, -0.5400638737290845981, -0.3530559997133363437 ) ) ;
#5856 = AXIS2_PLACEMENT_3D ( 'NONE', #19280, #44931, #6652 ) ;
#5857 = CARTESIAN_POINT ( 'NONE',  ( -1.522309711286088607, -0.5023911411419708095, 0.1820866141732285504 ) ) ;
#5858 = CARTESIAN_POINT ( 'NONE',  ( 1.587926509186352142, 0.05413385826771666132, 0.4176697321401328100 ) ) ;
#5859 = CARTESIAN_POINT ( 'NONE',  ( 8.195543980992789655E-16, -0.1870078740157480879, -0.4822834645669291653 ) ) ;
#5860 = CARTESIAN_POINT ( 'NONE',  ( -1.443569553805773564, 0.2306618581243847221, -0.2411417322834647770 ) ) ;
#5861 = CARTESIAN_POINT ( 'NONE',  ( 1.574803149606299746, -0.1870078740157479769, 0.4822834645669291653 ) ) ;
#5862 = CARTESIAN_POINT ( 'NONE',  ( 0.4117837489889513702, 1.301386200251873682, -2.666378553117691563 ) ) ;
#5863 = CARTESIAN_POINT ( 'NONE',  ( -0.3917322834645670104, -7.196005306013484475E-17, -0.03149606299212594218 ) ) ;
#5864 = CARTESIAN_POINT ( 'NONE',  ( 0.7217847769028878924, -0.004921259842519576551, 0.3153832671262227771 ) ) ;
#5865 = ORIENTED_EDGE ( 'NONE', *, *, #47465, .F. ) ;
#5866 = CARTESIAN_POINT ( 'NONE',  ( -0.3420746716998659953, -0.1974969037888706647, -0.3674540682414698667 ) ) ;
#5867 = ORIENTED_EDGE ( 'NONE', *, *, #17807, .T. ) ;
#5868 = CARTESIAN_POINT ( 'NONE',  ( -0.2296587926509179312, -0.2845877964562161244, -0.3641732283464567121 ) ) ;
#5869 = CARTESIAN_POINT ( 'NONE',  ( 0.1938976377952755792, -0.1938976377952756069, 0.1574803149606299191 ) ) ;
#5870 = CARTESIAN_POINT ( 'NONE',  ( 0.1902887139107617975, 0.2952755905511811885, 0.1292274648535926551 ) ) ;
#5871 = CARTESIAN_POINT ( 'NONE',  ( 0.5643044619422579178, -0.4281496062992127816, -0.4176697321401328100 ) ) ;
#5872 = ADVANCED_FACE ( 'NONE', ( #78018 ), #39702, .F. ) ;
#5873 = CARTESIAN_POINT ( 'NONE',  ( -0.6299212598425188991, -0.1870078740157479769, 0.4822834645669291653 ) ) ;
#5874 = VECTOR ( 'NONE', #57715, 39.37007874015748143 ) ;
#5875 = CARTESIAN_POINT ( 'NONE',  ( 0.2867679344610366554, -0.2867679344610365999, -1.669966822343518897 ) ) ;
#5876 = CARTESIAN_POINT ( 'NONE',  ( -1.227034120734907141, -0.6692913385826773087, -0.1292274648535924053 ) ) ;
#5877 = PRODUCT_DEFINITION ( 'UNKNOWN', '', #73237, #9976 ) ;
#5878 = CARTESIAN_POINT ( 'NONE',  ( -0.3917322834645669549, -0.1049643490035306603, -2.650262467191601079 ) ) ;
#5879 = CARTESIAN_POINT ( 'NONE',  ( 1.207349081364829990, -0.5023911411419708095, -0.1820866141732282451 ) ) ;
#5880 = CARTESIAN_POINT ( 'NONE',  ( 1.017060367454068803, -0.3162353388693405765, 0.4822834645669290543 ) ) ;
#5881 = CARTESIAN_POINT ( 'NONE',  ( 0.9645669291338591078, -0.5400638737290845981, -0.3530559997133363437 ) ) ;
#5882 = CARTESIAN_POINT ( 'NONE',  ( 0.3460692066303959202, 0.1998031496062993295, -0.9186351706036745002 ) ) ;
#5883 = CARTESIAN_POINT ( 'NONE',  ( -1.181102362204723644, -0.1870078740157480879, -0.4822834645669291653 ) ) ;
#5884 = CARTESIAN_POINT ( 'NONE',  ( 0.3996062992125986035, -0.1070741851644052972, -0.1883202099737532054 ) ) ;
#5885 = CARTESIAN_POINT ( 'NONE',  ( 0.3460692066303958092, 0.1998031496062993018, -0.05052493438320212332 ) ) ;
#5886 = CARTESIAN_POINT ( 'NONE',  ( -0.3149606299212590610, -0.1870078740157479769, 0.4822834645669291653 ) ) ;
#5887 = CARTESIAN_POINT ( 'NONE',  ( -0.1998031496062991907, -0.3460692066303959757, -2.900262467191600635 ) ) ;
#5888 =( BOUNDED_CURVE ( )  B_SPLINE_CURVE ( 2, ( #58608, #60281, #32942, #65782, #59859, #77570, #8941, #2631, #46391, #51865, #39674, #72086, #7702 ),
 .UNSPECIFIED., .F., .F. ) 
 B_SPLINE_CURVE_WITH_KNOTS ( ( 3, 2, 2, 2, 2, 2, 3 ),
 ( 0.2125000000000000222, 0.2166666666666667018, 0.2208333333333333537, 0.2250000000000000333, 0.2291666666666666852, 0.2333333333333333648, 0.2375000000000000167 ),
 .UNSPECIFIED. ) 
 CURVE ( )  GEOMETRIC_REPRESENTATION_ITEM ( )  RATIONAL_B_SPLINE_CURVE ( ( 0.9999999999999997780, 0.9659258262890685343, 1.000000000000000000, 0.9659258262890683122, 1.000000000000000000, 0.9659258262890683122, 1.000000000000000000, 0.9659258262890683122, 1.000000000000000000, 0.9659258262890683122, 1.000000000000000000, 0.9659258262890680902, 1.000000000000000222 ) ) 
 REPRESENTATION_ITEM ( '' )  );
#5889 = CARTESIAN_POINT ( 'NONE',  ( 0.1049643490035303689, 0.3917322834645670104, -1.652887139107611425 ) ) ;
#5890 = CARTESIAN_POINT ( 'NONE',  ( 1.089238845144357537, -0.4281496062992124485, 0.4176697321401328655 ) ) ;
#5891 = CARTESIAN_POINT ( 'NONE',  ( 1.338582677165355062, -0.1870078740157479769, 0.4822834645669291653 ) ) ;
#5892 = CARTESIAN_POINT ( 'NONE',  ( 0.3412073490813655186, -0.5023911411419708095, -0.1820866141732282451 ) ) ;
#5893 = CARTESIAN_POINT ( 'NONE',  ( 0.9120734908136489683, -0.6692913385826771977, 0.1292274648535927661 ) ) ;
#5894 = CARTESIAN_POINT ( 'NONE',  ( 0.1265901696524989462, 0.4724409448818897572, -1.487532808398950301 ) ) ;
#5895 = CARTESIAN_POINT ( 'NONE',  ( 0.4527559055118117182, 0.07958543189024071263, -0.2665933059059888421 ) ) ;
#5896 = EDGE_CURVE ( 'NONE', #82375, #62933, #50042, .T. ) ;
#5897 = CARTESIAN_POINT ( 'NONE',  ( 0.4986876640419954376, 0.2306618581243848609, 0.2411417322834645549 ) ) ;
#5898 = CARTESIAN_POINT ( 'NONE',  ( -0.3949938075777411073, 0.1058382717557497660, -0.8969816272965878134 ) ) ;
#5899 = CARTESIAN_POINT ( 'NONE',  ( -0.7611548556430438595, 0.2306618581243848609, 0.2411417322834645549 ) ) ;
#5900 = CARTESIAN_POINT ( 'NONE',  ( 0.9186351706036751663, -0.5023911411419708095, 0.1820866141732285504 ) ) ;
#5901 = EDGE_CURVE ( 'NONE', #68517, #51509, #31698, .T. ) ;
#5902 = CARTESIAN_POINT ( 'NONE',  ( -2.630268417803964809, 1.724409448818898127, -0.4359958488159723089 ) ) ;
#5903 = CARTESIAN_POINT ( 'NONE',  ( -0.1312335958005241554, 0.2306618581243848609, 0.2411417322834645549 ) ) ;
#5904 = CARTESIAN_POINT ( 'NONE',  ( 0.2165354330708668673, -0.4536011799217367080, 0.2665933059059888421 ) ) ;
#5905 = CARTESIAN_POINT ( 'NONE',  ( -2.723203318070452017, 1.231544801320239024, 0.3638227417423900434 ) ) ;
#5906 = CARTESIAN_POINT ( 'NONE',  ( -0.3149606299212590610, -0.1870078740157479769, 0.4822834645669291653 ) ) ;
#5907 = CARTESIAN_POINT ( 'NONE',  ( 0.5118110236220478892, 0.1771653543307087630, 0.000000000000000000 ) ) ;
#5908 = CARTESIAN_POINT ( 'NONE',  ( -0.3996062992125986590, 0.1070741851644051723, -2.156824146981627166 ) ) ;
#5909 = CARTESIAN_POINT ( 'NONE',  ( -0.1771653543307080136, 0.1660481256975883668, -0.3530559997133364547 ) ) ;
#5910 = CARTESIAN_POINT ( 'NONE',  ( 1.030183727034121421, -0.08942795157527998196, 0.3641732283464567121 ) ) ;
#5911 = CARTESIAN_POINT ( 'NONE',  ( 0.2099737532808405305, 0.2306618581243847221, -0.2411417322834647770 ) ) ;
#5912 = CARTESIAN_POINT ( 'NONE',  ( -0.2230971128608915943, -0.3690944881889765550, -0.3153832671262227771 ) ) ;
#5913 = CARTESIAN_POINT ( 'NONE',  ( -0.7545931758530177724, 0.1771653543307087630, 0.09757992244046791164 ) ) ;
#5914 = CARTESIAN_POINT ( 'NONE',  ( -0.1902887139107604098, 0.2952755905511810774, -0.1292274648535930714 ) ) ;
#5915 = CARTESIAN_POINT ( 'NONE',  ( 0.08530183727034192087, -0.3162353388693409650, -0.4822834645669289433 ) ) ;
#5916 = CARTESIAN_POINT ( 'NONE',  ( 1.017060367454068803, -0.2845877964562159024, 0.3641732283464567677 ) ) ;
#5917 = CARTESIAN_POINT ( 'NONE',  ( 0.3564806704966359541, 1.223997042866947993, -1.063963581927926283 ) ) ;
#5918 = CARTESIAN_POINT ( 'NONE',  ( 1.522309711286089939, -0.5023911411419708095, -0.1820866141732282451 ) ) ;
#5919 = AXIS2_PLACEMENT_3D ( 'NONE', #1142, #19644, #27208 ) ;
#5920 = EDGE_CURVE ( 'NONE', #57945, #32176, #21821, .T. ) ;
#5921 = CARTESIAN_POINT ( 'NONE',  ( 0.8333333333333340365, -0.6692913385826771977, 0.1292274648535927661 ) ) ;
#5922 = CARTESIAN_POINT ( 'NONE',  ( 0.3336463653988042677, 1.199832043049261721, -1.973860402524058255 ) ) ;
#5923 = CARTESIAN_POINT ( 'NONE',  ( -0.3937007874015740483, -0.1870078740157480879, -0.4822834645669291653 ) ) ;
#5924 = CARTESIAN_POINT ( 'NONE',  ( 0.1049643490035304938, -0.3917322834645669549, -0.7998687664041995715 ) ) ;
#5925 = CARTESIAN_POINT ( 'NONE',  ( 0.7677165354330716118, 0.1660481256975883668, -0.3530559997133364547 ) ) ;
#5926 = CARTESIAN_POINT ( 'NONE',  ( 0.7217847769028878924, 0.05413385826771666132, 0.4176697321401328100 ) ) ;
#5927 = CARTESIAN_POINT ( 'NONE',  ( -0.3133043865842751186, 1.179792816808425737, -3.924584650684677101 ) ) ;
#5928 = CARTESIAN_POINT ( 'NONE',  ( 0.5314960629921267055, -0.4536011799217367080, 0.2665933059059888421 ) ) ;
#5929 = CARTESIAN_POINT ( 'NONE',  ( 1.174540682414699111, -0.3162353388693405765, 0.4822834645669290543 ) ) ;
#5930 = EDGE_CURVE ( 'NONE', #47146, #19860, #59885, .T. ) ;
#5931 = CARTESIAN_POINT ( 'NONE',  ( -0.1706036745406816491, -0.3690944881889763329, 0.3153832671262228327 ) ) ;
#5932 = VECTOR ( 'NONE', #55530, 39.37007874015748143 ) ;
#5933 = CARTESIAN_POINT ( 'NONE',  ( -0.3215223097112853146, -0.05778040916215560624, -0.4822834645669293319 ) ) ;
#5934 = DIRECTION ( 'NONE',  ( 0.000000000000000000, 0.000000000000000000, 1.000000000000000000 ) ) ;
#5935 = CARTESIAN_POINT ( 'NONE',  ( 0.3215223097112867578, -0.05778040916215522460, 0.4822834645669289988 ) ) ;
#5936 = CARTESIAN_POINT ( 'NONE',  ( -0.9448818897637790704, -0.1870078740157480879, -0.4822834645669291653 ) ) ;
#5937 = CARTESIAN_POINT ( 'NONE',  ( -0.8595800524934373854, -0.2845877964562161244, -0.3641732283464567121 ) ) ;
#5938 = CARTESIAN_POINT ( 'NONE',  ( 0.5708661417322841158, -0.5400638737290845981, -0.3530559997133363437 ) ) ;
#5939 = CARTESIAN_POINT ( 'NONE',  ( -1.404199475065615932, 0.05413385826771666132, 0.4176697321401328100 ) ) ;
#5940 = CARTESIAN_POINT ( 'NONE',  ( -0.5577427821522301654, -0.3162353388693405765, 0.4822834645669290543 ) ) ;
#5941 = ADVANCED_FACE ( 'NONE', ( #19933 ), #46836, .F. ) ;
#5942 =( NAMED_UNIT ( * ) SI_UNIT ( $, .STERADIAN. ) SOLID_ANGLE_UNIT ( ) );
#5944 = CARTESIAN_POINT ( 'NONE',  ( 1.233595800524935227, -0.6046776061558807314, 0.2411417322834647770 ) ) ;
#5943 = DIRECTION ( 'NONE',  ( 0.000000000000000000, 1.000000000000000000, 0.000000000000000000 ) ) ;
#5945 = CARTESIAN_POINT ( 'NONE',  ( 1.318897637795276356, -0.5400638737290844871, 0.3530559997133364547 ) ) ;
#5946 = CARTESIAN_POINT ( 'NONE',  ( -0.3726288332202236653, -0.1208384647423932784, -1.929133858267952473 ) ) ;
#5947 = CARTESIAN_POINT ( 'NONE',  ( -1.614173228346455824, 0.2952755905511811885, 0.000000000000000000 ) ) ;
#5948 = CARTESIAN_POINT ( 'NONE',  ( -1.010498687664041384, -0.4281496062992127816, -0.4176697321401328100 ) ) ;
#5949 = CARTESIAN_POINT ( 'NONE',  ( 0.1265901696524989462, 0.4724409448818897572, -0.3083989501312335846 ) ) ;
#5950 = CARTESIAN_POINT ( 'NONE',  ( 0.3420746716998659953, 0.1974969037888705536, -2.650918635170603554 ) ) ;
#5951 = VERTEX_POINT ( 'NONE', #45582 ) ;
#5952 = CARTESIAN_POINT ( 'NONE',  ( -0.07874015748031421014, -0.1870078740157479769, 0.3641732283464567677 ) ) ;
#5953 = CARTESIAN_POINT ( 'NONE',  ( 0.1958661417322836440, -0.3392501089628017219, -1.186351706036745446 ) ) ;
#5954 = CARTESIAN_POINT ( 'NONE',  ( 0.6627296587926515548, 0.2952755905511811885, 0.1292274648535926551 ) ) ;
#5955 = DIRECTION ( 'NONE',  ( 0.7071067811865454633, 0.000000000000000000, 0.7071067811865495711 ) ) ;
#5956 = CARTESIAN_POINT ( 'NONE',  ( -1.604771003085130765, 0.4934440724007105872, 0.1466069496707737840 ) ) ;
#5957 = CARTESIAN_POINT ( 'NONE',  ( -0.6561679790026240244, 0.1283753931104746893, -0.1820866141732285504 ) ) ;
#5958 = DIRECTION ( 'NONE',  ( 0.000000000000000000, 1.000000000000000000, 0.000000000000000000 ) ) ;
#5959 = CARTESIAN_POINT ( 'NONE',  ( 0.9908136482939640111, -0.6692913385826771977, 0.1292274648535927661 ) ) ;
#5960 = CARTESIAN_POINT ( 'NONE',  ( 1.128608923884514947, 0.1283753931104748280, 0.1820866141732283561 ) ) ;
#5961 = CARTESIAN_POINT ( 'NONE',  ( 0.05905511811023709395, -0.5400638737290844871, 0.3530559997133364547 ) ) ;
#5962 = CARTESIAN_POINT ( 'NONE',  ( -0.1049643490035301746, -0.3917322834645670659, -0.6246526002286596491 ) ) ;
#5963 = CARTESIAN_POINT ( 'NONE',  ( -0.3215223097112853146, -0.05778040916215560624, -0.4822834645669293319 ) ) ;
#5964 = CARTESIAN_POINT ( 'NONE',  ( -1.522309711286088607, 0.1283753931104746893, -0.1820866141732285504 ) ) ;
#5965 = CARTESIAN_POINT ( 'NONE',  ( -0.4133858267716528645, 0.1660481256975883668, -0.3530559997133364547 ) ) ;
#5966 = CARTESIAN_POINT ( 'NONE',  ( 1.581364829396326277, -0.3162353388693409650, -0.4822834645669289433 ) ) ;
#5967 = B_SPLINE_CURVE_WITH_KNOTS ( 'NONE', 3,
 ( #44372, #70064, #32181, #70908 ),
 .UNSPECIFIED., .F., .F.,
 ( 4, 4 ),
 ( 0.03467931754515478360, 0.03492726069669743055 ),
 .UNSPECIFIED. ) ;
#5968 = CARTESIAN_POINT ( 'NONE',  ( -0.5314960629921325896, 2.729653112494254685, 1.868118600343975588 ) ) ;
#5969 = VERTEX_POINT ( 'NONE', #1003 ) ;
#5970 = CARTESIAN_POINT ( 'NONE',  ( 0.3392501089628018884, -0.1958661417322833942, -1.991489132054804934 ) ) ;
#5971 = CARTESIAN_POINT ( 'NONE',  ( 0.3608923884514443348, -0.6692913385826771977, 0.1292274648535927661 ) ) ;
#5972 = ORIENTED_EDGE ( 'NONE', *, *, #23961, .T. ) ;
#5973 = CARTESIAN_POINT ( 'NONE',  ( -0.6167979002624665030, 0.05413385826771666132, 0.4176697321401328100 ) ) ;
#5974 = CARTESIAN_POINT ( 'NONE',  ( -1.318897637795274802, 0.1660481256975885056, 0.3530559997133364547 ) ) ;
#5975 = CARTESIAN_POINT ( 'NONE',  ( 0.6299212598425204535, -0.1870078740157479769, 0.4822834645669291653 ) ) ;
#5976 = CARTESIAN_POINT ( 'NONE',  ( -0.1049868766404193215, -0.6046776061558807314, 0.2411417322834647770 ) ) ;
#5977 = CARTESIAN_POINT ( 'NONE',  ( -0.3392501089628017219, -0.1958661417322836718, -1.239501312335958172 ) ) ;
#5978 = CARTESIAN_POINT ( 'NONE',  ( -0.7152230971128602510, -0.05778040916215560624, -0.4822834645669293319 ) ) ;
#5979 = CARTESIAN_POINT ( 'NONE',  ( -0.2230971128608915943, 0.05413385826771666132, 0.4176697321401328100 ) ) ;
#5980 = CARTESIAN_POINT ( 'NONE',  ( -1.043307086614172041, -0.5400638737290844871, 0.3530559997133364547 ) ) ;
#5981 =( GEOMETRIC_REPRESENTATION_CONTEXT ( 3 ) GLOBAL_UNCERTAINTY_ASSIGNED_CONTEXT ( ( #3247 ) ) GLOBAL_UNIT_ASSIGNED_CONTEXT ( ( #79023, #60050, #39867 ) ) REPRESENTATION_CONTEXT ( 'NONE', 'WORKASPACE' ) );
#5982 = CARTESIAN_POINT ( 'NONE',  ( -0.2624671916010490880, -0.5023911411419708095, 0.1820866141732285504 ) ) ;
#5983 = CARTESIAN_POINT ( 'NONE',  ( -0.004548682155566147710, 0.3974711515625344305, 1.060393565926956833E-17 ) ) ;
#5984 = CARTESIAN_POINT ( 'NONE',  ( 0.1115485564304467270, -0.6692913385826773087, -0.1292274648535924053 ) ) ;
#5985 = DIRECTION ( 'NONE',  ( -0.000000000000000000, -1.000000000000000000, -0.000000000000000000 ) ) ;
#5986 = CARTESIAN_POINT ( 'NONE',  ( 1.240157480314961314, -0.5400638737290844871, 0.3530559997133364547 ) ) ;
#5987 = CARTESIAN_POINT ( 'NONE',  ( 0.1049643490035303689, 0.3917322834645670104, -2.820209973753280419 ) ) ;
#5988 = ORIENTED_EDGE ( 'NONE', *, *, #1342, .T. ) ;
#5989 = VERTEX_POINT ( 'NONE', #7299 ) ;
#5990 = CARTESIAN_POINT ( 'NONE',  ( 0.1246719160104994284, 0.2952755905511810774, -0.1292274648535930714 ) ) ;
#5991 = CARTESIAN_POINT ( 'NONE',  ( -0.01312335958005186876, -0.3690944881889763329, 0.3153832671262228327 ) ) ;
#5993 = FACE_OUTER_BOUND ( 'NONE', #26791, .T. ) ;
#5992 = CARTESIAN_POINT ( 'NONE',  ( 1.620734908136483465, -0.5511811023622046335, 0.09757992244046803654 ) ) ;
#5994 = CARTESIAN_POINT ( 'NONE',  ( 0.2867679344610365999, 0.2867679344610365999, -1.167322834645669438 ) ) ;
#5995 = CARTESIAN_POINT ( 'NONE',  ( 0.4091458600556403535, 0.2362204724409449896, -0.3654855643044619407 ) ) ;
#5996 = CARTESIAN_POINT ( 'NONE',  ( 1.489501312335958172, -0.2845877964562159024, 0.3641732283464567677 ) ) ;
#5997 = EDGE_CURVE ( 'NONE', #76797, #34953, #68869, .T. ) ;
#5998 = CARTESIAN_POINT ( 'NONE',  ( -1.633858267716534529, 0.1660481256975885056, 0.3530559997133364547 ) ) ;
#5999 = AXIS2_PLACEMENT_3D ( 'NONE', #65318, #14396, #38786 ) ;
#6000 = CARTESIAN_POINT ( 'NONE',  ( 0.2891555358219910499, -0.2891555358219909944, 0.1397637795275590844 ) ) ;
#6001 = CARTESIAN_POINT ( 'NONE',  ( 0.5774278215223103139, -0.6046776061558809534, -0.2411417322834644161 ) ) ;
#6002 = CARTESIAN_POINT ( 'NONE',  ( -1.102362204724408601, -0.1870078740157480879, -0.4822834645669291653 ) ) ;
#6003 = CARTESIAN_POINT ( 'NONE',  ( -1.286089238845143479, -0.6046776061558807314, 0.2411417322834647770 ) ) ;
#6004 = CARTESIAN_POINT ( 'NONE',  ( 0.2296587926509192634, -0.05778040916215560624, -0.4822834645669293319 ) ) ;
#6005 = CARTESIAN_POINT ( 'NONE',  ( 1.069553805774278610, -0.6692913385826771977, 0.1292274648535927661 ) ) ;
#6006 = CARTESIAN_POINT ( 'NONE',  ( 1.443569553805774897, -0.5023911411419708095, -0.1820866141732282451 ) ) ;
#6007 = ITEM_DEFINED_TRANSFORMATION ( 'NONE', 'NONE', #38301,  #22098 ) ;
#6008 = CARTESIAN_POINT ( 'NONE',  ( 0.9514435695538062676, -0.2845877964562161244, -0.3641732283464567121 ) ) ;
#6009 = CARTESIAN_POINT ( 'NONE',  ( -0.9186351706036736120, -0.6046776061558809534, -0.2411417322834644161 ) ) ;
#6010 = CARTESIAN_POINT ( 'NONE',  ( -0.3996062992125986590, 0.1070741851644051723, -0.4245406824146981672 ) ) ;
#6011 = CARTESIAN_POINT ( 'NONE',  ( -1.627296587926508442, 0.1283753931104748280, 0.1820866141732283561 ) ) ;
#6012 = CARTESIAN_POINT ( 'NONE',  ( 0.2867679344610365999, 0.2867679344610365999, -0.4448818897637794589 ) ) ;
#6014 = CARTESIAN_POINT ( 'NONE',  ( -0.06791843738634079086, 1.067571514150118084, 1.854636000526581840 ) ) ;
#6013 = CARTESIAN_POINT ( 'NONE',  ( 0.7808398950131241190, -0.05778040916215560624, -0.4822834645669293319 ) ) ;
#6015 = CARTESIAN_POINT ( 'NONE',  ( -1.666666666666665853, -0.004921259842519870586, -0.3153832671262229437 ) ) ;
#6016 = CARTESIAN_POINT ( 'NONE',  ( 0.03280839895013198948, -0.6692913385826773087, -0.1292274648535924053 ) ) ;
#6017 = CARTESIAN_POINT ( 'NONE',  ( 0.9448818897637802916, -0.1870078740157479769, 0.3641732283464567677 ) ) ;
#6018 = CARTESIAN_POINT ( 'NONE',  ( 0.8202099737532814183, -0.6692913385826773087, -0.1292274648535924053 ) ) ;
#6019 = FACE_OUTER_BOUND ( 'NONE', #57602, .T. ) ;
#6020 = CARTESIAN_POINT ( 'NONE',  ( -0.3608923884514428360, -0.5511811023622048555, -0.09757992244046775898 ) ) ;
#6021 = CARTESIAN_POINT ( 'NONE',  ( -0.5774278215223089816, 0.2306618581243847221, -0.2411417322834647770 ) ) ;
#6022 = CARTESIAN_POINT ( 'NONE',  ( 1.594488188976378673, -0.5400638737290845981, -0.3530559997133363437 ) ) ;
#6023 = CARTESIAN_POINT ( 'NONE',  ( -1.312335958005248715, -0.6046776061558809534, -0.2411417322834644161 ) ) ;
#6024 = CARTESIAN_POINT ( 'NONE',  ( 1.089238845144357759, 0.05413385826771626580, -0.4176697321401330321 ) ) ;
#6025 = CARTESIAN_POINT ( 'NONE',  ( 0.1049643490035304799, -0.3917322834645670104, -1.026922202920946825 ) ) ;
#6026 = B_SPLINE_CURVE_WITH_KNOTS ( 'NONE', 3,
 ( #57440, #70078, #25868, #12431 ),
 .UNSPECIFIED., .F., .F.,
 ( 4, 4 ),
 ( 0.0005422360305776403313, 0.001226984380451624388 ),
 .UNSPECIFIED. ) ;
#6027 = CARTESIAN_POINT ( 'NONE',  ( -1.135170603674539924, 0.1771653543307087075, -0.09757992244046823083 ) ) ;
#6028 = CARTESIAN_POINT ( 'NONE',  ( 2.586063147568535836, 1.653225543546883891, 0.4603267246303527904 ) ) ;
#6029 = CARTESIAN_POINT ( 'NONE',  ( 0.9186351706036751663, -0.6046776061558807314, 0.2411417322834647770 ) ) ;
#6030 = CARTESIAN_POINT ( 'NONE',  ( 0.4091458600556403535, 0.2362204724409449896, -2.255249343832020692 ) ) ;
#6031 = CARTESIAN_POINT ( 'NONE',  ( -1.528871391076114250, 0.2952755905511810774, -0.1292274648535930714 ) ) ;
#6032 = CARTESIAN_POINT ( 'NONE',  ( 1.653543307086614789, -0.1870078740157479769, 0.4822834645669291653 ) ) ;
#6033 = CARTESIAN_POINT ( 'NONE',  ( -0.8858267716535425107, 0.07958543189024071263, -0.2665933059059888421 ) ) ;
#6034 = CARTESIAN_POINT ( 'NONE',  ( 1.653543307086614789, -0.1870078740157479769, 0.3641732283464567677 ) ) ;
#6035 = CARTESIAN_POINT ( 'NONE',  ( -0.5971128608923877978, -0.6692913385826773087, -0.1292274648535924053 ) ) ;
#6036 = CARTESIAN_POINT ( 'NONE',  ( -0.5446194225721777693, -0.08942795157527998196, 0.3641732283464567121 ) ) ;
#6037 = CARTESIAN_POINT ( 'NONE',  ( -1.666666666666665853, -0.004921259842519870586, -0.3153832671262229437 ) ) ;
#6038 = CARTESIAN_POINT ( 'NONE',  ( 1.128608923884514947, 0.1283753931104748280, 0.1820866141732283561 ) ) ;
#6039 = CARTESIAN_POINT ( 'NONE',  ( 0.7742782152230979209, 0.05413385826771626580, -0.4176697321401330321 ) ) ;
#6040 = CARTESIAN_POINT ( 'NONE',  ( 1.594488188976378673, 0.1660481256975885056, 0.3530559997133364547 ) ) ;
#6041 = CARTESIAN_POINT ( 'NONE',  ( -0.06561679790026180015, -0.004921259842519576551, 0.3153832671262227771 ) ) ;
#6042 = AXIS2_PLACEMENT_3D ( 'NONE', #26712, #27958, #6935 ) ;
#6043 = CARTESIAN_POINT ( 'NONE',  ( 0.3871391076115493490, -0.3162353388693405765, 0.4822834645669290543 ) ) ;
#6044 = CARTESIAN_POINT ( 'NONE',  ( 0.3805774278215230400, -0.004921259842519870586, -0.3153832671262229437 ) ) ;
#6045 = CARTESIAN_POINT ( 'NONE',  ( 1.587926509186352142, 0.05413385826771666132, 0.4176697321401328100 ) ) ;
#6046 = CARTESIAN_POINT ( 'NONE',  ( -1.358267716535432434, -0.5400638737290844871, 0.3530559997133364547 ) ) ;
#6047 = CARTESIAN_POINT ( 'NONE',  ( -0.4527559055118102749, 0.1660481256975885056, 0.3530559997133364547 ) ) ;
#6048 = CARTESIAN_POINT ( 'NONE',  ( 0.1998031496062992740, 0.3460692066303959757, -0.4593175853018372501 ) ) ;
#6049 = CARTESIAN_POINT ( 'NONE',  ( -0.3996062992125985480, -7.340648628747423112E-17, -2.478346456692913868 ) ) ;
#6050 = CARTESIAN_POINT ( 'NONE',  ( 0.6299212598425204535, -0.1870078740157479769, 0.4822834645669291653 ) ) ;
#6051 = CARTESIAN_POINT ( 'NONE',  ( 1.095800524934383846, -0.2845877964562159024, 0.3641732283464567677 ) ) ;
#6052 = CARTESIAN_POINT ( 'NONE',  ( -0.4921259842519677963, 0.1660481256975883668, -0.3530559997133364547 ) ) ;
#6053 = CARTESIAN_POINT ( 'NONE',  ( 0.2034120734908142214, 0.2952755905511810774, -0.1292274648535930714 ) ) ;
#6054 = CARTESIAN_POINT ( 'NONE',  ( -0.1070741851644056997, 0.3996062992125986035, -2.211286089238845065 ) ) ;
#6055 = AXIS2_PLACEMENT_3D ( 'NONE', #41101, #74340, #73517 ) ;
#6056 = CARTESIAN_POINT ( 'NONE',  ( -0.1058382717557497937, -0.3949938075777411628, -1.489501312335957950 ) ) ;
#6057 = CARTESIAN_POINT ( 'NONE',  ( 0.1070741851644053527, 0.3996062992125986590, -2.828083989501312345 ) ) ;
#6058 = CARTESIAN_POINT ( 'NONE',  ( 3.908721163486909234, 1.601505345183718676, 0.4711385086307711689 ) ) ;
#6059 = CARTESIAN_POINT ( 'NONE',  ( -9.594673741351313045E-17, 0.3917322834645670104, -0.6220472440944880832 ) ) ;
#6060 = CARTESIAN_POINT ( 'NONE',  ( -0.5643044619422565855, -0.004921259842519870586, -0.3153832671262229437 ) ) ;
#6061 = CARTESIAN_POINT ( 'NONE',  ( -1.076115485564303809, 0.2306618581243848609, 0.2411417322834645549 ) ) ;
#6062 = CARTESIAN_POINT ( 'NONE',  ( -0.3949938075777411073, 0.1058382717557497660, -2.471784776902887337 ) ) ;
#6063 = CARTESIAN_POINT ( 'NONE',  ( 0.9448818897637802916, -0.1870078740157480879, -0.4822834645669291653 ) ) ;
#6064 = CARTESIAN_POINT ( 'NONE',  ( 1.167979002624672580, 0.05413385826771626580, -0.4176697321401330321 ) ) ;
#6065 = CARTESIAN_POINT ( 'NONE',  ( 0.6102362204724416372, -0.5400638737290844871, 0.3530559997133364547 ) ) ;
#6066 = CARTESIAN_POINT ( 'NONE',  ( 0.3458507752293908943, 0.3458507752293908943, -2.657480314960630530 ) ) ;
#6067 = CARTESIAN_POINT ( 'NONE',  ( -0.1998031496062994683, 0.3460692066303958092, -2.375328083989501238 ) ) ;
#6068 = CARTESIAN_POINT ( 'NONE',  ( 0.000000000000000000, 0.000000000000000000, -2.755905511811024056 ) ) ;
#6069 = CARTESIAN_POINT ( 'NONE',  ( 0.6627296587926515548, 0.2952755905511811885, 0.1292274648535926551 ) ) ;
#6070 = CARTESIAN_POINT ( 'NONE',  ( 0.7349081364829402885, -0.6046776061558809534, -0.2411417322834644161 ) ) ;
#6071 = CARTESIAN_POINT ( 'NONE',  ( 0.8792650918635177559, -0.3690944881889765550, -0.3153832671262227771 ) ) ;
#6072 = CARTESIAN_POINT ( 'NONE',  ( 1.384514435695538559, 0.2952755905511810774, -0.1292274648535930714 ) ) ;
#6073 = CARTESIAN_POINT ( 'NONE',  ( -0.1049643490035307020, 0.3917322834645669549, 0.06627296587926499727 ) ) ;
#6074 = CARTESIAN_POINT ( 'NONE',  ( 0.3937007874015754361, -0.1870078740157480879, -0.4822834645669291653 ) ) ;
#6075 = CARTESIAN_POINT ( 'NONE',  ( 1.246719160104987623, 0.05413385826771626580, -0.4176697321401330321 ) ) ;
#6076 = CARTESIAN_POINT ( 'NONE',  ( 0.5643044619422579178, 0.05413385826771666132, 0.4176697321401328100 ) ) ;
#6077 = CARTESIAN_POINT ( 'NONE',  ( -0.7426113562972006532, 2.209901789876323797, -0.5309055118110235227 ) ) ;
#6078 = CARTESIAN_POINT ( 'NONE',  ( -0.8792650918635160906, 0.05413385826771626580, -0.4176697321401330321 ) ) ;
#6079 = CARTESIAN_POINT ( 'NONE',  ( -0.9448818897637790704, -0.1870078740157479769, 0.4822834645669291653 ) ) ;
#6080 = CARTESIAN_POINT ( 'NONE',  ( 1.318897637795276356, 0.1660481256975883668, -0.3530559997133364547 ) ) ;
#6081 = CARTESIAN_POINT ( 'NONE',  ( 0.3917322834645670104, -0.1049643490035303411, -0.6686351706036747222 ) ) ;
#6082 = CARTESIAN_POINT ( 'NONE',  ( 0.3917322834645669549, 0.1049643490035304660, -1.376640419947506189 ) ) ;
#6083 = CARTESIAN_POINT ( 'NONE',  ( -0.1958661417322836718, 0.3392501089628017219, -2.682414698162729483 ) ) ;
#6084 = ORIENTED_EDGE ( 'NONE', *, *, #80096, .F. ) ;
#6085 = CARTESIAN_POINT ( 'NONE',  ( -0.3996062992125986035, -7.340648628747425578E-17, -0.1968503937007874405 ) ) ;
#6086 = ORIENTED_EDGE ( 'NONE', *, *, #79452, .T. ) ;
#6087 = CARTESIAN_POINT ( 'NONE',  ( 0.4177787735906999811, 1.312623414240995157, -1.714017618091133288 ) ) ;
#6088 = CARTESIAN_POINT ( 'NONE',  ( 1.377952755905512472, -0.5511811023622047445, 6.969142054262312111E-17 ) ) ;
#6089 = CARTESIAN_POINT ( 'NONE',  ( 0.3460692066303959757, -0.1998031496062991907, -1.522309711286089273 ) ) ;
#6090 = CARTESIAN_POINT ( 'NONE',  ( 1.220472440944882608, 0.1771653543307087630, 0.000000000000000000 ) ) ;
#6091 = CARTESIAN_POINT ( 'NONE',  ( 0.4724409448818898682, 2.892866454678787531E-17, -2.399606299212598604 ) ) ;
#6092 = CARTESIAN_POINT ( 'NONE',  ( 0.000000000000000000, 2.755905511811024056, 0.000000000000000000 ) ) ;
#6093 = CARTESIAN_POINT ( 'NONE',  ( 0.2362204724409449064, 0.000000000000000000, 0.1968503937007874405 ) ) ;
#6094 = CARTESIAN_POINT ( 'NONE',  ( -0.3392501089628019995, 0.1958661417322832277, -0.7408136482939633449 ) ) ;
#6095 = ADVANCED_FACE ( 'NONE', ( #52311 ), #1414, .F. ) ;
#6096 = CARTESIAN_POINT ( 'NONE',  ( -0.6167979002624665030, -0.3690944881889765550, -0.3153832671262227771 ) ) ;
#6097 = CARTESIAN_POINT ( 'NONE',  ( -1.463254593175852492, -0.5511811023622048555, -0.09757992244046775898 ) ) ;
#6098 = CARTESIAN_POINT ( 'NONE',  ( -1.325459317585300889, 0.05413385826771666132, 0.4176697321401328100 ) ) ;
#6099 = CARTESIAN_POINT ( 'NONE',  ( 0.07874015748031558404, -0.1870078740157480879, -0.4822834645669291653 ) ) ;
#6100 = CARTESIAN_POINT ( 'NONE',  ( -1.581364829396324945, -0.05778040916215560624, -0.4822834645669293319 ) ) ;
#6101 = VERTEX_POINT ( 'NONE', #48079 ) ;
#6102 = PLANE ( 'NONE',  #27217 ) ;
#6103 = DIRECTION ( 'NONE',  ( 0.000000000000000000, 1.000000000000000000, 0.000000000000000000 ) ) ;
#6104 = CARTESIAN_POINT ( 'NONE',  ( -0.4091458600556405756, 0.2362204724409446288, -1.916010498687664043 ) ) ;
#6105 = CARTESIAN_POINT ( 'NONE',  ( -1.595398199321656385, 1.564277624879635509, 0.1559797534342483860 ) ) ;
#6106 = CARTESIAN_POINT ( 'NONE',  ( -0.4658792650918627265, -0.2845877964562161244, -0.3641732283464567121 ) ) ;
#6107 = CARTESIAN_POINT ( 'NONE',  ( -1.128608923884513837, 0.2306618581243847221, -0.2411417322834647770 ) ) ;
#6108 = CARTESIAN_POINT ( 'NONE',  ( 1.056430446194226658, 0.2952755905511811885, 0.1292274648535926551 ) ) ;
#6109 = AXIS2_PLACEMENT_3D ( 'NONE', #66614, #8951, #63175 ) ;
#6110 = EDGE_LOOP ( 'NONE', ( #77754, #42485, #48014, #57282 ) ) ;
#6112 = CARTESIAN_POINT ( 'NONE',  ( 1.348312163386739426, 0.2755905511811023723, 0.7386866130305692613 ) ) ;
#6111 = CARTESIAN_POINT ( 'NONE',  ( -1.614173228346457378, 0.5038684218300933937, -0.1372047244094477536 ) ) ;
#6113 = CARTESIAN_POINT ( 'NONE',  ( 1.076115485564305141, 0.2306618581243847221, -0.2411417322834647770 ) ) ;
#6114 = CARTESIAN_POINT ( 'NONE',  ( -1.135170603674539924, -0.6692913385826771977, 0.1292274648535927661 ) ) ;
#6115 = CARTESIAN_POINT ( 'NONE',  ( 4.797336870675655290E-17, -0.3917322834645669549, -0.6312142800186859581 ) ) ;
#6116 = CARTESIAN_POINT ( 'NONE',  ( -0.5052493438320203589, -0.5511811023622046335, 0.09757992244046803654 ) ) ;
#6117 = CARTESIAN_POINT ( 'NONE',  ( -0.3917322834645671215, 0.1049643490035301469, -0.9048556430446195176 ) ) ;
#6118 = CARTESIAN_POINT ( 'NONE',  ( -0.7020997375328074108, -0.08942795157527998196, 0.3641732283464567121 ) ) ;
#6119 = CARTESIAN_POINT ( 'NONE',  ( -0.08530183727034056085, -0.08942795157528024563, -0.3641732283464568787 ) ) ;
#6120 = CARTESIAN_POINT ( 'NONE',  ( 5.463695987328526437E-16, -0.1870078740157479769, 0.4822834645669291653 ) ) ;
#6121 = CARTESIAN_POINT ( 'NONE',  ( -0.8267716535433065062, 0.1771653543307087630, 0.000000000000000000 ) ) ;
#6122 = CARTESIAN_POINT ( 'NONE',  ( -0.1958661417322834220, -0.3392501089628018884, -2.892388451443569153 ) ) ;
#6123 = CARTESIAN_POINT ( 'NONE',  ( 1.266404199475066328, -0.05778040916215522460, 0.4822834645669289988 ) ) ;
#6124 = CARTESIAN_POINT ( 'NONE',  ( -1.423884514435694859, -0.05778040916215560624, -0.4822834645669293319 ) ) ;
#6125 = CARTESIAN_POINT ( 'NONE',  ( 0.2362204724409449064, 0.4091458600556404646, -1.008530183727034180 ) ) ;
#6126 = CARTESIAN_POINT ( 'NONE',  ( -0.3543307086614165824, -0.6692913385826771977, 8.415575281601705876E-17 ) ) ;
#6127 = CARTESIAN_POINT ( 'NONE',  ( -1.135170603674539924, 0.2952755905511810774, -0.1292274648535930714 ) ) ;
#6128 = CARTESIAN_POINT ( 'NONE',  ( 1.384514435695538559, 0.1771653543307087075, -0.09757992244046823083 ) ) ;
#6129 = CARTESIAN_POINT ( 'NONE',  ( -0.4068241469816267775, -0.004921259842519870586, -0.3153832671262229437 ) ) ;
#6130 = CARTESIAN_POINT ( 'NONE',  ( -0.7152230971128602510, -0.05778040916215560624, -0.4822834645669293319 ) ) ;
#6131 = CARTESIAN_POINT ( 'NONE',  ( -1.141732283464566011, 0.2952755905511811885, 0.000000000000000000 ) ) ;
#6132 = DIRECTION ( 'NONE',  ( 0.000000000000000000, -1.000000000000000000, 0.000000000000000000 ) ) ;
#6133 = CARTESIAN_POINT ( 'NONE',  ( 1.095800524934383846, -0.08942795157528024563, -0.3641732283464568787 ) ) ;
#6134 = CARTESIAN_POINT ( 'NONE',  ( -0.1837270341207340729, 0.2306618581243847221, -0.2411417322834647770 ) ) ;
#6135 = CARTESIAN_POINT ( 'NONE',  ( -1.712598425196849572, 0.1660481256975885056, 0.3530559997133364547 ) ) ;
#6136 = ORIENTED_EDGE ( 'NONE', *, *, #67416, .T. ) ;
#6137 = CARTESIAN_POINT ( 'NONE',  ( -9.787531504996566615E-17, 0.3996062992125985480, -2.281496062992125928 ) ) ;
#6138 = CARTESIAN_POINT ( 'NONE',  ( -0.8005249343832011588, -0.004921259842519870586, -0.3153832671262229437 ) ) ;
#6139 = CARTESIAN_POINT ( 'NONE',  ( 1.069553805774278610, -0.6692913385826771977, 0.1292274648535927661 ) ) ;
#6140 = CARTESIAN_POINT ( 'NONE',  ( -1.003937007874015297, -0.4536011799217368745, -0.2665933059059886201 ) ) ;
#6141 = CARTESIAN_POINT ( 'NONE',  ( -9.787531504996566615E-17, 0.3996062992125985480, -1.336614173228346525 ) ) ;
#6142 = CARTESIAN_POINT ( 'NONE',  ( -0.8070866141732276899, -0.5400638737290844871, 0.3530559997133364547 ) ) ;
#6143 = VECTOR ( 'NONE', #26306, 39.37007874015748143 ) ;
#6144 = CARTESIAN_POINT ( 'NONE',  ( 0.8595800524934390507, -0.3162353388693405765, 0.4822834645669290543 ) ) ;
#6145 = CARTESIAN_POINT ( 'NONE',  ( 0.8661417322834653598, -0.1870078740157479769, 0.4822834645669291653 ) ) ;
#6146 = CARTESIAN_POINT ( 'NONE',  ( -0.4724409448818896462, -0.1265901696524993070, -0.04593175853018372640 ) ) ;
#6147 = CARTESIAN_POINT ( 'NONE',  ( -1.620734908136482577, -0.5511811023622048555, -0.09757992244046775898 ) ) ;
#6148 = CARTESIAN_POINT ( 'NONE',  ( -9.787531504996566615E-17, 0.3996062992125985480, -0.5492125984251968740 ) ) ;
#6149 = CARTESIAN_POINT ( 'NONE',  ( 0.3460692066303959202, 0.1998031496062993295, -0.7611548556430446366 ) ) ;
#6150 = CARTESIAN_POINT ( 'NONE',  ( -0.3949938075777409408, -0.1058382717557502933, -0.2034120734908137218 ) ) ;
#6151 = CARTESIAN_POINT ( 'NONE',  ( 0.4255991402441264837, 1.325803004855074407, 2.647315919250823768 ) ) ;
#6152 = CARTESIAN_POINT ( 'NONE',  ( 1.325459317585302665, -0.3690944881889763329, 0.3153832671262228327 ) ) ;
#6153 = CARTESIAN_POINT ( 'NONE',  ( 0.7545931758530188826, -0.5511811023622046335, 0.09757992244046803654 ) ) ;
#6154 = CARTESIAN_POINT ( 'NONE',  ( 0.2034120734908142214, 0.2952755905511810774, -0.1292274648535930714 ) ) ;
#6155 = CARTESIAN_POINT ( 'NONE',  ( 5.785732909357575061E-17, -0.4724409448818898682, -2.360236220472441193 ) ) ;
#6156 = CARTESIAN_POINT ( 'NONE',  ( 0.2891555358219910499, -0.2891555358219909944, -1.277559055118109965 ) ) ;
#6157 = CARTESIAN_POINT ( 'NONE',  ( 0.8333333333333340365, -0.5511811023622046335, 0.09757992244046803654 ) ) ;
#6158 = CARTESIAN_POINT ( 'NONE',  ( -0.4986876640419939388, 0.2306618581243847221, -0.2411417322834647770 ) ) ;
#6159 = CARTESIAN_POINT ( 'NONE',  ( -1.299212598425196097, 0.2952755905511811885, 0.000000000000000000 ) ) ;
#6160 = CARTESIAN_POINT ( 'NONE',  ( 0.7480314960629927956, 0.2952755905511811885, 0.000000000000000000 ) ) ;
#6161 = CARTESIAN_POINT ( 'NONE',  ( 0.4091458600556404646, -0.2362204724409448231, -1.679790026246719137 ) ) ;
#6162 = CARTESIAN_POINT ( 'NONE',  ( -0.1998031496062994683, 0.3460692066303958092, -2.690288713910760965 ) ) ;
#6163 = VERTEX_POINT ( 'NONE', #48908 ) ;
#6164 = ORIENTED_EDGE ( 'NONE', *, *, #35750, .T. ) ;
#6165 = CARTESIAN_POINT ( 'NONE',  ( -1.318897637795274802, -0.5400638737290845981, -0.3530559997133363437 ) ) ;
#6166 = CARTESIAN_POINT ( 'NONE',  ( -0.4199475065616791736, -0.6046776061558807314, 0.2411417322834647770 ) ) ;
#6168 = CARTESIAN_POINT ( 'NONE',  ( -0.5839895013123351797, -0.6692913385826771977, 0.1292274648535927661 ) ) ;
#6167 = CARTESIAN_POINT ( 'NONE',  ( -0.7349081364829387342, -0.5023911411419708095, 0.1820866141732285504 ) ) ;
#6169 = CARTESIAN_POINT ( 'NONE',  ( 0.1049643490035303689, 0.3917322834645668994, -2.120715592354644130 ) ) ;
#6170 = CARTESIAN_POINT ( 'NONE',  ( -0.3280839895013117347, 0.05413385826771626580, -0.4176697321401330321 ) ) ;
#6171 = CARTESIAN_POINT ( 'NONE',  ( 1.581364829396326277, -0.05778040916215522460, 0.4822834645669289988 ) ) ;
#6172 = CARTESIAN_POINT ( 'NONE',  ( -0.7020997375328076329, -0.3162353388693409650, -0.4822834645669289433 ) ) ;
#6173 = CARTESIAN_POINT ( 'NONE',  ( 0.2362204724409456558, -0.1870078740157480879, -0.4822834645669291653 ) ) ;
#6174 = CARTESIAN_POINT ( 'NONE',  ( -0.8792650918635160906, -0.4281496062992124485, 0.4176697321401328655 ) ) ;
#6175 = EDGE_CURVE ( 'NONE', #34953, #76797, #13784, .T. ) ;
#6176 = CARTESIAN_POINT ( 'NONE',  ( 0.3392501089628018329, 0.1958661417322835607, -1.540682414698162805 ) ) ;
#6177 = CARTESIAN_POINT ( 'NONE',  ( -0.6758530183727028406, 0.1771653543307087630, 0.09757992244046791164 ) ) ;
#6178 = ORIENTED_EDGE ( 'NONE', *, *, #57803, .T. ) ;
#6179 = CARTESIAN_POINT ( 'NONE',  ( 0.1058382717557499880, 0.3949938075777411073, -1.883202099737532720 ) ) ;
#6180 = ORIENTED_EDGE ( 'NONE', *, *, #54557, .T. ) ;
#6181 = CARTESIAN_POINT ( 'NONE',  ( -1.686351706036744558, 0.1771653543307087075, -0.09757992244046823083 ) ) ;
#6182 = CARTESIAN_POINT ( 'NONE',  ( -1.207349081364828436, -0.6046776061558807314, 0.2411417322834647770 ) ) ;
#6183 = CARTESIAN_POINT ( 'NONE',  ( -1.036745406824146176, -0.4281496062992124485, 0.4176697321401328655 ) ) ;
#6184 = CARTESIAN_POINT ( 'NONE',  ( -0.2925321140481930704, -0.2925321140481933480, -0.3740157480314960092 ) ) ;
#6185 = CARTESIAN_POINT ( 'NONE',  ( -1.207349081364828880, 0.2306618581243847221, -0.2411417322834647770 ) ) ;
#6186 = CARTESIAN_POINT ( 'NONE',  ( -1.089238845144356427, 0.05413385826771666132, 0.4176697321401328100 ) ) ;
#6187 = DIRECTION ( 'NONE',  ( -1.000000000000000000, -0.000000000000000000, 1.692413147294446216E-16 ) ) ;
#6188 = CARTESIAN_POINT ( 'NONE',  ( -1.646051170424378096, -0.1870078740157480046, 1.254653134982923898E-17 ) ) ;
#6189 = CARTESIAN_POINT ( 'NONE',  ( 0.4855643044619430415, -0.3690944881889765550, -0.3153832671262227771 ) ) ;
#6190 = CARTESIAN_POINT ( 'NONE',  ( -0.2952755905511810774, 0.000000000000000000, 6.062992125984251857 ) ) ;
#6191 = CARTESIAN_POINT ( 'NONE',  ( -9.594673741351313045E-17, 0.3917322834645670104, -0.2421259842519686289 ) ) ;
#6192 = CARTESIAN_POINT ( 'NONE',  ( -0.3805774278215216522, -0.3690944881889765550, -0.3153832671262227771 ) ) ;
#6193 = CARTESIAN_POINT ( 'NONE',  ( -0.5971128608923877978, -0.6692913385826773087, -0.1292274648535924053 ) ) ;
#6194 = CARTESIAN_POINT ( 'NONE',  ( 1.469816272965879911, 0.2306618581243847221, -0.2411417322834647770 ) ) ;
#6195 = CARTESIAN_POINT ( 'NONE',  ( -0.3477690288713902178, 0.2952755905511810774, -0.1292274648535930714 ) ) ;
#6196 = ORIENTED_EDGE ( 'NONE', *, *, #40336, .F. ) ;
#6197 = ORIENTED_EDGE ( 'NONE', *, *, #68902, .T. ) ;
#6198 = CARTESIAN_POINT ( 'NONE',  ( -0.2925321140481932369, 0.2925321140481931259, -1.828740157480315265 ) ) ;
#6199 = CARTESIAN_POINT ( 'NONE',  ( -0.5839895013123351797, -0.6692913385826771977, 0.1292274648535927661 ) ) ;
#6200 = CARTESIAN_POINT ( 'NONE',  ( 1.371391076115485719, -0.6692913385826773087, -0.1292274648535924053 ) ) ;
#6201 = CARTESIAN_POINT ( 'NONE',  ( -0.9645669291338575535, -0.4536011799217367080, 0.2665933059059888421 ) ) ;
#6202 = CARTESIAN_POINT ( 'NONE',  ( -1.299212598425196097, -0.6692913385826771977, 8.415575281601705876E-17 ) ) ;
#6203 = CARTESIAN_POINT ( 'NONE',  ( -0.4091458600556405756, 0.2362204724409446288, -0.6561679790026246906 ) ) ;
#6204 = DIRECTION ( 'NONE',  ( 0.000000000000000000, 0.000000000000000000, 1.000000000000000000 ) ) ;
#6205 = CARTESIAN_POINT ( 'NONE',  ( -0.1958661417322834220, -0.3392501089628018884, -2.827427821522309426 ) ) ;
#6206 = VECTOR ( 'NONE', #59638, 39.37007874015748143 ) ;
#6207 = CARTESIAN_POINT ( 'NONE',  ( -0.2867679344610364334, -0.2867679344610367109, -2.190944881889763440 ) ) ;
#6208 = CARTESIAN_POINT ( 'NONE',  ( 0.03280839895013198948, -0.6692913385826773087, -0.1292274648535924053 ) ) ;
#6209 = CARTESIAN_POINT ( 'NONE',  ( -0.9186351706036736120, -0.5023911411419708095, -0.1820866141732282451 ) ) ;
#6210 = CIRCLE ( 'NONE', #35856, 0.5118110236220471121 ) ;
#6211 = CARTESIAN_POINT ( 'NONE',  ( -0.6824146981627291497, -0.6046776061558809534, -0.2411417322834644161 ) ) ;
#6212 = CARTESIAN_POINT ( 'NONE',  ( -0.3458507752293906723, -0.3458507752293910609, -2.812992125984251857 ) ) ;
#6213 = CARTESIAN_POINT ( 'NONE',  ( -0.8923884514435688198, 0.2306618581243847221, -0.2411417322834647770 ) ) ;
#6214 = CARTESIAN_POINT ( 'NONE',  ( -1.122047244094487306, -0.5400638737290844871, 0.3530559997133364547 ) ) ;
#6215 = CARTESIAN_POINT ( 'NONE',  ( 0.3420746716998660508, 0.1974969037888705814, -2.097769028871391495 ) ) ;
#6216 = CARTESIAN_POINT ( 'NONE',  ( 0.8923884514435701520, -0.5023911411419708095, -0.1820866141732282451 ) ) ;
#6217 = CARTESIAN_POINT ( 'NONE',  ( -0.8333333333333323711, -0.5511811023622048555, -0.09757992244046775898 ) ) ;
#6218 = CARTESIAN_POINT ( 'NONE',  ( 0.6167979002624679463, -0.004921259842519870586, -0.3153832671262229437 ) ) ;
#6219 = CARTESIAN_POINT ( 'NONE',  ( -1.699475065616797398, 0.2952755905511811885, 0.1292274648535926551 ) ) ;
#6220 = CARTESIAN_POINT ( 'NONE',  ( 1.443569553805774897, 0.2306618581243848609, 0.2411417322834645549 ) ) ;
#6221 = CARTESIAN_POINT ( 'NONE',  ( 0.4724409448818904789, -0.1870078740157480601, -0.3641732283464567677 ) ) ;
#6222 = CARTESIAN_POINT ( 'NONE',  ( -0.1958661417322836718, 0.3392501089628017219, -1.422572178477690574 ) ) ;
#6223 = CARTESIAN_POINT ( 'NONE',  ( -0.7480314960629914633, -0.6692913385826771977, 8.415575281601705876E-17 ) ) ;
#6224 = CARTESIAN_POINT ( 'NONE',  ( 1.135170603674541256, 0.2952755905511811885, 0.1292274648535926551 ) ) ;
#6225 = AXIS2_PLACEMENT_3D ( 'NONE', #17119, #4465, #30548 ) ;
#6226 = CARTESIAN_POINT ( 'NONE',  ( 0.3458507752293908943, -0.3458507752293908943, 0.1397637795275590289 ) ) ;
#6227 = CARTESIAN_POINT ( 'NONE',  ( -0.2559055118110227234, -0.4536011799217367080, 0.2665933059059888421 ) ) ;
#6228 = DIRECTION ( 'NONE',  ( 1.000000000000000000, -0.000000000000000000, -0.000000000000000000 ) ) ;
#6229 = CARTESIAN_POINT ( 'NONE',  ( 0.5183727034120741983, -0.6692913385826771977, 0.1292274648535927661 ) ) ;
#6230 = CARTESIAN_POINT ( 'NONE',  ( 1.141732283464567566, 0.1771653543307087630, 0.000000000000000000 ) ) ;
#6231 = CARTESIAN_POINT ( 'NONE',  ( 0.1115485564304467270, -0.5511811023622048555, -0.09757992244046775898 ) ) ;
#6232 = CARTESIAN_POINT ( 'NONE',  ( -0.07217847769028787330, -0.05778040916215522460, 0.4822834645669289988 ) ) ;
#6233 = CARTESIAN_POINT ( 'NONE',  ( -1.377952755905511140, 0.2952755905511811885, 0.000000000000000000 ) ) ;
#6234 = CARTESIAN_POINT ( 'NONE',  ( -0.8530183727034112984, -0.004921259842519576551, 0.3153832671262227771 ) ) ;
#6235 = DIRECTION ( 'NONE',  ( 0.000000000000000000, 0.000000000000000000, 1.000000000000000000 ) ) ;
#6236 = CARTESIAN_POINT ( 'NONE',  ( -0.3937007874015740483, -0.1870078740157479769, 0.4822834645669291653 ) ) ;
#6237 = CARTESIAN_POINT ( 'NONE',  ( 4.893765752498283308E-17, -0.3996062992125985480, -1.100393700787401619 ) ) ;
#6238 = CARTESIAN_POINT ( 'NONE',  ( 0.2867679344610365999, 0.2867679344610365999, -2.427165354330708347 ) ) ;
#6239 = CARTESIAN_POINT ( 'NONE',  ( 0.07217847769028949700, -0.08942795157528024563, -0.3641732283464568787 ) ) ;
#6240 = CARTESIAN_POINT ( 'NONE',  ( -0.4855643044619415427, 0.05413385826771626580, -0.4176697321401330321 ) ) ;
#6241 = CARTESIAN_POINT ( 'NONE',  ( -1.266404199475064773, -0.05778040916215560624, -0.4822834645669293319 ) ) ;
#6242 = CARTESIAN_POINT ( 'NONE',  ( -0.6758530183727028406, 0.1771653543307087630, 0.09757992244046791164 ) ) ;
#6243 = CARTESIAN_POINT ( 'NONE',  ( -3.936548249448418080, 1.066819220836087379, -0.06211919455352141878 ) ) ;
#6244 = CARTESIAN_POINT ( 'NONE',  ( -0.6430446194225712953, 0.05413385826771626580, -0.4176697321401330321 ) ) ;
#6245 = CARTESIAN_POINT ( 'NONE',  ( -0.7217847769028863381, -0.3690944881889763329, 0.3153832671262228327 ) ) ;
#6246 = CARTESIAN_POINT ( 'NONE',  ( -1.594488188976377563, -0.4536011799217367080, 0.2665933059059888421 ) ) ;
#6247 = CARTESIAN_POINT ( 'NONE',  ( 1.299212598425197429, 0.2952755905511811885, 0.000000000000000000 ) ) ;
#6248 = CARTESIAN_POINT ( 'NONE',  ( -0.4735970878719478194, 1.569539909699054325, 1.017201612406801070 ) ) ;
#6249 = CARTESIAN_POINT ( 'NONE',  ( -0.1958661417322833942, -0.3392501089628018884, -2.109599368275277609 ) ) ;
#6250 = ORIENTED_EDGE ( 'NONE', *, *, #56357, .F. ) ;
#6251 = CYLINDRICAL_SURFACE ( 'NONE', #29748, 0.4744094488188972947 ) ;
#6252 = CARTESIAN_POINT ( 'NONE',  ( -1.240157480314959759, 0.1660481256975885056, 0.3530559997133364547 ) ) ;
#6253 = CARTESIAN_POINT ( 'NONE',  ( -0.6758530183727028406, -0.6692913385826773087, -0.1292274648535924053 ) ) ;
#6254 = CARTESIAN_POINT ( 'NONE',  ( 1.607611548556431069, 0.2952755905511811885, 0.1292274648535926551 ) ) ;
#6255 = CARTESIAN_POINT ( 'NONE',  ( -0.1049643490035307020, 0.3917322834645669549, -2.138451443569553412 ) ) ;
#6256 = CARTESIAN_POINT ( 'NONE',  ( -0.03611438844013053345, 0.3902087894128228873, -1.220472440944881498 ) ) ;
#6257 = CARTESIAN_POINT ( 'NONE',  ( 1.102362204724410155, -0.1870078740157480879, -0.4822834645669291653 ) ) ;
#6258 = CARTESIAN_POINT ( 'NONE',  ( -0.09186351706036663400, -0.4281496062992124485, 0.4176697321401328655 ) ) ;
#6259 = LINE ( 'NONE', #83288, #50328 ) ;
#6260 = AXIS2_PLACEMENT_3D ( 'NONE', #33780, #45971, #52701 ) ;
#6261 = VECTOR ( 'NONE', #17148, 39.37007874015748143 ) ;
#6262 = CARTESIAN_POINT ( 'NONE',  ( -0.1070741851644051862, -0.3996062992125986035, -2.668635170603674833 ) ) ;
#6263 = CARTESIAN_POINT ( 'NONE',  ( 1.358267716535433323, -0.4536011799217368745, -0.2665933059059886201 ) ) ;
#6264 = CARTESIAN_POINT ( 'NONE',  ( 0.3460692066303959202, 0.1998031496062993295, -1.233595800524934338 ) ) ;
#6265 = VERTEX_POINT ( 'NONE', #36285 ) ;
#6266 = CARTESIAN_POINT ( 'NONE',  ( -0.3917322834645671770, 0.1049643490035302024, -0.02954687483695727160 ) ) ;
#6267 = ORIENTED_EDGE ( 'NONE', *, *, #36825, .T. ) ;
#6268 = CARTESIAN_POINT ( 'NONE',  ( 5.463695987328526437E-16, -0.1870078740157479769, 0.4822834645669291653 ) ) ;
#6269 = CARTESIAN_POINT ( 'NONE',  ( -0.9120734908136475250, 0.2952755905511811885, 0.1292274648535926551 ) ) ;
#6270 = CARTESIAN_POINT ( 'NONE',  ( -1.469816272965878357, 0.2306618581243848609, 0.2411417322834645549 ) ) ;
#6271 = CARTESIAN_POINT ( 'NONE',  ( 0.5643044619422579178, 0.05413385826771666132, 0.4176697321401328100 ) ) ;
#6272 = CARTESIAN_POINT ( 'NONE',  ( 1.437007874015748810, -0.5400638737290845981, -0.3530559997133363437 ) ) ;
#6273 = CARTESIAN_POINT ( 'NONE',  ( 1.371391076115485719, -0.6692913385826773087, -0.1292274648535924053 ) ) ;
#6274 = CARTESIAN_POINT ( 'NONE',  ( -0.4921259842519677963, 0.1660481256975883668, -0.3530559997133364547 ) ) ;
#6275 = CARTESIAN_POINT ( 'NONE',  ( 0.3215223097112867578, -0.05778040916215522460, 0.4822834645669289988 ) ) ;
#6276 = CARTESIAN_POINT ( 'NONE',  ( -1.154855643044618851, 0.2306618581243848609, 0.2411417322834645549 ) ) ;
#6277 = CARTESIAN_POINT ( 'NONE',  ( 1.351706036745407458, -0.4281496062992127816, -0.4176697321401328100 ) ) ;
#6278 = CARTESIAN_POINT ( 'NONE',  ( 1.568241469816273659, -0.05778040916215560624, -0.4822834645669293319 ) ) ;
#6279 = CARTESIAN_POINT ( 'NONE',  ( 0.02624671916010564918, 0.2306618581243848609, 0.2411417322834645549 ) ) ;
#6280 = CARTESIAN_POINT ( 'NONE',  ( 0.3917322834645670104, -0.1049643490035303411, -0.2611548556430445256 ) ) ;
#6281 = CARTESIAN_POINT ( 'NONE',  ( 0.5118110236220480003, -0.5511811023622047445, 6.969142054262312111E-17 ) ) ;
#6282 = EDGE_LOOP ( 'NONE', ( #33449, #15016, #81145, #15753 ) ) ;
#6283 = CARTESIAN_POINT ( 'NONE',  ( -0.3949938075777409963, -7.255918531996591613E-17, -0.5118110236220473341 ) ) ;
#6284 = ORIENTED_EDGE ( 'NONE', *, *, #53723, .F. ) ;
#6285 = CARTESIAN_POINT ( 'NONE',  ( -0.09186351706036689768, -0.004921259842519870586, -0.3153832671262229437 ) ) ;
#6286 = B_SPLINE_CURVE_WITH_KNOTS ( 'NONE', 3,
 ( #29701, #5269, #56600, #56193 ),
 .UNSPECIFIED., .F., .F.,
 ( 4, 4 ),
 ( 9.341771812940338307E-18, 0.001510660848375616110 ),
 .UNSPECIFIED. ) ;
#6287 = CARTESIAN_POINT ( 'NONE',  ( 2.847313777101087240, 1.091897865355356601, -0.1662078246829617190 ) ) ;
#6288 = CARTESIAN_POINT ( 'NONE',  ( -0.05249343832020938322, -0.6046776061558809534, -0.2411417322834644161 ) ) ;
#6289 = CARTESIAN_POINT ( 'NONE',  ( -0.1049868766404193215, 0.2306618581243847221, -0.2411417322834647770 ) ) ;
#6290 = CARTESIAN_POINT ( 'NONE',  ( -0.3937007874015740483, -0.1870078740157480879, -0.4822834645669291653 ) ) ;
#6291 = CARTESIAN_POINT ( 'NONE',  ( -0.2867679344610367109, 0.2867679344610365444, -1.591226664863204077 ) ) ;
#6292 = CARTESIAN_POINT ( 'NONE',  ( -1.332020997375327642, -0.05778040916215522460, 0.4822834645669289988 ) ) ;
#6293 = CARTESIAN_POINT ( 'NONE',  ( 0.3917322834645669549, 0.1049643490035304660, -2.571522309711286258 ) ) ;
#6294 = CARTESIAN_POINT ( 'NONE',  ( 0.7152230971128614723, -0.2845877964562161244, -0.3641732283464567121 ) ) ;
#6295 = CARTESIAN_POINT ( 'NONE',  ( 1.095800524934383846, -0.05778040916215560624, -0.4822834645669293319 ) ) ;
#6296 = CARTESIAN_POINT ( 'NONE',  ( 0.8923884514435703741, 0.2306618581243848609, 0.2411417322834645549 ) ) ;
#6297 = CARTESIAN_POINT ( 'NONE',  ( 0.1070741851644054915, -0.3996062992125986035, -1.030183727034120533 ) ) ;
#6298 = CARTESIAN_POINT ( 'NONE',  ( -1.391076115485563758, 0.2306618581243848609, 0.2411417322834645549 ) ) ;
#6299 = CARTESIAN_POINT ( 'NONE',  ( -0.2925321140481930149, -0.2925321140481933480, -0.1358267716535432879 ) ) ;
#6300 = CARTESIAN_POINT ( 'NONE',  ( -0.1998031496062994405, 0.3460692066303957537, -0.08989501312335959615 ) ) ;
#6301 = CARTESIAN_POINT ( 'NONE',  ( -0.1115485564304456306, 0.2952755905511810774, -0.1292274648535930714 ) ) ;
#6302 = CARTESIAN_POINT ( 'NONE',  ( -0.1070741851644051862, -0.3996062992125987146, -2.906824146981627610 ) ) ;
#6303 = CARTESIAN_POINT ( 'NONE',  ( -0.1049643490035302024, -0.3917322834645671215, -1.731627296587926468 ) ) ;
#6304 = CARTESIAN_POINT ( 'NONE',  ( 1.482939632545932307, 0.05413385826771626580, -0.4176697321401330321 ) ) ;
#6305 = CARTESIAN_POINT ( 'NONE',  ( 1.213910761154856299, 0.2952755905511811885, 0.1292274648535926551 ) ) ;
#6306 = CARTESIAN_POINT ( 'NONE',  ( 0.1443569553805781891, -0.004921259842519870586, -0.3153832671262229437 ) ) ;
#6307 = CARTESIAN_POINT ( 'NONE',  ( 0.9317585301837276734, -0.4281496062992124485, 0.4176697321401328655 ) ) ;
#6308 = CARTESIAN_POINT ( 'NONE',  ( -0.3458507752293906723, -0.3458507752293910609, -1.553149606299212726 ) ) ;
#6309 = CARTESIAN_POINT ( 'NONE',  ( 0.5249343832021005074, -0.5023911411419708095, 0.1820866141732285504 ) ) ;
#6310 = CARTESIAN_POINT ( 'NONE',  ( 0.2559055118110243332, -0.5400638737290845981, -0.3530559997133363437 ) ) ;
#6311 = CARTESIAN_POINT ( 'NONE',  ( -0.2891555358219911054, 0.2891555358219909388, -1.041338582677165503 ) ) ;
#6312 = CARTESIAN_POINT ( 'NONE',  ( -1.102362204724408601, -0.1870078740157479769, 0.4822834645669291653 ) ) ;
#6313 = CARTESIAN_POINT ( 'NONE',  ( 0.9645669291338588858, 0.07958543189024085140, 0.2665933059059887866 ) ) ;
#6314 = CARTESIAN_POINT ( 'NONE',  ( -2.554262525012342966, 1.554943921348592273, -0.4744094488188976277 ) ) ;
#6316 = EDGE_CURVE ( 'NONE', #27965, #69251, #40309, .T. ) ;
#6315 = CARTESIAN_POINT ( 'NONE',  ( -0.1640419947506555343, -0.3162353388693405765, 0.4822834645669290543 ) ) ;
#6317 = CARTESIAN_POINT ( 'NONE',  ( -0.2887139107611542133, -0.5023911411419708095, -0.1820866141732282451 ) ) ;
#6318 = CARTESIAN_POINT ( 'NONE',  ( 0.1181102362204724254, 8.537024980200824098E-18, 0.000000000000000000 ) ) ;
#6319 = CARTESIAN_POINT ( 'NONE',  ( -0.4265091863517051496, 0.2952755905511810774, -0.1292274648535930714 ) ) ;
#6320 = CARTESIAN_POINT ( 'NONE',  ( 0.3805774278215230400, -0.004921259842519870586, -0.3153832671262229437 ) ) ;
#6321 = AXIS2_PLACEMENT_3D ( 'NONE', #26144, #18999, #70773 ) ;
#6322 = CARTESIAN_POINT ( 'NONE',  ( 0.2925321140481932369, 0.2925321140481932369, -2.261811023622047223 ) ) ;
#6323 = CARTESIAN_POINT ( 'NONE',  ( 0.05905511811023709395, -0.5400638737290844871, 0.3530559997133364547 ) ) ;
#6324 = ADVANCED_FACE ( 'NONE', ( #41763 ), #73360, .F. ) ;
#6325 = AXIS2_PLACEMENT_3D ( 'NONE', #24341, #42454, #56734 ) ;
#6327 = VECTOR ( 'NONE', #46784, 39.37007874015748143 ) ;
#6326 = CARTESIAN_POINT ( 'NONE',  ( 0.2867679344610365999, 0.2867679344610365999, -1.792631602853332007 ) ) ;
#6328 = VECTOR ( 'NONE', #58066, 39.37007874015748143 ) ;
#6329 = CARTESIAN_POINT ( 'NONE',  ( 1.345144356955381593, -0.08942795157527998196, 0.3641732283464567121 ) ) ;
#6330 = CARTESIAN_POINT ( 'NONE',  ( 1.607611548556431069, 0.2952755905511811885, 0.1292274648535926551 ) ) ;
#6331 = CARTESIAN_POINT ( 'NONE',  ( -0.9711286089238838626, -0.5023911411419708095, 0.1820866141732285504 ) ) ;
#6332 = CARTESIAN_POINT ( 'NONE',  ( -0.8727034120734901146, -0.08942795157528024563, -0.3641732283464568787 ) ) ;
#6333 = CARTESIAN_POINT ( 'NONE',  ( -0.2427821522309703550, -0.3162353388693405765, 0.4822834645669290543 ) ) ;
#6334 = CARTESIAN_POINT ( 'NONE',  ( -0.04593175853018302557, -0.6692913385826773087, -0.1292274648535924053 ) ) ;
#6335 = CARTESIAN_POINT ( 'NONE',  ( 0.4593175853018380828, -0.004921259842519870586, -0.3153832671262229437 ) ) ;
#6336 = CARTESIAN_POINT ( 'NONE',  ( -0.2814773692359251456, 0.08976595949324576995, 5.548806511850565393 ) ) ;
#6337 = CARTESIAN_POINT ( 'NONE',  ( 1.371391076115485719, -0.5511811023622048555, -0.09757992244046775898 ) ) ;
#6338 = CARTESIAN_POINT ( 'NONE',  ( 0.6233595800524942554, -0.05778040916215560624, -0.4822834645669293319 ) ) ;
#6339 = ADVANCED_FACE ( 'NONE', ( #67456 ), #35881, .F. ) ;
#6340 = CARTESIAN_POINT ( 'NONE',  ( -0.2925321140481930149, -0.2925321140481933480, 0.02165354330708659653 ) ) ;
#6341 = CARTESIAN_POINT ( 'NONE',  ( -0.2559055118110230564, 0.1660481256975883668, -0.3530559997133364547 ) ) ;
#6342 = CARTESIAN_POINT ( 'NONE',  ( 0.2867679344610365999, -0.2867679344610365444, -0.8129921259842518566 ) ) ;
#6343 = CARTESIAN_POINT ( 'NONE',  ( -1.574803149606298636, -0.1870078740157479769, 0.4822834645669291653 ) ) ;
#6344 = CARTESIAN_POINT ( 'NONE',  ( 0.8792650918635177559, 0.05413385826771666132, 0.4176697321401328100 ) ) ;
#6345 = CARTESIAN_POINT ( 'NONE',  ( 0.3805774278215230400, -0.4281496062992124485, 0.4176697321401328655 ) ) ;
#6346 = ADVANCED_FACE ( 'NONE', ( #36689, #61550 ), #81335, .T. ) ;
#6347 = CARTESIAN_POINT ( 'NONE',  ( -0.1528381195902957790, 1.087211650537911245, -3.934145130003242397 ) ) ;
#6348 = CARTESIAN_POINT ( 'NONE',  ( 0.4068241469816281097, -0.004921259842519576551, 0.3153832671262227771 ) ) ;
#6349 = CARTESIAN_POINT ( 'NONE',  ( 1.194225721784777594, 0.05413385826771666132, 0.4176697321401328100 ) ) ;
#6350 = CARTESIAN_POINT ( 'NONE',  ( -0.4002624671916004129, -0.08942795157528024563, -0.3641732283464568787 ) ) ;
#6351 = CARTESIAN_POINT ( 'NONE',  ( -0.8727034120734901146, -0.3162353388693405765, 0.4822834645669290543 ) ) ;
#6352 = PLANE ( 'NONE',  #9865 ) ;
#6353 = CARTESIAN_POINT ( 'NONE',  ( 0.07217847769028949700, -0.05778040916215560624, -0.4822834645669293319 ) ) ;
#6354 = CARTESIAN_POINT ( 'NONE',  ( -0.9908136482939626788, 0.2952755905511811885, 0.1292274648535926551 ) ) ;
#6355 = CARTESIAN_POINT ( 'NONE',  ( -0.7414698162729651543, 0.1771653543307087075, -0.09757992244046823083 ) ) ;
#6356 = CARTESIAN_POINT ( 'NONE',  ( 0.1902887139107617975, 0.2952755905511811885, 0.1292274648535926551 ) ) ;
#6357 = CARTESIAN_POINT ( 'NONE',  ( -1.345144356955379816, -0.05778040916215560624, -0.4822834645669293319 ) ) ;
#6358 = CARTESIAN_POINT ( 'NONE',  ( -0.3215223097112853146, -0.05778040916215560624, -0.4822834645669293319 ) ) ;
#6359 =( CONVERSION_BASED_UNIT ( 'INCH', #56455 ) LENGTH_UNIT ( ) NAMED_UNIT ( #62602 ) );
#6361 = CARTESIAN_POINT ( 'NONE',  ( 1.541994750656168645, -0.6692913385826771977, 0.1292274648535927661 ) ) ;
#6360 = CYLINDRICAL_SURFACE ( 'NONE', #32509, 0.07874015748031495954 ) ;
#6362 = CARTESIAN_POINT ( 'NONE',  ( 1.154855643044620184, -0.6046776061558807314, 0.2411417322834647770 ) ) ;
#6363 = CARTESIAN_POINT ( 'NONE',  ( -0.1958661417322834220, -0.3392501089628018884, -2.577427821522309426 ) ) ;
#6364 = CARTESIAN_POINT ( 'NONE',  ( 0.4687286201624442095, 1.750728371878954803, -0.5180200956804339452 ) ) ;
#6365 = CARTESIAN_POINT ( 'NONE',  ( -0.7545931758530177724, 0.2952755905511811885, 0.1292274648535926551 ) ) ;
#6366 = CARTESIAN_POINT ( 'NONE',  ( 0.3458507752293908943, -0.3458507752293908943, -0.4133858267716534196 ) ) ;
#6367 = CARTESIAN_POINT ( 'NONE',  ( 0.3996062992125986035, 2.446882876249141962E-17, -0.2755905511811024278 ) ) ;
#6368 = VERTEX_POINT ( 'NONE', #35462 ) ;
#6369 = CARTESIAN_POINT ( 'NONE',  ( 8.195543980992789655E-16, -0.1870078740157480601, -0.3641732283464567677 ) ) ;
#6370 = CARTESIAN_POINT ( 'NONE',  ( 0.3917322834645670104, 2.398668435337828261E-17, -1.685039370078740051 ) ) ;
#6371 = CARTESIAN_POINT ( 'NONE',  ( 0.8661417322834652488, -0.1870078740157480879, -0.4822834645669291653 ) ) ;
#6372 = FACE_OUTER_BOUND ( 'NONE', #54551, .T. ) ;
#6373 = PLANE ( 'NONE',  #70860 ) ;
#6374 = CARTESIAN_POINT ( 'NONE',  ( -0.5971128608923877978, -0.5511811023622048555, -0.09757992244046775898 ) ) ;
#6375 = CARTESIAN_POINT ( 'NONE',  ( 0.3805774278215230400, 0.05413385826771626580, -0.4176697321401330321 ) ) ;
#6376 = CARTESIAN_POINT ( 'NONE',  ( 1.351706036745407680, 0.05413385826771666132, 0.4176697321401328100 ) ) ;
#6377 = CARTESIAN_POINT ( 'NONE',  ( 0.7480314960629927956, -0.5511811023622047445, 6.969142054262312111E-17 ) ) ;
#6378 = CARTESIAN_POINT ( 'NONE',  ( -0.1377952755905504645, -0.5400638737290845981, -0.3530559997133363437 ) ) ;
#6379 = CARTESIAN_POINT ( 'NONE',  ( -0.1049643490035306742, 0.3917322834645668994, -0.5590358023283972244 ) ) ;
#6380 = CARTESIAN_POINT ( 'NONE',  ( -1.017060367454067249, -0.05778040916215522460, 0.4822834645669289988 ) ) ;
#6381 = CARTESIAN_POINT ( 'NONE',  ( -1.338582677165353729, -0.1870078740157480601, -0.3641732283464567677 ) ) ;
#6382 = CARTESIAN_POINT ( 'NONE',  ( -0.5511811023622041894, -0.1870078740157480879, -0.4822834645669291653 ) ) ;
#6383 =( BOUNDED_SURFACE ( )  B_SPLINE_SURFACE ( 1, 2, ( 
 ( #796, #27284, #45797, #13420, #52530, #51689, #58009, #20148, #34023, #46639, #77817, #65189, #32348, #13006, #78237, #52944, #64758, #77392, #39926, #40339, #78658, #20570, #46221, #13843, #19723, #71917, #65615, #33607, #72334, #66019, #8355, #59683, #44955, #2039, #71078, #70651, #27704, #19303, #38662, #64339, #29360, #9597, #2869, #72742, #28532, #10012, #22221, #61762, #80728, #79486, #10434, #21800, #42390, #15506, #34441, #47050, #60930, #34858, #74407, #29768, #55019, #35265, #54189, #15089, #79904, #35677, #47877, #4100, #23042, #47464, #36091, #73156, #68089, #41164, #73581, #2461, #66854, #61342, #3695, #79078, #40747, #9186, #15927, #60108, #48709, #16339, #28119, #60520, #41574, #21394, #66431, #53774, #8766, #67264, #3280, #16751, #28944, #54610, #80319, #22634, #48295, #73992, #41982, #67676, #43620, #49118, #38146, #63406, #18793, #81550, #30598, #76052, #5742, #69321, #24687, #50354, #57077, #49535, #82771, #74824, #44038, #69730, #62171, #5341, #43206, #42802, #12075, #62588, #4930, #63818, #11672, #6157, #50766, #49946, #18396, #10836, #25094, #75644, #76467, #75229, #17168, #31000, #56668, #55841, #37733, #31413, #30179, #37329, #11254, #44438, #81960, #17573, #63002, #4510, #36495, #56264, #70131, #12482, #24275, #17983, #68496, #23868, #82368, #55429, #68901, #36912, #81137, #23453, #71813, #65080, #13740, #45280, #6576, #26347, #70975, #691, #14164, #52008, #39396, #77713, #57492, #27182, #25927, #38973, #32662, #64656, #57907, #51585, #52846, #46534, #6994, #38561, #14583, #12902, #45694, #72234, #39820, #83184, #78557, #19618, #65509, #64241, #7418, #33088, #7841, #19200, #20882, #77287, #25506, #26768, #46119, #13320, #44849, #32247, #272, #40236, #58329, #65919, #51172, #20043, #76868, #71391, #31831, #70547, #58755, #1117, #52423, #78133, #20466, #33508, #59170, #1528, #22948, #79385, #60832, #21704, #15835, #21296, #42296, #48615, #9498, #3184, #28848, #34763, #34341, #74309, #53677, #1942, #16656, #79808, #35171, #29265, #22124, #73058, #80224, #47783, #8256, #33920, #46949, #73898, #54093, #54510, #22540, #14991, #60006, #47368, #48203, #72641, #41483, #16238, #61246, #8670, #73485, #59585, #15408, #67579, #2361, #27604, #54929, #53264, #67168, #35583, #40648, #41068, #66757, #9911, #80636, #41886, #3600, #78975, #66332, #28017, #9091, #60423, #2774, #28434, #64035, #19420, #11880, #32461, #58123, #26145, #82573, #55338, #76667, #50155, #51382, #490, #38776, #19846, #67993, #51806, #81046, #77087, #31627, #32046, #12700, #75851, #37532, #31212, #57705, #18193, #19000, #68, #64453, #69530, #50970, #10338, #24892, #45071, #63208, #77511, #6788, #29675, #44649, #13125, #43826, #18599, #44242, #70774, #36000, #25305, #70346, #25722, #38359, #5547, #69931, #61670, #82985, #6374, #4011, #24488, #56880, #50561, #76264, #12287, #37943, #63620, #5957, #57288, #27823, #8883, #15208, #79607, #39619, #52649, #46337, #78353, #71609, #65308, #66550, #60225, #20685, #52229, #28234, #26576, #59386, #2575, #2156, #13534, #34559, #33317, #79193, #77932, #53061, #78773, #21509, #32884, #40868, #7647, #71192, #40455, #59802, #58979, #58553, #45912, #20262, #53893, #13962, #45495, #64874, #72030, #7214, #1335, #39190, #919, #26984, #14386, #27401, #40044, #21097, #65730, #8063, #33724, #1744, #46756, #14798, #72449, #66134, #8472, #34141, #53483, #47167, #72859, #16872, #48409, #48002, #4622, #67380, #15627, #30293, #10134, #23156, #42914, #35798, #3400, #10548, #61465, #48825, #22342, #68211, #42509, #80023, #3813, #61050, #61875, #74109, #16041, #29475, #28653, #60636, #22749, #36606, #23567, #80439, #42100, #34973, #41284, #67797, #4216, #41687, #54312, #36206, #17286, #29880, #55133, #80843, #35385, #73701, #16455, #29063, #74526, #55543, #81252, #49238, #74941, #47585, #68609, #10949, #66970, #62285, #55959, #9714, #54734, #21924, #73279, #9303, #2987, #63526, #44555, #5857, #82077, #82482, #51285, #12191, #25211, #76577, #31948, #24390, #44970, #70666, #38676, #11788, #69018, #31533, #62708, #63936, #13022, #76988, #32361, #75756 ),
 ( #49650, #19318, #69435, #57609, #5046, #57189, #82891, #83300, #11369, #64354, #18098, #23983, #18905, #12601, #37441, #37026, #50061, #30715, #6691, #56378, #81672, #17689, #5453, #43319, #63115, #75342, #43731, #31114, #56782, #50877, #24797, #70245, #50465, #76169, #18506, #44149, #69841, #38259, #37848, #6272, #25622, #71931, #13856, #14697, #1234, #52123, #65629, #64771, #13434, #58876, #72755, #59698, #33212, #78252, #71091, #51703, #20583, #40353, #77831, #7110, #52959, #53384, #66032, #7960, #39943, #71509, #32781, #52543, #39515, #26883, #8370, #46235, #33622, #15104, #26044, #78673, #66445, #77405, #59285, #65203, #79091, #8781, #34036, #14280, #7539, #19740, #1642, #72349, #27300, #40760, #2053, #58449, #58023, #809, #21409, #20161, #20994, #26472, #45811, #27717, #47063, #387, #45394, #46656, #39090, #15522, #42404, #55034, #41180, #47891, #2884, #81151, #17182, #73172, #74838, #22236, #53788, #68102, #73599, #23467, #67690, #29781, #55443, #15941, #54203, #80334, #22649, #28133, #42815, #10448, #49133, #60534, #9611, #80741, #36104, #48308, #3710, #29373, #61775, #28547, #4116, #79500, #23055, #48723, #66870, #10026, #41588, #21815, #74420, #67278, #35280, #68509, #74005, #34454, #60123, #28958, #16766, #9200, #2474, #54623, #47479, #79920, #34873, #35691, #61356, #60943, #3294, #16352, #41996, #81974, #4523, #4944, #70144, #30193, #30613, #82785, #5353, #12496, #31012, #17998, #49548, #43632, #18807, #62603, #24699, #56277, #56681, #55855, #10849, #44452, #50368, #76066, #18408, #69335, #68917, #36510, #24288, #81564, #62186, #44051, #12088, #23883, #69743, #37343, #25106, #37745, #75243, #17587, #49960, #43219, #63420, #11267, #50779, #75657, #11685, #82382, #36926, #5757, #63015, #31427, #57089, #76480, #67962, #2741, #41854, #22090, #3153, #35970, #61640, #47750, #3981, #30056, #35137, #35550, #61213, #4388, #23742, #42265, #10304, #48998, #29645, #28816, #3568, #55717, #16623, #55307, #81015, #36376, #54481, #49415, #75109, #43085, #16207, #73449, #23328, #67134, #68380, #17455, #81427, #36784, #80192, #9881, #29235, #54899, #22510, #48171, #68782, #11126, #80605, #9463, #28401, #60799, #74697, #54059, #42682, #79774, #15799, #73867, #62050, #67546, #17042, #10719, #41450, #22915, #48582, #74279, #4795, #57367, #76747, #75928, #49822, #62880, #11543, #19495, #37199, #51461, #30879, #25800, #45149, #17861, #70852, #50232, #81841, #70422, #18269, #77163, #12362, #57781, #145, #43909, #82247, #24966, #50638, #56136, #13203, #12778, #62460, #5215, #37608, #83062, #38435, #76342, #31707, #25383, #64118, #56546, #6453, #24152, #51046, #19077, #69194, #38020, #69607, #75522, #44725, #11953, #63283, #30472, #18672, #43496, #24565, #56954, #32123, #5623, #31289, #82651, #44317, #70007, #63696, #6035, #80574, #75073, #61606, #55270, #80981, #3535, #3117, #43051, #22475, #54027, #68747, #48548, #3949, #81390, #74246, #41819, #48964, #16588, #11090, #17420, #73415, #42648, #22884, #23293, #29610, #67100, #28784, #48136, #74664, #41416, #10269, #17008, #30018, #60767, #42234, #60358, #16173, #79738, #54446, #35937, #68345, #22055, #10685, #4351, #9431, #9846, #35518, #62014, #23706, #67928, #36340, #55683, #49377, #80158, #61181, #2705, #28365, #47717, #15764, #35100, #73833, #67510, #29202, #54868, #50196, #24117, #44284, #17827, #19043, #110, #6418, #70819, #30845, #43874, #51426, #24531, #6002, #69974, #44690, #11509, #56921, #77128, #37986, #31671, #57332, #63248, #62845, #19462, #82212, #30436, #45112, #24932, #63661, #57748, #50602, #18234, #25349, #76309, #36746, #62423, #49786, #70386, #82616, #83026, #51011, #43460, #5181, #75894, #76710, #69158, #12328, #12742, #32087, #37165, #18640, #4760, #69572, #56101, #56510, #38401, #64081, #81805, #25765, #75487, #11920, #37575, #5587, #31254, #34180, #52686, #78394, #59427, #20725, #13579, #14002, #66176, #27025, #40081, #8100, #46796, #39233, #59845, #2197, #53525, #26616, #534, #46377, #77556, #78812, #27865, #8514, #47209, #7255, #20304, #39660, #45954, #64918, #32928, #79233, #21548, #71651 ) ),
 .UNSPECIFIED., .F., .F., .F. ) 
 B_SPLINE_SURFACE_WITH_KNOTS ( ( 2, 2 ),
 ( 3, 2, 2, 2, 2, 2, 2, 2, 2, 2, 2, 2, 2, 2, 2, 2, 2, 2, 2, 2, 2, 2, 2, 2, 2, 2, 2, 2, 2, 2, 2, 2, 2, 2, 2, 2, 2, 2, 2, 2, 2, 2, 2, 2, 2, 2, 2, 2, 2, 2, 2, 2, 2, 2, 2, 2, 2, 2, 2, 2, 2, 2, 2, 2, 2, 2, 2, 2, 2, 2, 2, 2, 2, 2, 2, 2, 2, 2, 2, 2, 2, 2, 2, 2, 2, 2, 2, 2, 2, 2, 2, 2, 2, 2, 2, 2, 2, 2, 2, 2, 2, 2, 2, 2, 2, 2, 2, 2, 2, 2, 2, 2, 2, 2, 2, 2, 2, 2, 2, 2, 2, 2, 2, 2, 2, 2, 2, 2, 2, 2, 2, 2, 2, 2, 2, 2, 2, 2, 2, 2, 2, 2, 2, 2, 2, 2, 2, 2, 2, 2, 2, 2, 2, 2, 2, 2, 2, 2, 2, 2, 2, 2, 2, 2, 2, 2, 2, 2, 2, 2, 2, 2, 2, 2, 2, 2, 2, 2, 2, 2, 2, 2, 2, 2, 2, 2, 2, 2, 2, 2, 2, 2, 2, 2, 2, 2, 2, 2, 2, 2, 2, 2, 2, 2, 2, 2, 2, 2, 2, 2, 2, 2, 2, 2, 2, 2, 2, 2, 2, 2, 2, 2, 2, 2, 2, 2, 2, 2, 2, 2, 2, 2, 2, 2, 2, 2, 2, 2, 2, 2, 2, 2, 2, 2, 2, 2, 2, 2, 2, 2, 2, 2, 2, 2, 2, 3 ),
 ( 0.000000000000000000, 1.000000000000000000 ),
 ( 0.000000000000000000, 0.003787878787878787984, 0.007575757575757575968, 0.01136363636363636395, 0.01515151515151515194, 0.01893939393939393992, 0.02272727272727272790, 0.02651515151515151589, 0.03030303030303030387, 0.03409090909090908839, 0.03787878787878787984, 0.04166666666666666435, 0.04545454545454545581, 0.04924242424242424032, 0.05303030303030303177, 0.05681818181818181629, 0.06060606060606060774, 0.06439393939393939226, 0.06818181818181817677, 0.07196969696969697516, 0.07575757575757575968, 0.07954545454545454419, 0.08333333333333332871, 0.08712121212121212710, 0.09090909090909091161, 0.09469696969696969613, 0.09848484848484848064, 0.1022727272727272790, 0.1060606060606060635, 0.1098484848484848481, 0.1136363636363636326, 0.1174242424242424310, 0.1212121212121212155, 0.1250000000000000000, 0.1287878787878787845, 0.1325757575757575690, 0.1363636363636363535, 0.1401515151515151381, 0.1439393939393939503, 0.1477272727272727348, 0.1515151515151515194, 0.1553030303030303039, 0.1590909090909090884, 0.1628787878787878729, 0.1666666666666666574, 0.1704545454545454419, 0.1742424242424242542, 0.1780303030303030387, 0.1818181818181818232, 0.1856060606060606077, 0.1893939393939393923, 0.1931818181818181768, 0.1969696969696969613, 0.2007575757575757458, 0.2045454545454545581, 0.2083333333333333426, 0.2121212121212121271, 0.2159090909090909116, 0.2196969696969696961, 0.2234848484848484806, 0.2272727272727272652, 0.2310606060606060497, 0.2348484848484848619, 0.2386363636363636465, 0.2424242424242424310, 0.2462121212121212155, 0.2500000000000000000, 0.2537878787878787845, 0.2575757575757575690, 0.2613636363636363535, 0.2651515151515151381, 0.2689393939393939226, 0.2727272727272727071, 0.2765151515151514916, 0.2803030303030302761, 0.2840909090909091161, 0.2878787878787879007, 0.2916666666666666852, 0.2954545454545454697, 0.2992424242424242542, 0.3030303030303030387, 0.3068181818181818232, 0.3106060606060606077, 0.3143939393939393923, 0.3181818181818181768, 0.3219696969696969613, 0.3257575757575757458, 0.3295454545454545303, 0.3333333333333333148, 0.3371212121212120993, 0.3409090909090908839, 0.3446969696969697239, 0.3484848484848485084, 0.3522727272727272929, 0.3560606060606060774, 0.3598484848484848619, 0.3636363636363636465, 0.3674242424242424310, 0.3712121212121212155, 0.3750000000000000000, 0.3787878787878787845, 0.3825757575757575690, 0.3863636363636363535, 0.3901515151515151381, 0.3939393939393939226, 0.3977272727272727071, 0.4015151515151514916, 0.4053030303030302761, 0.4090909090909091161, 0.4128787878787879007, 0.4166666666666666852, 0.4204545454545454697, 0.4242424242424242542, 0.4280303030303030387, 0.4318181818181818232, 0.4356060606060606077, 0.4393939393939393923, 0.4431818181818181768, 0.4469696969696969613, 0.4507575757575757458, 0.4545454545454545303, 0.4583333333333333148, 0.4621212121212120993, 0.4659090909090908839, 0.4696969696969697239, 0.4734848484848485084, 0.4772727272727272929, 0.4810606060606060774, 0.4848484848484848619, 0.4886363636363636465, 0.4924242424242424310, 0.4962121212121212155, 0.5000000000000000000, 0.5037878787878787845, 0.5075757575757575690, 0.5113636363636363535, 0.5151515151515151381, 0.5189393939393939226, 0.5227272727272727071, 0.5265151515151514916, 0.5303030303030302761, 0.5340909090909090606, 0.5378787878787878451, 0.5416666666666666297, 0.5454545454545454142, 0.5492424242424241987, 0.5530303030303029832, 0.5568181818181817677, 0.5606060606060605522, 0.5643939393939394478, 0.5681818181818182323, 0.5719696969696970168, 0.5757575757575758013, 0.5795454545454545858, 0.5833333333333333703, 0.5871212121212121549, 0.5909090909090909394, 0.5946969696969697239, 0.5984848484848485084, 0.6022727272727272929, 0.6060606060606060774, 0.6098484848484848619, 0.6136363636363636465, 0.6174242424242424310, 0.6212121212121212155, 0.6250000000000000000, 0.6287878787878787845, 0.6325757575757575690, 0.6363636363636363535, 0.6401515151515151381, 0.6439393939393939226, 0.6477272727272727071, 0.6515151515151514916, 0.6553030303030302761, 0.6590909090909090606, 0.6628787878787878451, 0.6666666666666666297, 0.6704545454545454142, 0.6742424242424241987, 0.6780303030303029832, 0.6818181818181817677, 0.6856060606060605522, 0.6893939393939394478, 0.6931818181818182323, 0.6969696969696970168, 0.7007575757575758013, 0.7045454545454545858, 0.7083333333333333703, 0.7121212121212121549, 0.7159090909090909394, 0.7196969696969697239, 0.7234848484848485084, 0.7272727272727272929, 0.7310606060606060774, 0.7348484848484848619, 0.7386363636363636465, 0.7424242424242424310, 0.7462121212121212155, 0.7500000000000000000, 0.7537878787878787845, 0.7575757575757575690, 0.7613636363636363535, 0.7651515151515151381, 0.7689393939393939226, 0.7727272727272727071, 0.7765151515151514916, 0.7803030303030302761, 0.7840909090909090606, 0.7878787878787878451, 0.7916666666666666297, 0.7954545454545454142, 0.7992424242424241987, 0.8030303030303029832, 0.8068181818181817677, 0.8106060606060605522, 0.8143939393939394478, 0.8181818181818182323, 0.8219696969696970168, 0.8257575757575758013, 0.8295454545454545858, 0.8333333333333333703, 0.8371212121212121549, 0.8409090909090909394, 0.8446969696969697239, 0.8484848484848485084, 0.8522727272727272929, 0.8560606060606060774, 0.8598484848484848619, 0.8636363636363636465, 0.8674242424242424310, 0.8712121212121212155, 0.8750000000000000000, 0.8787878787878787845, 0.8825757575757575690, 0.8863636363636363535, 0.8901515151515151381, 0.8939393939393939226, 0.8977272727272727071, 0.9015151515151514916, 0.9053030303030302761, 0.9090909090909090606, 0.9128787878787878451, 0.9166666666666666297, 0.9204545454545454142, 0.9242424242424241987, 0.9280303030303029832, 0.9318181818181817677, 0.9356060606060605522, 0.9393939393939394478, 0.9431818181818182323, 0.9469696969696970168, 0.9507575757575758013, 0.9545454545454545858, 0.9583333333333333703, 0.9621212121212121549, 0.9659090909090909394 ),
 .UNSPECIFIED. ) 
 GEOMETRIC_REPRESENTATION_ITEM ( )  RATIONAL_B_SPLINE_SURFACE ( (
 ( 1.000000000000000000, 0.9659258262890683122, 1.000000000000000000, 0.9659258262890683122, 1.000000000000000000, 0.9659258262890683122, 1.000000000000000000, 0.9659258262890683122, 1.000000000000000000, 0.9659258262890683122, 1.000000000000000000, 0.9659258262890683122, 1.000000000000000000, 0.9659258262890683122, 1.000000000000000000, 0.9659258262890683122, 1.000000000000000000, 0.9659258262890683122, 1.000000000000000000, 0.9659258262890683122, 1.000000000000000000, 0.9659258262890683122, 1.000000000000000000, 0.9659258262890683122, 1.000000000000000000, 0.9659258262890683122, 1.000000000000000000, 0.9659258262890683122, 1.000000000000000000, 0.9659258262890683122, 1.000000000000000000, 0.9659258262890683122, 1.000000000000000000, 0.9659258262890683122, 1.000000000000000000, 0.9659258262890683122, 1.000000000000000000, 0.9659258262890683122, 1.000000000000000000, 0.9659258262890683122, 1.000000000000000000, 0.9659258262890683122, 1.000000000000000000, 0.9659258262890683122, 1.000000000000000000, 0.9659258262890683122, 1.000000000000000000, 0.9659258262890683122, 1.000000000000000000, 0.9659258262890683122, 1.000000000000000000, 0.9659258262890683122, 1.000000000000000000, 0.9659258262890683122, 1.000000000000000000, 0.9659258262890683122, 1.000000000000000000, 0.9659258262890683122, 1.000000000000000000, 0.9659258262890683122, 1.000000000000000000, 0.9659258262890683122, 1.000000000000000000, 0.9659258262890683122, 1.000000000000000000, 0.9659258262890683122, 1.000000000000000000, 0.9659258262890683122, 1.000000000000000000, 0.9659258262890683122, 1.000000000000000000, 0.9659258262890683122, 1.000000000000000000, 0.9659258262890683122, 1.000000000000000000, 0.9659258262890683122, 1.000000000000000000, 0.9659258262890683122, 1.000000000000000000, 0.9659258262890683122, 1.000000000000000000, 0.9659258262890683122, 1.000000000000000000, 0.9659258262890683122, 1.000000000000000000, 0.9659258262890683122, 1.000000000000000000, 0.9659258262890683122, 1.000000000000000000, 0.9659258262890683122, 1.000000000000000000, 0.9659258262890683122, 1.000000000000000000, 0.9659258262890683122, 1.000000000000000000, 0.9659258262890683122, 1.000000000000000000, 0.9659258262890683122, 1.000000000000000000, 0.9659258262890683122, 1.000000000000000000, 0.9659258262890683122, 1.000000000000000000, 0.9659258262890683122, 1.000000000000000000, 0.9659258262890683122, 1.000000000000000000, 0.9659258262890683122, 1.000000000000000000, 0.9659258262890683122, 1.000000000000000000, 0.9659258262890683122, 1.000000000000000000, 0.9659258262890683122, 1.000000000000000000, 0.9659258262890683122, 1.000000000000000000, 0.9659258262890683122, 1.000000000000000000, 0.9659258262890683122, 1.000000000000000000, 0.9659258262890683122, 1.000000000000000000, 0.9659258262890683122, 1.000000000000000000, 0.9659258262890683122, 1.000000000000000000, 0.9659258262890683122, 1.000000000000000000, 0.9659258262890683122, 1.000000000000000000, 0.9659258262890683122, 1.000000000000000000, 0.9659258262890683122, 1.000000000000000000, 0.9659258262890683122, 1.000000000000000000, 0.9659258262890683122, 1.000000000000000000, 0.9659258262890683122, 1.000000000000000000, 0.9659258262890683122, 1.000000000000000000, 0.9659258262890683122, 1.000000000000000000, 0.9659258262890683122, 1.000000000000000000, 0.9659258262890683122, 1.000000000000000000, 0.9659258262890683122, 1.000000000000000000, 0.9659258262890683122, 1.000000000000000000, 0.9659258262890683122, 1.000000000000000000, 0.9659258262890683122, 1.000000000000000000, 0.9659258262890683122, 1.000000000000000000, 0.9659258262890683122, 1.000000000000000000, 0.9659258262890683122, 1.000000000000000000, 0.9659258262890683122, 1.000000000000000000, 0.9659258262890683122, 1.000000000000000000, 0.9659258262890683122, 1.000000000000000000, 0.9659258262890683122, 1.000000000000000000, 0.9659258262890683122, 1.000000000000000000, 0.9659258262890683122, 1.000000000000000000, 0.9659258262890683122, 1.000000000000000000, 0.9659258262890683122, 1.000000000000000000, 0.9659258262890683122, 1.000000000000000000, 0.9659258262890683122, 1.000000000000000000, 0.9659258262890683122, 1.000000000000000000, 0.9659258262890683122, 1.000000000000000000, 0.9659258262890683122, 1.000000000000000000, 0.9659258262890683122, 1.000000000000000000, 0.9659258262890683122, 1.000000000000000000, 0.9659258262890683122, 1.000000000000000000, 0.9659258262890683122, 1.000000000000000000, 0.9659258262890683122, 1.000000000000000000, 0.9659258262890683122, 1.000000000000000000, 0.9659258262890683122, 1.000000000000000000, 0.9659258262890683122, 1.000000000000000000, 0.9659258262890683122, 1.000000000000000000, 0.9659258262890683122, 1.000000000000000000, 0.9659258262890683122, 1.000000000000000000, 0.9659258262890683122, 1.000000000000000000, 0.9659258262890683122, 1.000000000000000000, 0.9659258262890683122, 1.000000000000000000, 0.9659258262890683122, 1.000000000000000000, 0.9659258262890683122, 1.000000000000000000, 0.9659258262890683122, 1.000000000000000000, 0.9659258262890683122, 1.000000000000000000, 0.9659258262890683122, 1.000000000000000000, 0.9659258262890683122, 1.000000000000000000, 0.9659258262890683122, 1.000000000000000000, 0.9659258262890683122, 1.000000000000000000, 0.9659258262890683122, 1.000000000000000000, 0.9659258262890683122, 1.000000000000000000, 0.9659258262890683122, 1.000000000000000000, 0.9659258262890683122, 1.000000000000000000, 0.9659258262890683122, 1.000000000000000000, 0.9659258262890683122, 1.000000000000000000, 0.9659258262890683122, 1.000000000000000000, 0.9659258262890683122, 1.000000000000000000, 0.9659258262890683122, 1.000000000000000000, 0.9659258262890683122, 1.000000000000000000, 0.9659258262890683122, 1.000000000000000000, 0.9659258262890683122, 1.000000000000000000, 0.9659258262890683122, 1.000000000000000000, 0.9659258262890683122, 1.000000000000000000, 0.9659258262890683122, 1.000000000000000000, 0.9659258262890683122, 1.000000000000000000, 0.9659258262890683122, 1.000000000000000000, 0.9659258262890683122, 1.000000000000000000, 0.9659258262890683122, 1.000000000000000000, 0.9659258262890683122, 1.000000000000000000, 0.9659258262890683122, 1.000000000000000000, 0.9659258262890683122, 1.000000000000000000, 0.9659258262890683122, 1.000000000000000000, 0.9659258262890683122, 1.000000000000000000, 0.9659258262890683122, 1.000000000000000000, 0.9659258262890683122, 1.000000000000000000, 0.9659258262890683122, 1.000000000000000000, 0.9659258262890683122, 1.000000000000000000, 0.9659258262890683122, 1.000000000000000000, 0.9659258262890683122, 1.000000000000000000, 0.9659258262890683122, 1.000000000000000000, 0.9659258262890683122, 1.000000000000000000, 0.9659258262890683122, 1.000000000000000000, 0.9659258262890683122, 1.000000000000000000, 0.9659258262890683122, 1.000000000000000000, 0.9659258262890683122, 1.000000000000000000, 0.9659258262890683122, 1.000000000000000000, 0.9659258262890683122, 1.000000000000000000, 0.9659258262890683122, 1.000000000000000000, 0.9659258262890683122, 1.000000000000000000, 0.9659258262890683122, 1.000000000000000000, 0.9659258262890683122, 1.000000000000000000, 0.9659258262890683122, 1.000000000000000000, 0.9659258262890683122, 1.000000000000000000, 0.9659258262890683122, 1.000000000000000000, 0.9659258262890683122, 1.000000000000000000, 0.9659258262890683122, 1.000000000000000000, 0.9659258262890683122, 1.000000000000000000, 0.9659258262890683122, 1.000000000000000000, 0.9659258262890683122, 1.000000000000000000, 0.9659258262890683122, 1.000000000000000000, 0.9659258262890683122, 1.000000000000000000, 0.9659258262890683122, 1.000000000000000000, 0.9659258262890683122, 1.000000000000000000, 0.9659258262890683122, 1.000000000000000000, 0.9659258262890683122, 1.000000000000000000, 0.9659258262890683122, 1.000000000000000000, 0.9659258262890683122, 1.000000000000000000, 0.9659258262890683122, 1.000000000000000000, 0.9659258262890683122, 1.000000000000000000, 0.9659258262890683122, 1.000000000000000000, 0.9659258262890683122, 1.000000000000000000, 0.9659258262890683122, 1.000000000000000000, 0.9659258262890683122, 1.000000000000000000, 0.9659258262890683122, 1.000000000000000000, 0.9659258262890683122, 1.000000000000000000, 0.9659258262890683122, 1.000000000000000000, 0.9659258262890683122, 1.000000000000000000, 0.9659258262890683122, 1.000000000000000000, 0.9659258262890683122, 1.000000000000000000, 0.9659258262890683122, 1.000000000000000000, 0.9659258262890683122, 1.000000000000000000, 0.9659258262890683122, 1.000000000000000000, 0.9659258262890683122, 1.000000000000000000, 0.9659258262890683122, 1.000000000000000000, 0.9659258262890683122, 1.000000000000000000, 0.9659258262890683122, 1.000000000000000000, 0.9659258262890683122, 1.000000000000000000, 0.9659258262890683122, 1.000000000000000000, 0.9659258262890683122, 1.000000000000000000, 0.9659258262890683122, 1.000000000000000000, 0.9659258262890683122, 1.000000000000000000, 0.9659258262890683122, 1.000000000000000000, 0.9659258262890683122, 1.000000000000000000, 0.9659258262890683122, 1.000000000000000000, 0.9659258262890683122, 1.000000000000000000, 0.9659258262890683122, 1.000000000000000000, 0.9659258262890683122, 1.000000000000000000, 0.9659258262890683122, 1.000000000000000000, 0.9659258262890683122, 1.000000000000000000, 0.9659258262890683122, 1.000000000000000000, 0.9659258262890683122, 1.000000000000000000, 0.9659258262890683122, 1.000000000000000000, 0.9659258262890683122, 1.000000000000000000, 0.9659258262890683122, 1.000000000000000000, 0.9659258262890683122, 1.000000000000000000, 0.9659258262890683122, 1.000000000000000000, 0.9659258262890683122, 1.000000000000000000, 0.9659258262890683122, 1.000000000000000000, 0.9659258262890683122, 1.000000000000000000, 0.9659258262890683122, 1.000000000000000000, 0.9659258262890683122, 1.000000000000000000, 0.9659258262890683122, 1.000000000000000000, 0.9659258262890683122, 1.000000000000000000, 0.9659258262890683122, 1.000000000000000000, 0.9659258262890683122, 1.000000000000000000, 0.9659258262890683122, 1.000000000000000000, 0.9659258262890683122, 1.000000000000000000, 0.9659258262890683122, 1.000000000000000000, 0.9659258262890683122, 1.000000000000000000, 0.9659258262890683122, 1.000000000000000000, 0.9659258262890683122, 1.000000000000000000, 0.9659258262890683122, 1.000000000000000000, 0.9659258262890683122, 1.000000000000000000, 0.9659258262890683122, 1.000000000000000000, 0.9659258262890683122, 1.000000000000000000, 0.9659258262890683122, 1.000000000000000000, 0.9659258262890683122, 1.000000000000000000, 0.9659258262890683122, 1.000000000000000000, 0.9659258262890683122, 1.000000000000000000, 0.9659258262890683122, 1.000000000000000000, 0.9659258262890683122, 1.000000000000000000, 0.9659258262890683122, 1.000000000000000000, 0.9659258262890683122, 1.000000000000000000, 0.9659258262890683122, 1.000000000000000000, 0.9659258262890683122, 1.000000000000000000, 0.9659258262890683122, 1.000000000000000000, 0.9659258262890683122, 1.000000000000000000, 0.9659258262890683122, 1.000000000000000000, 0.9659258262890683122, 1.000000000000000000, 0.9659258262890683122, 1.000000000000000000, 0.9659258262890683122, 1.000000000000000000, 0.9659258262890683122, 1.000000000000000000, 0.9659258262890683122, 1.000000000000000000, 0.9659258262890683122, 1.000000000000000000, 0.9659258262890683122, 1.000000000000000000, 0.9659258262890683122, 1.000000000000000000, 0.9659258262890683122, 1.000000000000000000, 0.9659258262890683122, 1.000000000000000000),
 ( 1.000000000000000000, 0.9659258262890683122, 1.000000000000000000, 0.9659258262890683122, 1.000000000000000000, 0.9659258262890683122, 1.000000000000000000, 0.9659258262890683122, 1.000000000000000000, 0.9659258262890683122, 1.000000000000000000, 0.9659258262890683122, 1.000000000000000000, 0.9659258262890683122, 1.000000000000000000, 0.9659258262890683122, 1.000000000000000000, 0.9659258262890683122, 1.000000000000000000, 0.9659258262890683122, 1.000000000000000000, 0.9659258262890683122, 1.000000000000000000, 0.9659258262890683122, 1.000000000000000000, 0.9659258262890683122, 1.000000000000000000, 0.9659258262890683122, 1.000000000000000000, 0.9659258262890683122, 1.000000000000000000, 0.9659258262890683122, 1.000000000000000000, 0.9659258262890683122, 1.000000000000000000, 0.9659258262890683122, 1.000000000000000000, 0.9659258262890683122, 1.000000000000000000, 0.9659258262890683122, 1.000000000000000000, 0.9659258262890683122, 1.000000000000000000, 0.9659258262890683122, 1.000000000000000000, 0.9659258262890683122, 1.000000000000000000, 0.9659258262890683122, 1.000000000000000000, 0.9659258262890683122, 1.000000000000000000, 0.9659258262890683122, 1.000000000000000000, 0.9659258262890683122, 1.000000000000000000, 0.9659258262890683122, 1.000000000000000000, 0.9659258262890683122, 1.000000000000000000, 0.9659258262890683122, 1.000000000000000000, 0.9659258262890683122, 1.000000000000000000, 0.9659258262890683122, 1.000000000000000000, 0.9659258262890683122, 1.000000000000000000, 0.9659258262890683122, 1.000000000000000000, 0.9659258262890683122, 1.000000000000000000, 0.9659258262890683122, 1.000000000000000000, 0.9659258262890683122, 1.000000000000000000, 0.9659258262890683122, 1.000000000000000000, 0.9659258262890683122, 1.000000000000000000, 0.9659258262890683122, 1.000000000000000000, 0.9659258262890683122, 1.000000000000000000, 0.9659258262890683122, 1.000000000000000000, 0.9659258262890683122, 1.000000000000000000, 0.9659258262890683122, 1.000000000000000000, 0.9659258262890683122, 1.000000000000000000, 0.9659258262890683122, 1.000000000000000000, 0.9659258262890683122, 1.000000000000000000, 0.9659258262890683122, 1.000000000000000000, 0.9659258262890683122, 1.000000000000000000, 0.9659258262890683122, 1.000000000000000000, 0.9659258262890683122, 1.000000000000000000, 0.9659258262890683122, 1.000000000000000000, 0.9659258262890683122, 1.000000000000000000, 0.9659258262890683122, 1.000000000000000000, 0.9659258262890683122, 1.000000000000000000, 0.9659258262890683122, 1.000000000000000000, 0.9659258262890683122, 1.000000000000000000, 0.9659258262890683122, 1.000000000000000000, 0.9659258262890683122, 1.000000000000000000, 0.9659258262890683122, 1.000000000000000000, 0.9659258262890683122, 1.000000000000000000, 0.9659258262890683122, 1.000000000000000000, 0.9659258262890683122, 1.000000000000000000, 0.9659258262890683122, 1.000000000000000000, 0.9659258262890683122, 1.000000000000000000, 0.9659258262890683122, 1.000000000000000000, 0.9659258262890683122, 1.000000000000000000, 0.9659258262890683122, 1.000000000000000000, 0.9659258262890683122, 1.000000000000000000, 0.9659258262890683122, 1.000000000000000000, 0.9659258262890683122, 1.000000000000000000, 0.9659258262890683122, 1.000000000000000000, 0.9659258262890683122, 1.000000000000000000, 0.9659258262890683122, 1.000000000000000000, 0.9659258262890683122, 1.000000000000000000, 0.9659258262890683122, 1.000000000000000000, 0.9659258262890683122, 1.000000000000000000, 0.9659258262890683122, 1.000000000000000000, 0.9659258262890683122, 1.000000000000000000, 0.9659258262890683122, 1.000000000000000000, 0.9659258262890683122, 1.000000000000000000, 0.9659258262890683122, 1.000000000000000000, 0.9659258262890683122, 1.000000000000000000, 0.9659258262890683122, 1.000000000000000000, 0.9659258262890683122, 1.000000000000000000, 0.9659258262890683122, 1.000000000000000000, 0.9659258262890683122, 1.000000000000000000, 0.9659258262890683122, 1.000000000000000000, 0.9659258262890683122, 1.000000000000000000, 0.9659258262890683122, 1.000000000000000000, 0.9659258262890683122, 1.000000000000000000, 0.9659258262890683122, 1.000000000000000000, 0.9659258262890683122, 1.000000000000000000, 0.9659258262890683122, 1.000000000000000000, 0.9659258262890683122, 1.000000000000000000, 0.9659258262890683122, 1.000000000000000000, 0.9659258262890683122, 1.000000000000000000, 0.9659258262890683122, 1.000000000000000000, 0.9659258262890683122, 1.000000000000000000, 0.9659258262890683122, 1.000000000000000000, 0.9659258262890683122, 1.000000000000000000, 0.9659258262890683122, 1.000000000000000000, 0.9659258262890683122, 1.000000000000000000, 0.9659258262890683122, 1.000000000000000000, 0.9659258262890683122, 1.000000000000000000, 0.9659258262890683122, 1.000000000000000000, 0.9659258262890683122, 1.000000000000000000, 0.9659258262890683122, 1.000000000000000000, 0.9659258262890683122, 1.000000000000000000, 0.9659258262890683122, 1.000000000000000000, 0.9659258262890683122, 1.000000000000000000, 0.9659258262890683122, 1.000000000000000000, 0.9659258262890683122, 1.000000000000000000, 0.9659258262890683122, 1.000000000000000000, 0.9659258262890683122, 1.000000000000000000, 0.9659258262890683122, 1.000000000000000000, 0.9659258262890683122, 1.000000000000000000, 0.9659258262890683122, 1.000000000000000000, 0.9659258262890683122, 1.000000000000000000, 0.9659258262890683122, 1.000000000000000000, 0.9659258262890683122, 1.000000000000000000, 0.9659258262890683122, 1.000000000000000000, 0.9659258262890683122, 1.000000000000000000, 0.9659258262890683122, 1.000000000000000000, 0.9659258262890683122, 1.000000000000000000, 0.9659258262890683122, 1.000000000000000000, 0.9659258262890683122, 1.000000000000000000, 0.9659258262890683122, 1.000000000000000000, 0.9659258262890683122, 1.000000000000000000, 0.9659258262890683122, 1.000000000000000000, 0.9659258262890683122, 1.000000000000000000, 0.9659258262890683122, 1.000000000000000000, 0.9659258262890683122, 1.000000000000000000, 0.9659258262890683122, 1.000000000000000000, 0.9659258262890683122, 1.000000000000000000, 0.9659258262890683122, 1.000000000000000000, 0.9659258262890683122, 1.000000000000000000, 0.9659258262890683122, 1.000000000000000000, 0.9659258262890683122, 1.000000000000000000, 0.9659258262890683122, 1.000000000000000000, 0.9659258262890683122, 1.000000000000000000, 0.9659258262890683122, 1.000000000000000000, 0.9659258262890683122, 1.000000000000000000, 0.9659258262890683122, 1.000000000000000000, 0.9659258262890683122, 1.000000000000000000, 0.9659258262890683122, 1.000000000000000000, 0.9659258262890683122, 1.000000000000000000, 0.9659258262890683122, 1.000000000000000000, 0.9659258262890683122, 1.000000000000000000, 0.9659258262890683122, 1.000000000000000000, 0.9659258262890683122, 1.000000000000000000, 0.9659258262890683122, 1.000000000000000000, 0.9659258262890683122, 1.000000000000000000, 0.9659258262890683122, 1.000000000000000000, 0.9659258262890683122, 1.000000000000000000, 0.9659258262890683122, 1.000000000000000000, 0.9659258262890683122, 1.000000000000000000, 0.9659258262890683122, 1.000000000000000000, 0.9659258262890683122, 1.000000000000000000, 0.9659258262890683122, 1.000000000000000000, 0.9659258262890683122, 1.000000000000000000, 0.9659258262890683122, 1.000000000000000000, 0.9659258262890683122, 1.000000000000000000, 0.9659258262890683122, 1.000000000000000000, 0.9659258262890683122, 1.000000000000000000, 0.9659258262890683122, 1.000000000000000000, 0.9659258262890683122, 1.000000000000000000, 0.9659258262890683122, 1.000000000000000000, 0.9659258262890683122, 1.000000000000000000, 0.9659258262890683122, 1.000000000000000000, 0.9659258262890683122, 1.000000000000000000, 0.9659258262890683122, 1.000000000000000000, 0.9659258262890683122, 1.000000000000000000, 0.9659258262890683122, 1.000000000000000000, 0.9659258262890683122, 1.000000000000000000, 0.9659258262890683122, 1.000000000000000000, 0.9659258262890683122, 1.000000000000000000, 0.9659258262890683122, 1.000000000000000000, 0.9659258262890683122, 1.000000000000000000, 0.9659258262890683122, 1.000000000000000000, 0.9659258262890683122, 1.000000000000000000, 0.9659258262890683122, 1.000000000000000000, 0.9659258262890683122, 1.000000000000000000, 0.9659258262890683122, 1.000000000000000000, 0.9659258262890683122, 1.000000000000000000, 0.9659258262890683122, 1.000000000000000000, 0.9659258262890683122, 1.000000000000000000, 0.9659258262890683122, 1.000000000000000000, 0.9659258262890683122, 1.000000000000000000, 0.9659258262890683122, 1.000000000000000000, 0.9659258262890683122, 1.000000000000000000, 0.9659258262890683122, 1.000000000000000000, 0.9659258262890683122, 1.000000000000000000, 0.9659258262890683122, 1.000000000000000000, 0.9659258262890683122, 1.000000000000000000, 0.9659258262890683122, 1.000000000000000000, 0.9659258262890683122, 1.000000000000000000, 0.9659258262890683122, 1.000000000000000000, 0.9659258262890683122, 1.000000000000000000, 0.9659258262890683122, 1.000000000000000000, 0.9659258262890683122, 1.000000000000000000, 0.9659258262890683122, 1.000000000000000000, 0.9659258262890683122, 1.000000000000000000, 0.9659258262890683122, 1.000000000000000000, 0.9659258262890683122, 1.000000000000000000, 0.9659258262890683122, 1.000000000000000000, 0.9659258262890683122, 1.000000000000000000, 0.9659258262890683122, 1.000000000000000000, 0.9659258262890683122, 1.000000000000000000, 0.9659258262890683122, 1.000000000000000000, 0.9659258262890683122, 1.000000000000000000, 0.9659258262890683122, 1.000000000000000000, 0.9659258262890683122, 1.000000000000000000, 0.9659258262890683122, 1.000000000000000000, 0.9659258262890683122, 1.000000000000000000, 0.9659258262890683122, 1.000000000000000000, 0.9659258262890683122, 1.000000000000000000, 0.9659258262890683122, 1.000000000000000000, 0.9659258262890683122, 1.000000000000000000, 0.9659258262890683122, 1.000000000000000000, 0.9659258262890683122, 1.000000000000000000, 0.9659258262890683122, 1.000000000000000000, 0.9659258262890683122, 1.000000000000000000, 0.9659258262890683122, 1.000000000000000000, 0.9659258262890683122, 1.000000000000000000, 0.9659258262890683122, 1.000000000000000000, 0.9659258262890683122, 1.000000000000000000, 0.9659258262890683122, 1.000000000000000000, 0.9659258262890683122, 1.000000000000000000, 0.9659258262890683122, 1.000000000000000000, 0.9659258262890683122, 1.000000000000000000, 0.9659258262890683122, 1.000000000000000000, 0.9659258262890683122, 1.000000000000000000, 0.9659258262890683122, 1.000000000000000000, 0.9659258262890683122, 1.000000000000000000, 0.9659258262890683122, 1.000000000000000000, 0.9659258262890683122, 1.000000000000000000, 0.9659258262890683122, 1.000000000000000000, 0.9659258262890683122, 1.000000000000000000, 0.9659258262890683122, 1.000000000000000000, 0.9659258262890683122, 1.000000000000000000, 0.9659258262890683122, 1.000000000000000000, 0.9659258262890683122, 1.000000000000000000, 0.9659258262890683122, 1.000000000000000000, 0.9659258262890683122, 1.000000000000000000, 0.9659258262890683122, 1.000000000000000000, 0.9659258262890683122, 1.000000000000000000, 0.9659258262890683122, 1.000000000000000000, 0.9659258262890683122, 1.000000000000000000, 0.9659258262890683122, 1.000000000000000000, 0.9659258262890683122, 1.000000000000000000, 0.9659258262890683122, 1.000000000000000000, 0.9659258262890683122, 1.000000000000000000, 0.9659258262890683122, 1.000000000000000000, 0.9659258262890683122, 1.000000000000000000) ) ) 
 REPRESENTATION_ITEM ( '' )  SURFACE ( )  );
#6384 = CARTESIAN_POINT ( 'NONE',  ( 0.5314960629921294810, 2.755905511811024056, -0.9881811337016621621 ) ) ;
#6385 = CARTESIAN_POINT ( 'NONE',  ( -0.5314960629921325896, 2.742776589945747467, 1.881759001202176318 ) ) ;
#6386 = VERTEX_POINT ( 'NONE', #11032 ) ;
#6387 = CARTESIAN_POINT ( 'NONE',  ( 4.797336870675656522E-17, -0.3917322834645670659, -2.122722727855329783 ) ) ;
#6388 = CARTESIAN_POINT ( 'NONE',  ( 0.4068241469816281097, 0.05413385826771666132, 0.4176697321401328100 ) ) ;
#6389 = ORIENTED_EDGE ( 'NONE', *, *, #38792, .F. ) ;
#6390 = CARTESIAN_POINT ( 'NONE',  ( -0.8727034120734901146, -0.05778040916215560624, -0.4822834645669293319 ) ) ;
#6391 = EDGE_CURVE ( 'NONE', #80751, #26586, #62364, .T. ) ;
#6392 = CARTESIAN_POINT ( 'NONE',  ( 1.364829396325459854, -0.6046776061558809534, -0.2411417322834644161 ) ) ;
#6393 = CARTESIAN_POINT ( 'NONE',  ( 0.5183727034120741983, 0.2952755905511810774, -0.1292274648535930714 ) ) ;
#6394 = CARTESIAN_POINT ( 'NONE',  ( 0.2165354330708668673, -0.5400638737290844871, 0.3530559997133364547 ) ) ;
#6395 = CARTESIAN_POINT ( 'NONE',  ( -0.3392501089628017219, -0.1958661417322836718, -1.396981627296587813 ) ) ;
#6396 = CARTESIAN_POINT ( 'NONE',  ( -0.7939632545931754048, -0.3162353388693405765, 0.4822834645669290543 ) ) ;
#6397 = CARTESIAN_POINT ( 'NONE',  ( -0.09186351706036663400, -0.4281496062992124485, 0.4176697321401328655 ) ) ;
#6398 = CARTESIAN_POINT ( 'NONE',  ( 0.07217847769028949700, -0.2845877964562159024, 0.3641732283464567677 ) ) ;
#6399 = CARTESIAN_POINT ( 'NONE',  ( -0.04037479286078369395, 0.3917864676224473985, 9.485496803828532453E-13 ) ) ;
#6400 = CARTESIAN_POINT ( 'NONE',  ( 0.01968503937007930540, 0.1660481256975885056, 0.3530559997133364547 ) ) ;
#6401 = CARTESIAN_POINT ( 'NONE',  ( 0.1265901696524990572, -0.4724409448818897017, -0.9494750656167977310 ) ) ;
#6402 = EDGE_CURVE ( 'NONE', #29384, #60118, #28731, .T. ) ;
#6403 = CARTESIAN_POINT ( 'NONE',  ( 0.9908136482939640111, 0.2952755905511810774, -0.1292274648535930714 ) ) ;
#6404 = CARTESIAN_POINT ( 'NONE',  ( 3.934067344273005418, 1.088024857645069288, -0.1528641246056967884 ) ) ;
#6405 = ORIENTED_EDGE ( 'NONE', *, *, #83038, .F. ) ;
#6406 = ORIENTED_EDGE ( 'NONE', *, *, #10993, .F. ) ;
#6407 = CARTESIAN_POINT ( 'NONE',  ( 0.2034120734908144990, -0.6692913385826771977, 0.1292274648535927661 ) ) ;
#6408 = CARTESIAN_POINT ( 'NONE',  ( -0.2624671916010490880, 0.1283753931104746893, -0.1820866141732285504 ) ) ;
#6410 = CARTESIAN_POINT ( 'NONE',  ( 5.785732909357575061E-17, -0.4724409448818898682, -0.3937007874015748254 ) ) ;
#6409 = CARTESIAN_POINT ( 'NONE',  ( 1.646981627296588035, -0.2845877964562159024, 0.3641732283464567677 ) ) ;
#6411 = CARTESIAN_POINT ( 'NONE',  ( -0.2867679344610365999, 0.2867679344610364889, -1.206692913385826627 ) ) ;
#6412 = CARTESIAN_POINT ( 'NONE',  ( 0.4724409448818898682, 2.892866454678787531E-17, -0.3523622047244094335 ) ) ;
#6413 = CARTESIAN_POINT ( 'NONE',  ( 1.430446194225722500, -0.3690944881889765550, -0.3153832671262227771 ) ) ;
#6414 = B_SPLINE_CURVE_WITH_KNOTS ( 'NONE', 3,
 ( #60719, #61961, #73363, #22426, #23241, #54816, #73785, #2660, #3897, #42595, #16539, #53980 ),
 .UNSPECIFIED., .F., .F.,
 ( 4, 2, 2, 2, 2, 4 ),
 ( 0.05454303362711762637, 0.05585633982237121070, 0.05651299291999801327, 0.05716964601762482279, 0.05848295221287842793, 0.05979625840813203308 ),
 .UNSPECIFIED. ) ;
#6415 = CARTESIAN_POINT ( 'NONE',  ( -1.541994750656167090, -0.6692913385826773087, -0.1292274648535924053 ) ) ;
#6416 = CARTESIAN_POINT ( 'NONE',  ( 0.3949938075777408852, 0.1058382717557500435, 0.1135170603674540979 ) ) ;
#6417 = CARTESIAN_POINT ( 'NONE',  ( -0.1246719160104980823, 0.2952755905511811885, 0.1292274648535926551 ) ) ;
#6418 = CARTESIAN_POINT ( 'NONE',  ( -1.062992125984250968, -0.6692913385826771977, 8.415575281601705876E-17 ) ) ;
#6419 = CARTESIAN_POINT ( 'NONE',  ( -1.017060367454067249, -0.3162353388693409650, -0.4822834645669289433 ) ) ;
#6420 = CARTESIAN_POINT ( 'NONE',  ( 0.4330708661417329575, -0.6692913385826771977, 8.415575281601705876E-17 ) ) ;
#6421 = CARTESIAN_POINT ( 'NONE',  ( 0.1058382717557499880, 0.3949938075777409408, 0.08727034120734906975 ) ) ;
#6422 = CARTESIAN_POINT ( 'NONE',  ( -1.528871391076114250, -0.5511811023622046335, 0.09757992244046803654 ) ) ;
#6423 = CARTESIAN_POINT ( 'NONE',  ( 0.7677165354330716118, -0.5400638737290844871, 0.3530559997133364547 ) ) ;
#6424 = CARTESIAN_POINT ( 'NONE',  ( 0.7742782152230979209, -0.004921259842519870586, -0.3153832671262229437 ) ) ;
#6425 = CARTESIAN_POINT ( 'NONE',  ( 0.8005249343832027131, 0.009842519685039463617, 0.3409548833797002576 ) ) ;
#6426 = CARTESIAN_POINT ( 'NONE',  ( 1.023622047244095334, -0.1870078740157479769, 0.3641732283464567677 ) ) ;
#6427 = CARTESIAN_POINT ( 'NONE',  ( -1.469816272965878357, 0.2306618581243848609, 0.2411417322834645549 ) ) ;
#6428 = CARTESIAN_POINT ( 'NONE',  ( -0.1998031496062991630, -0.3460692066303959202, -1.087270341207349000 ) ) ;
#6429 = CARTESIAN_POINT ( 'NONE',  ( 1.135170603674541256, -0.6692913385826773087, -0.1292274648535924053 ) ) ;
#6430 = CARTESIAN_POINT ( 'NONE',  ( -9.594673741351313045E-17, 0.3917322834645670104, -0.1496062992125983815 ) ) ;
#6432 = CARTESIAN_POINT ( 'NONE',  ( -0.4255991402441413052, 1.325803004855072187, 2.077093529568096120 ) ) ;
#6431 = CARTESIAN_POINT ( 'NONE',  ( 0.5446194225721792126, -0.3162353388693405765, 0.4822834645669290543 ) ) ;
#6433 = CARTESIAN_POINT ( 'NONE',  ( -1.456692913385826182, -0.5511811023622047445, 6.969142054262312111E-17 ) ) ;
#6434 = CARTESIAN_POINT ( 'NONE',  ( 0.08530183727034192087, -0.05778040916215522460, 0.4822834645669289988 ) ) ;
#6435 = CARTESIAN_POINT ( 'NONE',  ( 0.3215223097112867578, -0.08942795157527998196, 0.3641732283464567121 ) ) ;
#6436 = CARTESIAN_POINT ( 'NONE',  ( 0.9908136482939640111, -0.6692913385826771977, 0.1292274648535927661 ) ) ;
#6437 = DIRECTION ( 'NONE',  ( 0.000000000000000000, 0.000000000000000000, -1.000000000000000000 ) ) ;
#6438 = CARTESIAN_POINT ( 'NONE',  ( -0.4986876640419942164, -0.5023911411419708095, 0.1820866141732285504 ) ) ;
#6439 = CARTESIAN_POINT ( 'NONE',  ( -0.7611548556430438595, 0.2306618581243848609, 0.2411417322834645549 ) ) ;
#6440 = CARTESIAN_POINT ( 'NONE',  ( 1.673228346456693494, 0.1660481256975885056, 0.3530559997133364547 ) ) ;
#6441 = CARTESIAN_POINT ( 'NONE',  ( -1.089238845144356427, 0.05413385826771666132, 0.4176697321401328100 ) ) ;
#6442 = CARTESIAN_POINT ( 'NONE',  ( 0.9383202099737538715, -0.05778040916215560624, -0.4822834645669293319 ) ) ;
#6443 = CARTESIAN_POINT ( 'NONE',  ( 0.3917322834645670104, 0.1049643490035304660, -0.9088119667004745938 ) ) ;
#6444 = CARTESIAN_POINT ( 'NONE',  ( -1.272965879265091305, -0.004921259842519870586, -0.3153832671262229437 ) ) ;
#6445 = CARTESIAN_POINT ( 'NONE',  ( 1.022505811683676713, 1.428663316172101627, 0.4620424953995453943 ) ) ;
#6446 = CARTESIAN_POINT ( 'NONE',  ( 1.069553805774278610, -0.6692913385826771977, 0.1292274648535927661 ) ) ;
#6447 = VECTOR ( 'NONE', #46627, 39.37007874015748854 ) ;
#6448 = CARTESIAN_POINT ( 'NONE',  ( 0.3458507752293908943, 0.3458507752293908943, -2.261811023622047223 ) ) ;
#6449 = CARTESIAN_POINT ( 'NONE',  ( -1.535433070866141225, 0.2952755905511811885, 0.000000000000000000 ) ) ;
#6450 = CARTESIAN_POINT ( 'NONE',  ( -1.509186351706035767, -0.3690944881889763329, 0.3153832671262228327 ) ) ;
#6451 = CARTESIAN_POINT ( 'NONE',  ( -1.003937007874015297, -0.4536011799217368745, -0.2665933059059886201 ) ) ;
#6452 = CARTESIAN_POINT ( 'NONE',  ( 1.171093442848939681, -8.644661201599092366E-16, -0.4445507791589066171 ) ) ;
#6453 = CARTESIAN_POINT ( 'NONE',  ( -0.4461942257217840213, -0.6046776061558809534, -0.2411417322834644161 ) ) ;
#6454 = CARTESIAN_POINT ( 'NONE',  ( -0.2821522309711278487, -0.5511811023622048555, -0.09757992244046775898 ) ) ;
#6455 = CARTESIAN_POINT ( 'NONE',  ( -1.541994750656167090, 0.1771653543307087630, 0.09757992244046791164 ) ) ;
#6456 = CARTESIAN_POINT ( 'NONE',  ( 0.8202099737532813073, 0.1771653543307087630, 0.09757992244046791164 ) ) ;
#6457 = CARTESIAN_POINT ( 'NONE',  ( 0.4199475065616805614, 0.2306618581243848609, 0.2411417322834645549 ) ) ;
#6458 = CARTESIAN_POINT ( 'NONE',  ( 1.568241469816273437, -0.3162353388693405765, 0.4822834645669290543 ) ) ;
#6459 = CARTESIAN_POINT ( 'NONE',  ( 0.2230971128608932319, -0.3690944881889763329, 0.3153832671262228327 ) ) ;
#6460 = CARTESIAN_POINT ( 'NONE',  ( 0.6758530183727039509, -0.6692913385826771977, 0.1292274648535927661 ) ) ;
#6461 = CARTESIAN_POINT ( 'NONE',  ( 0.6561679790026253567, 0.1283753931104748280, 0.1820866141732283561 ) ) ;
#6462 = CARTESIAN_POINT ( 'NONE',  ( 1.535433070866142335, -0.6692913385826771977, 8.415575281601705876E-17 ) ) ;
#6463 = CARTESIAN_POINT ( 'NONE',  ( -1.174540682414697335, -0.05778040916215522460, 0.4822834645669289988 ) ) ;
#6464 = CARTESIAN_POINT ( 'NONE',  ( -0.4461942257217840213, 0.2306618581243848609, 0.2411417322834645549 ) ) ;
#6465 = CARTESIAN_POINT ( 'NONE',  ( 0.3460692066303959202, 0.1998031496062993295, -0.2887139107611548794 ) ) ;
#6466 = CARTESIAN_POINT ( 'NONE',  ( -0.3460692066303957537, -0.1998031496062994405, -2.491469816272966042 ) ) ;
#6467 = CARTESIAN_POINT ( 'NONE',  ( 0.6167979002624678353, -0.4281496062992124485, 0.4176697321401328655 ) ) ;
#6468 = CARTESIAN_POINT ( 'NONE',  ( 1.102362204724410155, -0.1870078740157479769, 0.3641732283464567677 ) ) ;
#6469 = CARTESIAN_POINT ( 'NONE',  ( -0.3018372703412066094, -0.4281496062992127816, -0.4176697321401328100 ) ) ;
#6470 = CARTESIAN_POINT ( 'NONE',  ( 0.3937007874015754361, -0.1870078740157480879, -0.4822834645669291653 ) ) ;
#6471 = EDGE_CURVE ( 'NONE', #74748, #6972, #29553, .T. ) ;
#6472 = CARTESIAN_POINT ( 'NONE',  ( 0.2925321140481932369, -0.2925321140481932369, -2.303149606299212060 ) ) ;
#6473 = CARTESIAN_POINT ( 'NONE',  ( 0.2891555358219910499, 0.2891555358219910499, -2.027559055118110631 ) ) ;
#6474 = CARTESIAN_POINT ( 'NONE',  ( 0.3460692066303959757, -0.1998031496062991907, -2.939632545931758489 ) ) ;
#6475 = DIRECTION ( 'NONE',  ( 0.000000000000000000, -1.000000000000000000, 0.000000000000000000 ) ) ;
#6476 = CARTESIAN_POINT ( 'NONE',  ( 0.1049643490035303689, 0.3917322834645670104, -0.9304461942257216123 ) ) ;
#6477 = EDGE_CURVE ( 'NONE', #8202, #1055, #56763, .T. ) ;
#6478 = CARTESIAN_POINT ( 'NONE',  ( -0.8727034120734901146, -0.08942795157528024563, -0.3641732283464568787 ) ) ;
#6479 = CARTESIAN_POINT ( 'NONE',  ( -0.9711286089238838626, -0.6046776061558807314, 0.2411417322834647770 ) ) ;
#6480 = CARTESIAN_POINT ( 'NONE',  ( 0.1974969037888704704, 0.3420746716998660508, -2.740813648293963567 ) ) ;
#6481 = CARTESIAN_POINT ( 'NONE',  ( 0.9383202099737538715, -0.05778040916215560624, -0.4822834645669293319 ) ) ;
#6482 = CARTESIAN_POINT ( 'NONE',  ( 1.325459317585302665, 0.05413385826771626580, -0.4176697321401330321 ) ) ;
#6483 = CARTESIAN_POINT ( 'NONE',  ( 0.9711286089238851948, 0.2306618581243848609, 0.2411417322834645549 ) ) ;
#6484 = CARTESIAN_POINT ( 'NONE',  ( -0.6175017169405814244, 0.000000000000000000, 0.3464511005275205946 ) ) ;
#6485 = CARTESIAN_POINT ( 'NONE',  ( 0.3460692066303959757, -0.1998031496062991907, -2.152230971128608950 ) ) ;
#6486 = CARTESIAN_POINT ( 'NONE',  ( 0.3917322834645670659, 2.398668435337828261E-17, -0.7447699719498183102 ) ) ;
#6487 = CARTESIAN_POINT ( 'NONE',  ( 1.620734908136483465, -0.6692913385826771977, 0.1292274648535927661 ) ) ;
#6488 = CARTESIAN_POINT ( 'NONE',  ( 0.6889763779527563470, 0.1660481256975883668, -0.3530559997133364547 ) ) ;
#6489 = CARTESIAN_POINT ( 'NONE',  ( 0.1640419947506569498, -0.05778040916215522460, 0.4822834645669289988 ) ) ;
#6490 = CARTESIAN_POINT ( 'NONE',  ( 0.9055118110236227702, -0.5511811023622047445, 6.969142054262312111E-17 ) ) ;
#6491 = CARTESIAN_POINT ( 'NONE',  ( 1.325459317585302665, -0.4281496062992124485, 0.4176697321401328655 ) ) ;
#6492 = CARTESIAN_POINT ( 'NONE',  ( -0.3917322834645671215, 0.1049643490035301469, -0.2749343832020998413 ) ) ;
#6493 = CARTESIAN_POINT ( 'NONE',  ( 0.5249343832021003964, 0.2306618581243847221, -0.2411417322834647770 ) ) ;
#6494 = CARTESIAN_POINT ( 'NONE',  ( 1.266404199475066328, -0.3162353388693409650, -0.4822834645669289433 ) ) ;
#6495 = CARTESIAN_POINT ( 'NONE',  ( 0.3871391076115493490, -0.3162353388693405765, 0.4822834645669290543 ) ) ;
#6496 = CARTESIAN_POINT ( 'NONE',  ( 1.200787401574803681, 0.07958543189024085140, 0.2665933059059887866 ) ) ;
#6497 = CARTESIAN_POINT ( 'NONE',  ( -0.9973753280839886548, -0.6046776061558809534, -0.2411417322834644161 ) ) ;
#6498 = CARTESIAN_POINT ( 'NONE',  ( -0.8202099737532801971, -0.6692913385826771977, 0.1292274648535927661 ) ) ;
#6499 = CARTESIAN_POINT ( 'NONE',  ( 1.102362204724410155, -0.1870078740157479769, 0.4822834645669291653 ) ) ;
#6500 = CARTESIAN_POINT ( 'NONE',  ( -0.1958661417322836718, 0.3392501089628017219, -0.4127296587926510552 ) ) ;
#6501 = CARTESIAN_POINT ( 'NONE',  ( 0.2867679344610365999, -0.2867679344610365444, -1.665354330708661124 ) ) ;
#6502 = CARTESIAN_POINT ( 'NONE',  ( -0.3917322834645670104, -7.196005306013484475E-17, -2.551181102362204633 ) ) ;
#6503 = ORIENTED_EDGE ( 'NONE', *, *, #83098, .F. ) ;
#6504 = CARTESIAN_POINT ( 'NONE',  ( -0.1998031496062994683, 0.3460692066303958092, 0.1443569553805774119 ) ) ;
#6505 = ORIENTED_EDGE ( 'NONE', *, *, #45400, .T. ) ;
#6506 = B_SPLINE_CURVE_WITH_KNOTS ( 'NONE', 3,
 ( #5193, #57762, #37997, #38415, #19057, #82225, #18246, #37586, #64096, #56523, #25363, #6432, #70834, #64511, #18651, #13182, #38832, #11521, #75907, #51026, #76725, #57344, #31267, #6848, #26202, #25779, #6014, #82629, #69170, #24943 ),
 .UNSPECIFIED., .F., .F.,
 ( 4, 2, 2, 2, 2, 2, 2, 2, 2, 2, 2, 2, 2, 2, 4 ),
 ( 0.01323639539072392693, 0.01388240907739107452, 0.01452842276405822385, 0.01582045013739251382, 0.01711247751072680900, 0.01840450488406109725, 0.02098855963072968414, 0.02357261437739826757, 0.02486464175073256622, 0.02615666912406686487, 0.02744869649740116352, 0.02874072387073546564, 0.03132477861740406294, 0.03261680599073836506, 0.03390883336407266024 ),
 .UNSPECIFIED. ) ;
#6507 = CARTESIAN_POINT ( 'NONE',  ( 1.463254593175853824, -0.6692913385826771977, 0.1292274648535927661 ) ) ;
#6508 = CARTESIAN_POINT ( 'NONE',  ( 1.135170603674541256, 0.1771653543307087630, 0.09757992244046791164 ) ) ;
#6509 = CARTESIAN_POINT ( 'NONE',  ( -9.787531504996567848E-17, 0.3996062992125986035, -1.259842519685039353 ) ) ;
#6510 = CARTESIAN_POINT ( 'NONE',  ( 1.240157480314961314, 0.07958543189024071263, -0.2665933059059888421 ) ) ;
#6511 = LINE ( 'NONE', #69667, #55911 ) ;
#6512 = CARTESIAN_POINT ( 'NONE',  ( -0.1049868766404193215, 0.2306618581243847221, -0.2411417322834647770 ) ) ;
#6513 = CARTESIAN_POINT ( 'NONE',  ( 0.2362204724409451007, -0.4091458600556402980, -1.194225721784776928 ) ) ;
#6514 = CARTESIAN_POINT ( 'NONE',  ( 0.1049643490035303689, 0.3917322834645670104, -1.022965879265091749 ) ) ;
#6515 = CARTESIAN_POINT ( 'NONE',  ( -0.8070866141732276899, 0.07958543189024071263, -0.2665933059059888421 ) ) ;
#6516 = CARTESIAN_POINT ( 'NONE',  ( -1.496062992125983815, -0.1870078740157480601, -0.3641732283464567677 ) ) ;
#6517 = CARTESIAN_POINT ( 'NONE',  ( -1.391076115485563314, -0.6046776061558809534, -0.2411417322834644161 ) ) ;
#6518 = CARTESIAN_POINT ( 'NONE',  ( -0.05249343832020938322, -0.6046776061558809534, -0.2411417322834644161 ) ) ;
#6519 = CARTESIAN_POINT ( 'NONE',  ( 1.469816272965879911, 0.2306618581243847221, -0.2411417322834647770 ) ) ;
#6520 = EDGE_LOOP ( 'NONE', ( #40258, #20988, #10021, #31875 ) ) ;
#6521 = CARTESIAN_POINT ( 'NONE',  ( -1.168329637866467818, 0.004960608223778821026, 0.3437734562760189072 ) ) ;
#6522 =( NAMED_UNIT ( * ) SI_UNIT ( $, .STERADIAN. ) SOLID_ANGLE_UNIT ( ) );
#6523 = CARTESIAN_POINT ( 'NONE',  ( -0.4091458600556405756, 0.2362204724409446288, -2.073490813648294129 ) ) ;
#6524 = CARTESIAN_POINT ( 'NONE',  ( -1.646051170424378096, 0.000000000000000000, 0.3464511005275205946 ) ) ;
#6525 = FACE_OUTER_BOUND ( 'NONE', #47789, .T. ) ;
#6526 = CARTESIAN_POINT ( 'NONE',  ( -0.8595800524934373854, -0.08942795157527998196, 0.3641732283464567121 ) ) ;
#6527 = CARTESIAN_POINT ( 'NONE',  ( -1.135170603674539924, 0.2952755905511810774, -0.1292274648535930714 ) ) ;
#6528 = CARTESIAN_POINT ( 'NONE',  ( 0.9120734908136490793, 0.2952755905511810774, -0.1292274648535930714 ) ) ;
#6529 = ORIENTED_EDGE ( 'NONE', *, *, #39869, .T. ) ;
#6531 = CARTESIAN_POINT ( 'NONE',  ( 0.4724409448818898682, 2.892866454678787531E-17, -2.714566929133858331 ) ) ;
#6530 = DIRECTION ( 'NONE',  ( 0.000000000000000000, 1.000000000000000000, 0.000000000000000000 ) ) ;
#6532 = CARTESIAN_POINT ( 'NONE',  ( 1.384514435695538559, 0.2952755905511810774, -0.1292274648535930714 ) ) ;
#6533 = CARTESIAN_POINT ( 'NONE',  ( -1.062992125984250968, 0.2952755905511811885, 0.000000000000000000 ) ) ;
#6534 = CARTESIAN_POINT ( 'NONE',  ( 0.2867679344610365999, -0.2867679344610365999, -0.6508993193887645523 ) ) ;
#6535 = CARTESIAN_POINT ( 'NONE',  ( -0.2690288713910754526, 0.1771653543307087075, -0.09757992244046823083 ) ) ;
#6536 = CARTESIAN_POINT ( 'NONE',  ( -0.3392501089628017219, -0.1958661417322836718, -0.9245406824146982228 ) ) ;
#6537 = CARTESIAN_POINT ( 'NONE',  ( -0.6364829396325453192, -0.08942795157528024563, -0.3641732283464568787 ) ) ;
#6538 = CARTESIAN_POINT ( 'NONE',  ( 0.1049868766404206816, -0.5023911411419708095, -0.1820866141732282451 ) ) ;
#6539 = CARTESIAN_POINT ( 'NONE',  ( 0.2755905511811031494, -0.6692913385826771977, 8.415575281601705876E-17 ) ) ;
#6540 = CARTESIAN_POINT ( 'NONE',  ( -0.9842519685039360366, 0.1771653543307087630, 0.000000000000000000 ) ) ;
#6541 = CARTESIAN_POINT ( 'NONE',  ( 0.1958661417322834775, 0.3392501089628018884, -2.813648293963254776 ) ) ;
#6542 = CARTESIAN_POINT ( 'NONE',  ( 1.312335958005249825, 0.2306618581243847221, -0.2411417322834647770 ) ) ;
#6543 = CARTESIAN_POINT ( 'NONE',  ( -1.259842519685038686, -0.1870078740157480879, -0.4822834645669291653 ) ) ;
#6544 = CARTESIAN_POINT ( 'NONE',  ( 0.3458507752293908943, 0.3458507752293908943, -1.159448818897637734 ) ) ;
#6545 = CARTESIAN_POINT ( 'NONE',  ( -0.1706036745406816491, -0.4281496062992124485, 0.4176697321401328655 ) ) ;
#6546 = CARTESIAN_POINT ( 'NONE',  ( -0.7480314960629914633, -0.6692913385826771977, 8.415575281601705876E-17 ) ) ;
#6547 = CARTESIAN_POINT ( 'NONE',  ( 0.6233595800524942554, -0.08942795157528024563, -0.3641732283464568787 ) ) ;
#6548 = CARTESIAN_POINT ( 'NONE',  ( -0.2690288713910754526, 0.1771653543307087075, -0.09757992244046823083 ) ) ;
#6549 = CARTESIAN_POINT ( 'NONE',  ( -0.5380577427821514602, -0.4281496062992127816, -0.4176697321401328100 ) ) ;
#6550 = CARTESIAN_POINT ( 'NONE',  ( -1.102362204724408601, -0.1870078740157480879, -0.4822834645669291653 ) ) ;
#6551 = CARTESIAN_POINT ( 'NONE',  ( -0.4051969335537399797, 5.961526036605507449E-15, -0.3791483426435156012 ) ) ;
#6552 = CARTESIAN_POINT ( 'NONE',  ( 1.102362204724410155, -0.1870078740157480601, -0.3641732283464567677 ) ) ;
#6553 = CARTESIAN_POINT ( 'NONE',  ( -0.4133858267716528645, -0.5400638737290844871, 0.3530559997133364547 ) ) ;
#6554 = CARTESIAN_POINT ( 'NONE',  ( -1.555118110236219930, 0.1660481256975885056, 0.3530559997133364547 ) ) ;
#6555 = ORIENTED_EDGE ( 'NONE', *, *, #31362, .F. ) ;
#6556 = CARTESIAN_POINT ( 'NONE',  ( 4.893765752498283308E-17, -0.3996062992125985480, -2.360236220472441193 ) ) ;
#6557 = CARTESIAN_POINT ( 'NONE',  ( -0.7217847769028863381, -0.3690944881889763329, 0.3153832671262228327 ) ) ;
#6558 = CARTESIAN_POINT ( 'NONE',  ( 0.9120734908136489683, -0.6692913385826771977, 0.1292274648535927661 ) ) ;
#6559 = CARTESIAN_POINT ( 'NONE',  ( -1.200787401574802349, 0.07958543189024071263, -0.2665933059059888421 ) ) ;
#6560 = CARTESIAN_POINT ( 'NONE',  ( 4.893765752498283308E-17, -0.3996062992125985480, -1.415354330708661568 ) ) ;
#6561 = CARTESIAN_POINT ( 'NONE',  ( -0.8595800524934373854, -0.3162353388693409650, -0.4822834645669289433 ) ) ;
#6562 = CARTESIAN_POINT ( 'NONE',  ( 0.9973753280839902091, -0.6046776061558807314, 0.2411417322834647770 ) ) ;
#6563 = CARTESIAN_POINT ( 'NONE',  ( 0.5380577427821529035, -0.4281496062992124485, 0.4176697321401328655 ) ) ;
#6564 = DIRECTION ( 'NONE',  ( -1.000000000000000000, -0.000000000000000000, -0.000000000000000000 ) ) ;
#6565 = CARTESIAN_POINT ( 'NONE',  ( -1.555118110236219930, 0.07958543189024085140, 0.2665933059059887866 ) ) ;
#6567 = ADVANCED_FACE ( 'NONE', ( #54813 ), #80515, .F. ) ;
#6566 = CARTESIAN_POINT ( 'NONE',  ( -0.3460692066303960313, 0.1998031496062989965, -0.5754593175853018883 ) ) ;
#6568 = CARTESIAN_POINT ( 'NONE',  ( -0.3460692066303960868, 0.1998031496062990242, -0.8136482939632546652 ) ) ;
#6569 = CARTESIAN_POINT ( 'NONE',  ( 4.837279021331060870E-17, -0.3949938075777409963, -0.2362204724409449619 ) ) ;
#6570 = LINE ( 'NONE', #32241, #39923 ) ;
#6571 = CARTESIAN_POINT ( 'NONE',  ( 1.115485564304462551, -0.3690944881889765550, -0.3153832671262227771 ) ) ;
#6572 = CARTESIAN_POINT ( 'NONE',  ( 0.4921259842519691285, 0.07958543189024085140, 0.2665933059059887866 ) ) ;
#6573 = CARTESIAN_POINT ( 'NONE',  ( 0.07874015748031558404, -0.1870078740157480879, -0.4822834645669291653 ) ) ;
#6574 = CARTESIAN_POINT ( 'NONE',  ( 1.502624671916010790, -0.3162353388693409650, -0.4822834645669289433 ) ) ;
#6575 = CARTESIAN_POINT ( 'NONE',  ( 0.3420746716998660508, 0.1974969037888705814, -1.152887139107611425 ) ) ;
#6576 = CARTESIAN_POINT ( 'NONE',  ( 0.5643044619422579178, -0.004921259842519576551, 0.3153832671262227771 ) ) ;
#6577 = CARTESIAN_POINT ( 'NONE',  ( -0.8464566929133852113, 0.1660481256975885056, 0.3530559997133364547 ) ) ;
#6578 = CARTESIAN_POINT ( 'NONE',  ( -1.148293963254592542, 0.2952755905511811885, 0.1292274648535926551 ) ) ;
#6579 = CARTESIAN_POINT ( 'NONE',  ( 0.8661417322834653598, -0.1870078740157479769, 0.4822834645669291653 ) ) ;
#6580 = CARTESIAN_POINT ( 'NONE',  ( -0.4724409448818895907, -0.1265901696524993070, -1.463254593175853158 ) ) ;
#6581 = CARTESIAN_POINT ( 'NONE',  ( -0.3996062992125985480, -0.1070741851644057135, -2.723097112860891844 ) ) ;
#6582 = VERTEX_POINT ( 'NONE', #42181 ) ;
#6583 = VERTEX_POINT ( 'NONE', #52 ) ;
#6584 = CARTESIAN_POINT ( 'NONE',  ( -1.220472440944881054, 0.2952755905511811885, 0.000000000000000000 ) ) ;
#6585 = CARTESIAN_POINT ( 'NONE',  ( -0.4068241469816264999, -0.4281496062992124485, 0.4176697321401328655 ) ) ;
#6587 = CARTESIAN_POINT ( 'NONE',  ( -0.6430446194225712953, 0.05413385826771626580, -0.4176697321401330321 ) ) ;
#6586 = CARTESIAN_POINT ( 'NONE',  ( -0.8333333333333323711, 0.1771653543307087630, 0.09757992244046791164 ) ) ;
#6588 = CARTESIAN_POINT ( 'NONE',  ( -0.2867679344610364334, -0.2867679344610368219, -2.186332390254906777 ) ) ;
#6589 = CARTESIAN_POINT ( 'NONE',  ( -0.2925321140481930149, -0.2925321140481933480, -2.812992125984251857 ) ) ;
#6590 = CARTESIAN_POINT ( 'NONE',  ( 1.640419947506562393, -0.4281496062992124485, 0.4176697321401328655 ) ) ;
#6591 = CARTESIAN_POINT ( 'NONE',  ( -1.397637795275589623, 0.1660481256975885056, 0.3530559997133364547 ) ) ;
#6592 = CARTESIAN_POINT ( 'NONE',  ( 0.5380577427821529035, 0.05413385826771626580, -0.4176697321401330321 ) ) ;
#6593 = CARTESIAN_POINT ( 'NONE',  ( -0.9973753280839886548, 0.2306618581243848609, 0.2411417322834645549 ) ) ;
#6594 = CARTESIAN_POINT ( 'NONE',  ( 4.797336870675656522E-17, -0.3917322834645670104, -1.645669291338582640 ) ) ;
#6595 = CARTESIAN_POINT ( 'NONE',  ( -0.6496062992125976043, 0.07958543189024071263, -0.2665933059059888421 ) ) ;
#6596 = ORIENTED_EDGE ( 'NONE', *, *, #26135, .F. ) ;
#6597 = CARTESIAN_POINT ( 'NONE',  ( -0.2891555358219911054, 0.2891555358219909388, -1.909448818897637956 ) ) ;
#6598 = ORIENTED_EDGE ( 'NONE', *, *, #78238, .T. ) ;
#6599 = CARTESIAN_POINT ( 'NONE',  ( -1.666666666666665853, -0.004921259842519870586, -0.3153832671262229437 ) ) ;
#6600 = CARTESIAN_POINT ( 'NONE',  ( -1.227034120734907141, -0.6692913385826773087, -0.1292274648535924053 ) ) ;
#6601 = CARTESIAN_POINT ( 'NONE',  ( -0.7611548556430438595, -0.6046776061558809534, -0.2411417322834644161 ) ) ;
#6602 = CARTESIAN_POINT ( 'NONE',  ( 0.1070741851644053527, 0.3996062992125986590, 0.006561679790026237087 ) ) ;
#6603 = CARTESIAN_POINT ( 'NONE',  ( -1.161417322834644716, -0.5400638737290845981, -0.3530559997133363437 ) ) ;
#6604 = CARTESIAN_POINT ( 'NONE',  ( -1.167979002624671470, -0.4281496062992127816, -0.4176697321401328100 ) ) ;
#6605 = CIRCLE ( 'NONE', #56351, 1.122047244094488194 ) ;
#6606 = FACE_OUTER_BOUND ( 'NONE', #58034, .T. ) ;
#6607 = CARTESIAN_POINT ( 'NONE',  ( 0.4265091863517067594, 0.1771653543307087630, 0.09757992244046791164 ) ) ;
#6608 = CARTESIAN_POINT ( 'NONE',  ( 1.586052503253845503, 0.4724409448818907564, 0.1653254495020587411 ) ) ;
#6609 = CARTESIAN_POINT ( 'NONE',  ( 0.3392501089628018884, -0.1958661417322834220, -0.3471128608923885195 ) ) ;
#6610 = CARTESIAN_POINT ( 'NONE',  ( -0.4527559055118102749, 0.07958543189024085140, 0.2665933059059887866 ) ) ;
#6611 = CARTESIAN_POINT ( 'NONE',  ( -0.7086614173228339419, -0.1870078740157479769, 0.4822834645669291653 ) ) ;
#6612 = CARTESIAN_POINT ( 'NONE',  ( 1.161417322834646271, 0.1660481256975883668, -0.3530559997133364547 ) ) ;
#6613 = CARTESIAN_POINT ( 'NONE',  ( -0.4330708661417315697, -0.6692913385826771977, 8.415575281601705876E-17 ) ) ;
#6614 = ORIENTED_EDGE ( 'NONE', *, *, #13640, .F. ) ;
#6615 = ORIENTED_EDGE ( 'NONE', *, *, #78384, .T. ) ;
#6616 = CARTESIAN_POINT ( 'NONE',  ( -0.1998031496062991630, -0.3460692066303959202, -1.874671916010498762 ) ) ;
#6617 = CARTESIAN_POINT ( 'NONE',  ( -0.9120734908136475250, -0.6692913385826773087, -0.1292274648535924053 ) ) ;
#6618 = CARTESIAN_POINT ( 'NONE',  ( 1.141732283464567566, 0.2952755905511811885, 0.000000000000000000 ) ) ;
#6619 = CARTESIAN_POINT ( 'NONE',  ( -1.122047244094487306, -0.4536011799217367080, 0.2665933059059888421 ) ) ;
#6620 = CARTESIAN_POINT ( 'NONE',  ( -1.220472440944881054, 0.2952755905511811885, 0.000000000000000000 ) ) ;
#6621 = CARTESIAN_POINT ( 'NONE',  ( -0.2362204724409451284, 0.4091458600556402425, -0.8005249343832020470 ) ) ;
#6622 = CARTESIAN_POINT ( 'NONE',  ( -0.4591639709769206878, 1.414133617986971458, 3.910145371492633970 ) ) ;
#6623 = CARTESIAN_POINT ( 'NONE',  ( -0.1049643490035302024, -0.3917322834645671215, -0.3792650918635169233 ) ) ;
#6624 = CARTESIAN_POINT ( 'NONE',  ( 0.08530183727034192087, -0.05778040916215522460, 0.4822834645669289988 ) ) ;
#6625 = CARTESIAN_POINT ( 'NONE',  ( -1.043307086614172041, -0.4536011799217367080, 0.2665933059059888421 ) ) ;
#6626 = CARTESIAN_POINT ( 'NONE',  ( -0.7874015748031489847, -0.1870078740157479769, 0.4822834645669291653 ) ) ;
#6627 = CARTESIAN_POINT ( 'NONE',  ( 0.4091458600556403535, 0.2362204724409449896, -2.727690288713910949 ) ) ;
#6628 = CARTESIAN_POINT ( 'NONE',  ( -1.364829396325458521, 0.2306618581243847221, -0.2411417322834647770 ) ) ;
#6629 = CARTESIAN_POINT ( 'NONE',  ( -0.9120734908136475250, 0.2952755905511811885, 0.1292274648535926551 ) ) ;
#6630 = CARTESIAN_POINT ( 'NONE',  ( 0.09186351706036799403, -0.4281496062992127816, -0.4176697321401328100 ) ) ;
#6631 = CARTESIAN_POINT ( 'NONE',  ( 0.2891555358219910499, 0.2891555358219910499, -2.576771653543307838 ) ) ;
#6632 = CARTESIAN_POINT ( 'NONE',  ( 0.7874015748031503170, -0.1870078740157479769, 0.3641732283464567677 ) ) ;
#6633 = CARTESIAN_POINT ( 'NONE',  ( -0.7020997375328076329, -0.2845877964562161244, -0.3641732283464567121 ) ) ;
#6634 = DIRECTION ( 'NONE',  ( -0.7071067811865462405, -0.000000000000000000, -0.7071067811865486830 ) ) ;
#6635 = CARTESIAN_POINT ( 'NONE',  ( 0.7742782152230979209, -0.004921259842519870586, -0.3153832671262229437 ) ) ;
#6636 = CARTESIAN_POINT ( 'NONE',  ( 1.299212598425197429, 0.1771653543307087630, 0.000000000000000000 ) ) ;
#6637 = CARTESIAN_POINT ( 'NONE',  ( 1.213910761154856299, -0.6692913385826773087, -0.1292274648535924053 ) ) ;
#6638 = CARTESIAN_POINT ( 'NONE',  ( -0.05249343832020911260, 0.1283753931104748280, 0.1820866141732283561 ) ) ;
#6639 = CARTESIAN_POINT ( 'NONE',  ( -0.3392501089628019995, 0.1958661417322832277, -1.435695538057742970 ) ) ;
#6640 = CARTESIAN_POINT ( 'NONE',  ( -0.7349081364829387342, -0.6046776061558807314, 0.2411417322834647770 ) ) ;
#6641 = CARTESIAN_POINT ( 'NONE',  ( 1.076115485564305141, -0.6046776061558807314, 0.2411417322834647770 ) ) ;
#6642 = CARTESIAN_POINT ( 'NONE',  ( 0.2362204724409449064, 0.4091458600556404646, 0.09383202099737532331 ) ) ;
#6643 = CARTESIAN_POINT ( 'NONE',  ( -0.3412073490813641308, 0.1283753931104746893, -0.1820866141732285504 ) ) ;
#6644 = CARTESIAN_POINT ( 'NONE',  ( 0.01312335958005323398, 0.05413385826771666132, 0.4176697321401328100 ) ) ;
#6645 = CARTESIAN_POINT ( 'NONE',  ( 0.1377952755905518800, 0.1660481256975883668, -0.3530559997133364547 ) ) ;
#6646 = CARTESIAN_POINT ( 'NONE',  ( -1.559171609364246924, 0.3937007874015747699, 0.6156134192599649335 ) ) ;
#6647 = CARTESIAN_POINT ( 'NONE',  ( 0.9383202099737536495, -0.2845877964562159024, 0.3641732283464567677 ) ) ;
#6648 = CARTESIAN_POINT ( 'NONE',  ( 0.1837270341207354329, 0.1283753931104748280, 0.1820866141732283561 ) ) ;
#6649 = CARTESIAN_POINT ( 'NONE',  ( -0.04593175853018302557, 0.2952755905511811885, 0.1292274648535926551 ) ) ;
#6650 = CARTESIAN_POINT ( 'NONE',  ( -1.312335958005248715, -0.6046776061558809534, -0.2411417322834644161 ) ) ;
#6651 = CARTESIAN_POINT ( 'NONE',  ( -0.7611548556430438595, -0.5023911411419708095, -0.1820866141732282451 ) ) ;
#6652 = DIRECTION ( 'NONE',  ( 0.000000000000000000, 0.000000000000000000, 1.000000000000000000 ) ) ;
#6653 = CARTESIAN_POINT ( 'NONE',  ( -0.6889763779527552368, 0.1660481256975885056, 0.3530559997133364547 ) ) ;
#6654 = CARTESIAN_POINT ( 'NONE',  ( 4.893765752498283308E-17, -0.3996062992125985480, -1.257874015748031260 ) ) ;
#6655 = EDGE_CURVE ( 'NONE', #66254, #65491, #69322, .T. ) ;
#6656 = CARTESIAN_POINT ( 'NONE',  ( 0.1958661417322836440, -0.3392501089628017219, -2.696194225721784576 ) ) ;
#6657 = B_SPLINE_CURVE_WITH_KNOTS ( 'NONE', 3,
 ( #23197, #48868, #16913, #37064 ),
 .UNSPECIFIED., .F., .F.,
 ( 4, 4 ),
 ( 1.999999999927407068E-07, 0.006970199999999936863 ),
 .UNSPECIFIED. ) ;
#6658 = CARTESIAN_POINT ( 'NONE',  ( 0.2559055118110243332, -0.4536011799217368745, -0.2665933059059886201 ) ) ;
#6659 = CARTESIAN_POINT ( 'NONE',  ( -0.9645669291338575535, 0.1660481256975883668, -0.3530559997133364547 ) ) ;
#6660 = CARTESIAN_POINT ( 'NONE',  ( -1.332020997375327642, -0.05778040916215522460, 0.4822834645669289988 ) ) ;
#6661 = CARTESIAN_POINT ( 'NONE',  ( -1.174540682414697335, -0.08942795157527998196, 0.3641732283464567121 ) ) ;
#6662 = CARTESIAN_POINT ( 'NONE',  ( 1.568241469816273659, -0.05778040916215560624, -0.4822834645669293319 ) ) ;
#6663 = CARTESIAN_POINT ( 'NONE',  ( -0.4855643044619415427, 0.05413385826771626580, -0.4176697321401330321 ) ) ;
#6664 = CARTESIAN_POINT ( 'NONE',  ( -0.8727034120734901146, -0.2845877964562159024, 0.3641732283464567677 ) ) ;
#6665 = CARTESIAN_POINT ( 'NONE',  ( -1.725721784776902190, -0.08942795157527998196, 0.3641732283464567121 ) ) ;
#6666 = CARTESIAN_POINT ( 'NONE',  ( 1.476377952755906220, 0.1660481256975883668, -0.3530559997133364547 ) ) ;
#6667 = CARTESIAN_POINT ( 'NONE',  ( -0.1070741851644056997, 0.3996062992125986035, 0.1509186351706036100 ) ) ;
#6668 = EDGE_CURVE ( 'NONE', #20489, #78980, #42000, .T. ) ;
#6669 = CARTESIAN_POINT ( 'NONE',  ( 0.2867679344610366554, -0.2867679344610365999, -2.142407767225408932 ) ) ;
#6670 = ORIENTED_EDGE ( 'NONE', *, *, #81439, .T. ) ;
#6671 = DIRECTION ( 'NONE',  ( -3.491481338843133355E-15, -0.000000000000000000, 1.000000000000000000 ) ) ;
#6672 = CARTESIAN_POINT ( 'NONE',  ( -1.299212598425196097, -0.6692913385826771977, 8.415575281601705876E-17 ) ) ;
#6673 = CARTESIAN_POINT ( 'NONE',  ( -0.9251968503937002541, 0.1660481256975885056, 0.3530559997133364547 ) ) ;
#6674 = CARTESIAN_POINT ( 'NONE',  ( -1.574803149606298192, -0.1870078740157480879, -0.4822834645669291653 ) ) ;
#6675 = CARTESIAN_POINT ( 'NONE',  ( 0.3917322834645669549, 0.1049643490035304660, -1.941601049868766582 ) ) ;
#6676 = CARTESIAN_POINT ( 'NONE',  ( 0.000000000000000000, 2.755905511811024056, 0.000000000000000000 ) ) ;
#6677 = CARTESIAN_POINT ( 'NONE',  ( 0.7152230971128616943, -0.05778040916215522460, 0.4822834645669289988 ) ) ;
#6678 = CARTESIAN_POINT ( 'NONE',  ( -0.1377952755905504645, -0.5400638737290845981, -0.3530559997133363437 ) ) ;
#6679 = CARTESIAN_POINT ( 'NONE',  ( -0.3499960723095489334, -0.3045081538226084295, -0.01928741089222641911 ) ) ;
#6680 = CARTESIAN_POINT ( 'NONE',  ( -0.6986524979670485358, -2.191421614605370878E-15, 0.4445507791589071167 ) ) ;
#6681 = CARTESIAN_POINT ( 'NONE',  ( 0.8661417322834652488, -0.1870078740157480601, -0.3641732283464567677 ) ) ;
#6682 = MANIFOLD_SOLID_BREP ( 'Fillet2', #39322 ) ;
#6683 = CARTESIAN_POINT ( 'NONE',  ( 0.3996062992125986035, 2.446882876249141962E-17, -1.377952755905511806 ) ) ;
#6684 = ORIENTED_EDGE ( 'NONE', *, *, #49555, .T. ) ;
#6685 = CARTESIAN_POINT ( 'NONE',  ( -0.3392501089628017219, -0.1958661417322836995, -0.04923191420703601495 ) ) ;
#6686 = ORIENTED_EDGE ( 'NONE', *, *, #14239, .T. ) ;
#6687 = CARTESIAN_POINT ( 'NONE',  ( -0.2165354330708654795, -0.5400638737290845981, -0.3530559997133363437 ) ) ;
#6688 = CARTESIAN_POINT ( 'NONE',  ( -0.8005249343832013809, -0.4281496062992124485, 0.4176697321401328655 ) ) ;
#6689 = CARTESIAN_POINT ( 'NONE',  ( -1.423884514435694859, -0.05778040916215560624, -0.4822834645669293319 ) ) ;
#6690 = CARTESIAN_POINT ( 'NONE',  ( 0.5511811023622055217, -0.1870078740157479769, 0.4822834645669291653 ) ) ;
#6691 = CARTESIAN_POINT ( 'NONE',  ( 1.574803149606299746, -0.1870078740157480879, -0.4822834645669291653 ) ) ;
#6692 = CARTESIAN_POINT ( 'NONE',  ( 1.456692913385827515, 0.2952755905511811885, 0.000000000000000000 ) ) ;
#6693 = CARTESIAN_POINT ( 'NONE',  ( -0.4790026246719152336, -0.05778040916215560624, -0.4822834645669293319 ) ) ;
#6694 = CARTESIAN_POINT ( 'NONE',  ( 0.4330708661417329575, -0.6692913385826771977, 8.415575281601705876E-17 ) ) ;
#6695 = CARTESIAN_POINT ( 'NONE',  ( -1.509186351706035767, -0.4281496062992124485, 0.4176697321401328655 ) ) ;
#6696 = CARTESIAN_POINT ( 'NONE',  ( 1.377952755905512472, -0.6692913385826771977, 8.415575281601705876E-17 ) ) ;
#6697 = CARTESIAN_POINT ( 'NONE',  ( 1.469816272965879911, -0.6046776061558807314, 0.2411417322834647770 ) ) ;
#6698 = CARTESIAN_POINT ( 'NONE',  ( -0.2624671916010490880, 0.2306618581243847221, -0.2411417322834647770 ) ) ;
#6699 = CARTESIAN_POINT ( 'NONE',  ( -0.3917322834645669549, -0.1049643490035306603, -0.03805774278215218187 ) ) ;
#6700 = CARTESIAN_POINT ( 'NONE',  ( 0.4133858267716541968, 0.07958543189024085140, 0.2665933059059887866 ) ) ;
#6701 = ORIENTED_EDGE ( 'NONE', *, *, #38498, .F. ) ;
#6702 = CARTESIAN_POINT ( 'NONE',  ( -0.3949938075777411628, 0.1058382717557497937, -0.5052493438320211361 ) ) ;
#6703 = ORIENTED_EDGE ( 'NONE', *, *, #63585, .F. ) ;
#6704 = CARTESIAN_POINT ( 'NONE',  ( -0.4790026246719154557, -0.2845877964562159024, 0.3641732283464567677 ) ) ;
#6705 = CARTESIAN_POINT ( 'NONE',  ( 2.554854094587847513, 1.520093187801265566, -0.4741711390158123707 ) ) ;
#6706 = CARTESIAN_POINT ( 'NONE',  ( 0.2624671916010504757, -0.6046776061558809534, -0.2411417322834644161 ) ) ;
#6707 = CARTESIAN_POINT ( 'NONE',  ( 0.01968503937007930540, 0.1660481256975885056, 0.3530559997133364547 ) ) ;
#6708 = CARTESIAN_POINT ( 'NONE',  ( -0.9908136482939626788, -0.6692913385826773087, -0.1292274648535924053 ) ) ;
#6709 = CARTESIAN_POINT ( 'NONE',  ( -9.594673741351313045E-17, 0.3917322834645670659, -1.571541625493125149 ) ) ;
#6710 = CARTESIAN_POINT ( 'NONE',  ( -1.292650918635170010, 0.2952755905511810774, -0.1292274648535930714 ) ) ;
#6711 = DIRECTION ( 'NONE',  ( 0.000000000000000000, 0.000000000000000000, -1.000000000000000000 ) ) ;
#6712 = CARTESIAN_POINT ( 'NONE',  ( 0.8267716535433077274, 0.1771653543307087630, 0.000000000000000000 ) ) ;
#6713 = CARTESIAN_POINT ( 'NONE',  ( 0.5971128608923891301, 0.2952755905511810774, -0.1292274648535930714 ) ) ;
#6714 = CARTESIAN_POINT ( 'NONE',  ( 0.6496062992125991586, -0.5400638737290845981, -0.3530559997133363437 ) ) ;
#6715 = CARTESIAN_POINT ( 'NONE',  ( -0.3460692066303958092, -0.1998031496062994683, -1.312335958005249381 ) ) ;
#6716 = CARTESIAN_POINT ( 'NONE',  ( -1.620734908136482577, -0.6692913385826773087, -0.1292274648535924053 ) ) ;
#6717 = CARTESIAN_POINT ( 'NONE',  ( -0.1070741851644051862, -0.3996062992125986590, -0.9363517060367454459 ) ) ;
#6718 = CARTESIAN_POINT ( 'NONE',  ( -0.1998031496062991630, -0.3460692066303959202, -0.1423884514435695692 ) ) ;
#6719 = CARTESIAN_POINT ( 'NONE',  ( -0.2427821522309703550, -0.05778040916215560624, -0.4822834645669293319 ) ) ;
#6720 = CARTESIAN_POINT ( 'NONE',  ( 0.1998031496062994405, -0.3460692066303958092, -2.769028871391076230 ) ) ;
#6721 = CARTESIAN_POINT ( 'NONE',  ( 0.3392501089628018329, 0.1958661417322835607, -1.633202099737532942 ) ) ;
#6722 = CARTESIAN_POINT ( 'NONE',  ( -1.089238845144356427, -0.3690944881889765550, -0.3153832671262227771 ) ) ;
#6723 = CARTESIAN_POINT ( 'NONE',  ( 1.371391076115485719, -0.6692913385826773087, -0.1292274648535924053 ) ) ;
#6724 = CARTESIAN_POINT ( 'NONE',  ( 1.345144356955381593, -0.05778040916215522460, 0.4822834645669289988 ) ) ;
#6725 = CARTESIAN_POINT ( 'NONE',  ( 0.1902887139107617975, -0.5511811023622048555, -0.09757992244046775898 ) ) ;
#6726 = CARTESIAN_POINT ( 'NONE',  ( 0.3412073490813655186, 0.2306618581243848609, 0.2411417322834645549 ) ) ;
#6727 = CARTESIAN_POINT ( 'NONE',  ( -0.3458507752293909498, 0.3458507752293907833, -1.356299212598425230 ) ) ;
#6728 = CARTESIAN_POINT ( 'NONE',  ( 0.2887139107611556010, 0.1283753931104746893, -0.1820866141732285504 ) ) ;
#6729 = CARTESIAN_POINT ( 'NONE',  ( 0.07217847769028949700, -0.05778040916215560624, -0.4822834645669293319 ) ) ;
#6730 = CARTESIAN_POINT ( 'NONE',  ( -0.1974969037888706924, 0.3420746716998658843, -1.349737532808398921 ) ) ;
#6731 = CARTESIAN_POINT ( 'NONE',  ( -1.076115485564303809, 0.2306618581243848609, 0.2411417322834645549 ) ) ;
#6732 = CARTESIAN_POINT ( 'NONE',  ( 0.7086614173228352742, -0.1870078740157480601, -0.3641732283464567677 ) ) ;
#6733 = CARTESIAN_POINT ( 'NONE',  ( -2.170146923806675510, 1.537401574803149984, 0.4744094488188970171 ) ) ;
#6734 = CARTESIAN_POINT ( 'NONE',  ( -0.5249343832020990641, -0.6046776061558809534, -0.2411417322834644161 ) ) ;
#6735 = CARTESIAN_POINT ( 'NONE',  ( -0.4068241469816264999, -0.3690944881889763329, 0.3153832671262228327 ) ) ;
#6736 = CARTESIAN_POINT ( 'NONE',  ( 1.348312163386739426, 0.2755905511811023723, 0.5221511799597032821 ) ) ;
#6737 = CARTESIAN_POINT ( 'NONE',  ( -0.4461942257217840213, 0.2306618581243848609, 0.2411417322834645549 ) ) ;
#6738 = CARTESIAN_POINT ( 'NONE',  ( -0.05249343832020911260, 0.2306618581243848609, 0.2411417322834645549 ) ) ;
#6739 = CARTESIAN_POINT ( 'NONE',  ( 0.3280839895013130669, -0.004921259842519576551, 0.3153832671262227771 ) ) ;
#6740 = CARTESIAN_POINT ( 'NONE',  ( -0.1070741851644051862, -0.3996062992125986590, -2.038713910761154491 ) ) ;
#6741 = CARTESIAN_POINT ( 'NONE',  ( 0.01312335958005323398, -0.4281496062992127816, -0.4176697321401328100 ) ) ;
#6742 = CARTESIAN_POINT ( 'NONE',  ( -0.3392501089628019439, 0.1958661417322832554, -1.681083046422885197 ) ) ;
#6743 = CARTESIAN_POINT ( 'NONE',  ( 0.7611548556430454138, 0.1283753931104746893, -0.1820866141732285504 ) ) ;
#6744 = CARTESIAN_POINT ( 'NONE',  ( 1.443569553805774897, 0.2306618581243848609, 0.2411417322834645549 ) ) ;
#6745 = CARTESIAN_POINT ( 'NONE',  ( -0.9186351706036736120, 0.1283753931104748280, 0.1820866141732283561 ) ) ;
#6746 = CARTESIAN_POINT ( 'NONE',  ( -0.7086614173228339419, -0.1870078740157480601, -0.3641732283464567677 ) ) ;
#6747 = CARTESIAN_POINT ( 'NONE',  ( -0.5446194225721777693, -0.05778040916215522460, 0.4822834645669289988 ) ) ;
#6748 = CARTESIAN_POINT ( 'NONE',  ( -0.09186351706036689768, 0.05413385826771626580, -0.4176697321401330321 ) ) ;
#6749 = CARTESIAN_POINT ( 'NONE',  ( 0.5249343832021005074, -0.5023911411419708095, 0.1820866141732285504 ) ) ;
#6750 = FACE_OUTER_BOUND ( 'NONE', #24618, .T. ) ;
#6751 = CARTESIAN_POINT ( 'NONE',  ( 1.200787401574803681, -0.4536011799217368745, -0.2665933059059886201 ) ) ;
#6752 = CARTESIAN_POINT ( 'NONE',  ( 0.8661417322834653598, -0.1870078740157479769, 0.4822834645669291653 ) ) ;
#6753 = CARTESIAN_POINT ( 'NONE',  ( 0.1070741851644054776, -0.3996062992125984925, 0.1528871391076115360 ) ) ;
#6754 = CARTESIAN_POINT ( 'NONE',  ( -0.1902887139107604098, -0.6692913385826771977, 0.1292274648535927661 ) ) ;
#6755 = CARTESIAN_POINT ( 'NONE',  ( -0.3392501089628019995, 0.1958661417322832277, -1.528215223097112885 ) ) ;
#6756 = CARTESIAN_POINT ( 'NONE',  ( 1.384514435695538337, -0.5511811023622046335, 0.09757992244046803654 ) ) ;
#6757 = CARTESIAN_POINT ( 'NONE',  ( 0.7217847769028878924, 0.05413385826771666132, 0.4176697321401328100 ) ) ;
#6758 = CARTESIAN_POINT ( 'NONE',  ( 0.2624671916010504757, 0.2306618581243848609, 0.2411417322834645549 ) ) ;
#6759 = CARTESIAN_POINT ( 'NONE',  ( -0.03443470937339728616, 0.2755905511811023723, -1.635441089090149402 ) ) ;
#6760 = CARTESIAN_POINT ( 'NONE',  ( 0.4265091863517067594, 0.1771653543307087630, 0.09757992244046791164 ) ) ;
#6761 = CARTESIAN_POINT ( 'NONE',  ( 0.9580052493438327987, -0.4281496062992127816, -0.4176697321401328100 ) ) ;
#6762 = CARTESIAN_POINT ( 'NONE',  ( -0.1640419947506555343, -0.2845877964562159024, 0.3641732283464567677 ) ) ;
#6763 = CARTESIAN_POINT ( 'NONE',  ( -0.5118110236220466680, 0.2952755905511811885, 0.000000000000000000 ) ) ;
#6764 = CARTESIAN_POINT ( 'NONE',  ( -0.3458507752293906723, -0.3458507752293910609, -2.578740157480315265 ) ) ;
#6765 = CARTESIAN_POINT ( 'NONE',  ( -0.03937007874015669567, -0.6692913385826771977, 8.415575281601705876E-17 ) ) ;
#6766 = APPLICATION_CONTEXT ( 'automotive_design' ) ;
#6767 = CARTESIAN_POINT ( 'NONE',  ( -1.108923884514435132, -0.05778040916215560624, -0.4822834645669293319 ) ) ;
#6768 = CARTESIAN_POINT ( 'NONE',  ( -0.6233595800524928121, -0.08942795157527998196, 0.3641732283464567121 ) ) ;
#6769 = CARTESIAN_POINT ( 'NONE',  ( 0.5380577427821529035, 0.05413385826771626580, -0.4176697321401330321 ) ) ;
#6770 = CARTESIAN_POINT ( 'NONE',  ( -1.266404199475064773, -0.3162353388693405765, 0.4822834645669290543 ) ) ;
#6771 = CARTESIAN_POINT ( 'NONE',  ( -0.2099737532808391705, 0.2306618581243848609, 0.2411417322834645549 ) ) ;
#6772 = CARTESIAN_POINT ( 'NONE',  ( 0.4697362858027160915, 1.605934398054998935, -2.158929595217815578 ) ) ;
#6774 = CARTESIAN_POINT ( 'NONE',  ( 1.259842519685040019, -0.1870078740157479769, 0.4822834645669291653 ) ) ;
#6773 = CARTESIAN_POINT ( 'NONE',  ( 1.090776338374008336, 0.02791078216816447743, -0.4328096321851892525 ) ) ;
#6775 = CARTESIAN_POINT ( 'NONE',  ( 1.299212598425197429, -0.6692913385826771977, 8.415575281601705876E-17 ) ) ;
#6776 = CARTESIAN_POINT ( 'NONE',  ( 0.3917322834645670104, 2.398668435337828261E-17, -2.314960629921259727 ) ) ;
#6777 = CARTESIAN_POINT ( 'NONE',  ( -1.627296587926508442, 0.2306618581243848609, 0.2411417322834645549 ) ) ;
#6778 = CARTESIAN_POINT ( 'NONE',  ( -0.8530183727034112984, -0.4281496062992127816, -0.4176697321401328100 ) ) ;
#6779 = CARTESIAN_POINT ( 'NONE',  ( -0.3458507752293909498, 0.3458507752293907833, -0.6496062992125984925 ) ) ;
#6780 = CARTESIAN_POINT ( 'NONE',  ( -0.1998031496062994683, 0.3460692066303958092, -0.1706036745406824540 ) ) ;
#6781 = EDGE_LOOP ( 'NONE', ( #54619, #28159, #27295, #66337 ) ) ;
#6782 = CARTESIAN_POINT ( 'NONE',  ( -0.2493438320209966919, -0.3690944881889763329, 0.3153832671262228327 ) ) ;
#6783 = CARTESIAN_POINT ( 'NONE',  ( 0.3917322834645669549, 0.1049643490035304660, -1.849081364829396223 ) ) ;
#6784 = ORIENTED_EDGE ( 'NONE', *, *, #83113, .F. ) ;
#6785 = CARTESIAN_POINT ( 'NONE',  ( 0.3740157480314966754, 0.1660481256975883668, -0.3530559997133364547 ) ) ;
#6786 = CARTESIAN_POINT ( 'NONE',  ( 0.5643044619422579178, -0.4281496062992127816, -0.4176697321401328100 ) ) ;
#6787 = CARTESIAN_POINT ( 'NONE',  ( 0.000000000000000000, 0.000000000000000000, 0.1574803149606299191 ) ) ;
#6788 = CARTESIAN_POINT ( 'NONE',  ( -0.4855643044619415427, -0.004921259842519870586, -0.3153832671262229437 ) ) ;
#6789 = CARTESIAN_POINT ( 'NONE',  ( -0.2229926280064457034, -0.1936066689571366572, 0.1399704324547693945 ) ) ;
#6790 = CARTESIAN_POINT ( 'NONE',  ( 0.9055118110236227702, 0.2952755905511811885, 0.000000000000000000 ) ) ;
#6791 = EDGE_CURVE ( 'NONE', #65941, #26273, #32031, .T. ) ;
#6792 = CARTESIAN_POINT ( 'NONE',  ( 1.069553805774278610, -0.5511811023622046335, 0.09757992244046803654 ) ) ;
#6793 = AXIS2_PLACEMENT_3D ( 'NONE', #76903, #75265, #18017 ) ;
#6794 = CARTESIAN_POINT ( 'NONE',  ( -0.6102362204724400829, -0.5400638737290845981, -0.3530559997133363437 ) ) ;
#6795 = CARTESIAN_POINT ( 'NONE',  ( -0.3917322834645670659, 0.1049643490035301607, -1.057723466370391829 ) ) ;
#6796 = CARTESIAN_POINT ( 'NONE',  ( -0.7545931758530176614, -0.6692913385826773087, -0.1292274648535924053 ) ) ;
#6797 = CARTESIAN_POINT ( 'NONE',  ( -1.358267716535432434, 0.07958543189024071263, -0.2665933059059888421 ) ) ;
#6798 = CARTESIAN_POINT ( 'NONE',  ( -0.8070866141732276899, -0.5400638737290844871, 0.3530559997133364547 ) ) ;
#6799 = CARTESIAN_POINT ( 'NONE',  ( 1.548556430446194954, 0.2306618581243847221, -0.2411417322834647770 ) ) ;
#6800 = CARTESIAN_POINT ( 'NONE',  ( -0.3635064842674102237, 1.231191414405744977, -2.000903845782021850 ) ) ;
#6801 = EDGE_LOOP ( 'NONE', ( #22046, #21938, #57621, #75683 ) ) ;
#6802 = CARTESIAN_POINT ( 'NONE',  ( 0.1958661417322836718, -0.3392501089628017219, -2.293326402396012487 ) ) ;
#6803 = CARTESIAN_POINT ( 'NONE',  ( 0.1312335958005257930, 0.2306618581243847221, -0.2411417322834647770 ) ) ;
#6804 = ORIENTED_EDGE ( 'NONE', *, *, #19351, .F. ) ;
#6805 = CARTESIAN_POINT ( 'NONE',  ( -0.8792650918635160906, 0.05413385826771626580, -0.4176697321401330321 ) ) ;
#6806 = CARTESIAN_POINT ( 'NONE',  ( 1.417322834645670104, -0.1870078740157479769, 0.4822834645669291653 ) ) ;
#6807 = CARTESIAN_POINT ( 'NONE',  ( 1.148293963254593653, 0.2952755905511810774, -0.1292274648535930714 ) ) ;
#6808 = CARTESIAN_POINT ( 'NONE',  ( 0.09186351706036799403, -0.4281496062992127816, -0.4176697321401328100 ) ) ;
#6809 = CARTESIAN_POINT ( 'NONE',  ( 0.09186351706036827158, 0.05413385826771666132, 0.4176697321401328100 ) ) ;
#6810 = CARTESIAN_POINT ( 'NONE',  ( 0.3917322834645669549, 0.1049643490035304660, -1.941601049868766582 ) ) ;
#6811 = CARTESIAN_POINT ( 'NONE',  ( -1.154855643044618851, -0.6046776061558809534, -0.2411417322834644161 ) ) ;
#6812 = CARTESIAN_POINT ( 'NONE',  ( -0.3018372703412066094, -0.4281496062992127816, -0.4176697321401328100 ) ) ;
#6813 = CARTESIAN_POINT ( 'NONE',  ( -0.2230971128608915943, -0.004921259842519576551, 0.3153832671262227771 ) ) ;
#6814 = CARTESIAN_POINT ( 'NONE',  ( 1.673228346456693494, 0.1660481256975885056, 0.3530559997133364547 ) ) ;
#6815 = VECTOR ( 'NONE', #51789, 39.37007874015748143 ) ;
#6816 = CARTESIAN_POINT ( 'NONE',  ( 1.377952755905512472, 0.2952755905511811885, 0.000000000000000000 ) ) ;
#6817 = CARTESIAN_POINT ( 'NONE',  ( -0.006561679790025524116, -0.3162353388693405765, 0.4822834645669290543 ) ) ;
#6818 = DIRECTION ( 'NONE',  ( -1.734723475976806848E-16, -1.000000000000000000, 0.000000000000000000 ) ) ;
#6819 = CARTESIAN_POINT ( 'NONE',  ( 1.017060367454068581, -0.05778040916215560624, -0.4822834645669293319 ) ) ;
#6820 = CARTESIAN_POINT ( 'NONE',  ( 0.5118110236220478892, 0.2066929133858268208, 0.000000000000000000 ) ) ;
#6821 = ORIENTED_EDGE ( 'NONE', *, *, #24369, .F. ) ;
#6822 = EDGE_CURVE ( 'NONE', #55042, #62471, #74745, .T. ) ;
#6823 = ORIENTED_EDGE ( 'NONE', *, *, #5521, .F. ) ;
#6824 = CARTESIAN_POINT ( 'NONE',  ( 0.4921259842519691285, -0.5400638737290845981, -0.3530559997133363437 ) ) ;
#6825 = CARTESIAN_POINT ( 'NONE',  ( -0.2362204724409442680, -0.1870078740157480601, -0.3641732283464567677 ) ) ;
#6827 = CARTESIAN_POINT ( 'NONE',  ( -0.2726377952755906220, -0.1133856558944467546, 0.1574803149606299191 ) ) ;
#6826 = CARTESIAN_POINT ( 'NONE',  ( 1.450131233595801428, -0.5511811023622048555, -0.09757992244046775898 ) ) ;
#6828 = CARTESIAN_POINT ( 'NONE',  ( -0.2362204724409451284, 0.4091458600556402425, -0.2473753280839895152 ) ) ;
#6829 = DIRECTION ( 'NONE',  ( 1.000000000000000000, -0.000000000000000000, -0.000000000000000000 ) ) ;
#6830 = CARTESIAN_POINT ( 'NONE',  ( -1.587926509186350810, 0.05413385826771626580, -0.4176697321401330321 ) ) ;
#6831 = CARTESIAN_POINT ( 'NONE',  ( -0.3460692066303957537, -0.1998031496062994405, -2.806430446194225770 ) ) ;
#6832 = CARTESIAN_POINT ( 'NONE',  ( 0.07217847769028949700, -0.05778040916215560624, -0.4822834645669293319 ) ) ;
#6833 = LINE ( 'NONE', #13167, #53920 ) ;
#6834 = CARTESIAN_POINT ( 'NONE',  ( -1.482939632545930975, -0.4281496062992127816, -0.4176697321401328100 ) ) ;
#6835 = CARTESIAN_POINT ( 'NONE',  ( 0.3740157480314966754, 0.1660481256975883668, -0.3530559997133364547 ) ) ;
#6836 = CARTESIAN_POINT ( 'NONE',  ( 0.3420746716998660508, -0.1974969037888704149, -0.02427821522309712640 ) ) ;
#6837 = CARTESIAN_POINT ( 'NONE',  ( -1.535433070866141225, -0.5511811023622047445, 6.969142054262312111E-17 ) ) ;
#6838 = CARTESIAN_POINT ( 'NONE',  ( 0.7545931758530188826, -0.6692913385826771977, 0.1292274648535927661 ) ) ;
#6839 = CARTESIAN_POINT ( 'NONE',  ( 1.095800524934383846, -0.08942795157528024563, -0.3641732283464568787 ) ) ;
#6840 = CARTESIAN_POINT ( 'NONE',  ( 0.8333333333333340365, 0.2066929133858267098, -0.1054918080437494132 ) ) ;
#6841 = CARTESIAN_POINT ( 'NONE',  ( 0.7545931758530189937, 0.1771653543307087075, -0.09757992244046823083 ) ) ;
#6842 = B_SPLINE_CURVE_WITH_KNOTS ( 'NONE', 3,
 ( #38385, #37148, #37971, #63646 ),
 .UNSPECIFIED., .F., .F.,
 ( 4, 4 ),
 ( 0.000000000000000000, 0.0007402370886711635454 ),
 .UNSPECIFIED. ) ;
#6843 = CARTESIAN_POINT ( 'NONE',  ( -1.450131233595799651, 0.2952755905511810774, -0.1292274648535930714 ) ) ;
#6844 = CARTESIAN_POINT ( 'NONE',  ( -0.1070741851644056997, 0.3996062992125984925, -1.028215223097112663 ) ) ;
#6845 = CARTESIAN_POINT ( 'NONE',  ( 1.246719160104987623, 0.05413385826771626580, -0.4176697321401330321 ) ) ;
#6846 = CARTESIAN_POINT ( 'NONE',  ( 0.1958661417322836440, -0.3392501089628017219, -0.5564304461942257696 ) ) ;
#6848 = CARTESIAN_POINT ( 'NONE',  ( -0.1656725442894096123, 1.091696002692741141, 1.876910173407116966 ) ) ;
#6847 = CARTESIAN_POINT ( 'NONE',  ( 0.9186351706036752773, 0.2306618581243847221, -0.2411417322834647770 ) ) ;
#6849 = CARTESIAN_POINT ( 'NONE',  ( -1.614173228346457378, 1.055049524192299693, 0.1372047244094476981 ) ) ;
#6850 = CARTESIAN_POINT ( 'NONE',  ( 0.4068241469816279987, -0.3690944881889765550, -0.3153832671262227771 ) ) ;
#6851 = CARTESIAN_POINT ( 'NONE',  ( 0.6758530183727039509, -0.6692913385826771977, 0.1292274648535927661 ) ) ;
#6852 = CARTESIAN_POINT ( 'NONE',  ( -0.4469586986359131431, 1.697151583350148263, 2.112655059233961907 ) ) ;
#6853 = CARTESIAN_POINT ( 'NONE',  ( -1.056430446194224881, 0.1771653543307087075, -0.09757992244046823083 ) ) ;
#6854 = CARTESIAN_POINT ( 'NONE',  ( -1.154855643044618851, -0.6046776061558809534, -0.2411417322834644161 ) ) ;
#6855 = CARTESIAN_POINT ( 'NONE',  ( 1.653543307086614789, -0.1870078740157479769, 0.4822834645669291653 ) ) ;
#6856 = CARTESIAN_POINT ( 'NONE',  ( -1.253280839895012377, -0.05778040916215522460, 0.4822834645669289988 ) ) ;
#6857 = VECTOR ( 'NONE', #7092, 39.37007874015748143 ) ;
#6858 = CARTESIAN_POINT ( 'NONE',  ( 1.122047244094488860, -0.5400638737290845981, -0.3530559997133363437 ) ) ;
#6859 = CARTESIAN_POINT ( 'NONE',  ( -1.220472440944881054, -0.5511811023622047445, 6.969142054262312111E-17 ) ) ;
#6860 = CARTESIAN_POINT ( 'NONE',  ( 1.096606552046649030, 1.126456178498281613, -0.2390280536361044927 ) ) ;
#6861 = CARTESIAN_POINT ( 'NONE',  ( 0.9383202099737536495, -0.3162353388693405765, 0.4822834645669290543 ) ) ;
#6862 = CARTESIAN_POINT ( 'NONE',  ( 0.4091458600556403535, 0.2362204724409449896, -2.570209973753280863 ) ) ;
#6863 = DIRECTION ( 'NONE',  ( 0.000000000000000000, 1.000000000000000000, 0.000000000000000000 ) ) ;
#6864 = CARTESIAN_POINT ( 'NONE',  ( 1.227034120734908917, 0.2952755905511810774, -0.1292274648535930714 ) ) ;
#6865 = CARTESIAN_POINT ( 'NONE',  ( -1.135170603674539924, -0.5511811023622046335, 0.09757992244046803654 ) ) ;
#6866 = CARTESIAN_POINT ( 'NONE',  ( 1.633858267716535639, -0.4536011799217367080, 0.2665933059059888421 ) ) ;
#6867 = CARTESIAN_POINT ( 'NONE',  ( -1.181102362204723644, -0.1870078740157479769, 0.3641732283464567677 ) ) ;
#6868 = CARTESIAN_POINT ( 'NONE',  ( -0.4921259842519677963, 0.07958543189024071263, -0.2665933059059888421 ) ) ;
#6869 = CARTESIAN_POINT ( 'NONE',  ( -1.410761154855642463, -0.08942795157527998196, 0.3641732283464567121 ) ) ;
#6870 = CARTESIAN_POINT ( 'NONE',  ( 0.8792650918635177559, -0.3690944881889765550, -0.3153832671262227771 ) ) ;
#6871 = CARTESIAN_POINT ( 'NONE',  ( 0.3477690288713918276, -0.6692913385826773087, -0.1292274648535924053 ) ) ;
#6872 = CARTESIAN_POINT ( 'NONE',  ( -1.646051170424378096, -0.1870078740157480046, 1.254653134982923898E-17 ) ) ;
#6873 = CARTESIAN_POINT ( 'NONE',  ( 0.2165354330708668673, -0.5400638737290844871, 0.3530559997133364547 ) ) ;
#6874 = AXIS2_PLACEMENT_3D ( 'NONE', #1627, #39077, #32767 ) ;
#6875 = CARTESIAN_POINT ( 'NONE',  ( 0.6102362204724416372, -0.4536011799217367080, 0.2665933059059888421 ) ) ;
#6876 = CARTESIAN_POINT ( 'NONE',  ( -1.614173228346455824, 0.2952755905511811885, 0.000000000000000000 ) ) ;
#6877 = CARTESIAN_POINT ( 'NONE',  ( -1.397637795275589623, -0.5400638737290845981, -0.3530559997133363437 ) ) ;
#6878 = CARTESIAN_POINT ( 'NONE',  ( -0.6627296587926503335, -0.6692913385826771977, 0.1292274648535927661 ) ) ;
#6879 = CARTESIAN_POINT ( 'NONE',  ( 0.3460692066303959757, -0.1998031496062991907, -0.4199475065616797842 ) ) ;
#6880 = DIRECTION ( 'NONE',  ( -0.000000000000000000, 1.000000000000000000, -0.000000000000000000 ) ) ;
#6881 = CARTESIAN_POINT ( 'NONE',  ( 0.04593175853018440641, 0.2952755905511810774, -0.1292274648535930714 ) ) ;
#6882 = CARTESIAN_POINT ( 'NONE',  ( 1.272965879265092637, -0.004921259842519576551, 0.3153832671262227771 ) ) ;
#6883 = CARTESIAN_POINT ( 'NONE',  ( -0.3674540682414689785, 0.2306618581243848609, 0.2411417322834645549 ) ) ;
#6884 = CARTESIAN_POINT ( 'NONE',  ( 0.4986876640419954376, 0.2306618581243848609, 0.2411417322834645549 ) ) ;
#6885 = CARTESIAN_POINT ( 'NONE',  ( 0.2925321140481932369, -0.2925321140481932369, -2.775590551181101429 ) ) ;
#6886 = CARTESIAN_POINT ( 'NONE',  ( -0.3949938075777409963, -7.255918531996591613E-17, -1.929133858267716439 ) ) ;
#6887 = CARTESIAN_POINT ( 'NONE',  ( -0.3392501089628017219, -0.1958661417322836718, -0.5170603674540682482 ) ) ;
#6888 = CARTESIAN_POINT ( 'NONE',  ( 0.2635551335312363852, -0.1334335510540912706, 5.584872361112684480 ) ) ;
#6889 = CARTESIAN_POINT ( 'NONE',  ( 0.3917322834645669549, 0.1049643490035304660, -0.9041994750656167090 ) ) ;
#6890 = EDGE_CURVE ( 'NONE', #49627, #80266, #43488, .T. ) ;
#6891 = CARTESIAN_POINT ( 'NONE',  ( -1.115485564304461219, -0.3690944881889763329, 0.3153832671262228327 ) ) ;
#6892 = CARTESIAN_POINT ( 'NONE',  ( -9.594673741351313045E-17, 0.3917322834645670104, -1.251968503937008093 ) ) ;
#6893 = CARTESIAN_POINT ( 'NONE',  ( -1.312335958005248715, -0.6046776061558809534, -0.2411417322834644161 ) ) ;
#6894 = CARTESIAN_POINT ( 'NONE',  ( 0.3392501089628018329, 0.1958661417322835052, 0.1036938564642537891 ) ) ;
#6895 = CARTESIAN_POINT ( 'NONE',  ( 0.2690288713910767848, 0.2952755905511811885, 0.1292274648535926551 ) ) ;
#6896 = CARTESIAN_POINT ( 'NONE',  ( 1.141732283464567566, 0.2952755905511811885, 0.000000000000000000 ) ) ;
#6897 = CARTESIAN_POINT ( 'NONE',  ( 0.6955380577427828781, 0.05413385826771626580, -0.4176697321401330321 ) ) ;
#6898 = CARTESIAN_POINT ( 'NONE',  ( -0.3458507752293909498, 0.3458507752293907833, -2.854330708661417138 ) ) ;
#6899 = CARTESIAN_POINT ( 'NONE',  ( 0.3996062992125986035, 2.446882876249141962E-17, -2.480314960629921295 ) ) ;
#6900 = CARTESIAN_POINT ( 'NONE',  ( -0.3917322834645671770, 0.1049643490035302024, -1.131909079561366882 ) ) ;
#6901 = CARTESIAN_POINT ( 'NONE',  ( 1.312335958005250269, -0.6046776061558807314, 0.2411417322834647770 ) ) ;
#6902 = CARTESIAN_POINT ( 'NONE',  ( 0.3805774278215230400, 0.05413385826771626580, -0.4176697321401330321 ) ) ;
#6903 = CARTESIAN_POINT ( 'NONE',  ( 0.1837270341207354329, 0.2306618581243848609, 0.2411417322834645549 ) ) ;
#6904 = CARTESIAN_POINT ( 'NONE',  ( 0.6167979002624678353, -0.3690944881889763329, 0.3153832671262228327 ) ) ;
#6905 = CARTESIAN_POINT ( 'NONE',  ( 1.102362204724410155, -0.1870078740157480879, -0.4822834645669291653 ) ) ;
#6906 = CARTESIAN_POINT ( 'NONE',  ( -0.1049643490035302024, -0.3917322834645671215, 0.0006561679790025351077 ) ) ;
#6907 = CARTESIAN_POINT ( 'NONE',  ( 0.1771653543307093182, 0.1660481256975885056, 0.3530559997133364547 ) ) ;
#6908 = CARTESIAN_POINT ( 'NONE',  ( 0.8858267716535438430, 0.1660481256975885056, 0.3530559997133364547 ) ) ;
#6909 = CARTESIAN_POINT ( 'NONE',  ( 0.5052493438320218022, -0.6692913385826773087, -0.1292274648535924053 ) ) ;
#6910 = CARTESIAN_POINT ( 'NONE',  ( 1.292650918635171564, -0.5511811023622048555, -0.09757992244046775898 ) ) ;
#6911 = CARTESIAN_POINT ( 'NONE',  ( -0.9251968503937002541, 0.1660481256975885056, 0.3530559997133364547 ) ) ;
#6912 = CARTESIAN_POINT ( 'NONE',  ( -1.148293963254592542, -0.6692913385826773087, -0.1292274648535924053 ) ) ;
#6913 = AXIS2_PLACEMENT_3D ( 'NONE', #43870, #69569, #31251 ) ;
#6914 = CARTESIAN_POINT ( 'NONE',  ( 1.312335958005249825, 0.2306618581243847221, -0.2411417322834647770 ) ) ;
#6915 = CARTESIAN_POINT ( 'NONE',  ( -0.1049643490035302024, -0.3917322834645671215, -0.4717847769028871152 ) ) ;
#6916 = CARTESIAN_POINT ( 'NONE',  ( 0.2867679344610365999, 0.2867679344610365999, -1.862204724409449064 ) ) ;
#6917 = CARTESIAN_POINT ( 'NONE',  ( -0.3917322834645670104, -7.196005306013484475E-17, -2.708661417322834275 ) ) ;
#6918 = ORIENTED_EDGE ( 'NONE', *, *, #26633, .F. ) ;
#6919 = CARTESIAN_POINT ( 'NONE',  ( 0.1070741851644054915, -0.3996062992125986035, -0.08530183727034119923 ) ) ;
#6920 = VERTEX_POINT ( 'NONE', #69916 ) ;
#6921 = CARTESIAN_POINT ( 'NONE',  ( 1.528871391076116026, 0.2952755905511811885, 0.1292274648535926551 ) ) ;
#6922 = CARTESIAN_POINT ( 'NONE',  ( 1.161417322834646271, 0.07958543189024071263, -0.2665933059059888421 ) ) ;
#6923 = CARTESIAN_POINT ( 'NONE',  ( 0.1070741851644054915, -0.3996062992125986035, -1.975065616797900381 ) ) ;
#6924 = CARTESIAN_POINT ( 'NONE',  ( 0.6199123404867349363, 8.471767977567108961E-16, -0.4445507791589058955 ) ) ;
#6925 = LINE ( 'NONE', #78486, #3373 ) ;
#6926 = CARTESIAN_POINT ( 'NONE',  ( 0.3957358693849762354, 0.01930322177395801808, -1.929133858268277546 ) ) ;
#6927 = CARTESIAN_POINT ( 'NONE',  ( 0.1049643490035303689, 0.3917322834645670104, -0.8654855643044619962 ) ) ;
#6928 = CARTESIAN_POINT ( 'NONE',  ( -1.128608923884513837, 0.1283753931104746893, -0.1820866141732285504 ) ) ;
#6929 = CARTESIAN_POINT ( 'NONE',  ( -1.437007874015747477, -0.4536011799217367080, 0.2665933059059888421 ) ) ;
#6930 = CARTESIAN_POINT ( 'NONE',  ( -1.102362204724408601, -0.1870078740157480879, -0.4822834645669291653 ) ) ;
#6931 = CARTESIAN_POINT ( 'NONE',  ( 0.2821522309711292364, -0.6692913385826771977, 0.1292274648535927661 ) ) ;
#6932 = CARTESIAN_POINT ( 'NONE',  ( 1.410761154855643795, -0.3162353388693405765, 0.4822834645669290543 ) ) ;
#6933 = VERTEX_POINT ( 'NONE', #57272 ) ;
#6934 = CARTESIAN_POINT ( 'NONE',  ( -1.121710378714982248, 1.063787285278161798, -0.03163150153590546521 ) ) ;
#6935 = DIRECTION ( 'NONE',  ( -0.8405202471921882079, 0.000000000000000000, 0.5417801344272261677 ) ) ;
#6936 = DIRECTION ( 'NONE',  ( 0.000000000000000000, 1.000000000000000000, -0.000000000000000000 ) ) ;
#6937 = DIRECTION ( 'NONE',  ( 0.000000000000000000, -1.000000000000000000, -0.000000000000000000 ) ) ;
#6938 = CARTESIAN_POINT ( 'NONE',  ( -0.8858267716535425107, -0.4536011799217367080, 0.2665933059059888421 ) ) ;
#6939 = CARTESIAN_POINT ( 'NONE',  ( 0.9317585301837276734, 0.009842519685039147898, -0.3409548833797004797 ) ) ;
#6940 = CARTESIAN_POINT ( 'NONE',  ( 0.5643044619422579178, 0.05413385826771666132, 0.4176697321401328100 ) ) ;
#6941 = EDGE_LOOP ( 'NONE', ( #43411, #49100, #7440, #82792 ) ) ;
#6943 = DIRECTION ( 'NONE',  ( 1.000000000000000000, -0.000000000000000000, -0.000000000000000000 ) ) ;
#6942 = DIRECTION ( 'NONE',  ( 0.000000000000000000, 0.000000000000000000, 1.000000000000000000 ) ) ;
#6944 = EDGE_CURVE ( 'NONE', #44534, #71433, #82970, .T. ) ;
#6945 = CARTESIAN_POINT ( 'NONE',  ( 1.194225721784777594, 0.05413385826771666132, 0.4176697321401328100 ) ) ;
#6946 = CARTESIAN_POINT ( 'NONE',  ( -1.450131233595799651, -0.6692913385826771977, 0.1292274648535927661 ) ) ;
#6947 = CARTESIAN_POINT ( 'NONE',  ( -0.1049643490035306742, 0.3917322834645668994, -0.8739964322496570626 ) ) ;
#6948 = CARTESIAN_POINT ( 'NONE',  ( -0.4133858267716528645, 0.07958543189024071263, -0.2665933059059888421 ) ) ;
#6949 = CARTESIAN_POINT ( 'NONE',  ( -1.594488188976377119, 0.07958543189024071263, -0.2665933059059888421 ) ) ;
#6950 = CARTESIAN_POINT ( 'NONE',  ( 0.1958661417322834775, 0.3392501089628018884, -1.173884514435695525 ) ) ;
#6951 = EDGE_CURVE ( 'NONE', #30815, #19015, #26558, .T. ) ;
#6952 = CARTESIAN_POINT ( 'NONE',  ( -0.5643044619422565855, -0.3690944881889763329, 0.3153832671262228327 ) ) ;
#6953 = CARTESIAN_POINT ( 'NONE',  ( 0.2755905511811031494, -0.5511811023622047445, 6.969142054262312111E-17 ) ) ;
#6954 = CARTESIAN_POINT ( 'NONE',  ( -0.05905511811023545637, -0.5400638737290845981, -0.3530559997133363437 ) ) ;
#6955 = CARTESIAN_POINT ( 'NONE',  ( -1.141732283464566011, 0.1771653543307087630, 0.000000000000000000 ) ) ;
#6956 = CARTESIAN_POINT ( 'NONE',  ( -0.3917322834645671215, 0.1049643490035301469, -2.859580052493438274 ) ) ;
#6957 = CARTESIAN_POINT ( 'NONE',  ( 1.227034120734908917, -0.6692913385826771977, 0.1292274648535927661 ) ) ;
#6958 = CARTESIAN_POINT ( 'NONE',  ( -1.417322834645668772, -0.1870078740157480879, -0.4822834645669291653 ) ) ;
#6959 = CARTESIAN_POINT ( 'NONE',  ( 0.1265901696524989462, 0.4724409448818897572, -1.172572178477690352 ) ) ;
#6960 = CARTESIAN_POINT ( 'NONE',  ( -0.2690288713910754526, 0.2952755905511810774, -0.1292274648535930714 ) ) ;
#6961 = CARTESIAN_POINT ( 'NONE',  ( 0.3608923884514443348, 0.1771653543307087075, -0.09757992244046823083 ) ) ;
#6962 = CARTESIAN_POINT ( 'NONE',  ( -1.115485564304461219, 0.05413385826771626580, -0.4176697321401330321 ) ) ;
#6963 = CARTESIAN_POINT ( 'NONE',  ( 0.9908136482939640111, -0.5511811023622046335, 0.09757992244046803654 ) ) ;
#6964 = CARTESIAN_POINT ( 'NONE',  ( -0.4002624671916004129, -0.08942795157528024563, -0.3641732283464568787 ) ) ;
#6965 = CARTESIAN_POINT ( 'NONE',  ( -0.8267716535433065062, -0.6692913385826771977, 8.415575281601705876E-17 ) ) ;
#6966 = CARTESIAN_POINT ( 'NONE',  ( -1.646981627296586703, -0.05778040916215522460, 0.4822834645669289988 ) ) ;
#6967 = CARTESIAN_POINT ( 'NONE',  ( -0.4040399068613288458, -1.283732188437465593E-15, -0.4281993546915532911 ) ) ;
#6968 = CARTESIAN_POINT ( 'NONE',  ( 1.450131233595801428, -0.5511811023622048555, -0.09757992244046775898 ) ) ;
#6969 = CARTESIAN_POINT ( 'NONE',  ( -1.515748031496062076, -0.5400638737290844871, 0.3530559997133364547 ) ) ;
#6970 = CARTESIAN_POINT ( 'NONE',  ( -1.607611548556429737, -0.6692913385826771977, 0.1292274648535927661 ) ) ;
#6971 = AXIS2_PLACEMENT_3D ( 'NONE', #37107, #43811, #24474 ) ;
#6972 = VERTEX_POINT ( 'NONE', #53467 ) ;
#6973 = EDGE_CURVE ( 'NONE', #11714, #13837, #49389, .T. ) ;
#6974 = CARTESIAN_POINT ( 'NONE',  ( -0.2925321140481932369, 0.2925321140481931259, -2.301181102362204633 ) ) ;
#6975 = CARTESIAN_POINT ( 'NONE',  ( -0.8792650918635160906, -0.3690944881889763329, 0.3153832671262228327 ) ) ;
#6976 = CARTESIAN_POINT ( 'NONE',  ( 0.8136482939632553313, 0.2306618581243848609, 0.2411417322834645549 ) ) ;
#6977 = CARTESIAN_POINT ( 'NONE',  ( -0.9973753280839886548, -0.5023911411419708095, -0.1820866141732282451 ) ) ;
#6978 = CARTESIAN_POINT ( 'NONE',  ( 0.1998031496062994128, -0.3460692066303957537, -1.900918635170603999 ) ) ;
#6979 = CARTESIAN_POINT ( 'NONE',  ( -0.9251968503937002541, 0.1660481256975885056, 0.3530559997133364547 ) ) ;
#6980 = CARTESIAN_POINT ( 'NONE',  ( 0.6627296587926517768, -0.6692913385826773087, -0.1292274648535924053 ) ) ;
#6981 = CARTESIAN_POINT ( 'NONE',  ( 0.4068241469816281097, 0.05413385826771666132, 0.4176697321401328100 ) ) ;
#6982 = FACE_OUTER_BOUND ( 'NONE', #33928, .T. ) ;
#6983 = CARTESIAN_POINT ( 'NONE',  ( -1.653543307086613234, -0.1870078740157480601, -0.3641732283464567677 ) ) ;
#6984 = CARTESIAN_POINT ( 'NONE',  ( -0.3996062992125984925, -0.1070741851644056719, -1.067585301837270517 ) ) ;
#6986 = EDGE_CURVE ( 'NONE', #30609, #61385, #59369, .T. ) ;
#6985 = CARTESIAN_POINT ( 'NONE',  ( -0.3460692066303960868, 0.1998031496062990242, -0.9711286089238845287 ) ) ;
#6987 = CARTESIAN_POINT ( 'NONE',  ( -0.1058382717557503211, 0.3949938075777409408, -0.4790026246719162328 ) ) ;
#6988 = CARTESIAN_POINT ( 'NONE',  ( 0.4359958488159444423, 1.724409448818900570, 2.630268417803970138 ) ) ;
#6989 = CARTESIAN_POINT ( 'NONE',  ( 0.8989501312335964611, 0.1771653543307087630, 0.09757992244046791164 ) ) ;
#6990 = CARTESIAN_POINT ( 'NONE',  ( 0.3346456692913390985, 0.07958543189024085140, 0.2665933059059887866 ) ) ;
#6991 = CARTESIAN_POINT ( 'NONE',  ( -0.02624671916010428221, -0.6046776061558807314, 0.2411417322834647770 ) ) ;
#6992 = CARTESIAN_POINT ( 'NONE',  ( 1.253280839895013710, -0.3162353388693405765, 0.4822834645669290543 ) ) ;
#6993 = CARTESIAN_POINT ( 'NONE',  ( -0.3420746716998660508, -0.1974969037888706924, -1.389107611548556553 ) ) ;
#6994 = CARTESIAN_POINT ( 'NONE',  ( 0.4461942257217856311, 0.1283753931104746893, -0.1820866141732285504 ) ) ;
#6995 = EDGE_CURVE ( 'NONE', #68098, #24318, #52632, .T. ) ;
#6996 = CARTESIAN_POINT ( 'NONE',  ( -0.5643044619422565855, -0.4281496062992124485, 0.4176697321401328655 ) ) ;
#6997 = CARTESIAN_POINT ( 'NONE',  ( -1.404199475065615932, -0.4281496062992127816, -0.4176697321401328100 ) ) ;
#6998 = CARTESIAN_POINT ( 'NONE',  ( 0.8464566929133866546, -0.5400638737290844871, 0.3530559997133364547 ) ) ;
#6999 = CARTESIAN_POINT ( 'NONE',  ( 0.2362204724409449064, 0.4091458600556404646, -1.719160104986876769 ) ) ;
#7000 = CARTESIAN_POINT ( 'NONE',  ( -0.7677165354330700575, 0.1660481256975885056, 0.3530559997133364547 ) ) ;
#7001 = ORIENTED_EDGE ( 'NONE', *, *, #4428, .F. ) ;
#7002 = VERTEX_POINT ( 'NONE', #472 ) ;
#7003 = CARTESIAN_POINT ( 'NONE',  ( -1.305774278215222184, -0.6692913385826773087, -0.1292274648535924053 ) ) ;
#7004 = CARTESIAN_POINT ( 'NONE',  ( -0.8202099737532799750, 0.2952755905511810774, -0.1292274648535930714 ) ) ;
#7006 = CARTESIAN_POINT ( 'NONE',  ( -0.9383202099737524282, -0.3162353388693409650, -0.4822834645669289433 ) ) ;
#7005 = CARTESIAN_POINT ( 'NONE',  ( -0.6889763779527552368, 0.07958543189024085140, 0.2665933059059887866 ) ) ;
#7007 = CARTESIAN_POINT ( 'NONE',  ( -0.1958661417322836440, 0.3392501089628016664, -1.825440001803462886 ) ) ;
#7008 = CARTESIAN_POINT ( 'NONE',  ( -0.3996062992125986590, 0.1070741851644051723, -2.786745406824146620 ) ) ;
#7009 = CARTESIAN_POINT ( 'NONE',  ( 1.535433070866142558, 0.2952755905511811885, 0.000000000000000000 ) ) ;
#7010 = CARTESIAN_POINT ( 'NONE',  ( -1.266404199475064773, -0.3162353388693405765, 0.4822834645669290543 ) ) ;
#7011 = CARTESIAN_POINT ( 'NONE',  ( 0.2034120734908142214, 0.2952755905511810774, -0.1292274648535930714 ) ) ;
#7012 = CARTESIAN_POINT ( 'NONE',  ( -0.7152230971128602510, -0.3162353388693405765, 0.4822834645669290543 ) ) ;
#7013 = CARTESIAN_POINT ( 'NONE',  ( 0.6692913385826777528, 0.2952755905511811885, 0.000000000000000000 ) ) ;
#7014 = CARTESIAN_POINT ( 'NONE',  ( 0.1049643490035303689, 0.3917322834645670104, -1.402887139107611647 ) ) ;
#7015 = CARTESIAN_POINT ( 'NONE',  ( -0.8070866141732276899, 0.07958543189024071263, -0.2665933059059888421 ) ) ;
#7016 = ORIENTED_EDGE ( 'NONE', *, *, #48672, .F. ) ;
#7017 = CARTESIAN_POINT ( 'NONE',  ( -0.2891555358219908833, -0.2891555358219912164, -1.948818897637795144 ) ) ;
#7018 = ORIENTED_EDGE ( 'NONE', *, *, #79927, .T. ) ;
#7019 = DIRECTION ( 'NONE',  ( -0.7071067811865472397, 0.000000000000000000, -0.7071067811865476838 ) ) ;
#7020 = CARTESIAN_POINT ( 'NONE',  ( -0.9580052493438311334, -0.4281496062992124485, 0.4176697321401328655 ) ) ;
#7021 = CARTESIAN_POINT ( 'NONE',  ( -1.148293963254592542, 0.2952755905511811885, 0.1292274648535926551 ) ) ;
#7022 = CARTESIAN_POINT ( 'NONE',  ( 4.893765752498283924E-17, -0.3996062992125986035, -0.07874015748031498729 ) ) ;
#7023 = CARTESIAN_POINT ( 'NONE',  ( -1.135170603674539924, -0.6692913385826771977, 0.1292274648535927661 ) ) ;
#7024 = CARTESIAN_POINT ( 'NONE',  ( -1.108923884514435132, -0.3162353388693405765, 0.4822834645669290543 ) ) ;
#7025 = CARTESIAN_POINT ( 'NONE',  ( -1.587926509186350810, 0.05413385826771626580, -0.4176697321401330321 ) ) ;
#7026 = CARTESIAN_POINT ( 'NONE',  ( 0.9324623468618423727, 2.784432375088962958E-17, -0.3464511005275205946 ) ) ;
#7027 = CARTESIAN_POINT ( 'NONE',  ( -0.2867679344610365999, 0.2867679344610364889, 0.2106299212598424508 ) ) ;
#7028 = CARTESIAN_POINT ( 'NONE',  ( -0.1049868766404193215, -0.5023911411419708095, 0.1820866141732285504 ) ) ;
#7029 = DIRECTION ( 'NONE',  ( -0.000000000000000000, -1.000000000000000000, -0.000000000000000000 ) ) ;
#7030 = CARTESIAN_POINT ( 'NONE',  ( -0.2867679344610364334, -0.2867679344610367109, -0.3011811023622048000 ) ) ;
#7031 = CARTESIAN_POINT ( 'NONE',  ( -0.3149606299212590610, -0.1870078740157479769, 0.3641732283464567677 ) ) ;
#7032 = CARTESIAN_POINT ( 'NONE',  ( -0.9055118110236215490, -0.6692913385826771977, 8.415575281601705876E-17 ) ) ;
#7033 = CARTESIAN_POINT ( 'NONE',  ( 1.312335958005249825, 0.2306618581243847221, -0.2411417322834647770 ) ) ;
#7034 = CARTESIAN_POINT ( 'NONE',  ( -0.6496062992125976043, 0.1660481256975883668, -0.3530559997133364547 ) ) ;
#7035 = ORIENTED_EDGE ( 'NONE', *, *, #5292, .F. ) ;
#7036 = VERTEX_POINT ( 'NONE', #7195 ) ;
#7037 = CARTESIAN_POINT ( 'NONE',  ( 0.1070741851644053388, 0.3996062992125986035, -1.802493438320209584 ) ) ;
#7039 = VECTOR ( 'NONE', #77599, 39.37007874015748143 ) ;
#7038 = CARTESIAN_POINT ( 'NONE',  ( -1.181102362204723644, -0.1870078740157479769, 0.4822834645669291653 ) ) ;
#7040 = CARTESIAN_POINT ( 'NONE',  ( 1.463254593175853824, 0.2952755905511810774, -0.1292274648535930714 ) ) ;
#7041 = CARTESIAN_POINT ( 'NONE',  ( -1.561679790026246017, -0.004921259842519576551, 0.3153832671262227771 ) ) ;
#7042 = CARTESIAN_POINT ( 'NONE',  ( -1.279527559055116948, -0.5400638737290844871, 0.3530559997133364547 ) ) ;
#7043 = CARTESIAN_POINT ( 'NONE',  ( 0.1265901696524989462, 0.4724409448818897572, -0.7808398950131233418 ) ) ;
#7044 = CARTESIAN_POINT ( 'NONE',  ( 0.000000000000000000, 2.755905511811024056, 0.000000000000000000 ) ) ;
#7045 = CARTESIAN_POINT ( 'NONE',  ( 0.1049643490035303689, 0.3917322834645670104, -0.1430446194225721002 ) ) ;
#7046 = CARTESIAN_POINT ( 'NONE',  ( 0.1049643490035303689, 0.3917322834645670104, -1.967847769028871374 ) ) ;
#7047 = CARTESIAN_POINT ( 'NONE',  ( -0.07874015748031421014, -0.1870078740157479769, 0.4822834645669291653 ) ) ;
#7048 = CARTESIAN_POINT ( 'NONE',  ( -1.587926509186350810, -0.004921259842519870586, -0.3153832671262229437 ) ) ;
#7049 = CARTESIAN_POINT ( 'NONE',  ( -0.6430446194225716283, -0.4281496062992124485, 0.4176697321401328655 ) ) ;
#7050 = CARTESIAN_POINT ( 'NONE',  ( -0.1070741851644056997, 0.3996062992125984925, 0.2316272965879264956 ) ) ;
#7052 = DIRECTION ( 'NONE',  ( -1.000000000000000000, 0.000000000000000000, 0.000000000000000000 ) ) ;
#7051 = CARTESIAN_POINT ( 'NONE',  ( -1.194225721784776262, 0.05413385826771626580, -0.4176697321401330321 ) ) ;
#7053 = ADVANCED_FACE ( 'NONE', ( #39173 ), #32342, .F. ) ;
#7054 = CARTESIAN_POINT ( 'NONE',  ( -0.8661417322834640276, -0.1870078740157480879, -0.4822834645669291653 ) ) ;
#7055 = CARTESIAN_POINT ( 'NONE',  ( -0.2690288713910754526, 0.2952755905511810774, -0.1292274648535930714 ) ) ;
#7056 = CARTESIAN_POINT ( 'NONE',  ( -0.3420746716998660508, -0.1974969037888706924, -2.648950131233596128 ) ) ;
#7057 = CARTESIAN_POINT ( 'NONE',  ( 0.9514435695538062676, -0.08942795157527998196, 0.3641732283464567121 ) ) ;
#7058 = CARTESIAN_POINT ( 'NONE',  ( 0.000000000000000000, 0.000000000000000000, -2.755905511811024056 ) ) ;
#7059 = CARTESIAN_POINT ( 'NONE',  ( 0.6496062992125991586, -0.4536011799217368745, -0.2665933059059886201 ) ) ;
#7060 = CARTESIAN_POINT ( 'NONE',  ( 1.286089238845145033, 0.1283753931104748280, 0.1820866141732283561 ) ) ;
#7061 = CARTESIAN_POINT ( 'NONE',  ( 1.266404199475066328, -0.05778040916215522460, 0.4822834645669289988 ) ) ;
#7062 = CARTESIAN_POINT ( 'NONE',  ( 0.2690288713910767848, 0.1771653543307087630, 0.09757992244046791164 ) ) ;
#7063 = CARTESIAN_POINT ( 'NONE',  ( 0.1958661417322834775, 0.3392501089628018884, -1.553805774278215202 ) ) ;
#7064 = CARTESIAN_POINT ( 'NONE',  ( -0.8202099737532799750, 0.2952755905511810774, -0.1292274648535930714 ) ) ;
#7065 = CARTESIAN_POINT ( 'NONE',  ( 1.220472440944882386, -0.6692913385826771977, 8.415575281601705876E-17 ) ) ;
#7066 = CARTESIAN_POINT ( 'NONE',  ( -0.1265901696524986964, -0.4724409448818899238, 0.008530183727034111943 ) ) ;
#7067 = CARTESIAN_POINT ( 'NONE',  ( -0.6102362204724400829, -0.4536011799217368745, -0.2665933059059886201 ) ) ;
#7068 = CARTESIAN_POINT ( 'NONE',  ( -0.4265091863517051496, 0.2952755905511810219, -0.1292274648535930437 ) ) ;
#7069 = CARTESIAN_POINT ( 'NONE',  ( 0.2493438320209980519, 0.05413385826771666132, 0.4176697321401328100 ) ) ;
#7070 = CARTESIAN_POINT ( 'NONE',  ( -1.646051170424378096, -0.1870078740157480046, 1.254653134982923898E-17 ) ) ;
#7071 = CARTESIAN_POINT ( 'NONE',  ( 0.8333333333333340365, 0.1771653543307087075, -0.09757992244046823083 ) ) ;
#7072 = CARTESIAN_POINT ( 'NONE',  ( 0.09842519685039434474, -0.4536011799217368745, -0.2665933059059886201 ) ) ;
#7073 = CARTESIAN_POINT ( 'NONE',  ( -0.2427821522309703550, -0.3162353388693405765, 0.4822834645669290543 ) ) ;
#7074 = CARTESIAN_POINT ( 'NONE',  ( -1.541994750656167090, 0.2952755905511811885, 0.1292274648535926551 ) ) ;
#7075 = CARTESIAN_POINT ( 'NONE',  ( -0.6036745406824141069, -0.5023911411419708095, -0.1820866141732282451 ) ) ;
#7076 = CARTESIAN_POINT ( 'NONE',  ( -1.614173228346457378, 1.055049524192299693, -0.1372047244094477536 ) ) ;
#7077 = CARTESIAN_POINT ( 'NONE',  ( -1.003937007874014853, 0.1660481256975885056, 0.3530559997133364547 ) ) ;
#7078 = CARTESIAN_POINT ( 'NONE',  ( -0.1998031496062994405, 0.3460692066303957537, -1.192257217847769057 ) ) ;
#7079 = CARTESIAN_POINT ( 'NONE',  ( -9.594673741351313045E-17, 0.3917322834645670104, -2.604330708661416693 ) ) ;
#7080 = CARTESIAN_POINT ( 'NONE',  ( -0.01312335958005186876, -0.3690944881889763329, 0.3153832671262228327 ) ) ;
#7081 = CARTESIAN_POINT ( 'NONE',  ( -0.5839895013123351797, -0.6692913385826771977, 0.1292274648535927661 ) ) ;
#7082 = CARTESIAN_POINT ( 'NONE',  ( -0.9251968503937002541, -0.5400638737290845981, -0.3530559997133363437 ) ) ;
#7083 = CARTESIAN_POINT ( 'NONE',  ( -1.181102362204723644, -0.1870078740157479769, 0.3641732283464567677 ) ) ;
#7084 = CARTESIAN_POINT ( 'NONE',  ( -1.646051170424378096, 0.000000000000000000, -0.3464511005275205946 ) ) ;
#7085 = CARTESIAN_POINT ( 'NONE',  ( -0.9514435695538050464, -0.08942795157528024563, -0.3641732283464568787 ) ) ;
#7086 = CARTESIAN_POINT ( 'NONE',  ( -1.417322834645668772, -0.1870078740157479769, 0.3641732283464567677 ) ) ;
#7087 = CARTESIAN_POINT ( 'NONE',  ( 1.364829396325459854, -0.6046776061558809534, -0.2411417322834644161 ) ) ;
#7088 = CARTESIAN_POINT ( 'NONE',  ( 0.4177787735907000366, 1.299212598425196985, -1.382006255033530806 ) ) ;
#7089 = VECTOR ( 'NONE', #81498, 39.37007874015748143 ) ;
#7090 = CARTESIAN_POINT ( 'NONE',  ( 0.2867679344610366554, -0.2867679344610365999, -2.457368397146668659 ) ) ;
#7091 = ORIENTED_EDGE ( 'NONE', *, *, #28945, .T. ) ;
#7092 = DIRECTION ( 'NONE',  ( 1.000000000000000000, -0.000000000000000000, -0.000000000000000000 ) ) ;
#7093 = CARTESIAN_POINT ( 'NONE',  ( -1.679790026246718693, 0.2306618581243847221, -0.2411417322834647770 ) ) ;
#7094 = CARTESIAN_POINT ( 'NONE',  ( -1.102362204724408601, -0.1870078740157479769, 0.4822834645669291653 ) ) ;
#7095 = CARTESIAN_POINT ( 'NONE',  ( 1.325459317585302665, 0.05413385826771626580, -0.4176697321401330321 ) ) ;
#7096 = CARTESIAN_POINT ( 'NONE',  ( -0.3392501089628017219, -0.1958661417322836718, -2.026902887139107712 ) ) ;
#7097 = LINE ( 'NONE', #7525, #63291 ) ;
#7098 = CARTESIAN_POINT ( 'NONE',  ( 0.5643044619422579178, 0.05413385826771666132, 0.4176697321401328100 ) ) ;
#7099 = CARTESIAN_POINT ( 'NONE',  ( 0.01968503937007957949, -0.5400638737290845981, -0.3530559997133363437 ) ) ;
#7100 = CARTESIAN_POINT ( 'NONE',  ( 0.1818635362617186391, 1.098419255088208812, -3.932883114322541118 ) ) ;
#7101 = CARTESIAN_POINT ( 'NONE',  ( -0.03178304480585582292, 0.3983403474834776858, -2.755905511811024500 ) ) ;
#7102 = CARTESIAN_POINT ( 'NONE',  ( 0.8464566929133865436, 0.07958543189024071263, -0.2665933059059888421 ) ) ;
#7103 = CARTESIAN_POINT ( 'NONE',  ( -0.3460692066303960868, 0.1998031496062990242, -1.286089238845144367 ) ) ;
#7104 = ORIENTED_EDGE ( 'NONE', *, *, #16133, .F. ) ;
#7105 = CARTESIAN_POINT ( 'NONE',  ( 0.3917322834645670659, -0.1049643490035303273, -0.1082870323172722415 ) ) ;
#7106 = ORIENTED_EDGE ( 'NONE', *, *, #79579, .F. ) ;
#7107 = CARTESIAN_POINT ( 'NONE',  ( 0.1509186351706042484, -0.3162353388693405765, 0.4822834645669290543 ) ) ;
#7108 = CARTESIAN_POINT ( 'NONE',  ( 1.601049868766404982, 0.2306618581243848609, 0.2411417322834645549 ) ) ;
#7109 = CARTESIAN_POINT ( 'NONE',  ( 0.6692913385826778638, -0.6692913385826771977, 8.415575281601705876E-17 ) ) ;
#7110 = CARTESIAN_POINT ( 'NONE',  ( 1.305774278215223960, -0.6692913385826771977, 0.1292274648535927661 ) ) ;
#7111 = CARTESIAN_POINT ( 'NONE',  ( 1.502624671916010790, -0.3162353388693409650, -0.4822834645669289433 ) ) ;
#7112 = CARTESIAN_POINT ( 'NONE',  ( -0.5839895013123351797, -0.6692913385826771977, 0.1292274648535927661 ) ) ;
#7113 = CARTESIAN_POINT ( 'NONE',  ( 0.2034120734908142214, 0.2952755905511810774, -0.1292274648535930714 ) ) ;
#7114 = CARTESIAN_POINT ( 'NONE',  ( -1.482939632545930975, 0.05413385826771666132, 0.4176697321401328100 ) ) ;
#7115 = CARTESIAN_POINT ( 'NONE',  ( 1.384514435695538337, -0.6692913385826771977, 0.1292274648535927661 ) ) ;
#7116 = CARTESIAN_POINT ( 'NONE',  ( 1.010498687664042716, -0.4281496062992124485, 0.4176697321401328655 ) ) ;
#7117 = CARTESIAN_POINT ( 'NONE',  ( -0.03937007874015669567, -0.6692913385826771977, 8.415575281601705876E-17 ) ) ;
#7118 = CARTESIAN_POINT ( 'NONE',  ( -0.1958661417322834220, -0.3392501089628018884, -0.3727034120734908362 ) ) ;
#7119 = CARTESIAN_POINT ( 'NONE',  ( 0.4461942257217856311, 0.1283753931104746893, -0.1820866141732285504 ) ) ;
#7120 = VERTEX_POINT ( 'NONE', #45895 ) ;
#7121 = CARTESIAN_POINT ( 'NONE',  ( 0.3949938075777409963, 2.418639510665530435E-17, -0.7480314960629920185 ) ) ;
#7122 = VERTEX_POINT ( 'NONE', #58535 ) ;
#7123 = CARTESIAN_POINT ( 'NONE',  ( -0.3018372703412066094, -0.004921259842519576551, 0.3153832671262227771 ) ) ;
#7124 = CARTESIAN_POINT ( 'NONE',  ( 2.585397804484631745, 1.422882880004780581, -0.4606469518571244537 ) ) ;
#7125 = CARTESIAN_POINT ( 'NONE',  ( 0.03937007874015806264, 0.2952755905511811885, 0.000000000000000000 ) ) ;
#7126 = CARTESIAN_POINT ( 'NONE',  ( -0.03280839895013062252, -0.6692913385826771977, 0.1292274648535927661 ) ) ;
#7127 = CARTESIAN_POINT ( 'NONE',  ( -1.095800524934382292, -0.05778040916215522460, 0.4822834645669289988 ) ) ;
#7128 = CARTESIAN_POINT ( 'NONE',  ( 1.496062992125985147, -0.1870078740157479769, 0.3641732283464567677 ) ) ;
#7129 = CARTESIAN_POINT ( 'NONE',  ( -1.640419947506561060, 0.05413385826771666132, 0.4176697321401328100 ) ) ;
#7130 = CARTESIAN_POINT ( 'NONE',  ( -0.4724409448818880364, -0.1265901696525023323, -2.723097112860892732 ) ) ;
#7131 = CARTESIAN_POINT ( 'NONE',  ( 0.8070866141732288002, 0.07958543189024085140, 0.2665933059059887866 ) ) ;
#7132 = VECTOR ( 'NONE', #48788, 39.37007874015748143 ) ;
#7133 = CARTESIAN_POINT ( 'NONE',  ( 0.6561679790026253567, -0.6046776061558809534, -0.2411417322834644161 ) ) ;
#7134 = CARTESIAN_POINT ( 'NONE',  ( 0.8070866141732289112, -0.5400638737290845981, -0.3530559997133363437 ) ) ;
#7135 = CARTESIAN_POINT ( 'NONE',  ( -0.3996062992125987146, 0.1070741851644051862, -1.135170603674540590 ) ) ;
#7136 = CARTESIAN_POINT ( 'NONE',  ( -1.640419947506561060, -0.4281496062992127816, -0.4176697321401328100 ) ) ;
#7137 = CARTESIAN_POINT ( 'NONE',  ( 0.1070741851644053388, 0.3996062992125986035, -0.7001312335958002064 ) ) ;
#7138 = CARTESIAN_POINT ( 'NONE',  ( -0.3996062992125986590, 0.1070741851644051723, -0.2670603674540683037 ) ) ;
#7139 = CARTESIAN_POINT ( 'NONE',  ( 5.463695987328526437E-16, -0.1870078740157479769, 0.4822834645669291653 ) ) ;
#7140 = CARTESIAN_POINT ( 'NONE',  ( -0.1070741851644056997, 0.3996062992125986035, -2.683727034120735322 ) ) ;
#7141 = CARTESIAN_POINT ( 'NONE',  ( 0.3917322834645669549, 0.1049643490035304660, -2.099081364829396446 ) ) ;
#7142 = CARTESIAN_POINT ( 'NONE',  ( -1.017060367454067249, -0.08942795157527998196, 0.3641732283464567121 ) ) ;
#7143 = CARTESIAN_POINT ( 'NONE',  ( 1.305774278215223960, 0.2952755905511810774, -0.1292274648535930714 ) ) ;
#7144 = CARTESIAN_POINT ( 'NONE',  ( 1.148293963254593875, -0.6692913385826771977, 0.1292274648535927661 ) ) ;
#7145 = CARTESIAN_POINT ( 'NONE',  ( 0.1771653543307093182, -0.4536011799217368745, -0.2665933059059886201 ) ) ;
#7146 = CARTESIAN_POINT ( 'NONE',  ( 0.3346456692913390985, 0.1660481256975885056, 0.3530559997133364547 ) ) ;
#7147 = CARTESIAN_POINT ( 'NONE',  ( 0.4724409448818897572, -0.1265901696524988906, -1.448162729658792669 ) ) ;
#7148 = CARTESIAN_POINT ( 'NONE',  ( 0.4396325459317593221, 0.1771653543307087075, -0.09757992244046823083 ) ) ;
#7149 = CARTESIAN_POINT ( 'NONE',  ( 0.1443569553805781891, -0.4281496062992124485, 0.4176697321401328655 ) ) ;
#7150 = EDGE_CURVE ( 'NONE', #49578, #9799, #39601, .T. ) ;
#7151 = CIRCLE ( 'NONE', #29971, 3.582677165354331450 ) ;
#7152 = CARTESIAN_POINT ( 'NONE',  ( -9.674558042662122972E-17, 0.3949938075777409963, -1.494094488188976388 ) ) ;
#7153 = CARTESIAN_POINT ( 'NONE',  ( -1.233595800524933894, 0.2306618581243848609, 0.2411417322834645549 ) ) ;
#7154 = CARTESIAN_POINT ( 'NONE',  ( 0.3805774278215230400, -0.004921259842519870586, -0.3153832671262229437 ) ) ;
#7155 = CARTESIAN_POINT ( 'NONE',  ( -1.167979002624671470, 0.05413385826771666132, 0.4176697321401328100 ) ) ;
#7156 = CARTESIAN_POINT ( 'NONE',  ( -0.7611548556430438595, 0.2306618581243848609, 0.2411417322834645549 ) ) ;
#7157 = CARTESIAN_POINT ( 'NONE',  ( -0.1312335958005241554, -0.5023911411419708095, -0.1820866141732282451 ) ) ;
#7158 = CARTESIAN_POINT ( 'NONE',  ( -2.554859668665151240, 1.520054044952884098, -0.4741688556381182251 ) ) ;
#7159 = CARTESIAN_POINT ( 'NONE',  ( -0.9448818897637790704, -0.1870078740157479769, 0.4822834645669291653 ) ) ;
#7160 = CARTESIAN_POINT ( 'NONE',  ( -0.05905511811023545637, 0.1660481256975885056, 0.3530559997133364547 ) ) ;
#7161 = CARTESIAN_POINT ( 'NONE',  ( 0.4921259842519691285, 0.07958543189024085140, 0.2665933059059887866 ) ) ;
#7162 = CARTESIAN_POINT ( 'NONE',  ( -0.3996062992125985480, -7.340648628747423112E-17, -2.320866141732283783 ) ) ;
#7163 = CARTESIAN_POINT ( 'NONE',  ( 0.03280839895013198948, -0.6692913385826773087, -0.1292274648535924053 ) ) ;
#7164 = CARTESIAN_POINT ( 'NONE',  ( 0.3392501089628018329, 0.1958661417322835052, -1.943550238023935561 ) ) ;
#7165 = DIRECTION ( 'NONE',  ( 1.047444401652940007E-14, -0.000000000000000000, -1.000000000000000000 ) ) ;
#7166 = CARTESIAN_POINT ( 'NONE',  ( 0.7677165354330716118, 0.07958543189024071263, -0.2665933059059888421 ) ) ;
#7167 = CARTESIAN_POINT ( 'NONE',  ( 1.417322834645670104, -0.1870078740157479769, 0.4822834645669291653 ) ) ;
#7168 = CARTESIAN_POINT ( 'NONE',  ( -0.8005249343832013809, -0.3690944881889763329, 0.3153832671262228327 ) ) ;
#7169 = CARTESIAN_POINT ( 'NONE',  ( -1.043307086614172707, 0.07958543189024071263, -0.2665933059059888421 ) ) ;
#7170 = CARTESIAN_POINT ( 'NONE',  ( -0.6496062992125976043, 0.1660481256975883668, -0.3530559997133364547 ) ) ;
#7171 = CARTESIAN_POINT ( 'NONE',  ( -0.1640419947506555343, -0.3162353388693405765, 0.4822834645669290543 ) ) ;
#7172 = CARTESIAN_POINT ( 'NONE',  ( 0.3937007874015754361, -0.1870078740157479769, 0.3641732283464567677 ) ) ;
#7173 = CARTESIAN_POINT ( 'NONE',  ( -1.968503937007874072, 0.000000000000000000, 5.701968306260621233 ) ) ;
#7174 = CARTESIAN_POINT ( 'NONE',  ( 0.9842519685039375910, 0.1771653543307087630, 0.000000000000000000 ) ) ;
#7175 = CARTESIAN_POINT ( 'NONE',  ( 0.3215223097112867578, -0.3162353388693409650, -0.4822834645669289433 ) ) ;
#7176 = CARTESIAN_POINT ( 'NONE',  ( 0.1998031496062994128, -0.3460692066303957537, 0.1463254593175852825 ) ) ;
#7177 = CARTESIAN_POINT ( 'NONE',  ( -0.3608923884514428360, -0.6692913385826773087, -0.1292274648535924053 ) ) ;
#7178 = CARTESIAN_POINT ( 'NONE',  ( -0.3917322834645669549, -0.1049643490035306603, -1.547900262467191590 ) ) ;
#7179 = CARTESIAN_POINT ( 'NONE',  ( 1.450131233595801428, 0.1771653543307087630, 0.09757992244046791164 ) ) ;
#7180 = CARTESIAN_POINT ( 'NONE',  ( 0.4790026246719168435, -0.3162353388693409650, -0.4822834645669289433 ) ) ;
#7181 = CARTESIAN_POINT ( 'NONE',  ( 0.3346456692913393205, -0.5400638737290845981, -0.3530559997133363437 ) ) ;
#7182 = CARTESIAN_POINT ( 'NONE',  ( 1.113061397484515158, -1.206088964116209378E-16, 0.4118477457932991359 ) ) ;
#7183 = CARTESIAN_POINT ( 'NONE',  ( -0.1049868766404193215, -0.5023911411419708095, 0.1820866141732285504 ) ) ;
#7184 = CARTESIAN_POINT ( 'NONE',  ( 0.8267716535433078384, -0.6692913385826771977, 8.415575281601705876E-17 ) ) ;
#7185 = CARTESIAN_POINT ( 'NONE',  ( -0.1312335958005241554, 0.1283753931104748280, 0.1820866141732283561 ) ) ;
#7186 = CARTESIAN_POINT ( 'NONE',  ( -0.8070866141732276899, 0.1660481256975883668, -0.3530559997133364547 ) ) ;
#7187 = CARTESIAN_POINT ( 'NONE',  ( -0.3149606299212590610, -0.1870078740157479769, 0.4822834645669291653 ) ) ;
#7188 = ORIENTED_EDGE ( 'NONE', *, *, #6175, .F. ) ;
#7189 = CARTESIAN_POINT ( 'NONE',  ( -1.161417322834644716, 0.1660481256975885056, 0.3530559997133364547 ) ) ;
#7190 = AXIS2_PLACEMENT_3D ( 'NONE', #65591, #352, #7503 ) ;
#7191 = CARTESIAN_POINT ( 'NONE',  ( -0.6955380577427815458, -0.3690944881889765550, -0.3153832671262227771 ) ) ;
#7192 = CARTESIAN_POINT ( 'NONE',  ( 0.09842519685039434474, -0.5400638737290845981, -0.3530559997133363437 ) ) ;
#7193 = CARTESIAN_POINT ( 'NONE',  ( -1.437007874015747477, -0.5400638737290844871, 0.3530559997133364547 ) ) ;
#7194 = CARTESIAN_POINT ( 'NONE',  ( -0.7808398950131222316, -0.3162353388693409650, -0.4822834645669289433 ) ) ;
#7195 = CARTESIAN_POINT ( 'NONE',  ( 0.5314960629921372526, 2.716535433070866645, -3.224202737261813834 ) ) ;
#7197 = CARTESIAN_POINT ( 'NONE',  ( 1.279527559055118724, 0.1660481256975885056, 0.3530559997133364547 ) ) ;
#7196 = CARTESIAN_POINT ( 'NONE',  ( 1.653543307086614789, -0.1870078740157479769, 0.4822834645669291653 ) ) ;
#7198 = CARTESIAN_POINT ( 'NONE',  ( 1.391076115485564868, 0.2306618581243847221, -0.2411417322834647770 ) ) ;
#7199 = CARTESIAN_POINT ( 'NONE',  ( -0.1049643490035307020, 0.3917322834645669549, -2.518372703412073754 ) ) ;
#7200 = CARTESIAN_POINT ( 'NONE',  ( 0.000000000000000000, 2.165354330708661568, 0.000000000000000000 ) ) ;
#7201 = B_SPLINE_CURVE_WITH_KNOTS ( 'NONE', 3,
 ( #3584, #82261, #42280, #29250, #43100, #74711, #24579 ),
 .UNSPECIFIED., .F., .F.,
 ( 4, 3, 4 ),
 ( 3.642919299551295515E-17, 0.001246232571205268744, 0.002492492258783277591 ),
 .UNSPECIFIED. ) ;
#7202 = CARTESIAN_POINT ( 'NONE',  ( -1.515748031496062076, 0.1660481256975883668, -0.3530559997133364547 ) ) ;
#7203 = CARTESIAN_POINT ( 'NONE',  ( 0.4724409448818896462, 0.1265901696524990294, -0.7545931758530182165 ) ) ;
#7204 = CARTESIAN_POINT ( 'NONE',  ( 0.3996062992125986590, -0.1070741851644053111, -0.1115485564304461857 ) ) ;
#7205 = VERTEX_POINT ( 'NONE', #13944 ) ;
#7206 = CARTESIAN_POINT ( 'NONE',  ( -0.1837270341207340729, 0.1283753931104746893, -0.1820866141732285504 ) ) ;
#7208 = CARTESIAN_POINT ( 'NONE',  ( -0.2867679344610364334, -0.2867679344610367109, -1.783464566929133577 ) ) ;
#7207 = VECTOR ( 'NONE', #69539, 39.37007874015748143 ) ;
#7209 = VERTEX_POINT ( 'NONE', #78757 ) ;
#7210 = CARTESIAN_POINT ( 'NONE',  ( 0.2690288713910767848, -0.6692913385826773087, -0.1292274648535924053 ) ) ;
#7211 = CARTESIAN_POINT ( 'NONE',  ( 0.3346456692913390985, 0.1660481256975885056, 0.3530559997133364547 ) ) ;
#7212 = CARTESIAN_POINT ( 'NONE',  ( -0.4091458600556402980, -0.2362204724409451284, -2.729658792650918375 ) ) ;
#7213 = CARTESIAN_POINT ( 'NONE',  ( 2.795275590551181466, 0.4724409448818907564, -3.234977217930338483E-16 ) ) ;
#7214 = CARTESIAN_POINT ( 'NONE',  ( -0.9448818897637790704, -0.1870078740157480601, -0.3641732283464567677 ) ) ;
#7215 = CARTESIAN_POINT ( 'NONE',  ( 0.9448818897637802916, -0.1870078740157480879, -0.4822834645669291653 ) ) ;
#7216 = CARTESIAN_POINT ( 'NONE',  ( 0.9448818897637802916, -0.1870078740157479769, 0.3641732283464567677 ) ) ;
#7217 = CARTESIAN_POINT ( 'NONE',  ( -0.3149606299212590610, -0.1870078740157480879, -0.4822834645669291653 ) ) ;
#7218 = CARTESIAN_POINT ( 'NONE',  ( -0.3917322834645669549, -7.196005306013483243E-17, -1.221765461121048224 ) ) ;
#7219 = CARTESIAN_POINT ( 'NONE',  ( -0.7480314960629914633, -0.6692913385826771977, 8.415575281601705876E-17 ) ) ;
#7220 = CARTESIAN_POINT ( 'NONE',  ( -1.653543307086613234, -0.1870078740157480601, -0.3641732283464567677 ) ) ;
#7221 = CARTESIAN_POINT ( 'NONE',  ( -0.8661417322834640276, -0.1870078740157480879, -0.4822834645669291653 ) ) ;
#7222 = CARTESIAN_POINT ( 'NONE',  ( 1.463254593175853824, -0.6692913385826771977, 0.1292274648535927661 ) ) ;
#7223 = CARTESIAN_POINT ( 'NONE',  ( -0.3811282389481102650, 1.253478596003495094, -2.019714574425724773 ) ) ;
#7224 = ORIENTED_EDGE ( 'NONE', *, *, #62746, .F. ) ;
#7225 = CARTESIAN_POINT ( 'NONE',  ( 0.3917322834645670659, -0.1049643490035303273, -2.470491756726720833 ) ) ;
#7226 = CARTESIAN_POINT ( 'NONE',  ( 0.006561679790026889343, -0.3162353388693409650, -0.4822834645669289433 ) ) ;
#7227 = ORIENTED_EDGE ( 'NONE', *, *, #28583, .T. ) ;
#7228 = CARTESIAN_POINT ( 'NONE',  ( -0.8530183727034112984, -0.4281496062992127816, -0.4176697321401328100 ) ) ;
#7229 = CARTESIAN_POINT ( 'NONE',  ( 1.351706036745407458, -0.4281496062992127816, -0.4176697321401328100 ) ) ;
#7230 = CARTESIAN_POINT ( 'NONE',  ( 1.108923884514436242, -0.05778040916215522460, 0.4822834645669289988 ) ) ;
#7231 = CARTESIAN_POINT ( 'NONE',  ( 0.3740157480314966754, 0.1660481256975883668, -0.3530559997133364547 ) ) ;
#7232 = CARTESIAN_POINT ( 'NONE',  ( -0.3543307086614165824, 0.2952755905511811885, 0.000000000000000000 ) ) ;
#7233 = CARTESIAN_POINT ( 'NONE',  ( -0.1049643490035307020, 0.3917322834645669549, -1.980971128608924214 ) ) ;
#7234 = CARTESIAN_POINT ( 'NONE',  ( -1.391076115485563758, 0.2306618581243848609, 0.2411417322834645549 ) ) ;
#7235 = CARTESIAN_POINT ( 'NONE',  ( 8.195543980992789655E-16, -0.1870078740157480879, -0.4822834645669291653 ) ) ;
#7236 = CARTESIAN_POINT ( 'NONE',  ( -0.07217847769028787330, -0.08942795157527998196, 0.3641732283464567121 ) ) ;
#7237 = DIRECTION ( 'NONE',  ( 1.000000000000000000, 0.000000000000000000, 0.000000000000000000 ) ) ;
#7238 = CARTESIAN_POINT ( 'NONE',  ( 1.384514435695538559, 0.2952755905511810774, -0.1292274648535930714 ) ) ;
#7239 = CARTESIAN_POINT ( 'NONE',  ( -0.7020997375328076329, -0.3162353388693409650, -0.4822834645669289433 ) ) ;
#7240 = CARTESIAN_POINT ( 'NONE',  ( 0.2486400153428833526, 3.421639014772782816E-16, 0.3464511005275203726 ) ) ;
#7241 = CARTESIAN_POINT ( 'NONE',  ( 1.213910761154856299, -0.6692913385826773087, -0.1292274648535924053 ) ) ;
#7242 = CARTESIAN_POINT ( 'NONE',  ( -1.646051170424378096, 0.000000000000000000, 0.3464511005275205946 ) ) ;
#7243 = EDGE_LOOP ( 'NONE', ( #13850, #31758, #70154, #14288 ) ) ;
#7244 = EDGE_CURVE ( 'NONE', #51509, #69851, #21492, .T. ) ;
#7245 = EDGE_LOOP ( 'NONE', ( #17930, #40654, #64677, #18814 ) ) ;
#7246 = CARTESIAN_POINT ( 'NONE',  ( 0.4199475065616805614, 0.2306618581243848609, 0.2411417322834645549 ) ) ;
#7247 = CARTESIAN_POINT ( 'NONE',  ( -0.4068241469816267775, -0.004921259842519870586, -0.3153832671262229437 ) ) ;
#7249 = CARTESIAN_POINT ( 'NONE',  ( 1.614173228346457378, 0.5038684218300978346, -0.1372047244094476148 ) ) ;
#7248 = CARTESIAN_POINT ( 'NONE',  ( 1.607611548556431069, -0.5511811023622048555, -0.09757992244046775898 ) ) ;
#7250 = CARTESIAN_POINT ( 'NONE',  ( -1.157146581871515012E-16, 0.4724409448818898682, -0.2342519685039370358 ) ) ;
#7251 = CARTESIAN_POINT ( 'NONE',  ( 1.660104986876641320, -0.08942795157527998196, 0.3641732283464567121 ) ) ;
#7252 = CARTESIAN_POINT ( 'NONE',  ( 1.148293963254593653, 0.2952755905511810774, -0.1292274648535930714 ) ) ;
#7253 = CARTESIAN_POINT ( 'NONE',  ( -0.1974969037888704149, -0.3420746716998661063, 0.01509186351706036378 ) ) ;
#7254 = CARTESIAN_POINT ( 'NONE',  ( 0.1902887139107617975, 0.2952755905511811885, 0.1292274648535926551 ) ) ;
#7255 = CARTESIAN_POINT ( 'NONE',  ( -1.601049868766403650, 0.2306618581243847221, -0.2411417322834647770 ) ) ;
#7256 = VECTOR ( 'NONE', #23687, 39.37007874015748143 ) ;
#7257 = CARTESIAN_POINT ( 'NONE',  ( -1.699475065616797398, 0.2952755905511811885, 0.1292274648535926551 ) ) ;
#7258 = CARTESIAN_POINT ( 'NONE',  ( 0.03937007874015806264, 0.2952755905511811885, 0.000000000000000000 ) ) ;
#7259 = CARTESIAN_POINT ( 'NONE',  ( -0.1974969037888704149, -0.3420746716998661063, 0.01509186351706036378 ) ) ;
#7260 = CARTESIAN_POINT ( 'NONE',  ( 1.640419947506562393, -0.4281496062992124485, 0.4176697321401328655 ) ) ;
#7261 = CARTESIAN_POINT ( 'NONE',  ( 0.6692913385826777528, 0.2952755905511811885, 0.000000000000000000 ) ) ;
#7262 = CARTESIAN_POINT ( 'NONE',  ( 0.9186351706036752773, 0.1283753931104746893, -0.1820866141732285504 ) ) ;
#7263 = CARTESIAN_POINT ( 'NONE',  ( 0.3104096989839266740, 1.295945406154406454, 0.04180176832660051356 ) ) ;
#7264 = CARTESIAN_POINT ( 'NONE',  ( 1.030183727034121421, -0.08942795157527998196, 0.3641732283464567121 ) ) ;
#7265 = CARTESIAN_POINT ( 'NONE',  ( -1.148293963254592542, 0.2952755905511811885, 0.1292274648535926551 ) ) ;
#7266 = CARTESIAN_POINT ( 'NONE',  ( -0.3460692066303960313, 0.1998031496062989965, -1.047900262467191590 ) ) ;
#7267 = CARTESIAN_POINT ( 'NONE',  ( 1.200787401574803681, 0.1660481256975885056, 0.3530559997133364547 ) ) ;
#7268 = CARTESIAN_POINT ( 'NONE',  ( 0.1049643490035303689, 0.3917322834645670104, -0.4580052493438320216 ) ) ;
#7270 = DIRECTION ( 'NONE',  ( -3.491481338843132961E-15, 0.000000000000000000, 1.000000000000000000 ) ) ;
#7269 = CARTESIAN_POINT ( 'NONE',  ( 0.6758530183727039509, -0.6692913385826771977, 0.1292274648535927661 ) ) ;
#7271 = CARTESIAN_POINT ( 'NONE',  ( 0.3983403474834781299, 0.03178304480585100733, -1.929133858267716661 ) ) ;
#7272 = CARTESIAN_POINT ( 'NONE',  ( 0.2755905511811031494, -0.5511811023622047445, 6.969142054262312111E-17 ) ) ;
#7273 = AXIS2_PLACEMENT_3D ( 'NONE', #67879, #55219, #80926 ) ;
#7274 = CARTESIAN_POINT ( 'NONE',  ( 0.5380577427821529035, -0.4281496062992124485, 0.4176697321401328655 ) ) ;
#7275 = CARTESIAN_POINT ( 'NONE',  ( -0.4741686481756466343, 1.554815631980117185, 2.169549097624130951 ) ) ;
#7276 = CARTESIAN_POINT ( 'NONE',  ( -0.9580052493438311334, -0.3690944881889763329, 0.3153832671262228327 ) ) ;
#7277 = CARTESIAN_POINT ( 'NONE',  ( -0.9448818897637790704, -0.1870078740157479769, 0.4822834645669291653 ) ) ;
#7278 = CARTESIAN_POINT ( 'NONE',  ( 1.187664041994751285, -0.05778040916215522460, 0.4822834645669289988 ) ) ;
#7279 = CARTESIAN_POINT ( 'NONE',  ( -1.574803149606298636, -0.1870078740157479769, 0.4822834645669291653 ) ) ;
#7280 = CARTESIAN_POINT ( 'NONE',  ( 1.102362204724410155, -0.1870078740157480879, -0.4822834645669291653 ) ) ;
#7281 = CARTESIAN_POINT ( 'NONE',  ( 1.450131233595801428, -0.6692913385826773087, -0.1292274648535924053 ) ) ;
#7282 = CARTESIAN_POINT ( 'NONE',  ( -0.3937527723457945883, 0.009287274676460462175, -1.220472440944884163 ) ) ;
#7283 = CARTESIAN_POINT ( 'NONE',  ( 0.9514435695538062676, -0.05778040916215522460, 0.4822834645669289988 ) ) ;
#7284 = CARTESIAN_POINT ( 'NONE',  ( -0.4724409448818899238, 0.1265901696524986686, -2.629265091863517423 ) ) ;
#7285 = CARTESIAN_POINT ( 'NONE',  ( 1.522309711286089939, 0.2306618581243848609, 0.2411417322834645549 ) ) ;
#7286 = CARTESIAN_POINT ( 'NONE',  ( 1.574803149606299746, -0.1870078740157480879, -0.4822834645669291653 ) ) ;
#7287 = CARTESIAN_POINT ( 'NONE',  ( -1.601049868766403650, -0.5023911411419708095, 0.1820866141732285504 ) ) ;
#7288 = CARTESIAN_POINT ( 'NONE',  ( 1.102362204724410155, -0.1870078740157480601, -0.3641732283464567677 ) ) ;
#7289 = CARTESIAN_POINT ( 'NONE',  ( -1.364829396325458521, -0.5023911411419708095, 0.1820866141732285504 ) ) ;
#7290 = CARTESIAN_POINT ( 'NONE',  ( -0.5708661417322825615, -0.4536011799217367080, 0.2665933059059888421 ) ) ;
#7291 = CARTESIAN_POINT ( 'NONE',  ( -1.377952755905511140, 0.1771653543307087630, 0.000000000000000000 ) ) ;
#7292 = CARTESIAN_POINT ( 'NONE',  ( 0.7545931758530188826, -0.5511811023622046335, 0.09757992244046803654 ) ) ;
#7293 = CARTESIAN_POINT ( 'NONE',  ( 0.7414698162729663755, 0.2952755905511811885, 0.1292274648535926551 ) ) ;
#7294 = CARTESIAN_POINT ( 'NONE',  ( 1.030183727034121421, -0.3162353388693409650, -0.4822834645669289433 ) ) ;
#7295 = CARTESIAN_POINT ( 'NONE',  ( 0.2296587926509192634, -0.3162353388693405765, 0.4822834645669290543 ) ) ;
#7296 = CARTESIAN_POINT ( 'NONE',  ( 0.4199475065616803948, -0.5023911411419708095, -0.1820866141732282451 ) ) ;
#7297 = CARTESIAN_POINT ( 'NONE',  ( 1.502624671916010790, -0.3162353388693409650, -0.4822834645669289433 ) ) ;
#7298 = SHAPE_REPRESENTATION ( 'Cast Iron Heavy Chuck Body', ( #22098 ), #5981 ) ;
#7299 = CARTESIAN_POINT ( 'NONE',  ( 0.9881811337016640495, 2.559055118110236560, 0.5314960629921260393 ) ) ;
#7300 = CARTESIAN_POINT ( 'NONE',  ( -0.5905511811023615998, 0.2952755905511811885, 0.000000000000000000 ) ) ;
#7301 = CARTESIAN_POINT ( 'NONE',  ( 0.1998031496062992740, 0.3460692066303959757, -0.3018372703412073865 ) ) ;
#7302 = DIRECTION ( 'NONE',  ( 0.000000000000000000, 0.000000000000000000, 1.000000000000000000 ) ) ;
#7303 = CARTESIAN_POINT ( 'NONE',  ( 0.1509186351706042484, -0.3162353388693405765, 0.4822834645669290543 ) ) ;
#7304 = CARTESIAN_POINT ( 'NONE',  ( -0.5118110236220466680, 0.2952755905511811885, 0.000000000000000000 ) ) ;
#7305 = CARTESIAN_POINT ( 'NONE',  ( -0.1377952755905504645, 0.1660481256975885056, 0.3530559997133364547 ) ) ;
#7306 = CARTESIAN_POINT ( 'NONE',  ( 0.3460692066303959202, 0.1998031496062993295, -2.808398950131233640 ) ) ;
#7307 = CARTESIAN_POINT ( 'NONE',  ( -0.2891555358219908833, -0.2891555358219912164, -1.948818897637795144 ) ) ;
#7308 = CARTESIAN_POINT ( 'NONE',  ( -0.3917322834645669549, -0.1049643490035306603, -0.6679790026246719137 ) ) ;
#7309 = CARTESIAN_POINT ( 'NONE',  ( 0.1694133573824175565, 1.763362281772084768E-16, 0.3627985898453517377 ) ) ;
#7310 = AXIS2_PLACEMENT_3D ( 'NONE', #58276, #26719, #70497 ) ;
#7311 = CARTESIAN_POINT ( 'NONE',  ( -0.3917322834645670104, -7.196005306013484475E-17, -0.9763779527559053317 ) ) ;
#7312 = CARTESIAN_POINT ( 'NONE',  ( -0.9448818897637790704, -0.1870078740157479769, 0.3641732283464567677 ) ) ;
#7313 = CARTESIAN_POINT ( 'NONE',  ( -0.3917322834645670104, -7.196005306013484475E-17, -1.133858267716535195 ) ) ;
#7314 = CARTESIAN_POINT ( 'NONE',  ( -1.286089238845143479, -0.6046776061558807314, 0.2411417322834647770 ) ) ;
#7315 = CARTESIAN_POINT ( 'NONE',  ( 4.837279021331061486E-17, -0.3949938075777409963, -2.832677165354331006 ) ) ;
#7316 = CARTESIAN_POINT ( 'NONE',  ( 0.5774278215223104249, 0.2306618581243848609, 0.2411417322834645549 ) ) ;
#7317 = CARTESIAN_POINT ( 'NONE',  ( 0.01312335958005323398, -0.004921259842519576551, 0.3153832671262227771 ) ) ;
#7318 = CARTESIAN_POINT ( 'NONE',  ( 1.410761154855643795, -0.3162353388693405765, 0.4822834645669290543 ) ) ;
#7319 = CARTESIAN_POINT ( 'NONE',  ( 0.2362204724409456558, -0.1870078740157480879, -0.4822834645669291653 ) ) ;
#7320 = FACE_OUTER_BOUND ( 'NONE', #72274, .T. ) ;
#7321 = CARTESIAN_POINT ( 'NONE',  ( 0.2925321140481932369, 0.2925321140481932369, -2.657480314960630530 ) ) ;
#7322 = CARTESIAN_POINT ( 'NONE',  ( -0.2867679344610365444, -0.2867679344610367664, -1.158155798721471896 ) ) ;
#7323 = CARTESIAN_POINT ( 'NONE',  ( 1.345144356955381593, -0.05778040916215522460, 0.4822834645669289988 ) ) ;
#7324 = CARTESIAN_POINT ( 'NONE',  ( 0.3083989501312343062, -0.3162353388693405765, 0.4822834645669290543 ) ) ;
#7325 = CARTESIAN_POINT ( 'NONE',  ( 0.3477690288713918276, 0.2952755905511811885, 0.1292274648535926551 ) ) ;
#7326 = AXIS2_PLACEMENT_3D ( 'NONE', #42206, #54000, #22028 ) ;
#7327 = CARTESIAN_POINT ( 'NONE',  ( 1.397637795275591177, 0.1660481256975883668, -0.3530559997133364547 ) ) ;
#7328 = CARTESIAN_POINT ( 'NONE',  ( -9.594673741351313045E-17, 0.3917322834645670104, -0.3996062992125985480 ) ) ;
#7329 = CARTESIAN_POINT ( 'NONE',  ( 0.2427821522309716595, -0.3162353388693409650, -0.4822834645669289433 ) ) ;
#7330 = CARTESIAN_POINT ( 'NONE',  ( 1.161417322834646493, -0.5400638737290844871, 0.3530559997133364547 ) ) ;
#7331 = CARTESIAN_POINT ( 'NONE',  ( 0.5839895013123367340, 0.2952755905511811885, 0.1292274648535926551 ) ) ;
#7332 = CARTESIAN_POINT ( 'NONE',  ( 1.128608923884515169, -0.5023911411419708095, -0.1820866141732282451 ) ) ;
#7333 = CARTESIAN_POINT ( 'NONE',  ( -1.043307086614172707, 0.1660481256975883668, -0.3530559997133364547 ) ) ;
#7334 = CARTESIAN_POINT ( 'NONE',  ( -1.489501312335957062, -0.3162353388693409650, -0.4822834645669289433 ) ) ;
#7335 = CARTESIAN_POINT ( 'NONE',  ( 0.7414698162729663755, -0.6692913385826773087, -0.1292274648535924053 ) ) ;
#7336 = CARTESIAN_POINT ( 'NONE',  ( -0.4724409448818890911, 0.1265901696525001952, -0.5820209973753279753 ) ) ;
#7337 = CARTESIAN_POINT ( 'NONE',  ( 0.3392501089628018329, 0.1958661417322835607, -1.855643044619422533 ) ) ;
#7338 = VERTEX_POINT ( 'NONE', #77915 ) ;
#7339 = CARTESIAN_POINT ( 'NONE',  ( 0.3996062992125986035, 2.446882876249141962E-17, -0.1181102362204724671 ) ) ;
#7340 = ORIENTED_EDGE ( 'NONE', *, *, #10682, .F. ) ;
#7341 = CARTESIAN_POINT ( 'NONE',  ( 1.417322834645670104, -0.1870078740157480879, -0.4822834645669291653 ) ) ;
#7342 = CARTESIAN_POINT ( 'NONE',  ( 0.8989501312335963501, -0.5511811023622048555, -0.09757992244046775898 ) ) ;
#7343 = CARTESIAN_POINT ( 'NONE',  ( 0.6179882174207333989, 6.425613173282222329E-18, -0.3627985898453512936 ) ) ;
#7344 = CARTESIAN_POINT ( 'NONE',  ( -0.1474713956048439301, -2.191421614605370878E-15, 0.4445507791589071167 ) ) ;
#7345 = LINE ( 'NONE', #33013, #68750 ) ;
#7346 = CARTESIAN_POINT ( 'NONE',  ( -0.2867679344610365999, 0.2867679344610364889, -1.049212598425196763 ) ) ;
#7347 = CARTESIAN_POINT ( 'NONE',  ( -1.240157480314959759, -0.4536011799217368745, -0.2665933059059886201 ) ) ;
#7348 = CARTESIAN_POINT ( 'NONE',  ( 1.574803149606299746, -0.1870078740157479769, 0.4822834645669291653 ) ) ;
#7349 = CARTESIAN_POINT ( 'NONE',  ( -1.548556430446193399, -0.6046776061558809534, -0.2411417322834644161 ) ) ;
#7350 = CARTESIAN_POINT ( 'NONE',  ( -0.3477690288713905509, -0.6692913385826771977, 0.1292274648535927661 ) ) ;
#7351 = CARTESIAN_POINT ( 'NONE',  ( 1.154855643044620184, 0.2306618581243847221, -0.2411417322834647770 ) ) ;
#7352 = ORIENTED_EDGE ( 'NONE', *, *, #40191, .F. ) ;
#7353 = CARTESIAN_POINT ( 'NONE',  ( -1.476377952755905110, -0.5400638737290845981, -0.3530559997133363437 ) ) ;
#7354 = CARTESIAN_POINT ( 'NONE',  ( -1.057085711732377087, 1.247373137590361836, -0.3766906164242062038 ) ) ;
#7355 = DIRECTION ( 'NONE',  ( -5.551115123125781470E-17, 1.000000000000000000, -1.938161486216356847E-31 ) ) ;
#7356 = CARTESIAN_POINT ( 'NONE',  ( 0.1938976377952755792, -0.1938976377952756069, -0.3740157480314971750 ) ) ;
#7357 = CARTESIAN_POINT ( 'NONE',  ( 3.937007874015748143, 1.724409448818897905, 0.4359958488159722534 ) ) ;
#7358 = CARTESIAN_POINT ( 'NONE',  ( -0.7742782152230962556, -0.3690944881889765550, -0.3153832671262227771 ) ) ;
#7359 = CARTESIAN_POINT ( 'NONE',  ( 0.4849061582275016602, 2.793565526369266028, 0.4921425059946345493 ) ) ;
#7360 = CARTESIAN_POINT ( 'NONE',  ( 0.4265091863517067594, 0.2952755905511811885, 0.1292274648535926551 ) ) ;
#7361 = VERTEX_POINT ( 'NONE', #20668 ) ;
#7363 = LINE ( 'NONE', #52374, #66737 ) ;
#7362 = DIRECTION ( 'NONE',  ( -0.000000000000000000, -1.000000000000000000, -0.000000000000000000 ) ) ;
#7364 = CARTESIAN_POINT ( 'NONE',  ( 1.417322834645670104, -0.1870078740157480879, -0.4822834645669291653 ) ) ;
#7365 = CARTESIAN_POINT ( 'NONE',  ( -1.496062992125983815, -0.1870078740157480879, -0.4822834645669291653 ) ) ;
#7366 = CARTESIAN_POINT ( 'NONE',  ( -0.3392501089628019439, 0.1958661417322832554, -0.8936814716197357678 ) ) ;
#7367 = CARTESIAN_POINT ( 'NONE',  ( -0.2296587926509179312, -0.2845877964562161244, -0.3641732283464567121 ) ) ;
#7368 = CARTESIAN_POINT ( 'NONE',  ( -1.614173228346455824, 0.1771653543307087630, 0.000000000000000000 ) ) ;
#7369 = CARTESIAN_POINT ( 'NONE',  ( -0.1049643490035301885, -0.3917322834645671215, -1.101706036745407014 ) ) ;
#7370 = CARTESIAN_POINT ( 'NONE',  ( -0.1070741851644056997, 0.3996062992125984925, -0.2408136482939632061 ) ) ;
#7371 = CARTESIAN_POINT ( 'NONE',  ( 0.2821522309711292364, -0.6692913385826771977, 0.1292274648535927661 ) ) ;
#7372 = CARTESIAN_POINT ( 'NONE',  ( -0.9383202099737524282, -0.2845877964562161244, -0.3641732283464567121 ) ) ;
#7373 = CARTESIAN_POINT ( 'NONE',  ( -0.01312335958005186876, -0.3690944881889763329, 0.3153832671262228327 ) ) ;
#7374 = ADVANCED_FACE ( 'NONE', ( #1728 ), #48504, .F. ) ;
#7375 = CARTESIAN_POINT ( 'NONE',  ( -0.01968503937007793844, -0.5400638737290844871, 0.3530559997133364547 ) ) ;
#7376 = CARTESIAN_POINT ( 'NONE',  ( -1.246719160104985846, -0.3690944881889765550, -0.3153832671262227771 ) ) ;
#7377 = CARTESIAN_POINT ( 'NONE',  ( 0.1049643490035303967, 0.3917322834645670659, -0.1476571110574297074 ) ) ;
#7378 = CARTESIAN_POINT ( 'NONE',  ( 0.7020997375328090762, -0.05778040916215560624, -0.4822834645669293319 ) ) ;
#7379 = EDGE_CURVE ( 'NONE', #70359, #76967, #40027, .T. ) ;
#7380 = CARTESIAN_POINT ( 'NONE',  ( -1.640419947506561060, 0.05413385826771666132, 0.4176697321401328100 ) ) ;
#7381 = CARTESIAN_POINT ( 'NONE',  ( 0.3458507752293908943, 0.3458507752293908943, -1.316929133858267598 ) ) ;
#7382 = CARTESIAN_POINT ( 'NONE',  ( -0.6824146981627291497, -0.6046776061558809534, -0.2411417322834644161 ) ) ;
#7383 = CARTESIAN_POINT ( 'NONE',  ( 0.3674540682414705883, 0.1283753931104746893, -0.1820866141732285504 ) ) ;
#7384 = CARTESIAN_POINT ( 'NONE',  ( -1.089238845144356427, -0.4281496062992127816, -0.4176697321401328100 ) ) ;
#7385 = CARTESIAN_POINT ( 'NONE',  ( 1.010498687664042716, -0.3690944881889763329, 0.3153832671262228327 ) ) ;
#7386 = AXIS2_PLACEMENT_3D ( 'NONE', #38077, #44373, #12011 ) ;
#7387 = CARTESIAN_POINT ( 'NONE',  ( -0.2296587926509179312, -0.2845877964562161244, -0.3641732283464567121 ) ) ;
#7388 = CARTESIAN_POINT ( 'NONE',  ( -0.5971128608923877978, 0.2952755905511811885, 0.1292274648535926551 ) ) ;
#7389 = CARTESIAN_POINT ( 'NONE',  ( -1.272965879265091305, -0.4281496062992124485, 0.4176697321401328655 ) ) ;
#7390 = CARTESIAN_POINT ( 'NONE',  ( -1.423884514435694859, -0.05778040916215560624, -0.4822834645669293319 ) ) ;
#7391 = CARTESIAN_POINT ( 'NONE',  ( -0.6912002287759484442, 1.909921116465415958, 0.5309055118110236338 ) ) ;
#7392 = CARTESIAN_POINT ( 'NONE',  ( 1.312335958005250269, -0.5023911411419708095, 0.1820866141732285504 ) ) ;
#7393 = CARTESIAN_POINT ( 'NONE',  ( 0.2887139107611556010, 0.2306618581243847221, -0.2411417322834647770 ) ) ;
#7394 = CARTESIAN_POINT ( 'NONE',  ( -1.640419947506561060, 0.05413385826771666132, 0.4176697321401328100 ) ) ;
#7395 = CARTESIAN_POINT ( 'NONE',  ( -1.633858267716534529, -0.5400638737290845981, -0.3530559997133363437 ) ) ;
#7396 = ORIENTED_EDGE ( 'NONE', *, *, #37360, .T. ) ;
#7397 = CARTESIAN_POINT ( 'NONE',  ( 0.2925321140481932369, 0.2925321140481932369, -2.576771653543307394 ) ) ;
#7398 = ADVANCED_FACE ( 'NONE', ( #7629 ), #13560, .T. ) ;
#7399 = CARTESIAN_POINT ( 'NONE',  ( -0.7480314960629914633, -0.5511811023622047445, 6.969142054262312111E-17 ) ) ;
#7400 = CARTESIAN_POINT ( 'NONE',  ( 0.8398950131233602345, 0.2306618581243847221, -0.2411417322834647770 ) ) ;
#7401 = CARTESIAN_POINT ( 'NONE',  ( -1.017060367454067249, -0.2845877964562161244, -0.3641732283464567121 ) ) ;
#7402 = CARTESIAN_POINT ( 'NONE',  ( 4.893765752498283308E-17, -0.3996062992125985480, -1.887795275590551158 ) ) ;
#7403 = CARTESIAN_POINT ( 'NONE',  ( -0.8136482939632537770, -0.6046776061558807314, 0.2411417322834647770 ) ) ;
#7404 = CARTESIAN_POINT ( 'NONE',  ( 0.9645669291338591078, -0.5400638737290845981, -0.3530559997133363437 ) ) ;
#7405 = CARTESIAN_POINT ( 'NONE',  ( 0.3215223097112867578, -0.3162353388693409650, -0.4822834645669289433 ) ) ;
#7406 = EDGE_CURVE ( 'NONE', #19993, #64046, #31183, .T. ) ;
#7407 = CARTESIAN_POINT ( 'NONE',  ( 1.089238845144357537, -0.4281496062992124485, 0.4176697321401328655 ) ) ;
#7408 = CARTESIAN_POINT ( 'NONE',  ( -1.410761154855642463, -0.08942795157527998196, 0.3641732283464567121 ) ) ;
#7409 = CARTESIAN_POINT ( 'NONE',  ( 0.2925321140481931814, -0.2925321140481931259, -1.120078740157480324 ) ) ;
#7410 = CARTESIAN_POINT ( 'NONE',  ( -0.3996062992125986035, -7.340648628747425578E-17, -1.299212598425196985 ) ) ;
#7411 = CARTESIAN_POINT ( 'NONE',  ( -0.3420746716998659953, -0.1974969037888706647, -0.5249343832020998413 ) ) ;
#7412 = CARTESIAN_POINT ( 'NONE',  ( 1.033875059083676717, 1.724409448818897905, 0.4359958488159722534 ) ) ;
#7413 = CARTESIAN_POINT ( 'NONE',  ( 0.7217847769028878924, -0.004921259842519576551, 0.3153832671262227771 ) ) ;
#7414 = CARTESIAN_POINT ( 'NONE',  ( 0.4199475065616803948, -0.5023911411419708095, -0.1820866141732282451 ) ) ;
#7415 = CARTESIAN_POINT ( 'NONE',  ( -0.07874015748031421014, -0.1870078740157480879, -0.4822834645669291653 ) ) ;
#7416 = CARTESIAN_POINT ( 'NONE',  ( 1.135170603674541256, 0.2952755905511811885, 0.1292274648535926551 ) ) ;
#7417 = CARTESIAN_POINT ( 'NONE',  ( -0.3420746716998662729, 0.1974969037888702206, -1.835301837270341130 ) ) ;
#7418 = CARTESIAN_POINT ( 'NONE',  ( 0.3674540682414705883, -0.5023911411419708095, 0.1820866141732285504 ) ) ;
#7419 = CARTESIAN_POINT ( 'NONE',  ( -0.9317585301837263412, -0.4281496062992127816, -0.4176697321401328100 ) ) ;
#7420 = CARTESIAN_POINT ( 'NONE',  ( 1.574803149606299746, -0.1870078740157479769, 0.4822834645669291653 ) ) ;
#7421 = CARTESIAN_POINT ( 'NONE',  ( 0.9711286089238851948, -0.6046776061558809534, -0.2411417322834644161 ) ) ;
#7422 = CARTESIAN_POINT ( 'NONE',  ( 0.3458507752293908943, -0.3458507752293908943, -1.988188976377952777 ) ) ;
#7423 = CARTESIAN_POINT ( 'NONE',  ( 1.169516495854323379, 0.02791078216816427274, -0.4328096321851894190 ) ) ;
#7424 = ORIENTED_EDGE ( 'NONE', *, *, #24704, .T. ) ;
#7425 = ORIENTED_EDGE ( 'NONE', *, *, #16767, .F. ) ;
#7426 = CARTESIAN_POINT ( 'NONE',  ( -1.154855643044618851, -0.6046776061558809534, -0.2411417322834644161 ) ) ;
#7427 = CARTESIAN_POINT ( 'NONE',  ( -1.187664041994749731, -0.3162353388693405765, 0.4822834645669290543 ) ) ;
#7429 = CARTESIAN_POINT ( 'NONE',  ( -0.6167979002624665030, -0.4281496062992127816, -0.4176697321401328100 ) ) ;
#7428 = CARTESIAN_POINT ( 'NONE',  ( -0.6233595800524928121, -0.2845877964562161244, -0.3641732283464567121 ) ) ;
#7430 = CARTESIAN_POINT ( 'NONE',  ( 0.3917322834645668994, 0.1049643490035304522, -2.409429503115799065 ) ) ;
#7431 = DIRECTION ( 'NONE',  ( 0.000000000000000000, 0.000000000000000000, -1.000000000000000000 ) ) ;
#7432 = CARTESIAN_POINT ( 'NONE',  ( 1.653543307086614789, -0.1870078740157479769, 0.4822834645669291653 ) ) ;
#7433 = CARTESIAN_POINT ( 'NONE',  ( -1.443569553805773564, -0.6046776061558807314, 0.2411417322834647770 ) ) ;
#7434 = CARTESIAN_POINT ( 'NONE',  ( 0.3740157480314966754, 0.1660481256975883668, -0.3530559997133364547 ) ) ;
#7435 = CARTESIAN_POINT ( 'NONE',  ( -1.062992125984250968, -0.6692913385826771977, 8.415575281601705876E-17 ) ) ;
#7436 = CARTESIAN_POINT ( 'NONE',  ( -0.1958661417322834220, -0.3392501089628018884, 0.1646981627296586759 ) ) ;
#7437 = CARTESIAN_POINT ( 'NONE',  ( 0.4855643044619428750, 0.05413385826771666132, 0.4176697321401328100 ) ) ;
#7438 = CARTESIAN_POINT ( 'NONE',  ( -9.594673741351313045E-17, 0.3917322834645670104, -2.039370078740157410 ) ) ;
#7439 = CARTESIAN_POINT ( 'NONE',  ( -0.8136482939632537770, 0.1283753931104746893, -0.1820866141732285504 ) ) ;
#7440 = ORIENTED_EDGE ( 'NONE', *, *, #45360, .F. ) ;
#7441 = CARTESIAN_POINT ( 'NONE',  ( 0.2891555358219910499, 0.2891555358219910499, -1.712598425196850682 ) ) ;
#7442 = ORIENTED_EDGE ( 'NONE', *, *, #73660, .T. ) ;
#7443 = CARTESIAN_POINT ( 'NONE',  ( 0.000000000000000000, 0.000000000000000000, -1.220472440944881942 ) ) ;
#7444 = VECTOR ( 'NONE', #36869, 39.37007874015748143 ) ;
#7445 = CARTESIAN_POINT ( 'NONE',  ( -1.122047244094487306, -0.5400638737290844871, 0.3530559997133364547 ) ) ;
#7446 = CARTESIAN_POINT ( 'NONE',  ( -1.417322834645668772, -0.1870078740157480879, -0.4822834645669291653 ) ) ;
#7447 = CARTESIAN_POINT ( 'NONE',  ( -0.2925321140481930704, -0.2925321140481933480, -0.6889763779527556808 ) ) ;
#7448 = CARTESIAN_POINT ( 'NONE',  ( -1.082677165354329896, 0.1660481256975885056, 0.3530559997133364547 ) ) ;
#7449 = CARTESIAN_POINT ( 'NONE',  ( -1.305774278215222184, -0.6692913385826773087, -0.1292274648535924053 ) ) ;
#7450 = CARTESIAN_POINT ( 'NONE',  ( -1.633858267716534529, 0.1660481256975885056, 0.3530559997133364547 ) ) ;
#7451 = CARTESIAN_POINT ( 'NONE',  ( 0.9329488473419933481, 3.212806586641111164E-18, -0.3627985898453516267 ) ) ;
#7452 = CARTESIAN_POINT ( 'NONE',  ( -0.8070866141732276899, 0.1660481256975883391, -0.3530559997133364547 ) ) ;
#7453 = CARTESIAN_POINT ( 'NONE',  ( 0.1771653543307093182, -0.4536011799217368745, -0.2665933059059886201 ) ) ;
#7454 = DIRECTION ( 'NONE',  ( 0.000000000000000000, 0.000000000000000000, -1.000000000000000000 ) ) ;
#7455 = CARTESIAN_POINT ( 'NONE',  ( 0.2867679344610365999, 0.2867679344610365999, -0.5374015748031496509 ) ) ;
#7456 = CARTESIAN_POINT ( 'NONE',  ( -0.4593175853018366950, -0.004921259842519576551, 0.3153832671262227771 ) ) ;
#7457 = CARTESIAN_POINT ( 'NONE',  ( -0.7152230971128602510, -0.3162353388693405765, 0.4822834645669290543 ) ) ;
#7458 = CARTESIAN_POINT ( 'NONE',  ( 1.122047244094488860, 0.1660481256975885056, 0.3530559997133364547 ) ) ;
#7459 = CARTESIAN_POINT ( 'NONE',  ( -0.5183727034120726440, 0.2952755905511811885, 0.1292274648535926551 ) ) ;
#7460 = ORIENTED_EDGE ( 'NONE', *, *, #27456, .F. ) ;
#7461 = EDGE_LOOP ( 'NONE', ( #52350, #72426, #9133 ) ) ;
#7462 = CARTESIAN_POINT ( 'NONE',  ( 0.3460692066303958092, 0.1998031496062993018, -2.097769028871391050 ) ) ;
#7463 = CARTESIAN_POINT ( 'NONE',  ( -0.8398950131233585692, 0.2306618581243848609, 0.2411417322834645549 ) ) ;
#7464 = CARTESIAN_POINT ( 'NONE',  ( 0.9514435695538062676, -0.05778040916215522460, 0.4822834645669289988 ) ) ;
#7465 = CARTESIAN_POINT ( 'NONE',  ( -1.601049868766403650, -0.5023911411419708095, 0.1820866141732285504 ) ) ;
#7466 = CARTESIAN_POINT ( 'NONE',  ( -1.633858267716534529, -0.5400638737290845981, -0.3530559997133363437 ) ) ;
#7467 = CARTESIAN_POINT ( 'NONE',  ( -0.4724409448818899238, 0.1265901696524986686, -1.135170603674540590 ) ) ;
#7468 = ADVANCED_FACE ( 'NONE', ( #14370 ), #65715, .F. ) ;
#7469 = DIRECTION ( 'NONE',  ( -0.000000000000000000, -1.000000000000000000, -0.000000000000000000 ) ) ;
#7470 = CARTESIAN_POINT ( 'NONE',  ( -0.1958661417322836718, 0.3392501089628017219, -0.4776902887139107268 ) ) ;
#7471 = CARTESIAN_POINT ( 'NONE',  ( 1.403614904275686858E-14, 1.537401574803149984, -3.937007874015761910 ) ) ;
#7472 = CARTESIAN_POINT ( 'NONE',  ( -0.2034120734908128059, 0.2952755905511811885, 0.1292274648535926551 ) ) ;
#7473 = CARTESIAN_POINT ( 'NONE',  ( -1.646981627296586703, -0.08942795157527998196, 0.3641732283464567121 ) ) ;
#7474 = CARTESIAN_POINT ( 'NONE',  ( -0.7283464566929126471, 0.1660481256975883668, -0.3530559997133364547 ) ) ;
#7475 = CARTESIAN_POINT ( 'NONE',  ( -0.3996062992125985480, -7.340648628747423112E-17, -0.2736220472440945017 ) ) ;
#7477 = CARTESIAN_POINT ( 'NONE',  ( 0.1265901696524990572, -0.4724409448818897017, -1.106955380577427706 ) ) ;
#7476 = CARTESIAN_POINT ( 'NONE',  ( -1.089238845144356427, 0.05413385826771666132, 0.4176697321401328100 ) ) ;
#7478 = B_SPLINE_CURVE_WITH_KNOTS ( 'NONE', 3,
 ( #51804, #20261, #56878, #50559, #12285, #32882, #82983, #58551, #25303, #26574, #50968, #68539, #30644, #68948, #62216, #75688, #29403, #29810 ),
 .UNSPECIFIED., .F., .F.,
 ( 4, 2, 2, 2, 2, 2, 2, 2, 4 ),
 ( 2.786138856325813435E-16, 0.001588476978679812012, 0.002382715468019578481, 0.002779834712689461824, 0.002978394335024402845, 0.003077674146191874006, 0.003127314051775609369, 0.003152134004567477051, 0.003176953957359344299 ),
 .UNSPECIFIED. ) ;
#7479 = CARTESIAN_POINT ( 'NONE',  ( -1.135170603674539924, -0.6692913385826771977, 0.1292274648535927661 ) ) ;
#7480 = CARTESIAN_POINT ( 'NONE',  ( -0.5249343832020990641, -0.6046776061558809534, -0.2411417322834644161 ) ) ;
#7481 = CARTESIAN_POINT ( 'NONE',  ( 0.1974969037888704704, 0.3420746716998660508, -2.583333333333333481 ) ) ;
#7482 = CARTESIAN_POINT ( 'NONE',  ( 0.9055118110236227702, -0.5511811023622047445, 6.969142054262312111E-17 ) ) ;
#7483 = CYLINDRICAL_SURFACE ( 'NONE', #73407, 0.4724409448818898682 ) ;
#7484 = CARTESIAN_POINT ( 'NONE',  ( 0.5577427821522316087, -0.08942795157527998196, 0.3641732283464567121 ) ) ;
#7485 = CARTESIAN_POINT ( 'NONE',  ( 1.338582677165355062, -0.1870078740157480601, -0.3641732283464567677 ) ) ;
#7486 = CARTESIAN_POINT ( 'NONE',  ( 1.174540682414699111, -0.05778040916215560624, -0.4822834645669293319 ) ) ;
#7487 = PRODUCT_DEFINITION_CONTEXT ( 'detailed design', #15402, 'design' ) ;
#7488 = CARTESIAN_POINT ( 'NONE',  ( 0.03280839895013198948, -0.5511811023622048555, -0.09757992244046775898 ) ) ;
#7489 = CARTESIAN_POINT ( 'NONE',  ( -0.3392501089628019995, 0.1958661417322832277, -1.908136482939632561 ) ) ;
#7490 = CARTESIAN_POINT ( 'NONE',  ( -1.397637795275589623, -0.5400638737290845981, -0.3530559997133363437 ) ) ;
#7491 = CARTESIAN_POINT ( 'NONE',  ( 1.404199475065617264, -0.4281496062992124485, 0.4176697321401328655 ) ) ;
#7492 = EDGE_CURVE ( 'NONE', #21709, #29467, #60600, .T. ) ;
#7493 = CARTESIAN_POINT ( 'NONE',  ( -0.3458507752293906723, -0.3458507752293910609, 0.1791338582677165503 ) ) ;
#7494 = CARTESIAN_POINT ( 'NONE',  ( -0.4658792650918627265, -0.2845877964562161244, -0.3641732283464567121 ) ) ;
#7495 = CARTESIAN_POINT ( 'NONE',  ( 1.348312163386739426, 1.062992125984252079, 0.7386866130305692613 ) ) ;
#7496 = CARTESIAN_POINT ( 'NONE',  ( 0.2362204724409456558, -0.1870078740157479769, 0.4822834645669291653 ) ) ;
#7497 = CARTESIAN_POINT ( 'NONE',  ( -0.6423408027444563739, -2.609869883881465018E-15, -0.3464511005275220379 ) ) ;
#7498 = CARTESIAN_POINT ( 'NONE',  ( 0.8005249343832027131, -0.004921259842519576551, 0.3153832671262227771 ) ) ;
#7499 = CARTESIAN_POINT ( 'NONE',  ( 0.1181102362204730916, -0.5511811023622047445, 6.969142054262312111E-17 ) ) ;
#7500 = CARTESIAN_POINT ( 'NONE',  ( -0.4658792650918627265, -0.3162353388693409650, -0.4822834645669289433 ) ) ;
#7501 = CARTESIAN_POINT ( 'NONE',  ( -1.213910761154854745, 0.2952755905511810774, -0.1292274648535930714 ) ) ;
#7502 = CARTESIAN_POINT ( 'NONE',  ( -0.6299212598425188991, -0.1870078740157480601, -0.3641732283464567677 ) ) ;
#7503 = DIRECTION ( 'NONE',  ( 0.000000000000000000, -0.000000000000000000, 1.000000000000000000 ) ) ;
#7504 = CARTESIAN_POINT ( 'NONE',  ( 0.4593175853018380828, 0.05413385826771626580, -0.4176697321401330321 ) ) ;
#7505 = CARTESIAN_POINT ( 'NONE',  ( -0.8530183727034112984, 0.05413385826771666132, 0.4176697321401328100 ) ) ;
#7506 = CARTESIAN_POINT ( 'NONE',  ( 0.3996062992125985480, 2.446882876249141654E-17, -1.297244094488188670 ) ) ;
#7507 = CARTESIAN_POINT ( 'NONE',  ( 0.3917322834645670104, -0.1049643490035303411, -2.873359580052493811 ) ) ;
#7508 = CARTESIAN_POINT ( 'NONE',  ( 0.1181102362204730916, -0.5511811023622047445, 6.969142054262312111E-17 ) ) ;
#7509 = CARTESIAN_POINT ( 'NONE',  ( -0.7808398950131222316, -0.3162353388693409650, -0.4822834645669289433 ) ) ;
#7510 = VECTOR ( 'NONE', #60353, 39.37007874015748143 ) ;
#7511 = CARTESIAN_POINT ( 'NONE',  ( -0.9842519685039360366, 0.2952755905511811885, 0.000000000000000000 ) ) ;
#7512 = CARTESIAN_POINT ( 'NONE',  ( -1.246719160104985846, -0.3690944881889765550, -0.3153832671262227771 ) ) ;
#7513 = CARTESIAN_POINT ( 'NONE',  ( 1.587926509186352586, -0.4281496062992127816, -0.4176697321401328100 ) ) ;
#7514 = CARTESIAN_POINT ( 'NONE',  ( -0.9055118110236215490, -0.5511811023622047445, 6.969142054262312111E-17 ) ) ;
#7515 = CARTESIAN_POINT ( 'NONE',  ( -2.170146923806554273, 1.537401574803149984, -0.4744094488188975722 ) ) ;
#7516 = CARTESIAN_POINT ( 'NONE',  ( 1.496062992125984703, -0.1870078740157480879, -0.4822834645669291653 ) ) ;
#7517 = CARTESIAN_POINT ( 'NONE',  ( -0.3460692066303958092, -0.1998031496062994683, 0.1049868766404199322 ) ) ;
#7518 = CARTESIAN_POINT ( 'NONE',  ( -9.594673741351313045E-17, 0.3917322834645670659, -2.516423515256904331 ) ) ;
#7519 = VERTEX_POINT ( 'NONE', #4201 ) ;
#7520 = CARTESIAN_POINT ( 'NONE',  ( 0.02899565511876438934, -0.3969271875946648320, -3.856971560569901962E-17 ) ) ;
#7521 = CARTESIAN_POINT ( 'NONE',  ( -1.653543307086613234, -0.1870078740157480879, -0.4822834645669291653 ) ) ;
#7522 = CARTESIAN_POINT ( 'NONE',  ( -1.266404199475064773, -0.3162353388693405765, 0.4822834645669290543 ) ) ;
#7523 = CARTESIAN_POINT ( 'NONE',  ( 1.108923884514436242, -0.05778040916215522460, 0.4822834645669289988 ) ) ;
#7524 = CARTESIAN_POINT ( 'NONE',  ( -0.3392501089628017219, -0.1958661417322836718, -2.341863517060367439 ) ) ;
#7525 = CARTESIAN_POINT ( 'NONE',  ( 0.6299212598425100174, 0.000000000000000000, 0.9285414500055778619 ) ) ;
#7526 = CARTESIAN_POINT ( 'NONE',  ( 0.4724409448818904789, -0.1870078740157480879, -0.4822834645669291653 ) ) ;
#7527 = CARTESIAN_POINT ( 'NONE',  ( -0.1181102362204717315, -0.6692913385826771977, 8.415575281601705876E-17 ) ) ;
#7528 = CARTESIAN_POINT ( 'NONE',  ( 0.4262761708485561241, 1.326877055403132388, -3.913880873785005488 ) ) ;
#7529 = CYLINDRICAL_SURFACE ( 'NONE', #4899, 0.4744094488188972947 ) ;
#7530 = CARTESIAN_POINT ( 'NONE',  ( 0.7152230971128614723, -0.2845877964562161244, -0.3641732283464567121 ) ) ;
#7531 = EDGE_CURVE ( 'NONE', #82661, #79084, #3796, .T. ) ;
#7532 = CARTESIAN_POINT ( 'NONE',  ( -0.3996062992125987146, 0.1070741851644051862, -1.450131233595800317 ) ) ;
#7533 = ORIENTED_EDGE ( 'NONE', *, *, #41165, .F. ) ;
#7534 = CARTESIAN_POINT ( 'NONE',  ( 0.3917322834645670659, 2.398668435337828261E-17, -0.1148487121072984812 ) ) ;
#7535 = ORIENTED_EDGE ( 'NONE', *, *, #66936, .T. ) ;
#7536 = CARTESIAN_POINT ( 'NONE',  ( 0.08530183727034192087, -0.3162353388693409650, -0.4822834645669289433 ) ) ;
#7537 = CARTESIAN_POINT ( 'NONE',  ( 1.391076115485564868, -0.6046776061558807314, 0.2411417322834647770 ) ) ;
#7538 = CARTESIAN_POINT ( 'NONE',  ( 0.8005249343832028242, -0.4281496062992127816, -0.4176697321401328100 ) ) ;
#7539 = CARTESIAN_POINT ( 'NONE',  ( 1.141732283464567788, -0.6692913385826771977, 8.415575281601705876E-17 ) ) ;
#7540 = EDGE_CURVE ( 'NONE', #3606, #39084, #61449, .T. ) ;
#7541 = CARTESIAN_POINT ( 'NONE',  ( -0.3674540682414689785, 0.2306618581243848609, 0.2411417322834645549 ) ) ;
#7542 = CARTESIAN_POINT ( 'NONE',  ( -0.09842519685039295696, 0.1660481256975883668, -0.3530559997133364547 ) ) ;
#7543 = CARTESIAN_POINT ( 'NONE',  ( 1.601049868766404982, 0.2306618581243848609, 0.2411417322834645549 ) ) ;
#7544 = CARTESIAN_POINT ( 'NONE',  ( 1.305774278215223960, 0.2952755905511810774, -0.1292274648535930714 ) ) ;
#7545 = CARTESIAN_POINT ( 'NONE',  ( 1.233595800524935227, 0.2306618581243847221, -0.2411417322834647770 ) ) ;
#7546 = CARTESIAN_POINT ( 'NONE',  ( 0.3392501089628018884, -0.1958661417322834220, -0.09711286089238840846 ) ) ;
#7547 = CARTESIAN_POINT ( 'NONE',  ( 0.4790026246719168435, -0.2845877964562161244, -0.3641732283464567121 ) ) ;
#7548 = ORIENTED_EDGE ( 'NONE', *, *, #29541, .T. ) ;
#7549 = CARTESIAN_POINT ( 'NONE',  ( 0.1974969037888704704, 0.3420746716998660508, -0.7742782152230970327 ) ) ;
#7550 = AXIS2_PLACEMENT_3D ( 'NONE', #1994, #7901, #34816 ) ;
#7551 = EDGE_LOOP ( 'NONE', ( #79618, #48716, #45301, #46126 ) ) ;
#7552 = CARTESIAN_POINT ( 'NONE',  ( -0.3149606299212590610, -0.1870078740157479769, 0.3641732283464567677 ) ) ;
#7553 = VECTOR ( 'NONE', #36566, 39.37007874015748143 ) ;
#7554 = CARTESIAN_POINT ( 'NONE',  ( -0.1771653543307080136, 0.1660481256975883668, -0.3530559997133364547 ) ) ;
#7555 = CARTESIAN_POINT ( 'NONE',  ( 2.822823420596364929, 1.118719813955008524, 0.2236424093447139938 ) ) ;
#7556 = CARTESIAN_POINT ( 'NONE',  ( 0.2952755905511816326, -0.5400638737290844871, 0.3530559997133364547 ) ) ;
#7557 = CARTESIAN_POINT ( 'NONE',  ( 0.06561679790026316017, 0.05413385826771626580, -0.4176697321401330321 ) ) ;
#7558 = CARTESIAN_POINT ( 'NONE',  ( -0.6692913385826764205, 0.2952755905511811885, 0.000000000000000000 ) ) ;
#7559 = CARTESIAN_POINT ( 'NONE',  ( -1.141732283464566011, -0.6692913385826771977, 8.415575281601705876E-17 ) ) ;
#7560 = CARTESIAN_POINT ( 'NONE',  ( 1.345144356955381593, -0.08942795157527998196, 0.3641732283464567121 ) ) ;
#7561 = CARTESIAN_POINT ( 'NONE',  ( 1.586052503253845503, 0.4724409448818907564, 0.1653254495020587411 ) ) ;
#7562 = CARTESIAN_POINT ( 'NONE',  ( 0.4359958488159797474, 1.724409448818897905, -2.094141031014984833 ) ) ;
#7563 = CARTESIAN_POINT ( 'NONE',  ( 0.9448818897637802916, -0.1870078740157479769, 0.3641732283464567677 ) ) ;
#7564 = CARTESIAN_POINT ( 'NONE',  ( 0.4002624671916016896, -0.05778040916215522460, 0.4822834645669289988 ) ) ;
#7565 = CARTESIAN_POINT ( 'NONE',  ( 0.6692913385826778638, -0.6692913385826771977, 8.415575281601705876E-17 ) ) ;
#7566 = CARTESIAN_POINT ( 'NONE',  ( -0.2925321140481930704, -0.2925321140481933480, -1.476377952755905554 ) ) ;
#7567 = DIRECTION ( 'NONE',  ( -0.000000000000000000, -1.000000000000000000, -0.000000000000000000 ) ) ;
#7568 = CARTESIAN_POINT ( 'NONE',  ( 0.1998031496062992463, 0.3460692066303959202, -0.5360892388451443669 ) ) ;
#7569 = CARTESIAN_POINT ( 'NONE',  ( 0.2925321140481932369, 0.2925321140481932369, -0.05708661417322837689 ) ) ;
#7570 = CARTESIAN_POINT ( 'NONE',  ( -0.4724409448818890911, -0.1870078740157479769, 0.4822834645669291653 ) ) ;
#7571 = CARTESIAN_POINT ( 'NONE',  ( -0.2925321140481932924, 0.2925321140481931814, -2.696850393700787052 ) ) ;
#7572 = CARTESIAN_POINT ( 'NONE',  ( 0.1049643490035303689, 0.3917322834645670104, -2.282808398950130879 ) ) ;
#7573 = CARTESIAN_POINT ( 'NONE',  ( -1.030183727034119867, -0.2845877964562159024, 0.3641732283464567677 ) ) ;
#7574 = CARTESIAN_POINT ( 'NONE',  ( 1.272965879265092637, 0.05413385826771666132, 0.4176697321401328100 ) ) ;
#7575 = VECTOR ( 'NONE', #5793, 39.37007874015748143 ) ;
#7576 = CARTESIAN_POINT ( 'NONE',  ( 0.8661417322834653598, -0.1870078740157479769, 0.4822834645669291653 ) ) ;
#7577 = CARTESIAN_POINT ( 'NONE',  ( -0.2362204724409440182, -0.1870078740157479769, 0.3641732283464567677 ) ) ;
#7578 = CARTESIAN_POINT ( 'NONE',  ( 0.4002624671916016896, -0.3162353388693409650, -0.4822834645669289433 ) ) ;
#7579 = CARTESIAN_POINT ( 'NONE',  ( -0.3458507752293909498, 0.3458507752293907833, -1.671259842519685179 ) ) ;
#7580 = CARTESIAN_POINT ( 'NONE',  ( 0.2493438320209980519, -0.004921259842519576551, 0.3153832671262227771 ) ) ;
#7581 = CARTESIAN_POINT ( 'NONE',  ( 0.1246719160104994284, -0.6692913385826771977, 0.1292274648535927661 ) ) ;
#7582 = CARTESIAN_POINT ( 'NONE',  ( -0.3949938075777411073, 0.1058382717557497660, -1.526902887139107934 ) ) ;
#7583 = CARTESIAN_POINT ( 'NONE',  ( -1.115485564304461219, -0.4281496062992124485, 0.4176697321401328655 ) ) ;
#7584 = CARTESIAN_POINT ( 'NONE',  ( 0.3477690288713918276, 0.1771653543307087630, 0.09757992244046791164 ) ) ;
#7585 = CARTESIAN_POINT ( 'NONE',  ( -1.169516495854322269, 0.02791078216816064370, 0.4328096321851915285 ) ) ;
#7586 = CARTESIAN_POINT ( 'NONE',  ( -0.8792650918635160906, 0.05413385826771626580, -0.4176697321401330321 ) ) ;
#7587 = CARTESIAN_POINT ( 'NONE',  ( -0.4658792650918627265, -0.2845877964562161244, -0.3641732283464567121 ) ) ;
#7588 = CARTESIAN_POINT ( 'NONE',  ( -1.473278426072734293, 0.2335363939278408130, 0.2780995266831702284 ) ) ;
#7589 = CARTESIAN_POINT ( 'NONE',  ( -0.8136482939632537770, -0.6046776061558807314, 0.2411417322834647770 ) ) ;
#7590 = CARTESIAN_POINT ( 'NONE',  ( -0.7545931758530176614, -0.6692913385826773087, -0.1292274648535924053 ) ) ;
#7591 = CARTESIAN_POINT ( 'NONE',  ( 0.4855643044619428750, -0.004921259842519576551, 0.3153832671262227771 ) ) ;
#7592 = CARTESIAN_POINT ( 'NONE',  ( -0.3460692066303957537, -0.1998031496062994405, -2.333989501312335957 ) ) ;
#7593 = CARTESIAN_POINT ( 'NONE',  ( -0.05249343832020911260, 0.2306618581243848609, 0.2411417322834645549 ) ) ;
#7594 = CARTESIAN_POINT ( 'NONE',  ( 0.3392501089628018329, 0.1958661417322835052, -2.258510867945195066 ) ) ;
#7595 = CARTESIAN_POINT ( 'NONE',  ( -1.607611548556429737, -0.5511811023622046335, 0.09757992244046803654 ) ) ;
#7596 = CARTESIAN_POINT ( 'NONE',  ( 0.8136482939632553313, -0.5023911411419708095, -0.1820866141732282451 ) ) ;
#7597 = CARTESIAN_POINT ( 'NONE',  ( 1.587926509186352142, 0.05413385826771666132, 0.4176697321401328100 ) ) ;
#7598 = CARTESIAN_POINT ( 'NONE',  ( -0.8727034120734901146, -0.08942795157528024563, -0.3641732283464568787 ) ) ;
#7599 = CARTESIAN_POINT ( 'NONE',  ( -0.9776902887139098386, -0.5511811023622046335, 0.09757992244046803654 ) ) ;
#7600 = CARTESIAN_POINT ( 'NONE',  ( -0.6430446194225712953, 0.05413385826771626580, -0.4176697321401330321 ) ) ;
#7601 = CARTESIAN_POINT ( 'NONE',  ( -0.03280839895013062252, -0.6692913385826771977, 0.1292274648535927661 ) ) ;
#7602 = CARTESIAN_POINT ( 'NONE',  ( 0.4986876640419954376, -0.5023911411419708095, -0.1820866141732282451 ) ) ;
#7603 = CARTESIAN_POINT ( 'NONE',  ( -0.2445414048442310917, 0.1655124888405462291, 5.638514421976805302 ) ) ;
#7604 = CARTESIAN_POINT ( 'NONE',  ( 0.8727034120734912248, -0.2845877964562161244, -0.3641732283464567121 ) ) ;
#7605 = CARTESIAN_POINT ( 'NONE',  ( 0.3346456692913393205, -0.5400638737290845981, -0.3530559997133363437 ) ) ;
#7606 = FACE_OUTER_BOUND ( 'NONE', #4750, .T. ) ;
#7607 = CARTESIAN_POINT ( 'NONE',  ( -0.7611548556430438595, 0.2306618581243848609, 0.2411417322834645549 ) ) ;
#7608 = CONICAL_SURFACE ( 'NONE', #58717, 1.968503937007874072, 0.7853981633974500554 ) ;
#7609 = CARTESIAN_POINT ( 'NONE',  ( 0.1049643490035303689, 0.3917322834645670104, -1.495406824146981117 ) ) ;
#7610 = CARTESIAN_POINT ( 'NONE',  ( 1.437007874015748810, 0.07958543189024085140, 0.2665933059059887866 ) ) ;
#7612 = CARTESIAN_POINT ( 'NONE',  ( 0.5577427821522316087, -0.05778040916215522460, 0.4822834645669289988 ) ) ;
#7611 = AXIS2_PLACEMENT_3D ( 'NONE', #53753, #2017, #16316 ) ;
#7613 = CIRCLE ( 'NONE', #61371, 0.5118110236220471121 ) ;
#7614 = CARTESIAN_POINT ( 'NONE',  ( 0.1049868766404206816, 0.2306618581243848609, 0.2411417322834645549 ) ) ;
#7615 = CARTESIAN_POINT ( 'NONE',  ( 1.141392835773559211, 0.3937007874015747699, 1.141392835773562764 ) ) ;
#7616 = CARTESIAN_POINT ( 'NONE',  ( -0.1509186351706028884, -0.2845877964562161244, -0.3641732283464567121 ) ) ;
#7617 = CARTESIAN_POINT ( 'NONE',  ( 0.7283464566929143125, 0.1660481256975885056, 0.3530559997133364547 ) ) ;
#7618 = CARTESIAN_POINT ( 'NONE',  ( -0.7152230971128602510, -0.08942795157528024563, -0.3641732283464568787 ) ) ;
#7619 = CARTESIAN_POINT ( 'NONE',  ( -0.6889763779527552368, 0.1660481256975885056, 0.3530559997133364547 ) ) ;
#7620 = CARTESIAN_POINT ( 'NONE',  ( 1.854472803289052507, 2.716535433070866645, 0.5314960629921260393 ) ) ;
#7621 = CARTESIAN_POINT ( 'NONE',  ( -0.1115485564304456306, 0.2952755905511810774, -0.1292274648535930714 ) ) ;
#7622 = ORIENTED_EDGE ( 'NONE', *, *, #18824, .T. ) ;
#7623 = CARTESIAN_POINT ( 'NONE',  ( -1.266404199475064773, -0.05778040916215560624, -0.4822834645669293319 ) ) ;
#7624 = CARTESIAN_POINT ( 'NONE',  ( -1.220472440944881054, 0.1771653543307087630, 0.000000000000000000 ) ) ;
#7625 = CARTESIAN_POINT ( 'NONE',  ( -0.1312335958005241554, 0.2306618581243848609, 0.2411417322834645549 ) ) ;
#7626 = CARTESIAN_POINT ( 'NONE',  ( 0.3985446848723406266, 0.001150535885505707878, -1.220472440944882386 ) ) ;
#7627 = CARTESIAN_POINT ( 'NONE',  ( -0.8464566929133852113, 0.1660481256975885056, 0.3530559997133364547 ) ) ;
#7628 =( BOUNDED_CURVE ( )  B_SPLINE_CURVE ( 2, ( #67773, #30271, #30692, #23958, #82054, #50037, #75734, #48804, #43297, #42484, #18074, #10928, #68587 ),
 .UNSPECIFIED., .F., .F. ) 
 B_SPLINE_CURVE_WITH_KNOTS ( ( 3, 2, 2, 2, 2, 2, 3 ),
 ( 0.7374999999999999334, 0.7416666666666665853, 0.7458333333333333481, 0.7500000000000000000, 0.7541666666666666519, 0.7583333333333334147, 0.7625000000000000666 ),
 .UNSPECIFIED. ) 
 CURVE ( )  GEOMETRIC_REPRESENTATION_ITEM ( )  RATIONAL_B_SPLINE_CURVE ( ( 1.000000000000000888, 0.9659258262890674240, 1.000000000000000000, 0.9659258262890683122, 1.000000000000000000, 0.9659258262890683122, 1.000000000000000000, 0.9659258262890683122, 1.000000000000000000, 0.9659258262890683122, 1.000000000000000000, 0.9659258262890674240, 1.000000000000000888 ) ) 
 REPRESENTATION_ITEM ( '' )  );
#7629 = FACE_OUTER_BOUND ( 'NONE', #1451, .T. ) ;
#7631 = CARTESIAN_POINT ( 'NONE',  ( 1.122047244094488860, 0.1660481256975885056, 0.3530559997133364547 ) ) ;
#7630 = CARTESIAN_POINT ( 'NONE',  ( -0.9120734908136473029, 0.2952755905511811885, 0.1292274648535926551 ) ) ;
#7632 = CARTESIAN_POINT ( 'NONE',  ( 1.417322834645670104, -0.1870078740157480879, -0.4822834645669291653 ) ) ;
#7633 = CARTESIAN_POINT ( 'NONE',  ( 0.1049643490035304799, -0.3917322834645669549, -2.597112860892388131 ) ) ;
#7634 = FACE_OUTER_BOUND ( 'NONE', #38153, .T. ) ;
#7635 = CARTESIAN_POINT ( 'NONE',  ( -1.141732283464566011, -0.6692913385826771977, 8.415575281601705876E-17 ) ) ;
#7636 = CARTESIAN_POINT ( 'NONE',  ( -0.4724409448818895907, -0.1265901696524993070, -0.6758530183727035068 ) ) ;
#7637 = EDGE_CURVE ( 'NONE', #65743, #23063, #1, .T. ) ;
#7638 = CARTESIAN_POINT ( 'NONE',  ( 0.3460692066303959757, -0.1998031496062991907, 0.05249343832020995915 ) ) ;
#7639 = ORIENTED_EDGE ( 'NONE', *, *, #55316, .T. ) ;
#7640 = CARTESIAN_POINT ( 'NONE',  ( -0.07217847769028787330, -0.08942795157527998196, 0.3641732283464567121 ) ) ;
#7641 = CARTESIAN_POINT ( 'NONE',  ( -0.1049643490035302024, -0.3917322834645671215, -1.639107611548556109 ) ) ;
#7642 = ORIENTED_EDGE ( 'NONE', *, *, #21253, .F. ) ;
#7643 = CARTESIAN_POINT ( 'NONE',  ( 0.07217847769028949700, -0.05778040916215560624, -0.4822834645669293319 ) ) ;
#7644 = CARTESIAN_POINT ( 'NONE',  ( 0.1049868766404206816, -0.6046776061558809534, -0.2411417322834644161 ) ) ;
#7645 = CARTESIAN_POINT ( 'NONE',  ( -0.5118110236220466680, 0.2952755905511811885, 0.000000000000000000 ) ) ;
#7646 = FACE_OUTER_BOUND ( 'NONE', #41699, .T. ) ;
#7647 = CARTESIAN_POINT ( 'NONE',  ( -0.8595800524934373854, -0.08942795157527998196, 0.3641732283464567121 ) ) ;
#7648 = DIRECTION ( 'NONE',  ( 0.000000000000000000, 0.000000000000000000, -1.000000000000000000 ) ) ;
#7649 = CARTESIAN_POINT ( 'NONE',  ( 0.7874015748031503170, -0.1870078740157480879, -0.4822834645669291653 ) ) ;
#7650 = CARTESIAN_POINT ( 'NONE',  ( 0.6496062992125991586, 0.07958543189024085140, 0.2665933059059887866 ) ) ;
#7651 = CARTESIAN_POINT ( 'NONE',  ( -0.2887139107611542133, -0.6046776061558809534, -0.2411417322834644161 ) ) ;
#7652 = CARTESIAN_POINT ( 'NONE',  ( 0.1958661417322836162, -0.3392501089628018329, -1.274258899441258031 ) ) ;
#7653 = CARTESIAN_POINT ( 'NONE',  ( -0.8792650918635160906, -0.4281496062992124485, 0.4176697321401328655 ) ) ;
#7654 = CARTESIAN_POINT ( 'NONE',  ( -1.541994750656167090, 0.1771653543307087630, 0.09757992244046791164 ) ) ;
#7655 = CARTESIAN_POINT ( 'NONE',  ( 1.351706036745407680, 0.05413385826771666132, 0.4176697321401328100 ) ) ;
#7656 = DIRECTION ( 'NONE',  ( 0.000000000000000000, 0.000000000000000000, -1.000000000000000000 ) ) ;
#7657 = EDGE_LOOP ( 'NONE', ( #44643, #65213, #39862, #19626 ) ) ;
#7658 = CARTESIAN_POINT ( 'NONE',  ( -0.2867679344610365444, -0.2867679344610367664, -2.417998318406511249 ) ) ;
#7659 = CARTESIAN_POINT ( 'NONE',  ( 0.08530183727034192087, -0.05778040916215522460, 0.4822834645669289988 ) ) ;
#7660 = ORIENTED_EDGE ( 'NONE', *, *, #71659, .F. ) ;
#7661 = CARTESIAN_POINT ( 'NONE',  ( -0.7742782152230965886, 0.05413385826771666132, 0.4176697321401328100 ) ) ;
#7662 = CARTESIAN_POINT ( 'NONE',  ( 1.568241469816273437, -0.3162353388693405765, 0.4822834645669290543 ) ) ;
#7663 = CARTESIAN_POINT ( 'NONE',  ( 1.345144356955381593, -0.3162353388693409650, -0.4822834645669289433 ) ) ;
#7664 = CARTESIAN_POINT ( 'NONE',  ( 0.2690288713910767848, -0.6692913385826773087, -0.1292274648535924053 ) ) ;
#7665 = CARTESIAN_POINT ( 'NONE',  ( -0.2099737532808391705, 0.2306618581243848609, 0.2411417322834645549 ) ) ;
#7666 = CARTESIAN_POINT ( 'NONE',  ( 0.1958661417322834775, 0.3392501089628018884, -1.961286089238845287 ) ) ;
#7667 = CARTESIAN_POINT ( 'NONE',  ( -1.102362204724408601, -0.1870078740157479769, 0.4822834645669291653 ) ) ;
#7668 = CARTESIAN_POINT ( 'NONE',  ( -0.2296587926509179312, -0.05778040916215522460, 0.4822834645669289988 ) ) ;
#7669 = CARTESIAN_POINT ( 'NONE',  ( -0.05249343832020911260, 0.1283753931104748280, 0.1820866141732283561 ) ) ;
#7670 = DIRECTION ( 'NONE',  ( -0.000000000000000000, -1.000000000000000000, 0.000000000000000000 ) ) ;
#7671 = CARTESIAN_POINT ( 'NONE',  ( -0.3543307086614165824, -0.6692913385826771977, 8.415575281601705876E-17 ) ) ;
#7672 = CARTESIAN_POINT ( 'NONE',  ( 1.148293963254593653, 0.2952755905511810774, -0.1292274648535930714 ) ) ;
#7673 = DIRECTION ( 'NONE',  ( -1.000000000000000000, -3.083952846180990774E-16, 0.000000000000000000 ) ) ;
#7674 = ORIENTED_EDGE ( 'NONE', *, *, #34817, .T. ) ;
#7675 = VECTOR ( 'NONE', #22908, 39.37007874015748143 ) ;
#7676 = CARTESIAN_POINT ( 'NONE',  ( -0.07217847769028787330, -0.05778040916215522460, 0.4822834645669289988 ) ) ;
#7677 = CARTESIAN_POINT ( 'NONE',  ( -0.09186351706036689768, -0.004921259842519870586, -0.3153832671262229437 ) ) ;
#7678 = AXIS2_PLACEMENT_3D ( 'NONE', #81376, #29594, #35088 ) ;
#7679 = CIRCLE ( 'NONE', #68116, 3.543307086614173596 ) ;
#7681 = CARTESIAN_POINT ( 'NONE',  ( -1.436417322834643739, 0.8346805926620878280, -0.3149606299212598381 ) ) ;
#7680 = CARTESIAN_POINT ( 'NONE',  ( 0.9973753280839902091, -0.5023911411419708095, 0.1820866141732285504 ) ) ;
#7682 = CARTESIAN_POINT ( 'NONE',  ( -0.4091458600556402980, -0.2362204724409451284, -0.4442257217847768724 ) ) ;
#7683 = CARTESIAN_POINT ( 'NONE',  ( 2.142213561789876319, 0.02617651024168224372, -0.4623158380715471361 ) ) ;
#7684 = CARTESIAN_POINT ( 'NONE',  ( 1.174540682414699111, -0.05778040916215560624, -0.4822834645669293319 ) ) ;
#7685 = CARTESIAN_POINT ( 'NONE',  ( -0.1974969037888704149, -0.3420746716998661063, -0.1423884514435695414 ) ) ;
#7686 = PRODUCT_DEFINITION_SHAPE ( 'NONE', 'NONE',  #83311 ) ;
#7687 = CARTESIAN_POINT ( 'NONE',  ( -0.05905511811023545637, -0.5400638737290845981, -0.3530559997133363437 ) ) ;
#7688 = DIRECTION ( 'NONE',  ( -0.000000000000000000, -1.000000000000000000, -0.000000000000000000 ) ) ;
#7689 = CARTESIAN_POINT ( 'NONE',  ( -1.423884514435694859, -0.3162353388693405765, 0.4822834645669290543 ) ) ;
#7690 = CARTESIAN_POINT ( 'NONE',  ( -0.1509186351706028884, -0.05778040916215522460, 0.4822834645669289988 ) ) ;
#7691 = CARTESIAN_POINT ( 'NONE',  ( 0.2891555358219910499, 0.2891555358219910499, -0.2145669291338582474 ) ) ;
#7692 = CARTESIAN_POINT ( 'NONE',  ( -1.515748031496062076, -0.4536011799217367080, 0.2665933059059888421 ) ) ;
#7693 = CARTESIAN_POINT ( 'NONE',  ( 0.5577427821522314977, -0.3162353388693409650, -0.4822834645669289433 ) ) ;
#7694 = CARTESIAN_POINT ( 'NONE',  ( 1.108923884514436686, -0.2845877964562161244, -0.3641732283464567121 ) ) ;
#7695 = DIRECTION ( 'NONE',  ( -0.000000000000000000, 1.000000000000000000, -0.000000000000000000 ) ) ;
#7696 = CARTESIAN_POINT ( 'NONE',  ( 0.2165354330708668673, -0.4536011799217367080, 0.2665933059059888421 ) ) ;
#7697 = CARTESIAN_POINT ( 'NONE',  ( -1.371391076115484609, -0.6692913385826771977, 0.1292274648535927661 ) ) ;
#7698 = CARTESIAN_POINT ( 'NONE',  ( -0.1070741851644051862, -0.3996062992125986590, -0.9363517060367454459 ) ) ;
#7699 = CARTESIAN_POINT ( 'NONE',  ( 0.9842519685039378130, -0.6692913385826771977, 8.415575281601705876E-17 ) ) ;
#7700 = CARTESIAN_POINT ( 'NONE',  ( 4.797336870675656522E-17, -0.3917322834645670104, -0.8582677165354329896 ) ) ;
#7702 = CARTESIAN_POINT ( 'NONE',  ( 0.4724409448818898682, 2.892866454678787531E-17, -0.5098425196850393526 ) ) ;
#7701 = CARTESIAN_POINT ( 'NONE',  ( 0.6692913385826778638, -0.6692913385826771977, 8.415575281601705876E-17 ) ) ;
#7703 = CARTESIAN_POINT ( 'NONE',  ( 1.348312163386739426, 0.2755905511811023723, 0.7386866130305692613 ) ) ;
#7704 = CARTESIAN_POINT ( 'NONE',  ( 0.2559055118110243332, -0.4536011799217368745, -0.2665933059059886201 ) ) ;
#7705 = CARTESIAN_POINT ( 'NONE',  ( 0.6299212598425204535, -0.1870078740157480879, -0.4822834645669291653 ) ) ;
#7706 = CARTESIAN_POINT ( 'NONE',  ( -0.4744094488189045666, 1.537401574803149984, 2.170146923806632877 ) ) ;
#7707 = CARTESIAN_POINT ( 'NONE',  ( -0.7742782152230965886, -0.004921259842519576551, 0.3153832671262227771 ) ) ;
#7708 = CARTESIAN_POINT ( 'NONE',  ( -0.8792650918635160906, 0.05413385826771626580, -0.4176697321401330321 ) ) ;
#7709 = CARTESIAN_POINT ( 'NONE',  ( -1.509186351706035767, 0.05413385826771626580, -0.4176697321401330321 ) ) ;
#7710 = CARTESIAN_POINT ( 'NONE',  ( 0.8989501312335964611, 0.2952755905511811885, 0.1292274648535926551 ) ) ;
#7711 = CARTESIAN_POINT ( 'NONE',  ( 1.568241469816273659, -0.05778040916215560624, -0.4822834645669293319 ) ) ;
#7712 = FACE_OUTER_BOUND ( 'NONE', #35981, .T. ) ;
#7713 = CARTESIAN_POINT ( 'NONE',  ( 0.7611548556430451917, -0.6046776061558807314, 0.2411417322834647770 ) ) ;
#7714 = CARTESIAN_POINT ( 'NONE',  ( 0.4724409448818897572, -0.1265901696524988906, -2.708005249343832688 ) ) ;
#7715 = CARTESIAN_POINT ( 'NONE',  ( 1.653543307086614789, -0.1870078740157479769, 0.4822834645669291653 ) ) ;
#7716 = CARTESIAN_POINT ( 'NONE',  ( 1.332020997375329197, -0.3162353388693405765, 0.4822834645669290543 ) ) ;
#7717 = CARTESIAN_POINT ( 'NONE',  ( -1.240157480314959759, 0.07958543189024085140, 0.2665933059059887866 ) ) ;
#7718 = CARTESIAN_POINT ( 'NONE',  ( 1.410761154855643795, -0.08942795157528024563, -0.3641732283464568787 ) ) ;
#7719 = CARTESIAN_POINT ( 'NONE',  ( -1.128608923884513837, 0.1283753931104746893, -0.1820866141732285504 ) ) ;
#7720 = CARTESIAN_POINT ( 'NONE',  ( -0.3871391076115476282, -0.08942795157527998196, 0.3641732283464567121 ) ) ;
#7721 = CARTESIAN_POINT ( 'NONE',  ( 0.1938976377952755792, -0.2726377952755905665, 0.1574803149606299191 ) ) ;
#7722 = CARTESIAN_POINT ( 'NONE',  ( 0.9251968503937015864, -0.4536011799217367080, 0.2665933059059888421 ) ) ;
#7723 = CARTESIAN_POINT ( 'NONE',  ( 0.7349081364829403995, 0.2306618581243848609, 0.2411417322834645549 ) ) ;
#7724 = CARTESIAN_POINT ( 'NONE',  ( 1.128608923884514947, 0.2306618581243848609, 0.2411417322834645549 ) ) ;
#7725 = CARTESIAN_POINT ( 'NONE',  ( 0.01312335958005323398, -0.4281496062992127816, -0.4176697321401328100 ) ) ;
#7726 = CARTESIAN_POINT ( 'NONE',  ( 0.6627296587926515548, 0.1771653543307087630, 0.09757992244046791164 ) ) ;
#7727 = CARTESIAN_POINT ( 'NONE',  ( 1.056430446194226436, -0.6692913385826773087, -0.1292274648535924053 ) ) ;
#7728 = ADVANCED_FACE ( 'NONE', ( #15610 ), #81236, .F. ) ;
#7729 = CARTESIAN_POINT ( 'NONE',  ( -1.587926509186350810, 0.05413385826771626580, -0.4176697321401330321 ) ) ;
#7730 = CARTESIAN_POINT ( 'NONE',  ( -0.6955380577427815458, -0.4281496062992127816, -0.4176697321401328100 ) ) ;
#7731 = CIRCLE ( 'NONE', #65534, 1.122047244094488194 ) ;
#7732 = CARTESIAN_POINT ( 'NONE',  ( 0.1998031496062994405, -0.3460692066303958092, -0.7217847769028871152 ) ) ;
#7733 = CARTESIAN_POINT ( 'NONE',  ( -0.3129921259842520231, 1.470107679032609971, 3.734948428837856094E-17 ) ) ;
#7734 = CARTESIAN_POINT ( 'NONE',  ( 0.01968503937007930540, 0.1660481256975885056, 0.3530559997133364547 ) ) ;
#7735 = VECTOR ( 'NONE', #74110, 39.37007874015748143 ) ;
#7736 = CARTESIAN_POINT ( 'NONE',  ( -0.2165354330708654795, 0.1660481256975885056, 0.3530559997133364547 ) ) ;
#7737 = CARTESIAN_POINT ( 'NONE',  ( -0.08530183727034056085, -0.05778040916215560624, -0.4822834645669293319 ) ) ;
#7738 = CARTESIAN_POINT ( 'NONE',  ( 0.1998031496062992740, 0.3460692066303959757, -2.821522309711286258 ) ) ;
#7739 = CARTESIAN_POINT ( 'NONE',  ( -0.3420746716998659953, -0.1974969037888706647, -1.942257217847769279 ) ) ;
#7740 = CARTESIAN_POINT ( 'NONE',  ( -0.2867679344610365999, 0.2867679344610364889, -0.6417322834645668994 ) ) ;
#7741 = EDGE_CURVE ( 'NONE', #36894, #26552, #70016, .T. ) ;
#7742 = CARTESIAN_POINT ( 'NONE',  ( 0.3917322834645669549, 0.06192927228921583233, -1.216469835425646240 ) ) ;
#7743 = CARTESIAN_POINT ( 'NONE',  ( -0.9317585301837263412, -0.004921259842519576551, 0.3153832671262227771 ) ) ;
#7744 = CARTESIAN_POINT ( 'NONE',  ( -0.3392501089628019995, 0.1958661417322832277, -1.278215223097112885 ) ) ;
#7745 = CARTESIAN_POINT ( 'NONE',  ( -0.9908136482939626788, -0.6692913385826773087, -0.1292274648535924053 ) ) ;
#7746 = CARTESIAN_POINT ( 'NONE',  ( 4.797336870675655290E-17, -0.3917322834645669549, 0.1561872947844637760 ) ) ;
#7747 = CARTESIAN_POINT ( 'NONE',  ( 0.6233595800524942554, -0.05778040916215560624, -0.4822834645669293319 ) ) ;
#7748 = CARTESIAN_POINT ( 'NONE',  ( -0.6627296587926503335, -0.5511811023622046335, 0.09757992244046803654 ) ) ;
#7749 = CARTESIAN_POINT ( 'NONE',  ( 1.200787401574803681, -0.5400638737290845981, -0.3530559997133363437 ) ) ;
#7750 = CARTESIAN_POINT ( 'NONE',  ( 0.3412073490813655186, 0.2306618581243848609, 0.2411417322834645549 ) ) ;
#7751 = CARTESIAN_POINT ( 'NONE',  ( 0.4744094488188940750, 1.506013545763978945, 1.016821367227985551 ) ) ;
#7752 = CARTESIAN_POINT ( 'NONE',  ( -0.1070741851644051862, -0.3996062992125987146, -2.749343832020996636 ) ) ;
#7753 = CARTESIAN_POINT ( 'NONE',  ( 0.2867679344610366554, -0.2867679344610365999, -1.355006192422259170 ) ) ;
#7754 = CARTESIAN_POINT ( 'NONE',  ( 1.200787401574803681, 0.1660481256975885056, 0.3530559997133364547 ) ) ;
#7755 = CARTESIAN_POINT ( 'NONE',  ( 0.6167979002624678353, -0.4281496062992124485, 0.4176697321401328655 ) ) ;
#7756 = CARTESIAN_POINT ( 'NONE',  ( 0.3608923884514443348, 0.2952755905511810774, -0.1292274648535930714 ) ) ;
#7757 = CARTESIAN_POINT ( 'NONE',  ( -1.594488188976377119, 0.1660481256975883668, -0.3530559997133364547 ) ) ;
#7758 = CARTESIAN_POINT ( 'NONE',  ( 0.8005249343832028242, -0.4281496062992127816, -0.4176697321401328100 ) ) ;
#7759 = CARTESIAN_POINT ( 'NONE',  ( -0.3917322834645670104, -7.196005306013484475E-17, -0.7539370078740157410 ) ) ;
#7760 = CARTESIAN_POINT ( 'NONE',  ( 0.2624671916010504757, -0.6046776061558809534, -0.2411417322834644161 ) ) ;
#7761 = CARTESIAN_POINT ( 'NONE',  ( 0.8989501312335964611, 0.2952755905511811885, 0.1292274648535926551 ) ) ;
#7762 = CARTESIAN_POINT ( 'NONE',  ( 0.4461942257217856311, 0.2306618581243847221, -0.2411417322834647770 ) ) ;
#7763 = CARTESIAN_POINT ( 'NONE',  ( 0.9448818897637802916, -0.1870078740157480601, -0.3641732283464567677 ) ) ;
#7764 = CARTESIAN_POINT ( 'NONE',  ( -0.7349081364829390672, 0.2306618581243847221, -0.2411417322834647770 ) ) ;
#7765 = CARTESIAN_POINT ( 'NONE',  ( -1.404199475065615932, 0.05413385826771666132, 0.4176697321401328100 ) ) ;
#7766 = CARTESIAN_POINT ( 'NONE',  ( 0.8792650918635177559, -0.4281496062992127816, -0.4176697321401328100 ) ) ;
#7767 = CARTESIAN_POINT ( 'NONE',  ( 0.000000000000000000, 0.000000000000000000, 0.000000000000000000 ) ) ;
#7768 = CARTESIAN_POINT ( 'NONE',  ( 0.1049643490035304938, -0.3917322834645669549, -2.124671916010498762 ) ) ;
#7769 = ORIENTED_EDGE ( 'NONE', *, *, #56823, .F. ) ;
#7770 = CARTESIAN_POINT ( 'NONE',  ( 0.1998031496062994405, -0.3460692066303958092, -0.4068241469816273326 ) ) ;
#7771 = ORIENTED_EDGE ( 'NONE', *, *, #49802, .T. ) ;
#7772 = CYLINDRICAL_SURFACE ( 'NONE', #43520, 0.09842519685039351207 ) ;
#7773 = CARTESIAN_POINT ( 'NONE',  ( 0.7808398950131240079, -0.2845877964562159024, 0.3641732283464567677 ) ) ;
#7774 = CARTESIAN_POINT ( 'NONE',  ( 0.5627669687126071185, 0.02791078216816386681, 0.4328096321851896966 ) ) ;
#7775 = CARTESIAN_POINT ( 'NONE',  ( -0.4567729623170651010, 1.408376684009858826, 2.593294524635601395 ) ) ;
#7776 = CARTESIAN_POINT ( 'NONE',  ( -0.3917322834645670104, -7.196005306013484475E-17, -0.9114173228346457156 ) ) ;
#7777 = CARTESIAN_POINT ( 'NONE',  ( 1.463254593175853824, 0.2952755905511810774, -0.1292274648535930714 ) ) ;
#7778 = CARTESIAN_POINT ( 'NONE',  ( 1.036041590146032698, 3.421639014772782816E-16, 0.3464511005275203726 ) ) ;
#7779 = CARTESIAN_POINT ( 'NONE',  ( -0.3149606299212590610, -0.1870078740157479769, 0.4822834645669291653 ) ) ;
#7780 = CARTESIAN_POINT ( 'NONE',  ( 1.049868766404200127, -0.6046776061558809534, -0.2411417322834644161 ) ) ;
#7781 = ORIENTED_EDGE ( 'NONE', *, *, #37866, .F. ) ;
#7782 = CARTESIAN_POINT ( 'NONE',  ( -1.679790026246718693, 0.2306618581243847221, -0.2411417322834647770 ) ) ;
#7783 = CARTESIAN_POINT ( 'NONE',  ( -1.022510163891046098, 1.428599907254325618, -0.4620330969692038603 ) ) ;
#7784 =( NAMED_UNIT ( * ) SI_UNIT ( $, .STERADIAN. ) SOLID_ANGLE_UNIT ( ) );
#7785 = DIRECTION ( 'NONE',  ( 0.000000000000000000, 0.000000000000000000, 1.000000000000000000 ) ) ;
#7786 = CARTESIAN_POINT ( 'NONE',  ( 0.000000000000000000, 0.000000000000000000, -2.362204724409448620 ) ) ;
#7787 = CARTESIAN_POINT ( 'NONE',  ( -0.9842519685039360366, 0.1771653543307087630, 0.000000000000000000 ) ) ;
#7788 = CARTESIAN_POINT ( 'NONE',  ( 0.9055118110236227702, 0.2066929133858268208, 0.000000000000000000 ) ) ;
#7789 = CARTESIAN_POINT ( 'NONE',  ( 0.6299212598425204535, -0.1870078740157480879, -0.4822834645669291653 ) ) ;
#7790 = VECTOR ( 'NONE', #9685, 39.37007874015748143 ) ;
#7791 = ORIENTED_EDGE ( 'NONE', *, *, #42337, .T. ) ;
#7793 = CARTESIAN_POINT ( 'NONE',  ( 0.000000000000000000, 0.000000000000000000, -0.4921259842519685179 ) ) ;
#7792 = CARTESIAN_POINT ( 'NONE',  ( 0.2262115530851599166, 8.471767977567108961E-16, -0.4445507791589058955 ) ) ;
#7794 = CARTESIAN_POINT ( 'NONE',  ( 0.8858267716535438430, 0.1660481256975885056, 0.3530559997133364547 ) ) ;
#7795 = CARTESIAN_POINT ( 'NONE',  ( -1.719160104986876103, 0.05413385826771666132, 0.4176697321401328100 ) ) ;
#7796 = CARTESIAN_POINT ( 'NONE',  ( -0.2867679344610364334, -0.2867679344610368219, -0.9264898705698668691 ) ) ;
#7797 = CARTESIAN_POINT ( 'NONE',  ( -0.7480314960629914633, 0.1771653543307087630, 0.000000000000000000 ) ) ;
#7798 = EDGE_CURVE ( 'NONE', #74653, #57006, #16281, .T. ) ;
#7799 = CARTESIAN_POINT ( 'NONE',  ( 1.673228346456693494, 0.1660481256975885056, 0.3530559997133364547 ) ) ;
#7800 = CARTESIAN_POINT ( 'NONE',  ( 0.2867679344610366554, -0.2867679344610365444, -1.127952755905511806 ) ) ;
#7801 = CARTESIAN_POINT ( 'NONE',  ( 0.2690288713910767848, -0.6692913385826773087, -0.1292274648535924053 ) ) ;
#7802 = CARTESIAN_POINT ( 'NONE',  ( -1.062992125984250968, -0.5511811023622047445, 6.969142054262312111E-17 ) ) ;
#7803 = CARTESIAN_POINT ( 'NONE',  ( 0.1377952755905518800, -0.4536011799217367080, 0.2665933059059888421 ) ) ;
#7804 = CARTESIAN_POINT ( 'NONE',  ( -0.4199475065616791736, 0.2306618581243847221, -0.2411417322834647770 ) ) ;
#7805 = CARTESIAN_POINT ( 'NONE',  ( -1.312335958005248715, 0.1283753931104748280, 0.1820866141732283561 ) ) ;
#7806 = CARTESIAN_POINT ( 'NONE',  ( -0.1049643490035302301, -0.3917322834645671770, -0.2263972685377446670 ) ) ;
#7807 = CARTESIAN_POINT ( 'NONE',  ( 0.6561679790026253567, 0.2306618581243848609, 0.2411417322834645549 ) ) ;
#7808 = CARTESIAN_POINT ( 'NONE',  ( -1.607611548556429737, 0.2952755905511810774, -0.1292274648535930714 ) ) ;
#7809 = CARTESIAN_POINT ( 'NONE',  ( -0.2362204724409451284, 0.4091458600556402425, -1.507217847769029007 ) ) ;
#7810 = CARTESIAN_POINT ( 'NONE',  ( -0.7349081364829390672, 0.2306618581243847221, -0.2411417322834647770 ) ) ;
#7811 = CARTESIAN_POINT ( 'NONE',  ( 5.463695987328526437E-16, -0.1870078740157479769, 0.3641732283464567677 ) ) ;
#7812 = CARTESIAN_POINT ( 'NONE',  ( -1.161417322834644716, 0.1660481256975885056, 0.3530559997133364547 ) ) ;
#7813 = CARTESIAN_POINT ( 'NONE',  ( 0.9120734908136490793, 0.1771653543307087075, -0.09757992244046823083 ) ) ;
#7814 = CARTESIAN_POINT ( 'NONE',  ( -0.6364829396325453192, -0.2845877964562159024, 0.3641732283464567677 ) ) ;
#7815 = CARTESIAN_POINT ( 'NONE',  ( -0.8923884514435688198, 0.2306618581243847221, -0.2411417322834647770 ) ) ;
#7816 = CARTESIAN_POINT ( 'NONE',  ( -1.023622047244094002, -0.1870078740157480879, -0.4822834645669291653 ) ) ;
#7817 = CARTESIAN_POINT ( 'NONE',  ( 1.653543307086614789, -0.1870078740157479769, 0.4822834645669291653 ) ) ;
#7818 = CARTESIAN_POINT ( 'NONE',  ( 0.4724409448818914781, 0.1265901696524960318, -2.091207349081364519 ) ) ;
#7819 = CARTESIAN_POINT ( 'NONE',  ( 1.030183727034121421, -0.08942795157527998196, 0.3641732283464567121 ) ) ;
#7820 = CARTESIAN_POINT ( 'NONE',  ( 0.3543307086614181922, -0.6692913385826771977, 8.415575281601705876E-17 ) ) ;
#7821 = CARTESIAN_POINT ( 'NONE',  ( -1.417322834645668772, -0.1870078740157480879, -0.4822834645669291653 ) ) ;
#7822 = CARTESIAN_POINT ( 'NONE',  ( -1.614173228346456268, -0.6692913385826771977, 8.415575281601705876E-17 ) ) ;
#7823 = ORIENTED_EDGE ( 'NONE', *, *, #67121, .F. ) ;
#7824 = CARTESIAN_POINT ( 'NONE',  ( -0.1974969037888706924, 0.3420746716998658843, 0.2250656167979003253 ) ) ;
#7825 = CARTESIAN_POINT ( 'NONE',  ( -1.417322834645668772, -0.1870078740157480601, -0.3641732283464567677 ) ) ;
#7826 = CARTESIAN_POINT ( 'NONE',  ( 0.5577427821522314977, -0.3162353388693409650, -0.4822834645669289433 ) ) ;
#7827 = CARTESIAN_POINT ( 'NONE',  ( -1.030183727034119867, -0.08942795157528024563, -0.3641732283464568787 ) ) ;
#7828 = CARTESIAN_POINT ( 'NONE',  ( -0.3460692066303960313, 0.1998031496062989965, -1.992782152230971437 ) ) ;
#7829 = CARTESIAN_POINT ( 'NONE',  ( -1.555118110236219930, 0.1660481256975885056, 0.3530559997133364547 ) ) ;
#7830 = CARTESIAN_POINT ( 'NONE',  ( 0.9514435695538062676, -0.3162353388693409650, -0.4822834645669289433 ) ) ;
#7831 = CARTESIAN_POINT ( 'NONE',  ( 0.6627296587926517768, -0.6692913385826773087, -0.1292274648535924053 ) ) ;
#7832 = CARTESIAN_POINT ( 'NONE',  ( 1.371391076115485719, -0.6692913385826773087, -0.1292274648535924053 ) ) ;
#7833 = CARTESIAN_POINT ( 'NONE',  ( 0.4724409448818898682, 2.892866454678787531E-17, -0.8248031496062991907 ) ) ;
#7834 = CARTESIAN_POINT ( 'NONE',  ( -0.3996062992125986035, -0.1070741851644056997, -1.305774278215223072 ) ) ;
#7835 = CARTESIAN_POINT ( 'NONE',  ( -0.3949938075777409408, -0.1058382717557502933, -0.5183727034120736432 ) ) ;
#7836 = CARTESIAN_POINT ( 'NONE',  ( 1.016821367227983774, 1.553651517367183654, 0.4744094488188976277 ) ) ;
#7837 = CARTESIAN_POINT ( 'NONE',  ( 0.3018372703412079971, -0.3690944881889763329, 0.3153832671262228327 ) ) ;
#7838 = CARTESIAN_POINT ( 'NONE',  ( -0.1115485564304456306, 0.2952755905511810774, -0.1292274648535930714 ) ) ;
#7839 = CARTESIAN_POINT ( 'NONE',  ( 1.338582677165355062, -0.1870078740157480879, -0.4822834645669291653 ) ) ;
#7840 = CARTESIAN_POINT ( 'NONE',  ( 0.3420746716998660508, -0.1974969037888704149, -1.756561679790026309 ) ) ;
#7841 = CARTESIAN_POINT ( 'NONE',  ( 0.3543307086614181922, -0.5511811023622047445, 6.969142054262312111E-17 ) ) ;
#7842 = CARTESIAN_POINT ( 'NONE',  ( -0.6496062992125976043, 0.1660481256975883668, -0.3530559997133364547 ) ) ;
#7843 = CARTESIAN_POINT ( 'NONE',  ( 1.614173228346457378, 0.2952755905511811885, 0.000000000000000000 ) ) ;
#7844 = CARTESIAN_POINT ( 'NONE',  ( 0.3740157480314966754, -0.5400638737290844871, 0.3530559997133364547 ) ) ;
#7845 = CARTESIAN_POINT ( 'NONE',  ( -0.1265901696524993347, 0.4724409448818895907, -2.053805774278214979 ) ) ;
#7846 = VECTOR ( 'NONE', #8983, 39.37007874015748143 ) ;
#7847 = CARTESIAN_POINT ( 'NONE',  ( 0.3910482532979353554, 0.02544847934400223943, -2.755905511811024500 ) ) ;
#7848 = ORIENTED_EDGE ( 'NONE', *, *, #9813, .T. ) ;
#7849 = ORIENTED_EDGE ( 'NONE', *, *, #37212, .T. ) ;
#7850 = CARTESIAN_POINT ( 'NONE',  ( -1.404199475065615932, 0.05413385826771666132, 0.4176697321401328100 ) ) ;
#7852 = CARTESIAN_POINT ( 'NONE',  ( -1.299212598425196097, 0.2952755905511811885, 0.000000000000000000 ) ) ;
#7851 = CARTESIAN_POINT ( 'NONE',  ( -1.358267716535432434, -0.4536011799217367080, 0.2665933059059888421 ) ) ;
#7853 = CARTESIAN_POINT ( 'NONE',  ( -0.1049643490035306742, 0.3917322834645668994, -2.291319266895325946 ) ) ;
#7854 = CARTESIAN_POINT ( 'NONE',  ( -2.795275590551181466, 2.125984251968505045, 0.000000000000000000 ) ) ;
#7855 = CARTESIAN_POINT ( 'NONE',  ( -1.568241469816272105, -0.2845877964562161244, -0.3641732283464567121 ) ) ;
#7856 = CARTESIAN_POINT ( 'NONE',  ( -1.102362204724408601, -0.1870078740157479769, 0.4822834645669291653 ) ) ;
#7857 = CARTESIAN_POINT ( 'NONE',  ( 0.3149606299212603933, -0.1870078740157479769, 0.4822834645669291653 ) ) ;
#7858 = EDGE_CURVE ( 'NONE', #28229, #61385, #152, .T. ) ;
#7859 = CARTESIAN_POINT ( 'NONE',  ( -1.266404199475064773, -0.05778040916215560624, -0.4822834645669293319 ) ) ;
#7860 = CARTESIAN_POINT ( 'NONE',  ( -0.1958661417322834497, -0.3392501089628018884, -2.822815329887452318 ) ) ;
#7861 = ADVANCED_FACE ( 'NONE', ( #49220 ), #47568, .F. ) ;
#7862 = CARTESIAN_POINT ( 'NONE',  ( 0.6102362204724416372, -0.5400638737290844871, 0.3530559997133364547 ) ) ;
#7863 = CARTESIAN_POINT ( 'NONE',  ( -0.1049643490035307020, 0.3917322834645669549, -1.888451443569553412 ) ) ;
#7864 = CARTESIAN_POINT ( 'NONE',  ( -0.8005249343832011588, -0.004921259842519870586, -0.3153832671262229437 ) ) ;
#7865 = VERTEX_POINT ( 'NONE', #22323 ) ;
#7866 = CARTESIAN_POINT ( 'NONE',  ( -0.3420746716998661618, 0.1974969037888702206, -2.073490813648294129 ) ) ;
#7867 = ORIENTED_EDGE ( 'NONE', *, *, #56862, .T. ) ;
#7868 = CARTESIAN_POINT ( 'NONE',  ( -0.6406204526026236801, -3.721645946415733147E-15, -0.4118477457933000796 ) ) ;
#7869 = CARTESIAN_POINT ( 'NONE',  ( -1.062992125984250968, 0.2952755905511811885, 0.000000000000000000 ) ) ;
#7870 = CARTESIAN_POINT ( 'NONE',  ( -1.108923884514435132, -0.05778040916215560624, -0.4822834645669293319 ) ) ;
#7871 = CARTESIAN_POINT ( 'NONE',  ( 0.3996062992125986035, 0.1070741851644054776, -0.7545931758530182165 ) ) ;
#7872 = CARTESIAN_POINT ( 'NONE',  ( -1.673228346456691717, 0.1660481256975883668, -0.3530559997133364547 ) ) ;
#7873 = CARTESIAN_POINT ( 'NONE',  ( -1.673228346456691717, 0.1660481256975883668, -0.3530559997133364547 ) ) ;
#7874 = CARTESIAN_POINT ( 'NONE',  ( -1.640419947506561060, 0.05413385826771666132, 0.4176697321401328100 ) ) ;
#7875 = CARTESIAN_POINT ( 'NONE',  ( -1.313877454013332224, 1.122131950691689140, 0.7983292792091805090 ) ) ;
#7876 = CARTESIAN_POINT ( 'NONE',  ( -2.503252890251015828, 2.755905511811024056, -0.5314960629921260393 ) ) ;
#7877 = CARTESIAN_POINT ( 'NONE',  ( 0.1509186351706045259, -0.08942795157528024563, -0.3641732283464568787 ) ) ;
#7878 = DIRECTION ( 'NONE',  ( 1.047444401652940007E-14, -0.000000000000000000, -1.000000000000000000 ) ) ;
#7879 = CARTESIAN_POINT ( 'NONE',  ( -0.3917322834645669549, -0.1049643490035306603, -0.4455380577427821565 ) ) ;
#7880 = CARTESIAN_POINT ( 'NONE',  ( -0.5183727034120726440, -0.5511811023622048555, -0.09757992244046775898 ) ) ;
#7881 = CARTESIAN_POINT ( 'NONE',  ( -0.6824146981627288167, 0.2306618581243848609, 0.2411417322834645549 ) ) ;
#7882 = CARTESIAN_POINT ( 'NONE',  ( 0.8923884514435701520, -0.6046776061558809534, -0.2411417322834644161 ) ) ;
#7883 = CARTESIAN_POINT ( 'NONE',  ( -1.115485564304461219, 0.05413385826771626580, -0.4176697321401330321 ) ) ;
#7884 = ORIENTED_EDGE ( 'NONE', *, *, #48595, .F. ) ;
#7885 = ORIENTED_EDGE ( 'NONE', *, *, #20353, .F. ) ;
#7886 = CARTESIAN_POINT ( 'NONE',  ( -1.122047244094487306, 0.1660481256975883668, -0.3530559997133364547 ) ) ;
#7887 = CARTESIAN_POINT ( 'NONE',  ( 0.8005249343832027131, 0.05413385826771666132, 0.4176697321401328100 ) ) ;
#7888 = EDGE_CURVE ( 'NONE', #13837, #1571, #55231, .T. ) ;
#7889 = CARTESIAN_POINT ( 'NONE',  ( -1.528871391076114250, 0.1771653543307087075, -0.09757992244046823083 ) ) ;
#7890 = CARTESIAN_POINT ( 'NONE',  ( -0.04868480690927201593, 1.072582076400621753, 0.2414116071904397476 ) ) ;
#7891 = CARTESIAN_POINT ( 'NONE',  ( -0.3458507752293906723, -0.3458507752293910609, -1.318897637795275690 ) ) ;
#7892 = DIRECTION ( 'NONE',  ( -0.000000000000000000, -1.000000000000000000, -0.000000000000000000 ) ) ;
#7893 = ADVANCED_FACE ( 'NONE', ( #73686 ), #47193, .T. ) ;
#7894 = CARTESIAN_POINT ( 'NONE',  ( 0.1958661417322834775, 0.3392501089628018884, -0.2939632545931757934 ) ) ;
#7895 = CARTESIAN_POINT ( 'NONE',  ( 0.3917322834645670104, 2.398668435337828261E-17, -2.250000000000000000 ) ) ;
#7896 = CARTESIAN_POINT ( 'NONE',  ( -0.3412073490813641308, 0.2306618581243847221, -0.2411417322834647770 ) ) ;
#7897 = CARTESIAN_POINT ( 'NONE',  ( -1.430446194225720724, -0.004921259842519870586, -0.3153832671262229437 ) ) ;
#7898 = CARTESIAN_POINT ( 'NONE',  ( -0.8595800524934373854, -0.3162353388693409650, -0.4822834645669289433 ) ) ;
#7899 = CARTESIAN_POINT ( 'NONE',  ( -0.3460692066303960313, 0.1998031496062989965, 0.05446194225721782967 ) ) ;
#7901 = DIRECTION ( 'NONE',  ( -0.000000000000000000, -1.000000000000000000, -0.000000000000000000 ) ) ;
#7900 = CARTESIAN_POINT ( 'NONE',  ( -1.154855643044618851, -0.6046776061558809534, -0.2411417322834644161 ) ) ;
#7902 = CARTESIAN_POINT ( 'NONE',  ( -1.128608923884513837, -0.6046776061558807314, 0.2411417322834647770 ) ) ;
#7903 = CARTESIAN_POINT ( 'NONE',  ( -0.4265091863517051496, 0.2952755905511810774, -0.1292274648535930714 ) ) ;
#7904 = CARTESIAN_POINT ( 'NONE',  ( 0.1058382717557500852, -0.3949938075777408852, -2.839238845144357093 ) ) ;
#7905 = CARTESIAN_POINT ( 'NONE',  ( 0.2559055118110243332, -0.4536011799217368745, -0.2665933059059886201 ) ) ;
#7906 = DIRECTION ( 'NONE',  ( -0.5144957554275267908, -0.8574929257125440962, 0.000000000000000000 ) ) ;
#7907 = CARTESIAN_POINT ( 'NONE',  ( 0.4855643044619430415, -0.3690944881889765550, -0.3153832671262227771 ) ) ;
#7908 = CARTESIAN_POINT ( 'NONE',  ( 1.364829396325459854, -0.5023911411419708095, -0.1820866141732282451 ) ) ;
#7909 = CARTESIAN_POINT ( 'NONE',  ( 0.9514435695538062676, -0.05778040916215522460, 0.4822834645669289988 ) ) ;
#7910 = CARTESIAN_POINT ( 'NONE',  ( 0.1902887139107617975, -0.5511811023622048555, -0.09757992244046775898 ) ) ;
#7911 = CARTESIAN_POINT ( 'NONE',  ( -0.3917322834645670104, -7.196005306013484475E-17, -1.921259842519684957 ) ) ;
#7912 = CARTESIAN_POINT ( 'NONE',  ( -1.430446194225720724, 0.05413385826771626580, -0.4176697321401330321 ) ) ;
#7913 = CARTESIAN_POINT ( 'NONE',  ( -0.2099737532808391705, -0.5023911411419708095, -0.1820866141732282451 ) ) ;
#7914 = CARTESIAN_POINT ( 'NONE',  ( -0.4724409448818899238, 0.1265901696524986686, 0.2053805774278214813 ) ) ;
#7915 = CARTESIAN_POINT ( 'NONE',  ( -0.5183727034120726440, 0.1771653543307087630, 0.09757992244046791164 ) ) ;
#7916 = CARTESIAN_POINT ( 'NONE',  ( -0.4678516549211644837, 1.617630162216313172, -1.019861537960136566 ) ) ;
#7917 = CARTESIAN_POINT ( 'NONE',  ( -0.1771653543307080136, 0.1660481256975883668, -0.3530559997133364547 ) ) ;
#7918 = CARTESIAN_POINT ( 'NONE',  ( 0.000000000000000000, 0.000000000000000000, 0.000000000000000000 ) ) ;
#7919 = CARTESIAN_POINT ( 'NONE',  ( 1.161417322834646271, 0.07958543189024071263, -0.2665933059059888421 ) ) ;
#7920 = CARTESIAN_POINT ( 'NONE',  ( -0.05249343832020938322, -0.5023911411419708095, -0.1820866141732282451 ) ) ;
#7921 = CARTESIAN_POINT ( 'NONE',  ( -0.1706036745406816491, 0.05413385826771626580, -0.4176697321401330321 ) ) ;
#7922 = CARTESIAN_POINT ( 'NONE',  ( 0.1181102362204724532, 0.09842519685039372024, 0.000000000000000000 ) ) ;
#7923 = CARTESIAN_POINT ( 'NONE',  ( -0.6889763779527552368, 0.07958543189024085140, 0.2665933059059887866 ) ) ;
#7924 = DIRECTION ( 'NONE',  ( 0.000000000000000000, 0.000000000000000000, 1.000000000000000000 ) ) ;
#7925 = CARTESIAN_POINT ( 'NONE',  ( 0.6889763779527566800, -0.5400638737290844871, 0.3530559997133364547 ) ) ;
#7926 = CARTESIAN_POINT ( 'NONE',  ( -0.7677165354330699465, -0.5400638737290845981, -0.3530559997133363437 ) ) ;
#7927 = CARTESIAN_POINT ( 'NONE',  ( -9.787531504996566615E-17, 0.3996062992125985480, -1.336614173228346303 ) ) ;
#7928 = CARTESIAN_POINT ( 'NONE',  ( -0.3917322834645671215, 0.1049643490035301469, -2.794619422572177658 ) ) ;
#7929 = CARTESIAN_POINT ( 'NONE',  ( 0.1837270341207354329, 0.1283753931104748280, 0.1820866141732283561 ) ) ;
#7930 = CARTESIAN_POINT ( 'NONE',  ( -0.9514435695538050464, -0.05778040916215560624, -0.4822834645669293319 ) ) ;
#7931 = CARTESIAN_POINT ( 'NONE',  ( -0.9908136482939626788, 0.2952755905511811885, 0.1292274648535926551 ) ) ;
#7932 = CARTESIAN_POINT ( 'NONE',  ( -1.384514435695537005, -0.5511811023622048555, -0.09757992244046775898 ) ) ;
#7933 = CARTESIAN_POINT ( 'NONE',  ( 1.686351706036745890, 0.2952755905511811885, 0.1292274648535926551 ) ) ;
#7934 = CARTESIAN_POINT ( 'NONE',  ( -1.069553805774277722, -0.5511811023622048555, -0.09757992244046775898 ) ) ;
#7935 = CARTESIAN_POINT ( 'NONE',  ( -0.7414698162729651543, 0.2066929133858267098, -0.1054918080437494132 ) ) ;
#7936 = CARTESIAN_POINT ( 'NONE',  ( 0.7480314960629927956, -0.6692913385826771977, 8.415575281601705876E-17 ) ) ;
#7937 = CARTESIAN_POINT ( 'NONE',  ( -0.3460692066303958092, -0.1998031496062994683, -0.2099737532808398921 ) ) ;
#7938 = CARTESIAN_POINT ( 'NONE',  ( 0.3392501089628018329, 0.1958661417322835607, -2.647657111057429624 ) ) ;
#7939 = ORIENTED_EDGE ( 'NONE', *, *, #28626, .T. ) ;
#7940 = DIRECTION ( 'NONE',  ( -0.000000000000000000, -1.000000000000000000, -0.000000000000000000 ) ) ;
#7941 = CARTESIAN_POINT ( 'NONE',  ( 1.502624671916010790, -0.2845877964562161244, -0.3641732283464567121 ) ) ;
#7942 = CARTESIAN_POINT ( 'NONE',  ( -1.135170603674539924, -0.6692913385826771977, 0.1292274648535927661 ) ) ;
#7943 = ADVANCED_FACE ( 'NONE', ( #3384 ), #56554, .T. ) ;
#7944 = CARTESIAN_POINT ( 'NONE',  ( 1.351706036745407458, -0.4281496062992127816, -0.4176697321401328100 ) ) ;
#7945 = CARTESIAN_POINT ( 'NONE',  ( 0.3917322834645670104, -0.1049643490035303411, -2.558398950131233196 ) ) ;
#7946 = DIRECTION ( 'NONE',  ( 0.000000000000000000, -1.000000000000000000, 0.000000000000000000 ) ) ;
#7947 = CARTESIAN_POINT ( 'NONE',  ( 0.5183727034120741983, -0.6692913385826771977, 0.1292274648535927661 ) ) ;
#7948 = CARTESIAN_POINT ( 'NONE',  ( -0.2165354330708654795, 0.1660481256975885056, 0.3530559997133364547 ) ) ;
#7949 = DIRECTION ( 'NONE',  ( 1.000000000000000000, 0.000000000000000000, 0.000000000000000000 ) ) ;
#7950 = CARTESIAN_POINT ( 'NONE',  ( 0.06632061457837788720, 2.409604939980833412E-17, -0.3464511005275205946 ) ) ;
#7951 = CARTESIAN_POINT ( 'NONE',  ( 0.6233595800524939223, -0.2845877964562159024, 0.3641732283464567677 ) ) ;
#7952 = CARTESIAN_POINT ( 'NONE',  ( 0.3996062992125986590, -0.1070741851644053111, -1.843832020997375309 ) ) ;
#7953 = ORIENTED_EDGE ( 'NONE', *, *, #1563, .T. ) ;
#7954 = CARTESIAN_POINT ( 'NONE',  ( -0.1049643490035307158, 0.3917322834645670104, -0.003300155676852285953 ) ) ;
#7955 = EDGE_LOOP ( 'NONE', ( #82606, #18516, #31125, #82166 ) ) ;
#7956 = CARTESIAN_POINT ( 'NONE',  ( 0.1706036745406830368, 0.05413385826771666132, 0.4176697321401328100 ) ) ;
#7957 = CARTESIAN_POINT ( 'NONE',  ( 1.272965879265092637, 0.05413385826771666132, 0.4176697321401328100 ) ) ;
#7958 = CARTESIAN_POINT ( 'NONE',  ( 0.2230971128608932319, -0.4281496062992124485, 0.4176697321401328655 ) ) ;
#7959 = CARTESIAN_POINT ( 'NONE',  ( -0.5511811023622038563, -0.1870078740157479769, 0.3641732283464567677 ) ) ;
#7960 = CARTESIAN_POINT ( 'NONE',  ( 1.279527559055118724, -0.5400638737290845981, -0.3530559997133363437 ) ) ;
#7961 = CARTESIAN_POINT ( 'NONE',  ( -0.3280839895013117347, 0.05413385826771626580, -0.4176697321401330321 ) ) ;
#7962 = CARTESIAN_POINT ( 'NONE',  ( 0.05905511811023681640, 0.1660481256975883668, -0.3530559997133364547 ) ) ;
#7963 = CARTESIAN_POINT ( 'NONE',  ( -1.581364829396324945, -0.05778040916215560624, -0.4822834645669293319 ) ) ;
#7964 = CARTESIAN_POINT ( 'NONE',  ( 1.154855643044620184, 0.2306618581243847221, -0.2411417322834647770 ) ) ;
#7965 = CARTESIAN_POINT ( 'NONE',  ( 1.318897637795276356, -0.5400638737290844871, 0.3530559997133364547 ) ) ;
#7966 = CARTESIAN_POINT ( 'NONE',  ( 0.1049643490035304938, -0.3917322834645669549, -0.5498687664041993495 ) ) ;
#7967 = CARTESIAN_POINT ( 'NONE',  ( 0.5052493438320218022, -0.5511811023622048555, -0.09757992244046775898 ) ) ;
#7968 = ORIENTED_EDGE ( 'NONE', *, *, #9731, .T. ) ;
#7969 = CARTESIAN_POINT ( 'NONE',  ( -0.3420746716998661618, 0.1974969037888702206, -0.8136482939632546652 ) ) ;
#7970 = VERTEX_POINT ( 'NONE', #54295 ) ;
#7971 = CARTESIAN_POINT ( 'NONE',  ( -0.4133858267716528645, 0.07958543189024071263, -0.2665933059059888421 ) ) ;
#7972 = CARTESIAN_POINT ( 'NONE',  ( -0.03937007874015669567, 0.2952755905511811885, 0.000000000000000000 ) ) ;
#7973 = CARTESIAN_POINT ( 'NONE',  ( 2.808613111760720926, 1.134406187872319505, 0.2508088161067695276 ) ) ;
#7974 = CARTESIAN_POINT ( 'NONE',  ( -0.09842519685039295696, 0.1660481256975883668, -0.3530559997133364547 ) ) ;
#7975 = CARTESIAN_POINT ( 'NONE',  ( 0.2034120734908142214, 0.2952755905511810774, -0.1292274648535930714 ) ) ;
#7976 = CARTESIAN_POINT ( 'NONE',  ( -0.9055118110236215490, -0.6692913385826771977, 8.415575281601705876E-17 ) ) ;
#7977 = CARTESIAN_POINT ( 'NONE',  ( -0.9317585301837263412, 0.05413385826771666132, 0.4176697321401328100 ) ) ;
#7978 = CARTESIAN_POINT ( 'NONE',  ( 1.167979002624672580, -0.3690944881889763329, 0.3153832671262228327 ) ) ;
#7979 = CARTESIAN_POINT ( 'NONE',  ( -1.528871391076114250, -0.6692913385826771977, 0.1292274648535927661 ) ) ;
#7980 = CARTESIAN_POINT ( 'NONE',  ( 0.5314960629921348101, 2.742784437388869900, -2.516666458167339471 ) ) ;
#7981 = CARTESIAN_POINT ( 'NONE',  ( 0.8923884514435701520, -0.5023911411419708095, -0.1820866141732282451 ) ) ;
#7982 = CARTESIAN_POINT ( 'NONE',  ( 0.5249343832021005074, -0.6046776061558807314, 0.2411417322834647770 ) ) ;
#7983 = CARTESIAN_POINT ( 'NONE',  ( 0.3477690288713918276, -0.6692913385826773087, -0.1292274648535924053 ) ) ;
#7984 = CARTESIAN_POINT ( 'NONE',  ( 0.2925321140481932369, 0.2925321140481932369, -1.082677165354330562 ) ) ;
#7985 = CARTESIAN_POINT ( 'NONE',  ( 0.3256598226813657848, 2.726622551019859153E-15, 0.4118477457932983032 ) ) ;
#7986 = CARTESIAN_POINT ( 'NONE',  ( 0.3996062992125986035, -0.1070741851644052972, -0.6607611548556431291 ) ) ;
#7987 = CARTESIAN_POINT ( 'NONE',  ( -0.1998031496062991630, -0.3460692066303959202, -0.4573490813648293796 ) ) ;
#7988 = CARTESIAN_POINT ( 'NONE',  ( -0.4855643044619415427, -0.4281496062992124485, 0.4176697321401328655 ) ) ;
#7989 = CARTESIAN_POINT ( 'NONE',  ( 0.4724409448818896462, 0.1265901696524990294, -0.1246719160104986929 ) ) ;
#7990 = CARTESIAN_POINT ( 'NONE',  ( 0.3917322834645669549, 0.1049643490035304660, -1.941601049868766582 ) ) ;
#7991 = CARTESIAN_POINT ( 'NONE',  ( -1.115485564304461219, -0.004921259842519870586, -0.3153832671262229437 ) ) ;
#7992 = CARTESIAN_POINT ( 'NONE',  ( 0.9908136482939640111, 0.2952755905511810774, -0.1292274648535930714 ) ) ;
#7993 = CARTESIAN_POINT ( 'NONE',  ( 0.9908136482939640111, -0.6692913385826771977, 0.1292274648535927661 ) ) ;
#7994 = CARTESIAN_POINT ( 'NONE',  ( -0.2230971128608915943, -0.004921259842519576551, 0.3153832671262227771 ) ) ;
#7995 = CARTESIAN_POINT ( 'NONE',  ( 0.2887139107611556010, -0.6046776061558807314, 0.2411417322834647770 ) ) ;
#7996 = CARTESIAN_POINT ( 'NONE',  ( -0.4091458600556405756, 0.2362204724409446288, -1.835301837270341352 ) ) ;
#7997 = CARTESIAN_POINT ( 'NONE',  ( 0.1115485564304470323, 0.1771653543307087630, 0.09757992244046791164 ) ) ;
#7998 =( BOUNDED_CURVE ( )  B_SPLINE_CURVE ( 2, ( #80631, #16651, #60001, #73893, #74304, #67574, #10333, #41880, #35995, #4006, #22942, #48609, #2356, #73480, #35166, #14984, #40643, #66327, #22119, #54924, #3595, #9086, #61665, #72636, #46944, #8665, #67163, #47362, #29260, #60827, #41478, #60418, #34336, #54088, #22535, #67988, #42291, #29670, #16233, #28012, #53672, #78970, #21291, #79380, #54505, #21699, #80219, #73053, #35578, #15403, #41063, #48198, #66752, #34758, #2769, #28428, #79803, #15830, #9906, #28843, #3179, #61241, #82271, #11568, #49025, #23354, #62075, #70032, #30903, #38043, #74721, #68403, #17479, #43110, #5239, #63308, #56570, #75954, #31313, #36400, #4821, #81452, #17885, #24991, #82675, #5646, #55744, #37632, #24589, #37227, #62904, #30082, #81865, #75545, #17070, #68806, #6059, #56978, #69220, #62487, #75134, #23769, #50666, #56162, #50257, #18293, #76366, #18699, #4413, #43938, #44341, #69632, #12385, #11977, #63719, #55332, #81041, #42707, #49440, #49846, #10743, #36811, #11152, #30499, #24177, #43521, #58222, #45170, #46430, #25407, #83085, #51070, #19944, #169, #39713, #45594, #77611, #13225, #70445, #6889, #58648, #14480, #32146, #6476, #72122, #31730, #1015, #33407, #78450, #38457, #7311, #64143, #32980, #57802, #71705, #25822, #51482, #26668, #65819, #77185, #19517, #70876, #32559, #1424, #59069, #52323, #51904, #57394, #78029, #71287, #76769, #19100, #38873, #40134, #20358, #44749, #12802, #64552, #589, #26245, #64974, #13635, #39287, #46009, #20776, #14059, #65404, #7742, #27080 ),
 .UNSPECIFIED., .F., .F. ) 
 B_SPLINE_CURVE_WITH_KNOTS ( ( 3, 2, 2, 2, 2, 2, 2, 2, 2, 2, 2, 2, 2, 2, 2, 2, 2, 2, 2, 2, 2, 2, 2, 2, 2, 2, 2, 2, 2, 2, 2, 2, 2, 2, 2, 2, 2, 2, 2, 2, 2, 2, 2, 2, 2, 2, 2, 2, 2, 2, 2, 2, 2, 2, 2, 2, 2, 2, 2, 2, 2, 2, 2, 2, 2, 2, 2, 2, 2, 2, 2, 2, 2, 2, 2, 2, 2, 2, 2, 2, 2, 2, 2, 2, 2, 2, 2, 2, 2, 2, 2, 2, 2, 2, 3 ),
 ( 0.05249317594045464080, 0.05416666666666666852, 0.05833333333333333426, 0.06250000000000000000, 0.06666666666666666574, 0.07083333333333333148, 0.07499999999999999722, 0.07916666666666666297, 0.08333333333333332871, 0.08749999999999999445, 0.09166666666666666019, 0.09583333333333333981, 0.1000000000000000056, 0.1041666666666666713, 0.1083333333333333370, 0.1125000000000000028, 0.1166666666666666685, 0.1208333333333333204, 0.1250000000000000000, 0.1291666666666666796, 0.1333333333333333315, 0.1375000000000000111, 0.1416666666666666630, 0.1458333333333333426, 0.1500000000000000222, 0.1541666666666666741, 0.1583333333333333259, 0.1625000000000000056, 0.1666666666666666574, 0.1708333333333333370, 0.1749999999999999889, 0.1791666666666666685, 0.1833333333333333204, 0.1875000000000000000, 0.1916666666666666796, 0.1958333333333333315, 0.2000000000000000111, 0.2041666666666666630, 0.2083333333333333426, 0.2124999999999999944, 0.2166666666666666741, 0.2208333333333333259, 0.2250000000000000333, 0.2291666666666666574, 0.2333333333333333370, 0.2374999999999999889, 0.2416666666666666685, 0.2458333333333333204, 0.2499999999999999722, 0.2541666666666666519, 0.2583333333333333592, 0.2625000000000000111, 0.2666666666666666630, 0.2708333333333333148, 0.2750000000000000222, 0.2791666666666666741, 0.2833333333333333259, 0.2874999999999999778, 0.2916666666666666852, 0.2958333333333333370, 0.2999999999999999889, 0.3041666666666666408, 0.3083333333333333481, 0.3125000000000000000, 0.3166666666666666519, 0.3208333333333333592, 0.3250000000000000111, 0.3291666666666666630, 0.3333333333333333148, 0.3375000000000000222, 0.3416666666666666741, 0.3458333333333333259, 0.3499999999999999778, 0.3541666666666666852, 0.3583333333333333370, 0.3624999999999999889, 0.3666666666666666408, 0.3708333333333333481, 0.3750000000000000000, 0.3791666666666666519, 0.3833333333333334147, 0.3875000000000000111, 0.3916666666666666630, 0.3958333333333333148, 0.4000000000000000222, 0.4041666666666666741, 0.4083333333333333814, 0.4124999999999999778, 0.4166666666666666852, 0.4208333333333332815, 0.4249999999999999889, 0.4291666666666666408, 0.4333333333333333481, 0.4375000000000000000, 0.4399931759404547282 ),
 .UNSPECIFIED. ) 
 CURVE ( )  GEOMETRIC_REPRESENTATION_ITEM ( )  RATIONAL_B_SPLINE_CURVE ( ( 0.9836222570911056229, 0.9863145247099402990, 1.000000000000000000, 0.9659258262890683122, 1.000000000000000000, 0.9659258262890683122, 1.000000000000000000, 0.9659258262890683122, 1.000000000000000000, 0.9659258262890683122, 1.000000000000000000, 0.9659258262890683122, 1.000000000000000000, 0.9659258262890683122, 1.000000000000000000, 0.9659258262890683122, 1.000000000000000000, 0.9659258262890683122, 1.000000000000000000, 0.9659258262890683122, 1.000000000000000000, 0.9659258262890683122, 1.000000000000000000, 0.9659258262890683122, 1.000000000000000000, 0.9659258262890683122, 1.000000000000000000, 0.9659258262890683122, 1.000000000000000000, 0.9659258262890683122, 1.000000000000000000, 0.9659258262890683122, 1.000000000000000000, 0.9659258262890683122, 1.000000000000000000, 0.9659258262890683122, 1.000000000000000000, 0.9659258262890683122, 1.000000000000000000, 0.9659258262890683122, 1.000000000000000000, 0.9659258262890683122, 1.000000000000000000, 0.9659258262890683122, 1.000000000000000000, 0.9659258262890683122, 1.000000000000000000, 0.9659258262890683122, 1.000000000000000000, 0.9659258262890683122, 1.000000000000000000, 0.9659258262890683122, 1.000000000000000000, 0.9659258262890683122, 1.000000000000000000, 0.9659258262890683122, 1.000000000000000000, 0.9659258262890683122, 1.000000000000000000, 0.9659258262890683122, 1.000000000000000000, 0.9659258262890683122, 1.000000000000000000, 0.9659258262890683122, 1.000000000000000000, 0.9659258262890683122, 1.000000000000000000, 0.9659258262890683122, 1.000000000000000000, 0.9659258262890683122, 1.000000000000000000, 0.9659258262890683122, 1.000000000000000000, 0.9659258262890683122, 1.000000000000000000, 0.9659258262890683122, 1.000000000000000000, 0.9659258262890683122, 1.000000000000000000, 0.9659258262890683122, 1.000000000000000000, 0.9659258262890683122, 1.000000000000000000, 0.9659258262890683122, 1.000000000000000000, 0.9659258262890683122, 1.000000000000000000, 0.9659258262890683122, 1.000000000000000000, 0.9659258262890683122, 1.000000000000000000, 0.9659258262890683122, 1.000000000000000000, 0.9659258262890683122, 1.000000000000000000, 0.9659258262890683122, 1.000000000000000000, 0.9659258262890683122, 1.000000000000000000, 0.9659258262890683122, 1.000000000000000000, 0.9659258262890683122, 1.000000000000000000, 0.9659258262890683122, 1.000000000000000000, 0.9659258262890683122, 1.000000000000000000, 0.9659258262890683122, 1.000000000000000000, 0.9659258262890683122, 1.000000000000000000, 0.9659258262890683122, 1.000000000000000000, 0.9659258262890683122, 1.000000000000000000, 0.9659258262890683122, 1.000000000000000000, 0.9659258262890683122, 1.000000000000000000, 0.9659258262890683122, 1.000000000000000000, 0.9659258262890683122, 1.000000000000000000, 0.9659258262890683122, 1.000000000000000000, 0.9659258262890683122, 1.000000000000000000, 0.9659258262890683122, 1.000000000000000000, 0.9659258262890683122, 1.000000000000000000, 0.9659258262890683122, 1.000000000000000000, 0.9659258262890683122, 1.000000000000000000, 0.9659258262890683122, 1.000000000000000000, 0.9659258262890683122, 1.000000000000000000, 0.9659258262890683122, 1.000000000000000000, 0.9659258262890683122, 1.000000000000000000, 0.9659258262890683122, 1.000000000000000000, 0.9659258262890683122, 1.000000000000000000, 0.9659258262890683122, 1.000000000000000000, 0.9659258262890683122, 1.000000000000000000, 0.9659258262890683122, 1.000000000000000000, 0.9659258262890683122, 1.000000000000000000, 0.9659258262890683122, 1.000000000000000000, 0.9659258262890683122, 1.000000000000000000, 0.9659258262890683122, 1.000000000000000000, 0.9659258262890683122, 1.000000000000000000, 0.9659258262890683122, 1.000000000000000000, 0.9659258262890683122, 1.000000000000000000, 0.9659258262890683122, 1.000000000000000000, 0.9659258262890683122, 1.000000000000000000, 0.9659258262890683122, 1.000000000000000000, 0.9659258262890683122, 1.000000000000000000, 0.9659258262890683122, 1.000000000000000000, 0.9659258262890683122, 1.000000000000000000, 0.9659258262890683122, 1.000000000000000000, 0.9659258262890683122, 1.000000000000000000, 0.9659258262890683122, 1.000000000000000000, 0.9659258262890683122, 1.000000000000000000, 0.9796113015791271250, 0.9836222570911059560 ) ) 
 REPRESENTATION_ITEM ( '' )  );
#7999 = CARTESIAN_POINT ( 'NONE',  ( 0.01312335958005323398, 0.05413385826771666132, 0.4176697321401328100 ) ) ;
#8000 = CARTESIAN_POINT ( 'NONE',  ( -0.3420746716998660508, -0.1974969037888706924, -1.546587926509186417 ) ) ;
#8001 = CARTESIAN_POINT ( 'NONE',  ( -1.325459317585300889, -0.4281496062992127816, -0.4176697321401328100 ) ) ;
#8002 = CARTESIAN_POINT ( 'NONE',  ( 0.4133858267716541968, -0.4536011799217368745, -0.2665933059059886201 ) ) ;
#8003 = CARTESIAN_POINT ( 'NONE',  ( 1.627296587926509996, -0.5023911411419708095, 0.1820866141732285504 ) ) ;
#8004 = CARTESIAN_POINT ( 'NONE',  ( -0.6889763779527552368, -0.5400638737290845981, -0.3530559997133363437 ) ) ;
#8005 = CARTESIAN_POINT ( 'NONE',  ( -0.3937007874015740483, -0.1870078740157479769, 0.3641732283464567677 ) ) ;
#8006 = CARTESIAN_POINT ( 'NONE',  ( -0.7213048242569877200, 1.923042556024872285, -0.5309055118110235227 ) ) ;
#8007 = CARTESIAN_POINT ( 'NONE',  ( -0.7545931758530177724, 0.2952755905511811885, 0.1292274648535926551 ) ) ;
#8008 = CARTESIAN_POINT ( 'NONE',  ( -0.6758530183727028406, 0.2952755905511811885, 0.1292274648535926551 ) ) ;
#8009 = CARTESIAN_POINT ( 'NONE',  ( 0.05905511811023709395, -0.5400638737290844871, 0.3530559997133364547 ) ) ;
#8010 = CARTESIAN_POINT ( 'NONE',  ( 0.2925321140481932369, -0.2925321140481931814, -2.694881889763780070 ) ) ;
#8011 = CARTESIAN_POINT ( 'NONE',  ( 0.3392501089628018329, 0.1958661417322835052, -2.101030552984564981 ) ) ;
#8012 = CARTESIAN_POINT ( 'NONE',  ( -1.633858267716534529, -0.4536011799217368745, -0.2665933059059886201 ) ) ;
#8013 = CARTESIAN_POINT ( 'NONE',  ( 0.5643044619422579178, -0.004921259842519576551, 0.3153832671262227771 ) ) ;
#8014 = CARTESIAN_POINT ( 'NONE',  ( 1.377952755905512472, -0.6692913385826771977, 8.415575281601705876E-17 ) ) ;
#8015 = CARTESIAN_POINT ( 'NONE',  ( -0.7349081364829390672, 0.1283753931104746893, -0.1820866141732285504 ) ) ;
#8016 = EDGE_CURVE ( 'NONE', #11783, #12200, #28217, .T. ) ;
#8017 = CARTESIAN_POINT ( 'NONE',  ( -1.207349081364828880, 0.1283753931104746893, -0.1820866141732285504 ) ) ;
#8018 = CARTESIAN_POINT ( 'NONE',  ( -0.6955380577427815458, 0.05413385826771666132, 0.4176697321401328100 ) ) ;
#8019 = CARTESIAN_POINT ( 'NONE',  ( -0.5052493438320203589, -0.6692913385826771977, 0.1292274648535927661 ) ) ;
#8020 = CARTESIAN_POINT ( 'NONE',  ( 0.4790026246719168435, -0.2845877964562161244, -0.3641732283464567121 ) ) ;
#8021 = CARTESIAN_POINT ( 'NONE',  ( -0.2431769186048377551, 0.1675026378872651045, 5.643961825897842566 ) ) ;
#8022 = CARTESIAN_POINT ( 'NONE',  ( 1.279527559055118724, 0.07958543189024085140, 0.2665933059059887866 ) ) ;
#8023 = EDGE_CURVE ( 'NONE', #72980, #79206, #5617, .T. ) ;
#8024 = CARTESIAN_POINT ( 'NONE',  ( 0.5183727034120741983, -0.6692913385826771977, 0.1292274648535927661 ) ) ;
#8025 = CARTESIAN_POINT ( 'NONE',  ( -0.1070741851644051862, -0.3996062992125986590, 0.1660104986876640432 ) ) ;
#8026 = CARTESIAN_POINT ( 'NONE',  ( -0.5839895013123351797, 0.2952755905511810774, -0.1292274648535930714 ) ) ;
#8027 = CARTESIAN_POINT ( 'NONE',  ( -0.2867679344610364334, -0.2867679344610367109, -1.403543307086614123 ) ) ;
#8028 = CARTESIAN_POINT ( 'NONE',  ( 1.456692913385827515, 0.1771653543307087630, 0.000000000000000000 ) ) ;
#8029 = CARTESIAN_POINT ( 'NONE',  ( 0.5839895013123367340, 0.2952755905511811885, 0.1292274648535926551 ) ) ;
#8030 = CARTESIAN_POINT ( 'NONE',  ( 0.3280839895013130669, -0.4281496062992127816, -0.4176697321401328100 ) ) ;
#8031 = CARTESIAN_POINT ( 'NONE',  ( -0.02624671916010428221, 0.1283753931104746893, -0.1820866141732285504 ) ) ;
#8032 = DIRECTION ( 'NONE',  ( -0.000000000000000000, -1.000000000000000000, -0.000000000000000000 ) ) ;
#8033 = CARTESIAN_POINT ( 'NONE',  ( 8.195543980992789655E-16, -0.1870078740157480601, -0.3641732283464567677 ) ) ;
#8034 = CARTESIAN_POINT ( 'NONE',  ( 0.9908136482939640111, -0.6692913385826771977, 0.1292274648535927661 ) ) ;
#8035 = CARTESIAN_POINT ( 'NONE',  ( -0.5839895013123351797, 0.1771653543307087075, -0.09757992244046823083 ) ) ;
#8036 = CARTESIAN_POINT ( 'NONE',  ( -0.5577427821522301654, -0.3162353388693405765, 0.4822834645669290543 ) ) ;
#8037 = DIRECTION ( 'NONE',  ( 0.000000000000000000, 0.000000000000000000, 1.000000000000000000 ) ) ;
#8038 = B_SPLINE_CURVE_WITH_KNOTS ( 'NONE', 3,
 ( #40201, #73020, #60385, #1905, #21259, #59550, #73861 ),
 .UNSPECIFIED., .F., .F.,
 ( 4, 3, 4 ),
 ( 7.703719777548943412E-34, 0.001246232571205256601, 0.002492492258783257208 ),
 .UNSPECIFIED. ) ;
#8039 = ORIENTED_EDGE ( 'NONE', *, *, #31019, .F. ) ;
#8040 = CARTESIAN_POINT ( 'NONE',  ( -1.312335958005248715, 0.2306618581243848609, 0.2411417322834645549 ) ) ;
#8041 = CARTESIAN_POINT ( 'NONE',  ( -1.128608923884513837, -0.5023911411419708095, 0.1820866141732285504 ) ) ;
#8042 = CARTESIAN_POINT ( 'NONE',  ( 0.1640419947506569498, -0.05778040916215522460, 0.4822834645669289988 ) ) ;
#8043 = ADVANCED_FACE ( 'NONE', ( #75741 ), #31100, .F. ) ;
#8044 = CARTESIAN_POINT ( 'NONE',  ( -1.660104986876639543, -0.05778040916215560624, -0.4822834645669293319 ) ) ;
#8045 = CARTESIAN_POINT ( 'NONE',  ( -0.6627296587926501115, 0.2952755905511810774, -0.1292274648535930714 ) ) ;
#8046 = DIRECTION ( 'NONE',  ( 0.000000000000000000, 0.000000000000000000, 1.000000000000000000 ) ) ;
#8048 = CARTESIAN_POINT ( 'NONE',  ( 0.8070866141732288002, 0.1660481256975885056, 0.3530559997133364547 ) ) ;
#8047 = LINE ( 'NONE', #72433, #37908 ) ;
#8049 = CARTESIAN_POINT ( 'NONE',  ( 0.7808398950131241190, -0.05778040916215560624, -0.4822834645669293319 ) ) ;
#8050 = CARTESIAN_POINT ( 'NONE',  ( 0.3392501089628018329, 0.1958661417322835607, -2.485564304461941987 ) ) ;
#8051 = CARTESIAN_POINT ( 'NONE',  ( 1.522309711286089939, -0.6046776061558809534, -0.2411417322834644161 ) ) ;
#8052 = CARTESIAN_POINT ( 'NONE',  ( -1.213910761154854745, 0.2952755905511810774, -0.1292274648535930714 ) ) ;
#8053 = CARTESIAN_POINT ( 'NONE',  ( 4.893765752498283924E-17, -0.3996062992125986035, -0.2362204724409449341 ) ) ;
#8055 = ADVANCED_FACE ( 'NONE', ( #5842 ), #69002, .F. ) ;
#8054 = ORIENTED_EDGE ( 'NONE', *, *, #7798, .T. ) ;
#8056 = CARTESIAN_POINT ( 'NONE',  ( -0.3674540682414689785, 0.1283753931104748280, 0.1820866141732283561 ) ) ;
#8057 = CARTESIAN_POINT ( 'NONE',  ( -0.1958661417322834220, -0.3392501089628018884, -1.790026246719160330 ) ) ;
#8058 = ORIENTED_EDGE ( 'NONE', *, *, #54557, .F. ) ;
#8059 = CARTESIAN_POINT ( 'NONE',  ( 0.2821522309711292364, -0.6692913385826771977, 0.1292274648535927661 ) ) ;
#8060 = CARTESIAN_POINT ( 'NONE',  ( 0.1115485564304467270, -0.6692913385826773087, -0.1292274648535924053 ) ) ;
#8061 = CARTESIAN_POINT ( 'NONE',  ( -0.6102362204724400829, -0.5400638737290845981, -0.3530559997133363437 ) ) ;
#8062 = CARTESIAN_POINT ( 'NONE',  ( 1.496062992125985147, -0.1870078740157479769, 0.4822834645669291653 ) ) ;
#8063 = CARTESIAN_POINT ( 'NONE',  ( -1.010498687664041384, -0.004921259842519576551, 0.3153832671262227771 ) ) ;
#8064 = CARTESIAN_POINT ( 'NONE',  ( 0.04057826866093373203, 1.064724180150604216, -1.477648957518036710 ) ) ;
#8065 = CARTESIAN_POINT ( 'NONE',  ( 0.9383202099737538715, -0.05778040916215560624, -0.4822834645669293319 ) ) ;
#8066 = CARTESIAN_POINT ( 'NONE',  ( 0.5446194225721792126, -0.08942795157528024563, -0.3641732283464568787 ) ) ;
#8067 = CARTESIAN_POINT ( 'NONE',  ( -0.2952755905511803003, -0.5400638737290845981, -0.3530559997133363437 ) ) ;
#8068 = CARTESIAN_POINT ( 'NONE',  ( 0.2867679344610365999, 0.2867679344610365999, -1.320190657971441528 ) ) ;
#8069 = CARTESIAN_POINT ( 'NONE',  ( -0.6692913385826764205, 0.2952755905511811885, 0.000000000000000000 ) ) ;
#8070 = CARTESIAN_POINT ( 'NONE',  ( -1.581364829396324945, -0.2845877964562159024, 0.3641732283464567677 ) ) ;
#8071 = CARTESIAN_POINT ( 'NONE',  ( 1.338582677165355062, -0.1870078740157479769, 0.4822834645669291653 ) ) ;
#8072 = CARTESIAN_POINT ( 'NONE',  ( -0.4734688692632945672, 1.503144958756605698, -2.167784222423876805 ) ) ;
#8073 = ORIENTED_EDGE ( 'NONE', *, *, #52442, .T. ) ;
#8074 = CARTESIAN_POINT ( 'NONE',  ( -0.1958661417322836995, 0.3392501089628017219, -2.372066559876327307 ) ) ;
#8075 = CARTESIAN_POINT ( 'NONE',  ( 0.1837270341207357105, -0.6046776061558809534, -0.2411417322834644161 ) ) ;
#8076 = ORIENTED_EDGE ( 'NONE', *, *, #32566, .F. ) ;
#8077 = CARTESIAN_POINT ( 'NONE',  ( -1.174540682414697335, -0.3162353388693409650, -0.4822834645669289433 ) ) ;
#8078 = CARTESIAN_POINT ( 'NONE',  ( 1.377952755905512472, -0.6692913385826771977, 8.415575281601705876E-17 ) ) ;
#8079 = CARTESIAN_POINT ( 'NONE',  ( 1.194225721784777594, -0.4281496062992127816, -0.4176697321401328100 ) ) ;
#8080 = CARTESIAN_POINT ( 'NONE',  ( 0.2821522309711292364, -0.6692913385826771977, 0.1292274648535927661 ) ) ;
#8081 = CARTESIAN_POINT ( 'NONE',  ( -0.2952755905511803003, -0.5400638737290845981, -0.3530559997133363437 ) ) ;
#8082 = CARTESIAN_POINT ( 'NONE',  ( -0.2867679344610365999, 0.2867679344610364889, -1.836614173228346747 ) ) ;
#8083 = CARTESIAN_POINT ( 'NONE',  ( -1.240157480314959759, 0.1660481256975885056, 0.3530559997133364547 ) ) ;
#8084 = CARTESIAN_POINT ( 'NONE',  ( -0.5446194225721777693, -0.05778040916215522460, 0.4822834645669289988 ) ) ;
#8085 = CARTESIAN_POINT ( 'NONE',  ( -0.6167979002624665030, -0.3690944881889765550, -0.3153832671262227771 ) ) ;
#8086 = CARTESIAN_POINT ( 'NONE',  ( 1.614173228346457378, -0.6692913385826771977, 8.415575281601705876E-17 ) ) ;
#8087 = CARTESIAN_POINT ( 'NONE',  ( -0.6496062992125976043, -0.5400638737290844871, 0.3530559997133364547 ) ) ;
#8088 = CARTESIAN_POINT ( 'NONE',  ( -0.5314960629921395840, 2.716830163678111365, 3.890345922373657839 ) ) ;
#8089 = CARTESIAN_POINT ( 'NONE',  ( 0.5839895013123367340, -0.6692913385826773087, -0.1292274648535924053 ) ) ;
#8090 = LINE ( 'NONE', #7242, #77886 ) ;
#8091 = CARTESIAN_POINT ( 'NONE',  ( 0.05249343832021075018, -0.6046776061558807314, 0.2411417322834647770 ) ) ;
#8092 = CARTESIAN_POINT ( 'NONE',  ( -0.1246719160104980823, 0.1771653543307087630, 0.09757992244046791164 ) ) ;
#8094 = CARTESIAN_POINT ( 'NONE',  ( 0.6967283859536044233, -4.069555009745408348E-17, -0.3627989612356146698 ) ) ;
#8093 = CARTESIAN_POINT ( 'NONE',  ( 1.161417322834646493, -0.4536011799217367080, 0.2665933059059888421 ) ) ;
#8095 = CARTESIAN_POINT ( 'NONE',  ( 0.4724409448818897572, -0.1265901696524988906, -0.5032808398950130435 ) ) ;
#8096 = CARTESIAN_POINT ( 'NONE',  ( 1.246719160104987623, -0.004921259842519870586, -0.3153832671262229437 ) ) ;
#8097 = CARTESIAN_POINT ( 'NONE',  ( 1.161417322834646271, 0.1660481256975883668, -0.3530559997133364547 ) ) ;
#8098 = CARTESIAN_POINT ( 'NONE',  ( -0.1058382717557503072, 0.3949938075777408852, -0.2408136482939632617 ) ) ;
#8099 = CARTESIAN_POINT ( 'NONE',  ( 0.006561679790026889343, -0.05778040916215522460, 0.4822834645669289988 ) ) ;
#8100 = CARTESIAN_POINT ( 'NONE',  ( -1.509186351706035767, -0.4281496062992124485, 0.4176697321401328655 ) ) ;
#8101 = CARTESIAN_POINT ( 'NONE',  ( 1.607611548556431069, 0.1771653543307087630, 0.09757992244046791164 ) ) ;
#8102 = CARTESIAN_POINT ( 'NONE',  ( -0.2362204724409442680, -0.1870078740157480879, -0.4822834645669291653 ) ) ;
#8103 = CARTESIAN_POINT ( 'NONE',  ( -0.1974969037888706924, 0.3420746716998658843, -0.2473753280839895707 ) ) ;
#8104 = CARTESIAN_POINT ( 'NONE',  ( -1.541994750656167090, -0.5511811023622048555, -0.09757992244046775898 ) ) ;
#8105 = CARTESIAN_POINT ( 'NONE',  ( 0.4265091863517067039, -0.6692913385826773087, -0.1292274648535924053 ) ) ;
#8106 = CARTESIAN_POINT ( 'NONE',  ( 0.8136482939632553313, -0.5023911411419708095, -0.1820866141732282451 ) ) ;
#8107 = CARTESIAN_POINT ( 'NONE',  ( 0.2748794045270251951, 1.142111962221293409, 0.1499919135227574252 ) ) ;
#8108 = CARTESIAN_POINT ( 'NONE',  ( 0.5511811023622055217, -0.1870078740157479769, 0.3641732283464567677 ) ) ;
#8109 = CARTESIAN_POINT ( 'NONE',  ( -1.397637795275589623, -0.5400638737290845981, -0.3530559997133363437 ) ) ;
#8110 = CARTESIAN_POINT ( 'NONE',  ( 4.893765752498283308E-17, -0.3996062992125985480, -0.9429133858267716439 ) ) ;
#8111 = CARTESIAN_POINT ( 'NONE',  ( 1.253280839895013710, -0.05778040916215560624, -0.4822834645669293319 ) ) ;
#8112 = CARTESIAN_POINT ( 'NONE',  ( 0.3392501089628018884, -0.1958661417322834220, -0.7270341207349080292 ) ) ;
#8114 = DIRECTION ( 'NONE',  ( 0.000000000000000000, 1.000000000000000000, 0.000000000000000000 ) ) ;
#8113 = CARTESIAN_POINT ( 'NONE',  ( 0.2887139107611556010, 0.2306618581243847221, -0.2411417322834647770 ) ) ;
#8115 = DIRECTION ( 'NONE',  ( -1.000000000000000000, 0.000000000000000000, 0.000000000000000000 ) ) ;
#8116 = CARTESIAN_POINT ( 'NONE',  ( 0.6430446194225728496, -0.004921259842519576551, 0.3153832671262227771 ) ) ;
#8117 = ADVANCED_FACE ( 'NONE', ( #24782 ), #42899, .F. ) ;
#8118 = CARTESIAN_POINT ( 'NONE',  ( 0.6955380577427828781, -0.4281496062992124485, 0.4176697321401328655 ) ) ;
#8119 = CARTESIAN_POINT ( 'NONE',  ( 0.7210809602247731931, 4.888820689338890882E-16, 0.3464511005275202615 ) ) ;
#8120 = CARTESIAN_POINT ( 'NONE',  ( -0.9251968503937002541, 0.07958543189024085140, 0.2665933059059887866 ) ) ;
#8121 = CARTESIAN_POINT ( 'NONE',  ( -1.187664041994750175, -0.05778040916215560624, -0.4822834645669293319 ) ) ;
#8122 = CARTESIAN_POINT ( 'NONE',  ( -1.732283464566928277, -0.1870078740157479769, 0.4822834645669291653 ) ) ;
#8123 = CARTESIAN_POINT ( 'NONE',  ( 0.3740157480314966754, -0.5400638737290844871, 0.3530559997133364547 ) ) ;
#8124 = CARTESIAN_POINT ( 'NONE',  ( -1.614173228346455824, 0.1771653543307087630, 0.000000000000000000 ) ) ;
#8125 =( BOUNDED_CURVE ( )  B_SPLINE_CURVE ( 2, ( #27115, #46466, #71323, #52778, #78487, #25859, #20811, #13672, #6513, #40168, #38910, #72160, #14515 ),
 .UNSPECIFIED., .F., .F. ) 
 B_SPLINE_CURVE_WITH_KNOTS ( ( 3, 2, 2, 2, 2, 2, 3 ),
 ( 0.4125000000000000333, 0.4166666666666667407, 0.4208333333333333925, 0.4250000000000000444, 0.4291666666666666408, 0.4333333333333333481, 0.4375000000000000000 ),
 .UNSPECIFIED. ) 
 CURVE ( )  GEOMETRIC_REPRESENTATION_ITEM ( )  RATIONAL_B_SPLINE_CURVE ( ( 0.9999999999999995559, 0.9659258262890687563, 1.000000000000000000, 0.9659258262890683122, 1.000000000000000000, 0.9659258262890683122, 1.000000000000000000, 0.9659258262890683122, 1.000000000000000000, 0.9659258262890683122, 1.000000000000000000, 0.9659258262890683122, 1.000000000000000000 ) ) 
 REPRESENTATION_ITEM ( '' )  );
#8126 = CARTESIAN_POINT ( 'NONE',  ( -3.937007874015748143, 1.537401574803149984, -2.901595197523589142E-16 ) ) ;
#8127 = CARTESIAN_POINT ( 'NONE',  ( 0.6167979002624678353, -0.4281496062992124485, 0.4176697321401328655 ) ) ;
#8128 = CARTESIAN_POINT ( 'NONE',  ( 0.1070741851644054776, -0.3996062992125984925, 0.1528871391076114805 ) ) ;
#8129 = LINE ( 'NONE', #59459, #15912 ) ;
#8130 = CARTESIAN_POINT ( 'NONE',  ( 1.397637795275591177, 0.1660481256975883668, -0.3530559997133364547 ) ) ;
#8131 = CARTESIAN_POINT ( 'NONE',  ( -1.430446194225721390, -0.3690944881889763329, 0.3153832671262228327 ) ) ;
#8132 = CARTESIAN_POINT ( 'NONE',  ( 1.030183727034121421, -0.08942795157527998196, 0.3641732283464567121 ) ) ;
#8133 = CARTESIAN_POINT ( 'NONE',  ( -1.450131233595799651, 0.1771653543307087075, -0.09757992244046823083 ) ) ;
#8134 = CARTESIAN_POINT ( 'NONE',  ( -0.7808398950131222316, -0.2845877964562161244, -0.3641732283464567121 ) ) ;
#8135 = CARTESIAN_POINT ( 'NONE',  ( 1.581364829396326277, -0.05778040916215522460, 0.4822834645669289988 ) ) ;
#8136 = CARTESIAN_POINT ( 'NONE',  ( 0.5905511811023629321, -0.5511811023622047445, 6.969142054262312111E-17 ) ) ;
#8137 = CARTESIAN_POINT ( 'NONE',  ( 0.5183727034120741983, -0.6692913385826771977, 0.1292274648535927661 ) ) ;
#8138 = CARTESIAN_POINT ( 'NONE',  ( 1.312335958005249825, 0.2306618581243847221, -0.2411417322834647770 ) ) ;
#8139 = CARTESIAN_POINT ( 'NONE',  ( 0.2559055118110243332, 0.1660481256975885056, 0.3530559997133364547 ) ) ;
#8140 = CARTESIAN_POINT ( 'NONE',  ( 0.3477690288713918276, 0.1771653543307087630, 0.09757992244046791164 ) ) ;
#8141 = CARTESIAN_POINT ( 'NONE',  ( 1.377952755905512472, -0.6692913385826771977, 8.415575281601705876E-17 ) ) ;
#8142 = CARTESIAN_POINT ( 'NONE',  ( 1.403614904275686858E-14, 1.537401574803149984, -3.937007874015761910 ) ) ;
#8143 = CARTESIAN_POINT ( 'NONE',  ( -1.069553805774277722, 0.2952755905511811885, 0.1292274648535926551 ) ) ;
#8144 = CARTESIAN_POINT ( 'NONE',  ( -0.3996062992125985480, -0.1070741851644057135, -0.6758530183727033958 ) ) ;
#8145 = CARTESIAN_POINT ( 'NONE',  ( -0.2835710216259798577, 1.159555538018685716, 0.1328243903749163624 ) ) ;
#8146 = CARTESIAN_POINT ( 'NONE',  ( -0.01968503937007793844, -0.5400638737290844871, 0.3530559997133364547 ) ) ;
#8147 = CARTESIAN_POINT ( 'NONE',  ( -0.8333333333333323711, 0.2952755905511811885, 0.1292274648535926551 ) ) ;
#8148 = CARTESIAN_POINT ( 'NONE',  ( 0.05249343832021075018, 0.2306618581243847221, -0.2411417322834647770 ) ) ;
#8149 = CARTESIAN_POINT ( 'NONE',  ( -0.1070741851644051862, -0.3996062992125987146, -2.434383202099737353 ) ) ;
#8150 = CARTESIAN_POINT ( 'NONE',  ( 0.1058382717557500713, -0.3949938075777409408, -1.975065616797900159 ) ) ;
#8151 = CARTESIAN_POINT ( 'NONE',  ( 0.3917322834645670104, -0.1049643490035303411, -0.7335958005249343383 ) ) ;
#8152 = CARTESIAN_POINT ( 'NONE',  ( 0.4965823432763554757, 1.491030243898183949, 0.5309055118110234117 ) ) ;
#8153 = CARTESIAN_POINT ( 'NONE',  ( -0.7677165354330699465, 0.07958543189024085140, 0.2665933059059887866 ) ) ;
#8154 = CARTESIAN_POINT ( 'NONE',  ( -0.1049643490035302024, -0.3917322834645671215, -1.009186351706036433 ) ) ;
#8155 = CARTESIAN_POINT ( 'NONE',  ( -1.541994750656167090, 0.2952755905511811885, 0.1292274648535926551 ) ) ;
#8156 = CARTESIAN_POINT ( 'NONE',  ( -0.1958661417322836440, 0.3392501089628016664, 0.2218040926847262562 ) ) ;
#8157 = CARTESIAN_POINT ( 'NONE',  ( 0.5183727034120741983, -0.6692913385826771977, 0.1292274648535927661 ) ) ;
#8158 = CARTESIAN_POINT ( 'NONE',  ( -0.5708661417322828946, 0.07958543189024071263, -0.2665933059059888421 ) ) ;
#8159 = CARTESIAN_POINT ( 'NONE',  ( 0.8595800524934390507, -0.05778040916215560624, -0.4822834645669293319 ) ) ;
#8160 = CARTESIAN_POINT ( 'NONE',  ( 0.3280839895013130669, 0.05413385826771666132, 0.4176697321401328100 ) ) ;
#8161 = CARTESIAN_POINT ( 'NONE',  ( 4.194656359284241426E-16, 0.03937007874015747977, 3.405511811023621771 ) ) ;
#8162 = CARTESIAN_POINT ( 'NONE',  ( 0.1070741851644054915, -0.3996062992125986035, -2.447506561679789527 ) ) ;
#8163 = CARTESIAN_POINT ( 'NONE',  ( 0.3392501089628018884, -0.1958661417322833942, -1.046607242291025752 ) ) ;
#8164 = CARTESIAN_POINT ( 'NONE',  ( 1.115485564304462551, -0.4281496062992127816, -0.4176697321401328100 ) ) ;
#8165 = CARTESIAN_POINT ( 'NONE',  ( -0.1049868766404193215, 0.2306618581243847221, -0.2411417322834647770 ) ) ;
#8166 = CARTESIAN_POINT ( 'NONE',  ( -1.614173228346455824, 0.2952755905511811885, 0.000000000000000000 ) ) ;
#8167 = CARTESIAN_POINT ( 'NONE',  ( 0.7349081364829403995, 0.2306618581243848609, 0.2411417322834645549 ) ) ;
#8168 = CARTESIAN_POINT ( 'NONE',  ( 0.1958661417322836440, -0.3392501089628017219, -0.6489501312335959060 ) ) ;
#8169 = CARTESIAN_POINT ( 'NONE',  ( 0.1574803149606306130, -0.1870078740157479769, 0.4822834645669291653 ) ) ;
#8170 = CARTESIAN_POINT ( 'NONE',  ( 0.5708661417322842269, 0.1660481256975885056, 0.3530559997133364547 ) ) ;
#8171 = CARTESIAN_POINT ( 'NONE',  ( -0.1509186351706028884, -0.3162353388693409650, -0.4822834645669289433 ) ) ;
#8172 = CARTESIAN_POINT ( 'NONE',  ( 1.194225721784777594, -0.004921259842519576551, 0.3153832671262227771 ) ) ;
#8173 = CARTESIAN_POINT ( 'NONE',  ( -1.227034120734907585, 0.2952755905511811885, 0.1292274648535926551 ) ) ;
#8174 = CARTESIAN_POINT ( 'NONE',  ( -1.423884514435694859, -0.3162353388693405765, 0.4822834645669290543 ) ) ;
#8175 = CARTESIAN_POINT ( 'NONE',  ( 0.7677165354330716118, -0.5400638737290844871, 0.3530559997133364547 ) ) ;
#8176 = CARTESIAN_POINT ( 'NONE',  ( 0.3527845929030716809, -0.1716039559343439380, -1.929133858267717549 ) ) ;
#8177 = CARTESIAN_POINT ( 'NONE',  ( -0.1049643490035307020, 0.3917322834645669549, -2.045931758530183497 ) ) ;
#8178 = ORIENTED_EDGE ( 'NONE', *, *, #42409, .T. ) ;
#8179 = CARTESIAN_POINT ( 'NONE',  ( 0.2925321140481932369, 0.2925321140481932369, -0.4527559055118109965 ) ) ;
#8180 = VERTEX_POINT ( 'NONE', #63100 ) ;
#8181 = CARTESIAN_POINT ( 'NONE',  ( 1.299212598425197429, -0.6692913385826771977, 8.415575281601705876E-17 ) ) ;
#8182 = CARTESIAN_POINT ( 'NONE',  ( 1.069553805774278610, -0.5511811023622046335, 0.09757992244046803654 ) ) ;
#8183 = CARTESIAN_POINT ( 'NONE',  ( 0.5611900217179910388, 1.223219560026271499E-15, 0.4445507791589056734 ) ) ;
#8184 = CARTESIAN_POINT ( 'NONE',  ( -0.4741693035498695252, 1.520070061304625408, 2.554858552206048738 ) ) ;
#8185 = DIRECTION ( 'NONE',  ( 0.000000000000000000, 0.000000000000000000, -1.000000000000000000 ) ) ;
#8186 = CARTESIAN_POINT ( 'NONE',  ( 0.3917322834645669549, 0.1049643490035304660, -1.311679790026246906 ) ) ;
#8187 = CARTESIAN_POINT ( 'NONE',  ( 1.299212598425197429, 0.2952755905511811885, 0.000000000000000000 ) ) ;
#8188 = CARTESIAN_POINT ( 'NONE',  ( -1.646981627296586703, -0.05778040916215522460, 0.4822834645669289988 ) ) ;
#8189 = CARTESIAN_POINT ( 'NONE',  ( -0.4986876640419942164, -0.6046776061558807314, 0.2411417322834647770 ) ) ;
#8190 = CARTESIAN_POINT ( 'NONE',  ( 1.043307086614173818, -0.5400638737290845981, -0.3530559997133363437 ) ) ;
#8191 = ORIENTED_EDGE ( 'NONE', *, *, #7492, .F. ) ;
#8192 = AXIS2_PLACEMENT_3D ( 'NONE', #30838, #56094, #62415 ) ;
#8193 = CARTESIAN_POINT ( 'NONE',  ( -1.496062992125983815, -0.1870078740157480879, -0.4822834645669291653 ) ) ;
#8194 = FACE_OUTER_BOUND ( 'NONE', #12845, .T. ) ;
#8195 = CARTESIAN_POINT ( 'NONE',  ( 1.161414421331475211, 3.916330350904249524, 5.973313079581512142 ) ) ;
#8196 = CARTESIAN_POINT ( 'NONE',  ( 1.653543307086614789, -0.1870078740157479769, 0.3641732283464567677 ) ) ;
#8197 = FACE_OUTER_BOUND ( 'NONE', #22520, .T. ) ;
#8198 = CARTESIAN_POINT ( 'NONE',  ( -0.7152230971128602510, -0.2845877964562159024, 0.3641732283464567677 ) ) ;
#8199 = EDGE_CURVE ( 'NONE', #32861, #44548, #39071, .T. ) ;
#8200 = CARTESIAN_POINT ( 'NONE',  ( -1.541994750656167090, -0.6692913385826773087, -0.1292274648535924053 ) ) ;
#8201 = CARTESIAN_POINT ( 'NONE',  ( 0.5905511811023629321, 0.2952755905511811885, 0.000000000000000000 ) ) ;
#8202 = VERTEX_POINT ( 'NONE', #69827 ) ;
#8204 = CARTESIAN_POINT ( 'NONE',  ( -0.4061203303035118561, -2.613618158232546091E-15, -0.3464511005275220379 ) ) ;
#8203 = CARTESIAN_POINT ( 'NONE',  ( 1.581364829396326277, -0.3162353388693409650, -0.4822834645669289433 ) ) ;
#8205 = CARTESIAN_POINT ( 'NONE',  ( -0.8727034120734901146, -0.08942795157528024563, -0.3641732283464568787 ) ) ;
#8206 = CARTESIAN_POINT ( 'NONE',  ( 0.8333333333333340365, -0.6692913385826771977, 0.1292274648535927661 ) ) ;
#8207 = CARTESIAN_POINT ( 'NONE',  ( -1.535433070866141225, 0.2952755905511811885, 0.000000000000000000 ) ) ;
#8208 = CARTESIAN_POINT ( 'NONE',  ( 0.3917322834645668994, 0.1049643490035304522, -1.307067298391389354 ) ) ;
#8209 = CARTESIAN_POINT ( 'NONE',  ( -0.7217847769028863381, -0.004921259842519870586, -0.3153832671262229437 ) ) ;
#8210 = CARTESIAN_POINT ( 'NONE',  ( 1.594488188976378673, -0.5400638737290845981, -0.3530559997133363437 ) ) ;
#8211 = CARTESIAN_POINT ( 'NONE',  ( 4.797336870675656522E-17, -0.3917322834645670104, -1.108267716535433101 ) ) ;
#8212 = CARTESIAN_POINT ( 'NONE',  ( 0.5314960629921264834, 0.1660481256975883668, -0.3530559997133364547 ) ) ;
#8213 = CARTESIAN_POINT ( 'NONE',  ( -0.9514435695538050464, -0.08942795157528024563, -0.3641732283464568787 ) ) ;
#8214 = CARTESIAN_POINT ( 'NONE',  ( -0.5249343832020990641, -0.5023911411419708095, -0.1820866141732282451 ) ) ;
#8215 = AXIS2_PLACEMENT_3D ( 'NONE', #23552, #79591, #61860 ) ;
#8216 = CARTESIAN_POINT ( 'NONE',  ( -0.1377952755905504645, 0.1660481256975885056, 0.3530559997133364547 ) ) ;
#8217 = CARTESIAN_POINT ( 'NONE',  ( -1.187664041994749731, -0.2845877964562159024, 0.3641732283464567677 ) ) ;
#8218 = CARTESIAN_POINT ( 'NONE',  ( 0.2867679344610366554, 0.2867679344610366554, -0.1345337514773772281 ) ) ;
#8219 = CARTESIAN_POINT ( 'NONE',  ( 0.7349081364829402885, -0.6046776061558809534, -0.2411417322834644161 ) ) ;
#8220 = CARTESIAN_POINT ( 'NONE',  ( 0.4091458600556404646, -0.2362204724409448231, -0.2624671916010498651 ) ) ;
#8221 = CARTESIAN_POINT ( 'NONE',  ( -1.157146581871515012E-16, 0.4724409448818898682, -1.809055118110236560 ) ) ;
#8222 = CARTESIAN_POINT ( 'NONE',  ( -0.8530183727034112984, -0.4281496062992127816, -0.4176697321401328100 ) ) ;
#8223 = CARTESIAN_POINT ( 'NONE',  ( -0.1574803149606292529, -0.1870078740157479769, 0.3641732283464567677 ) ) ;
#8224 = CARTESIAN_POINT ( 'NONE',  ( -1.266404199475064773, -0.05778040916215560624, -0.4822834645669293319 ) ) ;
#8225 = CARTESIAN_POINT ( 'NONE',  ( 0.6692913385826778638, -0.5511811023622047445, 6.969142054262312111E-17 ) ) ;
#8226 = CARTESIAN_POINT ( 'NONE',  ( -0.8202099737532801971, -0.5511811023622046335, 0.09757992244046803654 ) ) ;
#8227 = CARTESIAN_POINT ( 'NONE',  ( -1.043307086614172707, 0.1660481256975883668, -0.3530559997133364547 ) ) ;
#8228 = CARTESIAN_POINT ( 'NONE',  ( -1.673228346456691717, 0.1660481256975883668, -0.3530559997133364547 ) ) ;
#8229 = CARTESIAN_POINT ( 'NONE',  ( -1.535433070866141225, -0.6692913385826771977, 8.415575281601705876E-17 ) ) ;
#8230 = CARTESIAN_POINT ( 'NONE',  ( 1.069553805774278832, 0.2066929133858267098, -0.1054918080437494132 ) ) ;
#8231 = CARTESIAN_POINT ( 'NONE',  ( 0.7611548556430454138, 0.1283753931104746893, -0.1820866141732285504 ) ) ;
#8232 = CARTESIAN_POINT ( 'NONE',  ( 0.3412073490813655186, -0.6046776061558809534, -0.2411417322834644161 ) ) ;
#8233 = CARTESIAN_POINT ( 'NONE',  ( -1.653543307086613234, -0.1870078740157479769, 0.4822834645669291653 ) ) ;
#8234 = CARTESIAN_POINT ( 'NONE',  ( 1.253280839895013710, -0.2845877964562159024, 0.3641732283464567677 ) ) ;
#8235 = ORIENTED_EDGE ( 'NONE', *, *, #75011, .T. ) ;
#8236 = CARTESIAN_POINT ( 'NONE',  ( -0.3460692066303957537, -0.1998031496062994405, -2.648950131233595684 ) ) ;
#8237 = CARTESIAN_POINT ( 'NONE',  ( -1.259842519685038686, -0.1870078740157480601, -0.3641732283464567677 ) ) ;
#8238 = CARTESIAN_POINT ( 'NONE',  ( -0.5314960629921250401, 0.1660481256975885056, 0.3530559997133364547 ) ) ;
#8239 = CARTESIAN_POINT ( 'NONE',  ( 0.1377952755905518800, -0.5400638737290844871, 0.3530559997133364547 ) ) ;
#8240 = CARTESIAN_POINT ( 'NONE',  ( -1.620734908136482577, -0.5511811023622048555, -0.09757992244046775898 ) ) ;
#8241 = CARTESIAN_POINT ( 'NONE',  ( -0.1998031496062994405, 0.3460692066303957537, -1.822178477690288956 ) ) ;
#8242 = CARTESIAN_POINT ( 'NONE',  ( -1.272965879265091305, -0.4281496062992124485, 0.4176697321401328655 ) ) ;
#8243 = CARTESIAN_POINT ( 'NONE',  ( 0.4658792650918641698, -0.05778040916215560624, -0.4822834645669293319 ) ) ;
#8244 = B_SPLINE_CURVE_WITH_KNOTS ( 'NONE', 3,
 ( #18218, #75470, #70798, #18623, #30829, #81790, #57730, #43853, #50994, #62831, #82600, #82196, #5165, #37146, #50181, #56494, #32069, #11492, #36729, #45094, #56085, #62405, #24917, #24513, #44266, #77111, #4744, #19444, #51409, #75876, #69957, #24101, #49770, #69556, #17810, #11904, #5572, #93, #43443, #76692 ),
 .UNSPECIFIED., .F., .F.,
 ( 4, 2, 2, 2, 2, 2, 2, 2, 2, 2, 2, 2, 2, 2, 2, 2, 2, 2, 2, 4 ),
 ( 0.01443715752414749011, 0.01533768712752721711, 0.01623821673090694584, 0.01713874633428667110, 0.01803927593766639637, 0.01893980554104612163, 0.01984033514442585036, 0.02029059994611567483, 0.02074086474780550277, 0.02119112954949533070, 0.02164139435118515864, 0.02254192395456481104, 0.02344245355794446345, 0.02434298316132411932, 0.02524351276470376826, 0.02614404236808342413, 0.02659430716977325207, 0.02704457197146308001, 0.02794510157484273241, 0.02884563117822238482 ),
 .UNSPECIFIED. ) ;
#8245 = CARTESIAN_POINT ( 'NONE',  ( 0.3149606299212606708, -0.1870078740157480879, -0.4822834645669291653 ) ) ;
#8246 = CARTESIAN_POINT ( 'NONE',  ( 1.023622047244095112, -0.1870078740157480879, -0.4822834645669291653 ) ) ;
#8247 = CARTESIAN_POINT ( 'NONE',  ( -0.3983403474834782965, -0.03178304480584832892, -1.220472440944881942 ) ) ;
#8248 = CARTESIAN_POINT ( 'NONE',  ( -0.1070741851644056997, 0.3996062992125986035, -1.423884514435695525 ) ) ;
#8249 = CARTESIAN_POINT ( 'NONE',  ( -0.1974969037888703871, -0.3420746716998661063, -0.5380577427821522374 ) ) ;
#8250 = LINE ( 'NONE', #40231, #37397 ) ;
#8251 = CARTESIAN_POINT ( 'NONE',  ( 0.1115485564304467270, -0.5511811023622048555, -0.09757992244046775898 ) ) ;
#8252 = VECTOR ( 'NONE', #78653, 39.37007874015748143 ) ;
#8253 = CARTESIAN_POINT ( 'NONE',  ( -0.1246719160104980823, 0.2952755905511811885, 0.1292274648535926551 ) ) ;
#8254 = CARTESIAN_POINT ( 'NONE',  ( 1.318897637795276356, 0.1660481256975883668, -0.3530559997133364547 ) ) ;
#8255 = CARTESIAN_POINT ( 'NONE',  ( -0.2891555358219909388, -0.2891555358219912164, -1.710629921259842590 ) ) ;
#8256 = CARTESIAN_POINT ( 'NONE',  ( 0.01312335958005323398, -0.3690944881889765550, -0.3153832671262227771 ) ) ;
#8257 = CARTESIAN_POINT ( 'NONE',  ( -1.345144356955379816, -0.3162353388693405765, 0.4822834645669290543 ) ) ;
#8258 = CARTESIAN_POINT ( 'NONE',  ( 1.555118110236221041, -0.5400638737290844871, 0.3530559997133364547 ) ) ;
#8259 = CARTESIAN_POINT ( 'NONE',  ( 0.5971128608923891301, 0.2952755905511810774, -0.1292274648535930714 ) ) ;
#8260 = CARTESIAN_POINT ( 'NONE',  ( -0.1265901696524993347, 0.4724409448818895907, -2.211286089238845065 ) ) ;
#8261 = CARTESIAN_POINT ( 'NONE',  ( 0.3902087894128212775, 0.03611438844014681904, -2.755905511811024944 ) ) ;
#8262 = ORIENTED_EDGE ( 'NONE', *, *, #22956, .T. ) ;
#8263 = ORIENTED_EDGE ( 'NONE', *, *, #80947, .F. ) ;
#8264 = CARTESIAN_POINT ( 'NONE',  ( -1.594488188976377563, -0.5400638737290844871, 0.3530559997133364547 ) ) ;
#8266 = CARTESIAN_POINT ( 'NONE',  ( -1.318897637795274802, 0.1660481256975885056, 0.3530559997133364547 ) ) ;
#8265 = CARTESIAN_POINT ( 'NONE',  ( -1.266404199475064773, -0.08942795157528024563, -0.3641732283464568787 ) ) ;
#8267 = CARTESIAN_POINT ( 'NONE',  ( 0.3917322834645669549, 2.398668435337827645E-17, -2.402867823325772090 ) ) ;
#8268 = CARTESIAN_POINT ( 'NONE',  ( 0.2061694042878472188, -0.2114133405073580219, 0.1284558427095352229 ) ) ;
#8269 = CARTESIAN_POINT ( 'NONE',  ( -1.561679790026246017, -0.3690944881889765550, -0.3153832671262227771 ) ) ;
#8270 = CARTESIAN_POINT ( 'NONE',  ( -1.161417322834644716, -0.5400638737290845981, -0.3530559997133363437 ) ) ;
#8271 = CARTESIAN_POINT ( 'NONE',  ( 0.03937007874015806264, 0.2952755905511811885, 0.000000000000000000 ) ) ;
#8272 = CARTESIAN_POINT ( 'NONE',  ( -1.194225721784776262, -0.4281496062992124485, 0.4176697321401328655 ) ) ;
#8273 = CARTESIAN_POINT ( 'NONE',  ( -9.594673741351310580E-17, 0.3917322834645669549, -2.757198531987190115 ) ) ;
#8274 = CARTESIAN_POINT ( 'NONE',  ( 0.5249343832021003964, 0.2306618581243847221, -0.2411417322834647770 ) ) ;
#8275 = CARTESIAN_POINT ( 'NONE',  ( -0.1049643490035302024, -0.3917322834645671215, -1.954068241469816503 ) ) ;
#8276 = CARTESIAN_POINT ( 'NONE',  ( -1.227034120734907141, -0.5511811023622048555, -0.09757992244046775898 ) ) ;
#8277 = ORIENTED_EDGE ( 'NONE', *, *, #17800, .T. ) ;
#8278 = CARTESIAN_POINT ( 'NONE',  ( -0.2891555358219911054, 0.2891555358219909388, -2.381889763779527769 ) ) ;
#8279 = ORIENTED_EDGE ( 'NONE', *, *, #49168, .F. ) ;
#8280 = CARTESIAN_POINT ( 'NONE',  ( 1.220472440944882386, 0.000000000000000000, 0.000000000000000000 ) ) ;
#8281 = CARTESIAN_POINT ( 'NONE',  ( -1.030183727034119867, -0.05778040916215560624, -0.4822834645669293319 ) ) ;
#8282 = CARTESIAN_POINT ( 'NONE',  ( -1.194225721784776262, -0.4281496062992124485, 0.4176697321401328655 ) ) ;
#8283 = CARTESIAN_POINT ( 'NONE',  ( 0.3460692066303959757, -0.1998031496062991907, -0.4199475065616797842 ) ) ;
#8284 = CARTESIAN_POINT ( 'NONE',  ( -1.391076115485563758, 0.2306618581243848609, 0.2411417322834645549 ) ) ;
#8285 = CARTESIAN_POINT ( 'NONE',  ( -1.528871391076114250, 0.2952755905511810774, -0.1292274648535930714 ) ) ;
#8286 = CARTESIAN_POINT ( 'NONE',  ( -1.443569553805773564, 0.2306618581243847221, -0.2411417322834647770 ) ) ;
#8287 = CARTESIAN_POINT ( 'NONE',  ( 1.614173228346456712, 2.401574803149606474, 0.1372047244094478646 ) ) ;
#8288 = CARTESIAN_POINT ( 'NONE',  ( 0.3392501089628018329, 0.1958661417322835607, -0.2158792650918636147 ) ) ;
#8289 = CARTESIAN_POINT ( 'NONE',  ( 0.2296587926509192634, -0.2845877964562159024, 0.3641732283464567677 ) ) ;
#8290 = CARTESIAN_POINT ( 'NONE',  ( 0.1049643490035303689, 0.3917322834645670104, -0.7080052493438320216 ) ) ;
#8291 = CARTESIAN_POINT ( 'NONE',  ( -0.5905511811023615998, 0.1771653543307087630, 0.000000000000000000 ) ) ;
#8292 = CARTESIAN_POINT ( 'NONE',  ( -1.069553805774277722, -0.6692913385826773087, -0.1292274648535924053 ) ) ;
#8293 = CARTESIAN_POINT ( 'NONE',  ( 1.076115485564305141, -0.6046776061558807314, 0.2411417322834647770 ) ) ;
#8294 = CARTESIAN_POINT ( 'NONE',  ( -0.9383202099737524282, -0.3162353388693409650, -0.4822834645669289433 ) ) ;
#8295 = CARTESIAN_POINT ( 'NONE',  ( 0.5314960629921394730, 2.736617272820978108, -3.873860110281695412 ) ) ;
#8296 = ORIENTED_EDGE ( 'NONE', *, *, #45555, .F. ) ;
#8297 = CARTESIAN_POINT ( 'NONE',  ( -0.9514435695538050464, -0.05778040916215560624, -0.4822834645669293319 ) ) ;
#8298 = CARTESIAN_POINT ( 'NONE',  ( 0.9383202099737536495, -0.3162353388693405765, 0.4822834645669290543 ) ) ;
#8299 = CARTESIAN_POINT ( 'NONE',  ( -1.699475065616797398, 0.1771653543307087630, 0.09757992244046791164 ) ) ;
#8300 = CARTESIAN_POINT ( 'NONE',  ( -1.732283464566928277, -0.1870078740157479769, 0.4822834645669291653 ) ) ;
#8301 = CARTESIAN_POINT ( 'NONE',  ( 0.3458507752293908943, 0.3458507752293908943, -1.240157480314960647 ) ) ;
#8302 = CARTESIAN_POINT ( 'NONE',  ( 1.857294464233405273, 1.070443199938752699, 0.08545185031211080529 ) ) ;
#8303 = ADVANCED_FACE ( 'NONE', ( #68593 ), #12176, .F. ) ;
#8304 = CARTESIAN_POINT ( 'NONE',  ( -0.2867679344610365999, 0.2867679344610364889, -0.4842519685039369248 ) ) ;
#8305 = CARTESIAN_POINT ( 'NONE',  ( -0.3917322834645669549, -0.1049643490035306603, -2.492782152230970993 ) ) ;
#8306 = CARTESIAN_POINT ( 'NONE',  ( -0.2296587926509179312, -0.05778040916215522460, 0.4822834645669289988 ) ) ;
#8307 = CARTESIAN_POINT ( 'NONE',  ( -1.653543307086613234, -0.1870078740157479769, 0.3641732283464567677 ) ) ;
#8308 = CARTESIAN_POINT ( 'NONE',  ( 0.1998031496062992463, 0.3460692066303959202, 0.09383202099737530943 ) ) ;
#8310 = DIRECTION ( 'NONE',  ( 1.000000000000000000, -0.000000000000000000, -0.000000000000000000 ) ) ;
#8309 = CARTESIAN_POINT ( 'NONE',  ( -1.437007874015747477, -0.5400638737290844871, 0.3530559997133364547 ) ) ;
#8311 = CARTESIAN_POINT ( 'NONE',  ( -1.253280839895012377, -0.05778040916215522460, 0.4822834645669289988 ) ) ;
#8312 = CARTESIAN_POINT ( 'NONE',  ( -0.2165354330708654795, -0.5400638737290845981, -0.3530559997133363437 ) ) ;
#8313 = CARTESIAN_POINT ( 'NONE',  ( 4.837279021331061486E-17, -0.3949938075777409963, -2.675196850393700920 ) ) ;
#8314 = CARTESIAN_POINT ( 'NONE',  ( 0.6299212598425204535, -0.1870078740157479769, 0.3641732283464567677 ) ) ;
#8315 = DIRECTION ( 'NONE',  ( 1.408710688920637755E-15, -1.000000000000000000, 4.918487082195260922E-30 ) ) ;
#8316 = CARTESIAN_POINT ( 'NONE',  ( 0.3740157480314966754, -0.4536011799217367080, 0.2665933059059888421 ) ) ;
#8317 = CARTESIAN_POINT ( 'NONE',  ( 1.305774278215223960, 0.1771653543307087075, -0.09757992244046823083 ) ) ;
#8318 = COLOUR_RGB ( '', 0.72549020, 0.75294118, 0.79215686) ;
#8319 = CARTESIAN_POINT ( 'NONE',  ( 0.7545931758530188826, -0.6692913385826771977, 0.1292274648535927661 ) ) ;
#8320 = CARTESIAN_POINT ( 'NONE',  ( -0.03937007874015669567, 0.1771653543307087630, 0.000000000000000000 ) ) ;
#8321 = CARTESIAN_POINT ( 'NONE',  ( -0.3392501089628019995, 0.1958661417322832277, -2.065616797900262647 ) ) ;
#8322 = CARTESIAN_POINT ( 'NONE',  ( -1.272965879265091305, 0.05413385826771626580, -0.4176697321401330321 ) ) ;
#8323 = CARTESIAN_POINT ( 'NONE',  ( 0.1049868766404206816, -0.5023911411419708095, -0.1820866141732282451 ) ) ;
#8324 = CARTESIAN_POINT ( 'NONE',  ( -1.364829396325458521, -0.5023911411419708095, 0.1820866141732285504 ) ) ;
#8325 = CARTESIAN_POINT ( 'NONE',  ( 0.4091458600556403535, 0.2362204724409449896, -0.2080052493438320216 ) ) ;
#8326 = CARTESIAN_POINT ( 'NONE',  ( -0.3740157480314953431, 0.07958543189024085140, 0.2665933059059887866 ) ) ;
#8327 = CARTESIAN_POINT ( 'NONE',  ( 0.4492688262921352149, 1.384998324914241019, -1.544058616794434791 ) ) ;
#8328 = CARTESIAN_POINT ( 'NONE',  ( -0.2296587926509179312, -0.05778040916215522460, 0.4822834645669289988 ) ) ;
#8329 = CARTESIAN_POINT ( 'NONE',  ( 0.1265901696524989184, 0.4724409448818898127, -0.7001312335958003175 ) ) ;
#8330 = CARTESIAN_POINT ( 'NONE',  ( 0.6233595800524939223, -0.2845877964562159024, 0.3641732283464567677 ) ) ;
#8331 = CARTESIAN_POINT ( 'NONE',  ( -0.08530183727034056085, -0.08942795157528024563, -0.3641732283464568787 ) ) ;
#8332 = CARTESIAN_POINT ( 'NONE',  ( -0.4199475065616791736, -0.6046776061558807314, 0.2411417322834647770 ) ) ;
#8333 = FACE_OUTER_BOUND ( 'NONE', #43661, .T. ) ;
#8334 = CARTESIAN_POINT ( 'NONE',  ( -1.023622047244093558, -0.1870078740157479769, 0.3641732283464567677 ) ) ;
#8335 = CYLINDRICAL_SURFACE ( 'NONE', #27379, 0.3937007874015748254 ) ;
#8336 = EDGE_CURVE ( 'NONE', #54436, #17596, #44540, .T. ) ;
#8337 = CARTESIAN_POINT ( 'NONE',  ( 0.5118110236220480003, -0.6692913385826771977, 8.415575281601705876E-17 ) ) ;
#8338 = CARTESIAN_POINT ( 'NONE',  ( -0.9645669291338575535, 0.1660481256975883668, -0.3530559997133364547 ) ) ;
#8339 = CARTESIAN_POINT ( 'NONE',  ( -0.3996062992125985480, -7.340648628747423112E-17, -1.375984251968503713 ) ) ;
#8340 = CARTESIAN_POINT ( 'NONE',  ( -0.3392501089628019995, 0.1958661417322832277, -2.788057742782152459 ) ) ;
#8341 = CARTESIAN_POINT ( 'NONE',  ( -0.07217847769028813698, -0.2845877964562161244, -0.3641732283464567121 ) ) ;
#8342 = CARTESIAN_POINT ( 'NONE',  ( -1.338582677165353729, -0.1870078740157479769, 0.4822834645669291653 ) ) ;
#8343 = CARTESIAN_POINT ( 'NONE',  ( 1.541994750656168645, 0.2952755905511810774, -0.1292274648535930714 ) ) ;
#8344 = CARTESIAN_POINT ( 'NONE',  ( -0.3149606299212460159, 2.755905511811024056, -3.924389226575469625 ) ) ;
#8345 = CARTESIAN_POINT ( 'NONE',  ( -0.5052493438320203589, -0.5511811023622046335, 0.09757992244046803654 ) ) ;
#8346 = CARTESIAN_POINT ( 'NONE',  ( 0.4606732211681152100, 1.541615089183626441, 0.5309055118110234117 ) ) ;
#8347 = CARTESIAN_POINT ( 'NONE',  ( 0.7742782152230978099, -0.4281496062992124485, 0.4176697321401328655 ) ) ;
#8348 = CARTESIAN_POINT ( 'NONE',  ( 0.1070741851644054915, -0.3996062992125986035, -0.08530183727034119923 ) ) ;
#8349 = CARTESIAN_POINT ( 'NONE',  ( 0.3917322834645670659, 2.398668435337828261E-17, -2.319573121556117279 ) ) ;
#8350 = CARTESIAN_POINT ( 'NONE',  ( 0.4670044181572728936, 1.622388320715301147, -2.571776478002881561 ) ) ;
#8351 = CARTESIAN_POINT ( 'NONE',  ( 1.607611548556431069, 0.1771653543307087630, 0.09757992244046791164 ) ) ;
#8352 = CARTESIAN_POINT ( 'NONE',  ( -1.174540682414697335, -0.3162353388693409650, -0.4822834645669289433 ) ) ;
#8353 = CARTESIAN_POINT ( 'NONE',  ( 1.122047244094488860, 0.1660481256975885056, 0.3530559997133364547 ) ) ;
#8354 = CARTESIAN_POINT ( 'NONE',  ( 0.1049643490035304938, -0.3917322834645669549, -2.374671916010498762 ) ) ;
#8355 = CARTESIAN_POINT ( 'NONE',  ( 1.496062992125985147, -0.1870078740157479769, 0.3641732283464567677 ) ) ;
#8356 = ADVANCED_FACE ( 'NONE', ( #4606 ), #43094, .F. ) ;
#8357 = CARTESIAN_POINT ( 'NONE',  ( 0.6824146981627303710, -0.6046776061558807314, 0.2411417322834647770 ) ) ;
#8358 = CARTESIAN_POINT ( 'NONE',  ( -0.4724409448818890911, -0.1870078740157480879, -0.4822834645669291653 ) ) ;
#8359 = CARTESIAN_POINT ( 'NONE',  ( 1.482939632545932307, -0.4281496062992124485, 0.4176697321401328655 ) ) ;
#8360 = CARTESIAN_POINT ( 'NONE',  ( 3.898836503597932435, 2.697992270790282365, 0.5314960629921259283 ) ) ;
#8361 = CARTESIAN_POINT ( 'NONE',  ( 0.8792650918635177559, -0.3690944881889765550, -0.3153832671262227771 ) ) ;
#8362 = EDGE_LOOP ( 'NONE', ( #48731, #59177, #43741, #30607 ) ) ;
#8363 = CARTESIAN_POINT ( 'NONE',  ( -0.3917322834645670659, -7.196005306013484475E-17, -0.3510691845482433182 ) ) ;
#8364 = EDGE_LOOP ( 'NONE', ( #21501, #34901, #37005 ) ) ;
#8365 = CARTESIAN_POINT ( 'NONE',  ( -0.2624671916010490880, 0.2306618581243847221, -0.2411417322834647770 ) ) ;
#8366 = PRODUCT ( 'Spindle Dowel Pin', 'Spindle Dowel Pin', '', ( #30024 ) ) ;
#8367 = CARTESIAN_POINT ( 'NONE',  ( 1.496062992125984703, -0.1870078740157480879, -0.4822834645669291653 ) ) ;
#8368 = CARTESIAN_POINT ( 'NONE',  ( 0.3215223097112867578, -0.3162353388693409650, -0.4822834645669289433 ) ) ;
#8369 = CARTESIAN_POINT ( 'NONE',  ( -0.5249343832020990641, 0.1283753931104748280, 0.1820866141732283561 ) ) ;
#8370 = CARTESIAN_POINT ( 'NONE',  ( 1.233595800524935227, 0.2306618581243847221, -0.2411417322834647770 ) ) ;
#8371 = CARTESIAN_POINT ( 'NONE',  ( -1.017060367454067249, -0.05778040916215522460, 0.4822834645669289988 ) ) ;
#8372 = CARTESIAN_POINT ( 'NONE',  ( 0.03280839895013198948, 0.2952755905511811885, 0.1292274648535926551 ) ) ;
#8373 = CARTESIAN_POINT ( 'NONE',  ( 1.528871391076116026, -0.6692913385826773087, -0.1292274648535924053 ) ) ;
#8374 = AXIS2_PLACEMENT_3D ( 'NONE', #61103, #54789, #80492 ) ;
#8375 = CARTESIAN_POINT ( 'NONE',  ( 0.9448818897637802916, -0.1870078740157479769, 0.4822834645669291653 ) ) ;
#8376 = CARTESIAN_POINT ( 'NONE',  ( 1.364829396325460076, 0.2306618581243848609, 0.2411417322834645549 ) ) ;
#8377 = CARTESIAN_POINT ( 'NONE',  ( -9.594673741351313045E-17, 0.3917322834645670104, -0.7795275590551180578 ) ) ;
#8378 = CARTESIAN_POINT ( 'NONE',  ( 0.1377952755905518800, 0.07958543189024071263, -0.2665933059059888421 ) ) ;
#8379 = EDGE_LOOP ( 'NONE', ( #39070, #16362, #34965, #30302 ) ) ;
#8380 = CARTESIAN_POINT ( 'NONE',  ( 0.3420746716998659953, 0.1974969037888705536, -0.9186351706036742781 ) ) ;
#8381 = EDGE_LOOP ( 'NONE', ( #22954, #58872, #54936, #35606 ) ) ;
#8382 = CARTESIAN_POINT ( 'NONE',  ( -0.3346456692913377662, -0.4536011799217367080, 0.2665933059059888421 ) ) ;
#8383 = CARTESIAN_POINT ( 'NONE',  ( 8.195543980992789655E-16, -0.1870078740157480879, -0.4822834645669291653 ) ) ;
#8384 = CARTESIAN_POINT ( 'NONE',  ( -1.559171609364246924, 0.3937007874015748254, 0.4177787735906735578 ) ) ;
#8385 = CARTESIAN_POINT ( 'NONE',  ( -0.3412073490813641308, -0.6046776061558807314, 0.2411417322834647770 ) ) ;
#8386 = CARTESIAN_POINT ( 'NONE',  ( -0.3805774278215216522, -0.4281496062992127816, -0.4176697321401328100 ) ) ;
#8387 = CARTESIAN_POINT ( 'NONE',  ( -0.7349081364829387342, -0.6046776061558807314, 0.2411417322834647770 ) ) ;
#8388 = CARTESIAN_POINT ( 'NONE',  ( -1.043307086614172707, 0.1660481256975883668, -0.3530559997133364547 ) ) ;
#8389 = CARTESIAN_POINT ( 'NONE',  ( 1.548556430446194954, 0.1283753931104746893, -0.1820866141732285504 ) ) ;
#8390 = CARTESIAN_POINT ( 'NONE',  ( -3.937007874015748143, 2.165354330708661568, -0.3149606299212600047 ) ) ;
#8391 = CARTESIAN_POINT ( 'NONE',  ( 0.1341536278048623965, 1.050682278017460725, 0.2827841492639507348 ) ) ;
#8392 = CARTESIAN_POINT ( 'NONE',  ( 0.2690288713910767848, -0.5511811023622048555, -0.09757992244046775898 ) ) ;
#8393 = CARTESIAN_POINT ( 'NONE',  ( 0.6102362204724416372, 0.1660481256975883668, -0.3530559997133364547 ) ) ;
#8394 = CARTESIAN_POINT ( 'NONE',  ( 0.4461942257217856311, 0.2306618581243847221, -0.2411417322834647770 ) ) ;
#8395 = CARTESIAN_POINT ( 'NONE',  ( -0.1998031496062994683, 0.3460692066303958092, -1.272965879265091749 ) ) ;
#8396 = CARTESIAN_POINT ( 'NONE',  ( -2.554262525012223062, 1.546132656481030043, 0.4744094488188971837 ) ) ;
#8397 = CARTESIAN_POINT ( 'NONE',  ( 0.3460692066303959202, -0.1998031496062991630, -0.6541994750656167090 ) ) ;
#8398 = CARTESIAN_POINT ( 'NONE',  ( -0.3460692066303960313, 0.1998031496062989965, -0.7329396325459317518 ) ) ;
#8399 = CARTESIAN_POINT ( 'NONE',  ( -0.4330708661417315697, 0.2952755905511811885, 0.000000000000000000 ) ) ;
#8400 = CARTESIAN_POINT ( 'NONE',  ( -0.4091458600556402980, -0.2362204724409451284, 0.1049868766404199460 ) ) ;
#8401 = CARTESIAN_POINT ( 'NONE',  ( -0.3392501089628019995, 0.1958661417322832277, -2.158136482939632561 ) ) ;
#8402 = CARTESIAN_POINT ( 'NONE',  ( -1.377952755905511140, -0.5511811023622047445, 6.969142054262312111E-17 ) ) ;
#8403 = CARTESIAN_POINT ( 'NONE',  ( 0.8398950131233602345, 0.2306618581243847221, -0.2411417322834647770 ) ) ;
#8404 = CARTESIAN_POINT ( 'NONE',  ( 0.8070866141732289112, -0.5400638737290845981, -0.3530559997133363437 ) ) ;
#8405 = CARTESIAN_POINT ( 'NONE',  ( -0.3215223097112853146, -0.08942795157528024563, -0.3641732283464568787 ) ) ;
#8406 = CARTESIAN_POINT ( 'NONE',  ( 0.4265091863517067039, -0.6692913385826773087, -0.1292274648535924053 ) ) ;
#8407 = CARTESIAN_POINT ( 'NONE',  ( 0.1265901696524990294, -0.4724409448818896462, -2.051837270341206665 ) ) ;
#8408 = CARTESIAN_POINT ( 'NONE',  ( 0.02624671916010564918, -0.5023911411419708095, -0.1820866141732282451 ) ) ;
#8409 = CARTESIAN_POINT ( 'NONE',  ( -0.1640419947506555343, -0.3162353388693405765, 0.4822834645669290543 ) ) ;
#8410 = CARTESIAN_POINT ( 'NONE',  ( -0.3949938075777408852, -0.1058382717557502933, -1.225065616797900159 ) ) ;
#8411 = CARTESIAN_POINT ( 'NONE',  ( 1.607611548556431069, 0.1771653543307087630, 0.09757992244046791164 ) ) ;
#8412 = CARTESIAN_POINT ( 'NONE',  ( 0.6036745406824153282, -0.5023911411419708095, 0.1820866141732285504 ) ) ;
#8413 = CARTESIAN_POINT ( 'NONE',  ( 1.456692913385827515, -0.5511811023622047445, 6.969142054262312111E-17 ) ) ;
#8414 = CARTESIAN_POINT ( 'NONE',  ( -0.7086614173228339419, -0.1870078740157480879, -0.4822834645669291653 ) ) ;
#8415 = CARTESIAN_POINT ( 'NONE',  ( -0.6692913385826764205, 0.1771653543307087630, 0.000000000000000000 ) ) ;
#8416 = LINE ( 'NONE', #2935, #69540 ) ;
#8417 = CARTESIAN_POINT ( 'NONE',  ( -0.5971128608923877978, 0.2952755905511811885, 0.1292274648535926551 ) ) ;
#8418 = CARTESIAN_POINT ( 'NONE',  ( -0.7677165354330699465, -0.5400638737290845981, -0.3530559997133363437 ) ) ;
#8419 = CARTESIAN_POINT ( 'NONE',  ( 0.1443569553805781891, 0.05413385826771626580, -0.4176697321401330321 ) ) ;
#8420 = CARTESIAN_POINT ( 'NONE',  ( 0.3996062992125985480, 2.446882876249141654E-17, -2.557086614173228689 ) ) ;
#8421 = CARTESIAN_POINT ( 'NONE',  ( -0.3392501089628018329, -0.1958661417322836440, -2.022290395504250160 ) ) ;
#8422 = CARTESIAN_POINT ( 'NONE',  ( -1.850419646634100301, 1.063020117359136263, -0.01785754392578375524 ) ) ;
#8423 = CARTESIAN_POINT ( 'NONE',  ( 0.6430446194225729606, -0.3690944881889765550, -0.3153832671262227771 ) ) ;
#8424 = CARTESIAN_POINT ( 'NONE',  ( 1.482939632545932307, 0.05413385826771626580, -0.4176697321401330321 ) ) ;
#8425 = CARTESIAN_POINT ( 'NONE',  ( -1.128608923884513837, -0.5023911411419708095, 0.1820866141732285504 ) ) ;
#8426 = CARTESIAN_POINT ( 'NONE',  ( -1.299212598425196097, -0.5511811023622047445, 6.969142054262312111E-17 ) ) ;
#8427 = VECTOR ( 'NONE', #41525, 39.37007874015748143 ) ;
#8428 = CARTESIAN_POINT ( 'NONE',  ( -0.7217847769028863381, 0.05413385826771626580, -0.4176697321401330321 ) ) ;
#8429 = CARTESIAN_POINT ( 'NONE',  ( -0.05249343832020911260, 0.1283753931104748280, 0.1820866141732283561 ) ) ;
#8430 = CARTESIAN_POINT ( 'NONE',  ( -0.1265901696524986964, -0.4724409448818899238, -0.8595800524934383846 ) ) ;
#8431 = CARTESIAN_POINT ( 'NONE',  ( 0.9317585301837276734, -0.3690944881889763329, 0.3153832671262228327 ) ) ;
#8432 = EDGE_CURVE ( 'NONE', #36021, #65941, #31015, .T. ) ;
#8433 = CARTESIAN_POINT ( 'NONE',  ( 0.2296587926509192634, -0.3162353388693405765, 0.4822834645669290543 ) ) ;
#8434 = CARTESIAN_POINT ( 'NONE',  ( -0.1070741851644056997, 0.3996062992125984925, -0.2408136482939632061 ) ) ;
#8435 = CARTESIAN_POINT ( 'NONE',  ( -0.6889763779527552368, -0.5400638737290845981, -0.3530559997133363437 ) ) ;
#8436 = CARTESIAN_POINT ( 'NONE',  ( 0.3917322834645670104, -0.1049643490035303411, -1.456036745406824151 ) ) ;
#8437 = CARTESIAN_POINT ( 'NONE',  ( 1.489501312335958172, -0.08942795157528024563, -0.3641732283464568787 ) ) ;
#8438 = CARTESIAN_POINT ( 'NONE',  ( 0.3412073490813655186, -0.6046776061558809534, -0.2411417322834644161 ) ) ;
#8439 = CARTESIAN_POINT ( 'NONE',  ( -0.02624671916010428221, 0.2306618581243847221, -0.2411417322834647770 ) ) ;
#8440 = CARTESIAN_POINT ( 'NONE',  ( -0.1574803149606292529, -0.1870078740157480601, -0.3641732283464567677 ) ) ;
#8441 = CARTESIAN_POINT ( 'NONE',  ( 0.6036745406824154392, 0.1539470093639521697, -0.1968503937007875793 ) ) ;
#8442 = CARTESIAN_POINT ( 'NONE',  ( -0.2493438320209966919, -0.3690944881889763329, 0.3153832671262228327 ) ) ;
#8443 = CARTESIAN_POINT ( 'NONE',  ( 0.6692913385826778638, -0.6692913385826771977, 8.415575281601705876E-17 ) ) ;
#8444 = CARTESIAN_POINT ( 'NONE',  ( -0.8595800524934373854, -0.2845877964562161244, -0.3641732283464567121 ) ) ;
#8445 = CARTESIAN_POINT ( 'NONE',  ( 0.2925321140481932369, 0.2925321140481932369, -1.001968503937007871 ) ) ;
#8446 = CARTESIAN_POINT ( 'NONE',  ( -1.141732283464566011, 0.2952755905511811885, 0.000000000000000000 ) ) ;
#8447 = CARTESIAN_POINT ( 'NONE',  ( -1.614173228346456712, 2.362204724409448620, -0.1372047244094478091 ) ) ;
#8448 = ORIENTED_EDGE ( 'NONE', *, *, #24627, .T. ) ;
#8449 = CARTESIAN_POINT ( 'NONE',  ( -1.259842519685038686, -0.1870078740157479769, 0.3641732283464567677 ) ) ;
#8450 = CARTESIAN_POINT ( 'NONE',  ( 0.05249343832021075018, 0.2306618581243847221, -0.2411417322834647770 ) ) ;
#8451 = CARTESIAN_POINT ( 'NONE',  ( -1.469816272965878357, -0.6046776061558809534, -0.2411417322834644161 ) ) ;
#8452 = CARTESIAN_POINT ( 'NONE',  ( -0.9580052493438311334, 0.05413385826771626580, -0.4176697321401330321 ) ) ;
#8453 = CARTESIAN_POINT ( 'NONE',  ( -1.076935383196057749, -5.463695987328518425E-17, 0.3149606299212591720 ) ) ;
#8454 = EDGE_CURVE ( 'NONE', #24205, #6101, #33195, .T. ) ;
#8456 = CARTESIAN_POINT ( 'NONE',  ( 0.9842519685039375910, 0.2952755905511811885, 0.000000000000000000 ) ) ;
#8455 = CARTESIAN_POINT ( 'NONE',  ( 1.587926509186352586, -0.4281496062992127816, -0.4176697321401328100 ) ) ;
#8457 = CARTESIAN_POINT ( 'NONE',  ( 0.8792650918635177559, 0.05413385826771666132, 0.4176697321401328100 ) ) ;
#8458 = CARTESIAN_POINT ( 'NONE',  ( -0.3021879055830032357, 0.004960608223778823628, 0.3437734562760190182 ) ) ;
#8459 = CARTESIAN_POINT ( 'NONE',  ( 1.496062992125984703, -0.1870078740157480879, -0.4822834645669291653 ) ) ;
#8460 = EDGE_CURVE ( 'NONE', #5432, #36021, #7097, .T. ) ;
#8461 = CARTESIAN_POINT ( 'NONE',  ( -1.167979002624671470, -0.4281496062992127816, -0.4176697321401328100 ) ) ;
#8462 = CARTESIAN_POINT ( 'NONE',  ( -0.3460692066303958092, -0.1998031496062994683, -0.3674540682414698112 ) ) ;
#8463 = VERTEX_POINT ( 'NONE', #26457 ) ;
#8464 = CARTESIAN_POINT ( 'NONE',  ( -0.7020997375328074108, -0.08942795157527998196, 0.3641732283464567121 ) ) ;
#8465 = CARTESIAN_POINT ( 'NONE',  ( -0.2867679344610365999, 0.2867679344610364889, -2.059055118110236116 ) ) ;
#8466 = ORIENTED_EDGE ( 'NONE', *, *, #18760, .F. ) ;
#8467 = CARTESIAN_POINT ( 'NONE',  ( 0.4658792650918640033, -0.3162353388693405765, 0.4822834645669290543 ) ) ;
#8468 = CARTESIAN_POINT ( 'NONE',  ( 0.1246719160104994284, -0.6692913385826771977, 0.1292274648535927661 ) ) ;
#8469 = CARTESIAN_POINT ( 'NONE',  ( -0.6364829396325453192, -0.05778040916215560624, -0.4822834645669293319 ) ) ;
#8470 = CARTESIAN_POINT ( 'NONE',  ( 1.371391076115485941, 0.2952755905511811885, 0.1292274648535926551 ) ) ;
#8471 = AXIS2_PLACEMENT_3D ( 'NONE', #49421, #3159, #10725 ) ;
#8472 = CARTESIAN_POINT ( 'NONE',  ( -1.056430446194224881, -0.5511811023622046335, 0.09757992244046803654 ) ) ;
#8473 = CARTESIAN_POINT ( 'NONE',  ( -0.7443564587111910491, 2.208176010582810989, -0.5309055118110235227 ) ) ;
#8474 = CARTESIAN_POINT ( 'NONE',  ( 0.6036745406824154392, 0.2306618581243847221, -0.2411417322834647770 ) ) ;
#8475 = CARTESIAN_POINT ( 'NONE',  ( 0.5643044619422579178, -0.3690944881889765550, -0.3153832671262227771 ) ) ;
#8476 = CARTESIAN_POINT ( 'NONE',  ( -0.5314960629921250401, 0.1660481256975885056, 0.3530559997133364547 ) ) ;
#8477 = CARTESIAN_POINT ( 'NONE',  ( 0.1049643490035303689, 0.3917322834645668994, -1.175833702590864283 ) ) ;
#8478 = CARTESIAN_POINT ( 'NONE',  ( -1.187664041994749731, -0.3162353388693405765, 0.4822834645669290543 ) ) ;
#8479 = CARTESIAN_POINT ( 'NONE',  ( -0.5314960629921122726, 2.755905511811024056, -3.937007874015763687 ) ) ;
#8480 = CARTESIAN_POINT ( 'NONE',  ( 1.259842519685040019, -0.1870078740157480879, -0.4822834645669291653 ) ) ;
#8481 = CARTESIAN_POINT ( 'NONE',  ( 1.272965879265092637, -0.3690944881889765550, -0.3153832671262227771 ) ) ;
#8482 = ORIENTED_EDGE ( 'NONE', *, *, #49112, .T. ) ;
#8483 = CARTESIAN_POINT ( 'NONE',  ( -0.3917322834645670659, -7.196005306013484475E-17, -2.555793593997062629 ) ) ;
#8484 = CARTESIAN_POINT ( 'NONE',  ( 0.09842519685039434474, 0.1660481256975885056, 0.3530559997133364547 ) ) ;
#8485 = ORIENTED_EDGE ( 'NONE', *, *, #75428, .F. ) ;
#8486 = CARTESIAN_POINT ( 'NONE',  ( 0.8727034120734912248, -0.2845877964562161244, -0.3641732283464567121 ) ) ;
#8487 = CARTESIAN_POINT ( 'NONE',  ( -1.017060367454067249, -0.3162353388693409650, -0.4822834645669289433 ) ) ;
#8488 = CARTESIAN_POINT ( 'NONE',  ( 1.122047244094488860, 0.1660481256975885056, 0.3530559997133364547 ) ) ;
#8489 = CARTESIAN_POINT ( 'NONE',  ( 0.8267716535433077274, 0.2952755905511811885, 0.000000000000000000 ) ) ;
#8490 = ADVANCED_FACE ( 'NONE', ( #71495 ), #39501, .T. ) ;
#8491 =( BOUNDED_CURVE ( )  B_SPLINE_CURVE ( 2, ( #58214, #52314, #78021, #72533, #45161, #20769, #13627, #64543, #39279, #27073, #39705, #20349, #580 ),
 .UNSPECIFIED., .F., .F. ) 
 B_SPLINE_CURVE_WITH_KNOTS ( ( 3, 2, 2, 2, 2, 2, 3 ),
 ( 0.4375000000000000000, 0.4416666666666666519, 0.4458333333333334147, 0.4500000000000000666, 0.4541666666666667185, 0.4583333333333334259, 0.4625000000000001332 ),
 .UNSPECIFIED. ) 
 CURVE ( )  GEOMETRIC_REPRESENTATION_ITEM ( )  RATIONAL_B_SPLINE_CURVE ( ( 1.000000000000000000, 0.9659258262890683122, 1.000000000000000000, 0.9659258262890683122, 1.000000000000000000, 0.9659258262890683122, 1.000000000000000000, 0.9659258262890683122, 1.000000000000000000, 0.9659258262890683122, 1.000000000000000000, 0.9659258262890674240, 1.000000000000000888 ) ) 
 REPRESENTATION_ITEM ( '' )  );
#8492 = CARTESIAN_POINT ( 'NONE',  ( 0.1181102362204730916, -0.6692913385826771977, 8.415575281601705876E-17 ) ) ;
#8493 = CARTESIAN_POINT ( 'NONE',  ( -0.5052493438320203589, 0.2952755905511810774, -0.1292274648535930714 ) ) ;
#8494 = CARTESIAN_POINT ( 'NONE',  ( 0.2867679344610365999, 0.2867679344610365999, -1.639763779527558807 ) ) ;
#8495 = CARTESIAN_POINT ( 'NONE',  ( -1.364829396325458521, 0.2306618581243847221, -0.2411417322834647770 ) ) ;
#8496 = CARTESIAN_POINT ( 'NONE',  ( -0.5183727034120726440, 0.2952755905511811885, 0.1292274648535926551 ) ) ;
#8497 = EDGE_CURVE ( 'NONE', #4531, #11477, #58863, .T. ) ;
#8498 = CARTESIAN_POINT ( 'NONE',  ( -0.4986876640419939388, 0.1283753931104746893, -0.1820866141732285504 ) ) ;
#8499 = CARTESIAN_POINT ( 'NONE',  ( -0.05060072268091472814, 0.3900885325447118746, -8.192289201638894699E-18 ) ) ;
#8500 = CARTESIAN_POINT ( 'NONE',  ( 1.476377952755906442, -0.5400638737290844871, 0.3530559997133364547 ) ) ;
#8501 = CARTESIAN_POINT ( 'NONE',  ( -0.5249343832020990641, -0.6046776061558809534, -0.2411417322834644161 ) ) ;
#8502 = CARTESIAN_POINT ( 'NONE',  ( -0.5314960629921395840, 2.729373344522950440, 3.881211926161856507 ) ) ;
#8503 = CARTESIAN_POINT ( 'NONE',  ( 0.5314960629921264834, 0.1660481256975883668, -0.3530559997133364547 ) ) ;
#8504 = CARTESIAN_POINT ( 'NONE',  ( 0.2925321140481932369, -0.2925321140481932369, -1.673228346456692828 ) ) ;
#8505 = CARTESIAN_POINT ( 'NONE',  ( 3.929929591340561856, 1.125488309886446991, 0.2373865333886654438 ) ) ;
#8506 = CARTESIAN_POINT ( 'NONE',  ( -0.3346456692913377662, 0.1660481256975883668, -0.3530559997133364547 ) ) ;
#8508 = DIRECTION ( 'NONE',  ( 0.000000000000000000, 0.000000000000000000, -1.000000000000000000 ) ) ;
#8507 = CARTESIAN_POINT ( 'NONE',  ( 1.128608923884515169, -0.5023911411419708095, -0.1820866141732282451 ) ) ;
#8509 = CARTESIAN_POINT ( 'NONE',  ( -0.4091458600556402980, -0.2362204724409451284, -0.7591863517060367661 ) ) ;
#8510 = CARTESIAN_POINT ( 'NONE',  ( 1.174540682414699111, -0.2845877964562159024, 0.3641732283464567677 ) ) ;
#8511 = CARTESIAN_POINT ( 'NONE',  ( 1.325459317585302665, 0.05413385826771626580, -0.4176697321401330321 ) ) ;
#8512 = CARTESIAN_POINT ( 'NONE',  ( -9.674558042662122972E-17, 0.3949938075777409963, -0.2342519685039370914 ) ) ;
#8513 = CARTESIAN_POINT ( 'NONE',  ( -0.2559055118110230564, 0.1660481256975883668, -0.3530559997133364547 ) ) ;
#8514 = CARTESIAN_POINT ( 'NONE',  ( -1.587926509186350810, 0.05413385826771626580, -0.4176697321401330321 ) ) ;
#8515 = CARTESIAN_POINT ( 'NONE',  ( -1.581364829396324945, -0.3162353388693405765, 0.4822834645669290543 ) ) ;
#8516 = CARTESIAN_POINT ( 'NONE',  ( -0.3149606299212590610, -0.1870078740157479769, 0.4822834645669291653 ) ) ;
#8517 = CARTESIAN_POINT ( 'NONE',  ( -0.3949938075777411073, 0.1058382717557497660, -0.5820209973753280863 ) ) ;
#8518 = CARTESIAN_POINT ( 'NONE',  ( 1.115485564304462551, -0.4281496062992127816, -0.4176697321401328100 ) ) ;
#8519 = CARTESIAN_POINT ( 'NONE',  ( 0.4724409448818904789, -0.1870078740157479769, 0.4822834645669291653 ) ) ;
#8520 = CARTESIAN_POINT ( 'NONE',  ( 0.6364829396325465405, -0.2845877964562161244, -0.3641732283464567121 ) ) ;
#8521 = CARTESIAN_POINT ( 'NONE',  ( 0.3937007874015754361, -0.1870078740157479769, 0.3641732283464567677 ) ) ;
#8522 = CARTESIAN_POINT ( 'NONE',  ( -1.620734908136482577, 0.2952755905511811885, 0.1292274648535926551 ) ) ;
#8523 = ADVANCED_FACE ( 'NONE', ( #1220 ), #58434, .T. ) ;
#8524 = CARTESIAN_POINT ( 'NONE',  ( -0.1070741851644051862, -0.3996062992125986590, -1.408792650918635259 ) ) ;
#8525 = CARTESIAN_POINT ( 'NONE',  ( 0.7283464566929143125, 0.1660481256975885056, 0.3530559997133364547 ) ) ;
#8526 = CARTESIAN_POINT ( 'NONE',  ( -0.3917322834645669549, -0.1049643490035306603, -0.6679790026246719137 ) ) ;
#8527 = CARTESIAN_POINT ( 'NONE',  ( -0.4498537592782897998, 0.000000000000000000, -2.118110236220472675 ) ) ;
#8528 = CARTESIAN_POINT ( 'NONE',  ( -0.7974104941589342799, -2.567464376874931580E-15, -0.4445507791589072832 ) ) ;
#8529 = CARTESIAN_POINT ( 'NONE',  ( -0.07217847769028813698, -0.2845877964562161244, -0.3641732283464567121 ) ) ;
#8530 = ADVANCED_FACE ( 'NONE', ( #52109 ), #6383, .F. ) ;
#8531 = CARTESIAN_POINT ( 'NONE',  ( 0.3937007874015754361, -0.1870078740157479769, 0.4822834645669291653 ) ) ;
#8532 = CARTESIAN_POINT ( 'NONE',  ( 1.220472440944882608, 0.1771653543307087630, 0.000000000000000000 ) ) ;
#8533 = CARTESIAN_POINT ( 'NONE',  ( -0.7808398950131225646, -0.08942795157527998196, 0.3641732283464567121 ) ) ;
#8534 = CARTESIAN_POINT ( 'NONE',  ( -0.9251968503937002541, 0.1660481256975885056, 0.3530559997133364547 ) ) ;
#8535 = CONICAL_SURFACE ( 'NONE', #74443, 3.543307086614174484, 0.8726646259971734265 ) ;
#8536 = CARTESIAN_POINT ( 'NONE',  ( -1.607611548556429737, -0.6692913385826771977, 0.1292274648535927661 ) ) ;
#8537 = CARTESIAN_POINT ( 'NONE',  ( 0.4724409448818904789, -0.1870078740157480879, -0.4822834645669291653 ) ) ;
#8538 = CARTESIAN_POINT ( 'NONE',  ( 1.430446194225722500, -0.4281496062992127816, -0.4176697321401328100 ) ) ;
#8539 = EDGE_CURVE ( 'NONE', #9025, #20402, #6833, .T. ) ;
#8540 = CARTESIAN_POINT ( 'NONE',  ( -0.3974833285012852047, -0.03087045868620486369, -1.220472440944937453 ) ) ;
#8541 = CARTESIAN_POINT ( 'NONE',  ( 0.4986876640419954376, 0.2306618581243848609, 0.2411417322834645549 ) ) ;
#8542 = CARTESIAN_POINT ( 'NONE',  ( 0.2362204724409449064, 0.4091458600556404646, -2.740813648293963567 ) ) ;
#8543 = CARTESIAN_POINT ( 'NONE',  ( 1.673228346456693494, 0.1660481256975885056, 0.3530559997133364547 ) ) ;
#8544 = CARTESIAN_POINT ( 'NONE',  ( 1.384514435695538559, 0.2952755905511810774, -0.1292274648535930714 ) ) ;
#8545 = CARTESIAN_POINT ( 'NONE',  ( -1.561679790026246017, -0.004921259842519576551, 0.3153832671262227771 ) ) ;
#8546 = CARTESIAN_POINT ( 'NONE',  ( 1.213910761154856299, 0.1771653543307087630, 0.09757992244046791164 ) ) ;
#8547 = CARTESIAN_POINT ( 'NONE',  ( -1.332020997375327642, -0.08942795157527998196, 0.3641732283464567121 ) ) ;
#8548 = CARTESIAN_POINT ( 'NONE',  ( -0.8005249343832011588, -0.004921259842519870586, -0.3153832671262229437 ) ) ;
#8549 = CARTESIAN_POINT ( 'NONE',  ( 0.4265091863517067039, -0.5511811023622048555, -0.09757992244046775898 ) ) ;
#8550 = AXIS2_PLACEMENT_3D ( 'NONE', #25731, #51392, #38368 ) ;
#8551 = CARTESIAN_POINT ( 'NONE',  ( -0.07874015748031421014, -0.1870078740157479769, 0.4822834645669291653 ) ) ;
#8552 = CARTESIAN_POINT ( 'NONE',  ( 0.9580052493438326877, 0.05413385826771666132, 0.4176697321401328100 ) ) ;
#8553 = CARTESIAN_POINT ( 'NONE',  ( 0.1312335958005257930, 0.2306618581243847221, -0.2411417322834647770 ) ) ;
#8554 = CARTESIAN_POINT ( 'NONE',  ( 0.05249343832021075018, 0.1283753931104746893, -0.1820866141732285504 ) ) ;
#8555 = CARTESIAN_POINT ( 'NONE',  ( 1.364829396325459854, -0.6046776061558809534, -0.2411417322834644161 ) ) ;
#8556 = DIRECTION ( 'NONE',  ( -3.096699300667737957E-16, 1.000000000000000000, -0.000000000000000000 ) ) ;
#8557 = CARTESIAN_POINT ( 'NONE',  ( -0.9711286089238838626, -0.6046776061558807314, 0.2411417322834647770 ) ) ;
#8558 = CARTESIAN_POINT ( 'NONE',  ( -0.3996062992125986590, 0.1070741851644051862, -0.6627296587926508886 ) ) ;
#8559 = DIRECTION ( 'NONE',  ( -0.000000000000000000, 1.000000000000000000, -0.000000000000000000 ) ) ;
#8560 = CARTESIAN_POINT ( 'NONE',  ( -0.6889763779527552368, 0.1660481256975885056, 0.3530559997133364547 ) ) ;
#8561 = CARTESIAN_POINT ( 'NONE',  ( 0.006561679790026889343, -0.05778040916215522460, 0.4822834645669289988 ) ) ;
#8562 = CARTESIAN_POINT ( 'NONE',  ( 4.893765752498283924E-17, -0.3996062992125986035, -2.440944881889763884 ) ) ;
#8563 = CARTESIAN_POINT ( 'NONE',  ( 0.3949938075777411073, -0.1058382717557499464, -2.473753280839894764 ) ) ;
#8564 = ORIENTED_EDGE ( 'NONE', *, *, #32130, .F. ) ;
#8565 = CARTESIAN_POINT ( 'NONE',  ( -0.3917322834645669549, -0.1049643490035306603, -0.9829396325459317518 ) ) ;
#8566 = CARTESIAN_POINT ( 'NONE',  ( 3.861376881555339757, 2.746034003362845866, -0.5314960629921258173 ) ) ;
#8567 = CARTESIAN_POINT ( 'NONE',  ( -1.259842519685038686, -0.1870078740157479769, 0.3641732283464567677 ) ) ;
#8568 = CARTESIAN_POINT ( 'NONE',  ( -0.2867679344610365999, 0.2867679344610364889, -0.9566929133858265155 ) ) ;
#8569 = CARTESIAN_POINT ( 'NONE',  ( 1.594488188976378673, 0.07958543189024085140, 0.2665933059059887866 ) ) ;
#8570 = CARTESIAN_POINT ( 'NONE',  ( -0.1049643490035301746, -0.3917322834645670659, 0.1627489745744900018 ) ) ;
#8571 = CARTESIAN_POINT ( 'NONE',  ( 0.3608923884514443348, -0.6692913385826771977, 0.1292274648535927661 ) ) ;
#8572 = CARTESIAN_POINT ( 'NONE',  ( -0.4461942257217840213, 0.1283753931104748280, 0.1820866141732283561 ) ) ;
#8573 = CARTESIAN_POINT ( 'NONE',  ( 0.7152230971128614723, -0.3162353388693409650, -0.4822834645669289433 ) ) ;
#8574 = CARTESIAN_POINT ( 'NONE',  ( 0.4461942257217855201, -0.6046776061558807314, 0.2411417322834647770 ) ) ;
#8575 = CARTESIAN_POINT ( 'NONE',  ( -0.1998031496062991907, -0.3460692066303959757, -2.427821522309711266 ) ) ;
#8576 = CARTESIAN_POINT ( 'NONE',  ( -0.3392501089628019995, 0.1958661417322831999, -1.282827714731970215 ) ) ;
#8577 = CARTESIAN_POINT ( 'NONE',  ( 1.430446194225722500, -0.4281496062992127816, -0.4176697321401328100 ) ) ;
#8578 = CARTESIAN_POINT ( 'NONE',  ( -0.1377952755905504645, 0.1660481256975885056, 0.3530559997133364547 ) ) ;
#8579 = EDGE_CURVE ( 'NONE', #78909, #25966, #72070, .T. ) ;
#8580 = CARTESIAN_POINT ( 'NONE',  ( 1.423884514435696191, -0.05778040916215522460, 0.4822834645669289988 ) ) ;
#8581 = CARTESIAN_POINT ( 'NONE',  ( 0.8727034120734913358, -0.05778040916215522460, 0.4822834645669289988 ) ) ;
#8582 = CARTESIAN_POINT ( 'NONE',  ( -0.2867679344610364334, -0.2867679344610367109, -0.4586614173228347746 ) ) ;
#8583 = CARTESIAN_POINT ( 'NONE',  ( 0.08530183727034192087, -0.3162353388693409650, -0.4822834645669289433 ) ) ;
#8584 = CARTESIAN_POINT ( 'NONE',  ( 0.8070866141732289112, -0.5400638737290845981, -0.3530559997133363437 ) ) ;
#8585 = CARTESIAN_POINT ( 'NONE',  ( 0.01312335958005323398, -0.4281496062992127816, -0.4176697321401328100 ) ) ;
#8586 = CIRCLE ( 'NONE', #61027, 3.543307086614173596 ) ;
#8587 = CARTESIAN_POINT ( 'NONE',  ( 0.6036745406824154392, 0.1283753931104746893, -0.1820866141732285504 ) ) ;
#8588 = CARTESIAN_POINT ( 'NONE',  ( -1.200787401574802349, 0.1660481256975883668, -0.3530559997133364547 ) ) ;
#8589 = CARTESIAN_POINT ( 'NONE',  ( -1.213910761154854745, 0.2952755905511810774, -0.1292274648535930714 ) ) ;
#8590 = CARTESIAN_POINT ( 'NONE',  ( 0.8989501312335963501, -0.6692913385826773087, -0.1292274648535924053 ) ) ;
#8591 = CARTESIAN_POINT ( 'NONE',  ( 0.1188761721695186374, -0.3738583250853876883, -1.929133858267716883 ) ) ;
#8592 = CARTESIAN_POINT ( 'NONE',  ( -0.3392501089628019995, 0.1958661417322832277, -1.750656167979002698 ) ) ;
#8593 = VERTEX_POINT ( 'NONE', #38817 ) ;
#8594 = CARTESIAN_POINT ( 'NONE',  ( -0.1998031496062994683, 0.3460692066303958092, -0.6430446194225721834 ) ) ;
#8595 = ORIENTED_EDGE ( 'NONE', *, *, #57961, .F. ) ;
#8596 = CARTESIAN_POINT ( 'NONE',  ( 1.062992125984252745, 0.2952755905511811885, 0.000000000000000000 ) ) ;
#8597 = CARTESIAN_POINT ( 'NONE',  ( 0.3346456692913390985, 0.07958543189024085140, 0.2665933059059887866 ) ) ;
#8598 = DIRECTION ( 'NONE',  ( -1.000000000000000000, -8.805702923740138355E-17, 0.000000000000000000 ) ) ;
#8599 = DIRECTION ( 'NONE',  ( 0.000000000000000000, -1.000000000000000000, -0.000000000000000000 ) ) ;
#8600 = CARTESIAN_POINT ( 'NONE',  ( -0.5314960629921294810, 0.000000000000000000, 0.9881811337016621621 ) ) ;
#8601 = CARTESIAN_POINT ( 'NONE',  ( 4.797336870675656522E-17, -0.3917322834645670104, -1.265748031496062964 ) ) ;
#8602 = AXIS2_PLACEMENT_3D ( 'NONE', #33269, #1287, #20636 ) ;
#8603 = CARTESIAN_POINT ( 'NONE',  ( 1.207349081364829990, -0.6046776061558809534, -0.2411417322834644161 ) ) ;
#8604 = CARTESIAN_POINT ( 'NONE',  ( -0.3985446848722469237, -0.001150535885714259370, -1.929133858267716217 ) ) ;
#8605 = CARTESIAN_POINT ( 'NONE',  ( -0.4068241469816267775, 0.05413385826771626580, -0.4176697321401330321 ) ) ;
#8606 = CARTESIAN_POINT ( 'NONE',  ( 1.030183727034121421, -0.3162353388693409650, -0.4822834645669289433 ) ) ;
#8607 = ORIENTED_EDGE ( 'NONE', *, *, #38964, .F. ) ;
#8608 = FACE_OUTER_BOUND ( 'NONE', #10442, .T. ) ;
#8609 = CARTESIAN_POINT ( 'NONE',  ( -1.109428599580102537, 1.093625931280370001, -0.1684409714770037092 ) ) ;
#8610 = DIRECTION ( 'NONE',  ( 1.000000000000000222, 7.187676440535286524E-17, -6.740548460485784122E-17 ) ) ;
#8611 = CARTESIAN_POINT ( 'NONE',  ( 1.692913385826772421, 0.1771653543307087630, 0.000000000000000000 ) ) ;
#8612 = CARTESIAN_POINT ( 'NONE',  ( 0.1070741851644053527, 0.3996062992125985480, -2.117454068241469756 ) ) ;
#8613 = CARTESIAN_POINT ( 'NONE',  ( -1.509186351706035767, -0.3690944881889763329, 0.3153832671262228327 ) ) ;
#8614 =( BOUNDED_CURVE ( )  B_SPLINE_CURVE ( 2, ( #72912, #15264, #71249, #20318, #1796, #27458, #13595, #53117, #79246, #976, #1387, #27040, #66605 ),
 .UNSPECIFIED., .F., .F. ) 
 B_SPLINE_CURVE_WITH_KNOTS ( ( 3, 2, 2, 2, 2, 2, 3 ),
 ( 0.2187856400893463116, 0.2196969696969696961, 0.2234848484848484806, 0.2272727272727272652, 0.2310606060606060497, 0.2348484848484848619, 0.2357598144561083298 ),
 .UNSPECIFIED. ) 
 CURVE ( )  GEOMETRIC_REPRESENTATION_ITEM ( )  RATIONAL_B_SPLINE_CURVE ( ( 0.9875488213027527884, 0.9918020599134683701, 1.000000000000000000, 0.9659258262890683122, 1.000000000000000000, 0.9659258262890683122, 1.000000000000000000, 0.9659258262890683122, 1.000000000000000000, 0.9659258262890683122, 1.000000000000000000, 0.9918020599134675930, 0.9875488213027519002 ) ) 
 REPRESENTATION_ITEM ( '' )  );
#8615 = CARTESIAN_POINT ( 'NONE',  ( -1.653543307086613234, -0.1870078740157479769, 0.4822834645669291653 ) ) ;
#8616 = CARTESIAN_POINT ( 'NONE',  ( 0.6561679790026253567, -0.6046776061558809534, -0.2411417322834644161 ) ) ;
#8617 = VERTEX_POINT ( 'NONE', #32503 ) ;
#8619 = DIRECTION ( 'NONE',  ( -1.000000000000000000, -2.664535259100376091E-15, 0.000000000000000000 ) ) ;
#8618 = DIRECTION ( 'NONE',  ( 0.8660254037844361541, 0.000000000000000000, 0.5000000000000043299 ) ) ;
#8620 = CARTESIAN_POINT ( 'NONE',  ( -0.8398950131233589023, -0.5023911411419708095, -0.1820866141732282451 ) ) ;
#8621 = CARTESIAN_POINT ( 'NONE',  ( 0.8005249343832028242, -0.4281496062992127816, -0.4176697321401328100 ) ) ;
#8622 = CARTESIAN_POINT ( 'NONE',  ( -1.463254593175852492, -0.6692913385826773087, -0.1292274648535924053 ) ) ;
#8623 = CARTESIAN_POINT ( 'NONE',  ( -0.2867679344610364334, -0.2867679344610368219, -1.083970185530496844 ) ) ;
#8624 = CARTESIAN_POINT ( 'NONE',  ( -0.8792650918635160906, -0.004921259842519870586, -0.3153832671262229437 ) ) ;
#8625 = CARTESIAN_POINT ( 'NONE',  ( -1.548556430446193399, -0.5023911411419708095, -0.1820866141732282451 ) ) ;
#8626 = CARTESIAN_POINT ( 'NONE',  ( 0.3917322834645670104, 2.398668435337828261E-17, -1.147637795275590733 ) ) ;
#8627 = CARTESIAN_POINT ( 'NONE',  ( 0.6299212598425204535, -0.1870078740157479769, 0.4822834645669291653 ) ) ;
#8628 = CARTESIAN_POINT ( 'NONE',  ( -1.082677165354329896, -0.4536011799217368745, -0.2665933059059886201 ) ) ;
#8629 = CARTESIAN_POINT ( 'NONE',  ( -0.2165354330708654795, -0.4536011799217368745, -0.2665933059059886201 ) ) ;
#8630 = CARTESIAN_POINT ( 'NONE',  ( -0.2362204724409442680, -0.1870078740157480879, -0.4822834645669291653 ) ) ;
#8631 = CARTESIAN_POINT ( 'NONE',  ( 1.594488188976378673, -0.5400638737290845981, -0.3530559997133363437 ) ) ;
#8632 = CARTESIAN_POINT ( 'NONE',  ( 0.3917322834645670659, 2.398668435337828261E-17, -0.2723290270679284419 ) ) ;
#8633 = CARTESIAN_POINT ( 'NONE',  ( 0.8202099737532813073, 0.2952755905511811885, 0.1292274648535926551 ) ) ;
#8634 = DIRECTION ( 'NONE',  ( -1.000000000000000000, 0.000000000000000000, 0.000000000000000000 ) ) ;
#8635 = CARTESIAN_POINT ( 'NONE',  ( 0.4091458600556403535, 0.2362204724409449896, -1.625328083989501460 ) ) ;
#8636 = CARTESIAN_POINT ( 'NONE',  ( -0.6299212598425188991, -0.1870078740157479769, 0.4822834645669291653 ) ) ;
#8637 = CARTESIAN_POINT ( 'NONE',  ( -0.07217847769028813698, -0.2845877964562161244, -0.3641732283464567121 ) ) ;
#8638 = CARTESIAN_POINT ( 'NONE',  ( -1.272965879265091305, 0.05413385826771626580, -0.4176697321401330321 ) ) ;
#8639 = CARTESIAN_POINT ( 'NONE',  ( 0.4593175853018380828, -0.004921259842519870586, -0.3153832671262229437 ) ) ;
#8640 = CARTESIAN_POINT ( 'NONE',  ( -0.7086614173228339419, -0.1870078740157480601, -0.3641732283464567677 ) ) ;
#8641 = CARTESIAN_POINT ( 'NONE',  ( -1.135170603674539924, -0.6692913385826771977, 0.1292274648535927661 ) ) ;
#8642 = CARTESIAN_POINT ( 'NONE',  ( -1.646981627296586703, -0.3162353388693409650, -0.4822834645669289433 ) ) ;
#8643 = CARTESIAN_POINT ( 'NONE',  ( 1.233595800524935227, 0.2306618581243847221, -0.2411417322834647770 ) ) ;
#8644 = FACE_OUTER_BOUND ( 'NONE', #51295, .T. ) ;
#8645 = CARTESIAN_POINT ( 'NONE',  ( 0.7349081364829403995, 0.1283753931104748280, 0.1820866141732283561 ) ) ;
#8646 = VECTOR ( 'NONE', #43185, 39.37007874015748854 ) ;
#8647 = CARTESIAN_POINT ( 'NONE',  ( 0.5052493438320218022, -0.6692913385826773087, -0.1292274648535924053 ) ) ;
#8648 = CARTESIAN_POINT ( 'NONE',  ( -1.633858267716534529, 0.1660481256975885056, 0.3530559997133364547 ) ) ;
#8649 = CARTESIAN_POINT ( 'NONE',  ( 1.541994750656168645, -0.5511811023622046335, 0.09757992244046803654 ) ) ;
#8650 = VERTEX_POINT ( 'NONE', #19889 ) ;
#8651 = CARTESIAN_POINT ( 'NONE',  ( 0.2925321140481932369, 0.2925321140481932369, -2.734251968503936148 ) ) ;
#8652 = CARTESIAN_POINT ( 'NONE',  ( -1.200787401574802349, -0.4536011799217367080, 0.2665933059059888421 ) ) ;
#8653 = CARTESIAN_POINT ( 'NONE',  ( -0.3543307086614165824, 0.2952755905511811885, 0.000000000000000000 ) ) ;
#8654 = CARTESIAN_POINT ( 'NONE',  ( 0.3412073490813655186, 0.2306618581243848609, 0.2411417322834645549 ) ) ;
#8655 = CARTESIAN_POINT ( 'NONE',  ( -1.502624671916009680, -0.08942795157528024563, -0.3641732283464568787 ) ) ;
#8656 = CARTESIAN_POINT ( 'NONE',  ( -0.3460692066303957537, -0.1998031496062994405, -1.704068241469816281 ) ) ;
#8657 = CARTESIAN_POINT ( 'NONE',  ( -1.489501312335957062, -0.3162353388693409650, -0.4822834645669289433 ) ) ;
#8658 = CARTESIAN_POINT ( 'NONE',  ( 0.3346456692913393205, -0.5400638737290845981, -0.3530559997133363437 ) ) ;
#8659 = CARTESIAN_POINT ( 'NONE',  ( 0.1049868766404206816, 0.2306618581243848609, 0.2411417322834645549 ) ) ;
#8660 = CARTESIAN_POINT ( 'NONE',  ( 1.181102362204724976, -0.1870078740157480879, -0.4822834645669291653 ) ) ;
#8661 = CARTESIAN_POINT ( 'NONE',  ( 0.1070741851644054637, -0.3996062992125984925, -0.9494750656167977310 ) ) ;
#8662 = CARTESIAN_POINT ( 'NONE',  ( -0.3460692066303958092, -0.1998031496062994683, -1.154855643044619518 ) ) ;
#8663 = CONICAL_SURFACE ( 'NONE', #82613, 3.444881889763779625, 0.7853981633974500554 ) ;
#8664 = CARTESIAN_POINT ( 'NONE',  ( 0.3420746716998659953, 0.1974969037888705536, -0.7611548556430446366 ) ) ;
#8665 = CARTESIAN_POINT ( 'NONE',  ( -0.1049643490035307020, 0.3917322834645669549, -0.1561679790026246073 ) ) ;
#8666 = CARTESIAN_POINT ( 'NONE',  ( -0.2362204724409442680, -0.1870078740157480601, -0.3641732283464567677 ) ) ;
#8667 = CARTESIAN_POINT ( 'NONE',  ( -0.3674540682414692561, -0.6046776061558809534, -0.2411417322834644161 ) ) ;
#8668 = CARTESIAN_POINT ( 'NONE',  ( 1.030183727034121421, -0.3162353388693409650, -0.4822834645669289433 ) ) ;
#8669 = CARTESIAN_POINT ( 'NONE',  ( -0.1974969037888706924, 0.3420746716998658843, -1.822178477690288512 ) ) ;
#8670 = CARTESIAN_POINT ( 'NONE',  ( -0.08530183727034056085, -0.2845877964562159024, 0.3641732283464567677 ) ) ;
#8671 = CARTESIAN_POINT ( 'NONE',  ( -1.207349081364828436, -0.6046776061558807314, 0.2411417322834647770 ) ) ;
#8672 = CARTESIAN_POINT ( 'NONE',  ( -1.640419947506561060, 0.05413385826771666132, 0.4176697321401328100 ) ) ;
#8673 = CARTESIAN_POINT ( 'NONE',  ( 0.2362204724409449064, 0.4091458600556404646, -1.876640419947506411 ) ) ;
#8674 = DIRECTION ( 'NONE',  ( 0.000000000000000000, 0.000000000000000000, -1.000000000000000000 ) ) ;
#8675 = ORIENTED_EDGE ( 'NONE', *, *, #29379, .T. ) ;
#8676 = EDGE_CURVE ( 'NONE', #26273, #44534, #27067, .T. ) ;
#8677 = ORIENTED_EDGE ( 'NONE', *, *, #14300, .F. ) ;
#8678 = CARTESIAN_POINT ( 'NONE',  ( 1.259842519685040019, -0.1870078740157479769, 0.4822834645669291653 ) ) ;
#8679 = CARTESIAN_POINT ( 'NONE',  ( -1.699475065616797398, 0.2952755905511811885, 0.1292274648535926551 ) ) ;
#8681 = CARTESIAN_POINT ( 'NONE',  ( -1.272965879265091305, 0.05413385826771626580, -0.4176697321401330321 ) ) ;
#8680 = CARTESIAN_POINT ( 'NONE',  ( -1.364829396325458521, -0.5023911411419708095, 0.1820866141732285504 ) ) ;
#8682 = CARTESIAN_POINT ( 'NONE',  ( 0.1049643490035304522, -0.3917322834645668994, -2.527539739336271296 ) ) ;
#8683 = CARTESIAN_POINT ( 'NONE',  ( 1.220472440944882386, -0.1870078740157480046, 1.254653134982923898E-17 ) ) ;
#8684 = CARTESIAN_POINT ( 'NONE',  ( 1.312335958005250269, -0.6046776061558807314, 0.2411417322834647770 ) ) ;
#8685 = CARTESIAN_POINT ( 'NONE',  ( -0.4724409448818896462, -0.1265901696524993070, -2.408136482939632561 ) ) ;
#8686 = CARTESIAN_POINT ( 'NONE',  ( -0.2427821522309703550, -0.05778040916215560624, -0.4822834645669293319 ) ) ;
#8687 = CARTESIAN_POINT ( 'NONE',  ( -0.1509186351706028884, -0.05778040916215522460, 0.4822834645669289988 ) ) ;
#8688 = CARTESIAN_POINT ( 'NONE',  ( -1.076115485564303809, -0.6046776061558809534, -0.2411417322834644161 ) ) ;
#8689 = CARTESIAN_POINT ( 'NONE',  ( 4.797336870675655290E-17, -0.3917322834645669549, -2.678458374506874851 ) ) ;
#8690 = CARTESIAN_POINT ( 'NONE',  ( 0.4199475065616803948, -0.6046776061558809534, -0.2411417322834644161 ) ) ;
#8691 = CARTESIAN_POINT ( 'NONE',  ( 0.3392501089628018884, -0.1958661417322834220, -1.986876640419947604 ) ) ;
#8692 = CARTESIAN_POINT ( 'NONE',  ( -1.148293963254592542, 0.1771653543307087630, 0.09757992244046791164 ) ) ;
#8693 = ORIENTED_EDGE ( 'NONE', *, *, #22304, .F. ) ;
#8694 = CARTESIAN_POINT ( 'NONE',  ( -0.3949938075777409408, -0.1058382717557502933, -2.093175853018372834 ) ) ;
#8695 = VERTEX_POINT ( 'NONE', #64495 ) ;
#8696 = CARTESIAN_POINT ( 'NONE',  ( -1.614173228346456712, 2.401574803149606474, -0.1372047244094478091 ) ) ;
#8697 = CARTESIAN_POINT ( 'NONE',  ( -1.233595800524933894, 0.2306618581243848609, 0.2411417322834645549 ) ) ;
#8698 = CARTESIAN_POINT ( 'NONE',  ( -1.253280839895012377, -0.3162353388693409650, -0.4822834645669289433 ) ) ;
#8699 = CARTESIAN_POINT ( 'NONE',  ( -0.3460692066303960868, 0.1998031496062990242, -0.8136482939632546652 ) ) ;
#8700 = CARTESIAN_POINT ( 'NONE',  ( -1.528871391076114250, 0.2952755905511810774, -0.1292274648535930714 ) ) ;
#8701 = DIRECTION ( 'NONE',  ( 0.5931762764594944448, -9.392846415265724076E-15, -0.8050726085550603539 ) ) ;
#8702 = PLANE ( 'NONE',  #14134 ) ;
#8703 = CARTESIAN_POINT ( 'NONE',  ( -0.3280839895013117347, 0.05413385826771626580, -0.4176697321401330321 ) ) ;
#8704 = CARTESIAN_POINT ( 'NONE',  ( -0.1958661417322834220, -0.3392501089628018884, -0.1502624671916011345 ) ) ;
#8705 = CARTESIAN_POINT ( 'NONE',  ( 0.3018372703412079971, -0.004921259842519870586, -0.3153832671262229437 ) ) ;
#8706 = CARTESIAN_POINT ( 'NONE',  ( -0.6889763779527552368, -0.4536011799217368745, -0.2665933059059886201 ) ) ;
#8707 = CARTESIAN_POINT ( 'NONE',  ( -1.351706036745406347, -0.4281496062992124485, 0.4176697321401328655 ) ) ;
#8708 = CARTESIAN_POINT ( 'NONE',  ( 1.049868766404200127, -0.6046776061558809534, -0.2411417322834644161 ) ) ;
#8709 = CARTESIAN_POINT ( 'NONE',  ( -0.7349081364829387342, -0.6046776061558807314, 0.2411417322834647770 ) ) ;
#8710 = CARTESIAN_POINT ( 'NONE',  ( 0.5314960629921394730, 2.739927440807262915, -3.869764100875847213 ) ) ;
#8711 = ORIENTED_EDGE ( 'NONE', *, *, #51054, .T. ) ;
#8712 = CARTESIAN_POINT ( 'NONE',  ( -1.535433070866141225, -0.6692913385826771977, 8.415575281601705876E-17 ) ) ;
#8713 = CARTESIAN_POINT ( 'NONE',  ( -1.364829396325458521, 0.1283753931104746893, -0.1820866141732285504 ) ) ;
#8714 = CARTESIAN_POINT ( 'NONE',  ( -1.646981627296586703, -0.3162353388693409650, -0.4822834645669289433 ) ) ;
#8715 = CARTESIAN_POINT ( 'NONE',  ( 5.785732909357575061E-17, -0.4724409448818898682, -1.338582677165354173 ) ) ;
#8716 = CARTESIAN_POINT ( 'NONE',  ( 1.854617417371074772, 1.067551433859868615, -0.06782095098398562005 ) ) ;
#8717 = CARTESIAN_POINT ( 'NONE',  ( 0.3392501089628018884, -0.1958661417322834220, -0.5695538057742781657 ) ) ;
#8718 = CARTESIAN_POINT ( 'NONE',  ( -0.1049643490035301885, -0.3917322834645671215, -2.519028871391075786 ) ) ;
#8719 = CARTESIAN_POINT ( 'NONE',  ( -0.2559055118110227234, -0.5400638737290844871, 0.3530559997133364547 ) ) ;
#8720 = CARTESIAN_POINT ( 'NONE',  ( -1.450131233595799651, 0.1771653543307087075, -0.09757992244046823083 ) ) ;
#8721 = CARTESIAN_POINT ( 'NONE',  ( 0.2925321140481932369, -0.2925321140481931814, -0.1751968503937008370 ) ) ;
#8723 = CARTESIAN_POINT ( 'NONE',  ( 0.000000000000000000, 0.000000000000000000, 6.043307086614173151 ) ) ;
#8722 = CARTESIAN_POINT ( 'NONE',  ( -1.548556430446193399, 0.2306618581243848609, 0.2411417322834645549 ) ) ;
#8724 = CARTESIAN_POINT ( 'NONE',  ( -1.299212598425196097, -0.6692913385826771977, 8.415575281601705876E-17 ) ) ;
#8725 = CARTESIAN_POINT ( 'NONE',  ( -0.4986876640419942164, -0.6046776061558807314, 0.2411417322834647770 ) ) ;
#8726 = AXIS2_PLACEMENT_3D ( 'NONE', #13333, #65093, #7431 ) ;
#8727 = CARTESIAN_POINT ( 'NONE',  ( 4.797336870675655290E-17, -0.3917322834645669549, 0.1561872947844637760 ) ) ;
#8728 = CARTESIAN_POINT ( 'NONE',  ( 0.5511811023622054106, -0.1870078740157480601, -0.3641732283464567677 ) ) ;
#8729 = CARTESIAN_POINT ( 'NONE',  ( 0.1049643490035304799, -0.3917322834645669549, -0.01246719160104995359 ) ) ;
#8730 = CARTESIAN_POINT ( 'NONE',  ( 0.3937007874015754361, -0.1870078740157479769, 0.3641732283464567677 ) ) ;
#8731 = CARTESIAN_POINT ( 'NONE',  ( 0.8136482939632553313, 0.1283753931104748280, 0.1820866141732283561 ) ) ;
#8732 = CARTESIAN_POINT ( 'NONE',  ( 0.8464566929133865436, 0.1660481256975883668, -0.3530559997133364547 ) ) ;
#8733 = CARTESIAN_POINT ( 'NONE',  ( -0.4068241469816264999, -0.3690944881889763329, 0.3153832671262228327 ) ) ;
#8734 = CARTESIAN_POINT ( 'NONE',  ( -0.2867679344610365999, 0.2867679344610364889, -1.901574803149606252 ) ) ;
#8735 = CARTESIAN_POINT ( 'NONE',  ( -1.338582677165353729, -0.1870078740157479769, 0.4822834645669291653 ) ) ;
#8736 = CARTESIAN_POINT ( 'NONE',  ( -0.2362204724409442680, -0.1870078740157480601, -0.3641732283464567677 ) ) ;
#8737 = CARTESIAN_POINT ( 'NONE',  ( -1.154855643044618851, 0.1283753931104748280, 0.1820866141732283561 ) ) ;
#8738 = CARTESIAN_POINT ( 'NONE',  ( 0.2362204724409449064, 0.4091458600556404646, -0.3786089238845143923 ) ) ;
#8739 = CARTESIAN_POINT ( 'NONE',  ( -0.7349081364829387342, -0.5023911411419708095, 0.1820866141732285504 ) ) ;
#8740 = LINE ( 'NONE', #2433, #43986 ) ;
#8741 = CARTESIAN_POINT ( 'NONE',  ( -0.1902887139107604098, 0.2952755905511810774, -0.1292274648535930714 ) ) ;
#8742 = CARTESIAN_POINT ( 'NONE',  ( -2.556891458315154519, 2.729656612766095947, 0.5314960629921260393 ) ) ;
#8743 = CARTESIAN_POINT ( 'NONE',  ( 0.4855643044619428750, -0.004921259842519576551, 0.3153832671262227771 ) ) ;
#8744 = CARTESIAN_POINT ( 'NONE',  ( -0.09186351706036689768, -0.004921259842519870586, -0.3153832671262229437 ) ) ;
#8745 = CARTESIAN_POINT ( 'NONE',  ( -0.2952755905511803003, -0.5400638737290845981, -0.3530559997133363437 ) ) ;
#8746 = DIRECTION ( 'NONE',  ( -0.000000000000000000, -1.000000000000000000, -0.000000000000000000 ) ) ;
#8747 = CARTESIAN_POINT ( 'NONE',  ( -0.9120734908136475250, -0.5511811023622048555, -0.09757992244046775898 ) ) ;
#8748 = FACE_OUTER_BOUND ( 'NONE', #40960, .T. ) ;
#8749 = CARTESIAN_POINT ( 'NONE',  ( 0.5708661417322842269, 0.1660481256975885056, 0.3530559997133364547 ) ) ;
#8750 = CARTESIAN_POINT ( 'NONE',  ( 0.1998031496062992463, 0.3460692066303959202, -1.638451443569553634 ) ) ;
#8751 = CARTESIAN_POINT ( 'NONE',  ( 1.410761154855643795, -0.3162353388693405765, 0.4822834645669290543 ) ) ;
#8752 = CARTESIAN_POINT ( 'NONE',  ( -0.2624671916010490880, 0.1283753931104746893, -0.1820866141732285504 ) ) ;
#8753 = CARTESIAN_POINT ( 'NONE',  ( -1.574803149606298192, -0.1870078740157480879, -0.4822834645669291653 ) ) ;
#8754 = CARTESIAN_POINT ( 'NONE',  ( 1.509186351706037543, 0.05413385826771666132, 0.4176697321401328100 ) ) ;
#8755 = CARTESIAN_POINT ( 'NONE',  ( 1.358267716535433323, 0.1660481256975885056, 0.3530559997133364547 ) ) ;
#8756 = CARTESIAN_POINT ( 'NONE',  ( -0.5774278215223089816, 0.1283753931104746893, -0.1820866141732285504 ) ) ;
#8757 = CARTESIAN_POINT ( 'NONE',  ( -1.614173228346457378, 1.881821177735609085, 0.1372047244094476981 ) ) ;
#8758 = CARTESIAN_POINT ( 'NONE',  ( 0.8923884514435701520, -0.6046776061558809534, -0.2411417322834644161 ) ) ;
#8759 = CARTESIAN_POINT ( 'NONE',  ( -0.3996062992125987146, 0.1070741851644051862, -0.03280839895013124008 ) ) ;
#8760 = CARTESIAN_POINT ( 'NONE',  ( 0.1049643490035304799, -0.3917322834645670104, -2.601725352527246127 ) ) ;
#8761 = CARTESIAN_POINT ( 'NONE',  ( -3.900966923095589678, 2.687614851728675092, -0.5314960629921259283 ) ) ;
#8762 = CARTESIAN_POINT ( 'NONE',  ( 1.548556430446194954, -0.5023911411419708095, 0.1820866141732285504 ) ) ;
#8763 = CARTESIAN_POINT ( 'NONE',  ( -1.345144356955379816, -0.05778040916215560624, -0.4822834645669293319 ) ) ;
#8764 = CARTESIAN_POINT ( 'NONE',  ( 1.272965879265092637, 0.05413385826771666132, 0.4176697321401328100 ) ) ;
#8765 = CARTESIAN_POINT ( 'NONE',  ( 0.3392501089628018329, 0.1958661417322835607, -2.263123359580052618 ) ) ;
#8766 = CARTESIAN_POINT ( 'NONE',  ( 1.089238845144357759, -0.004921259842519870586, -0.3153832671262229437 ) ) ;
#8767 = EDGE_CURVE ( 'NONE', #65017, #55450, #26188, .T. ) ;
#8768 = CARTESIAN_POINT ( 'NONE',  ( -0.02624671916010428221, 0.2306618581243847221, -0.2411417322834647770 ) ) ;
#8769 = CARTESIAN_POINT ( 'NONE',  ( -0.1968503937007867743, 0.2952755905511811885, 0.000000000000000000 ) ) ;
#8770 = CARTESIAN_POINT ( 'NONE',  ( 1.614173228346457378, -0.6692913385826771977, 8.415575281601705876E-17 ) ) ;
#8771 = CARTESIAN_POINT ( 'NONE',  ( 3.831845081856512181, 2.755400581649067426, 0.5314960629921259283 ) ) ;
#8772 = CARTESIAN_POINT ( 'NONE',  ( 0.2624671916010504757, -0.5023911411419708095, -0.1820866141732282451 ) ) ;
#8773 = ORIENTED_EDGE ( 'NONE', *, *, #25189, .F. ) ;
#8775 = CARTESIAN_POINT ( 'NONE',  ( -0.3917322834645670104, -0.1049643490035307020, -0.5151111792988996019 ) ) ;
#8774 = VECTOR ( 'NONE', #29278, 39.37007874015748143 ) ;
#8776 = ORIENTED_EDGE ( 'NONE', *, *, #34523, .T. ) ;
#8777 = CARTESIAN_POINT ( 'NONE',  ( -0.3083989501312330295, -0.05778040916215522460, 0.4822834645669289988 ) ) ;
#8778 = CARTESIAN_POINT ( 'NONE',  ( 1.332020997375328974, -0.05778040916215560624, -0.4822834645669293319 ) ) ;
#8779 = CARTESIAN_POINT ( 'NONE',  ( 0.08530183727034192087, -0.05778040916215522460, 0.4822834645669289988 ) ) ;
#8780 = CARTESIAN_POINT ( 'NONE',  ( -0.2952755905511803003, -0.4536011799217368745, -0.2665933059059886201 ) ) ;
#8781 = CARTESIAN_POINT ( 'NONE',  ( 1.161417322834646493, -0.5400638737290844871, 0.3530559997133364547 ) ) ;
#8782 = CARTESIAN_POINT ( 'NONE',  ( -0.7414698162729651543, -0.6692913385826771977, 0.1292274648535927661 ) ) ;
#8783 = CARTESIAN_POINT ( 'NONE',  ( 0.1246719160104994284, -0.6692913385826771977, 0.1292274648535927661 ) ) ;
#8784 = CARTESIAN_POINT ( 'NONE',  ( -0.9251968503937002541, 0.1660481256975885056, 0.3530559997133364547 ) ) ;
#8785 = CARTESIAN_POINT ( 'NONE',  ( 1.371391076115485719, -0.6692913385826773087, -0.1292274648535924053 ) ) ;
#8786 = CARTESIAN_POINT ( 'NONE',  ( 0.9055118110236227702, -0.6692913385826771977, 8.415575281601705876E-17 ) ) ;
#8787 = CARTESIAN_POINT ( 'NONE',  ( 1.279527559055118724, -0.5400638737290845981, -0.3530559997133363437 ) ) ;
#8788 = CARTESIAN_POINT ( 'NONE',  ( -0.1958661417322836718, 0.3392501089628017219, -0.4776902887139107268 ) ) ;
#8789 = CARTESIAN_POINT ( 'NONE',  ( 0.1115485564304470323, 0.1771653543307087630, 0.09757992244046791164 ) ) ;
#8790 = ORIENTED_EDGE ( 'NONE', *, *, #44899, .T. ) ;
#8791 = CARTESIAN_POINT ( 'NONE',  ( 0.1974969037888706369, -0.3420746716998659953, -0.8792650918635170898 ) ) ;
#8792 = VERTEX_POINT ( 'NONE', #51849 ) ;
#8793 = CARTESIAN_POINT ( 'NONE',  ( -0.7545931758530177724, 0.1771653543307087630, 0.09757992244046791164 ) ) ;
#8794 = CARTESIAN_POINT ( 'NONE',  ( -0.06561679790026180015, 0.05413385826771666132, 0.4176697321401328100 ) ) ;
#8795 = CARTESIAN_POINT ( 'NONE',  ( -1.491404278319911736, 1.136671166205875716, 0.2539434599294014827 ) ) ;
#8796 = CARTESIAN_POINT ( 'NONE',  ( -0.3871391076115479057, -0.3162353388693409650, -0.4822834645669289433 ) ) ;
#8797 = CARTESIAN_POINT ( 'NONE',  ( -0.5314960629921254842, -0.5400638737290845981, -0.3530559997133363437 ) ) ;
#8798 = CARTESIAN_POINT ( 'NONE',  ( -0.6824146981627288167, 0.2306618581243848609, 0.2411417322834645549 ) ) ;
#8799 = CARTESIAN_POINT ( 'NONE',  ( -1.371391076115484831, 0.2952755905511810774, -0.1292274648535930714 ) ) ;
#8800 = CARTESIAN_POINT ( 'NONE',  ( 1.456692913385827515, -0.5511811023622047445, 6.969142054262312111E-17 ) ) ;
#8801 = DIRECTION ( 'NONE',  ( 0.000000000000000000, -8.673617379884024625E-16, 1.000000000000000000 ) ) ;
#8802 = CARTESIAN_POINT ( 'NONE',  ( 0.2373513483963055337, 0.1756490242921440736, 5.678081160219037749 ) ) ;
#8803 = CARTESIAN_POINT ( 'NONE',  ( 0.3083989501312343062, -0.2845877964562159024, 0.3641732283464567677 ) ) ;
#8804 = CARTESIAN_POINT ( 'NONE',  ( -0.06561679790026180015, 0.05413385826771666132, 0.4176697321401328100 ) ) ;
#8805 = CARTESIAN_POINT ( 'NONE',  ( 0.1902887139107617975, -0.6692913385826773087, -0.1292274648535924053 ) ) ;
#8806 = ORIENTED_EDGE ( 'NONE', *, *, #13185, .T. ) ;
#8807 = CARTESIAN_POINT ( 'NONE',  ( -0.1998031496062994683, 0.3460692066303958092, -1.902887139107611647 ) ) ;
#8808 = CARTESIAN_POINT ( 'NONE',  ( -0.6175017169405814244, 0.000000000000000000, 0.3464511005275205946 ) ) ;
#8809 = CARTESIAN_POINT ( 'NONE',  ( -0.2925321140481932369, 0.2925321140481931259, -1.198818897637795367 ) ) ;
#8810 = CARTESIAN_POINT ( 'NONE',  ( 0.2925321140481932369, -0.2925321140481931814, -0.3326771653543306728 ) ) ;
#8811 = CARTESIAN_POINT ( 'NONE',  ( -0.4199475065616791736, 0.2306618581243847221, -0.2411417322834647770 ) ) ;
#8812 = CARTESIAN_POINT ( 'NONE',  ( -0.3458507752293909498, 0.3458507752293907833, -0.1771653543307086520 ) ) ;
#8813 = CARTESIAN_POINT ( 'NONE',  ( -0.2867679344610365999, 0.2867679344610364889, -2.151574803149605586 ) ) ;
#8814 = CARTESIAN_POINT ( 'NONE',  ( -1.640419947506561060, -0.004921259842519576551, 0.3153832671262227771 ) ) ;
#8815 = CARTESIAN_POINT ( 'NONE',  ( 1.017060367454068581, -0.05778040916215560624, -0.4822834645669293319 ) ) ;
#8816 = CARTESIAN_POINT ( 'NONE',  ( 0.7808398950131241190, -0.05778040916215560624, -0.4822834645669293319 ) ) ;
#8817 = CARTESIAN_POINT ( 'NONE',  ( -0.2165354330708654795, 0.07958543189024085140, 0.2665933059059887866 ) ) ;
#8818 = CARTESIAN_POINT ( 'NONE',  ( -0.1181102362204717315, 0.2952755905511811885, 0.000000000000000000 ) ) ;
#8819 = CARTESIAN_POINT ( 'NONE',  ( -0.2362204724409451284, 0.4091458600556402425, -1.979658792650918597 ) ) ;
#8820 = CARTESIAN_POINT ( 'NONE',  ( -0.1377952755905504645, -0.4536011799217368745, -0.2665933059059886201 ) ) ;
#8821 = CARTESIAN_POINT ( 'NONE',  ( -0.3674540682414692561, -0.6046776061558809534, -0.2411417322834644161 ) ) ;
#8822 = CARTESIAN_POINT ( 'NONE',  ( -0.3949938075777408852, -0.1058382717557502933, -2.012467191601050143 ) ) ;
#8823 = CARTESIAN_POINT ( 'NONE',  ( -1.673228346456691717, 0.1660481256975883668, -0.3530559997133364547 ) ) ;
#8824 = CARTESIAN_POINT ( 'NONE',  ( 0.2362204724409456558, -0.1870078740157480601, -0.3641732283464567677 ) ) ;
#8825 = CARTESIAN_POINT ( 'NONE',  ( 1.673228346456693494, 0.07958543189024085140, 0.2665933059059887866 ) ) ;
#8826 = CARTESIAN_POINT ( 'NONE',  ( -1.010498687664041384, -0.4281496062992127816, -0.4176697321401328100 ) ) ;
#8827 = CARTESIAN_POINT ( 'NONE',  ( -0.6430446194225712953, -0.004921259842519870586, -0.3153832671262229437 ) ) ;
#8828 = CYLINDRICAL_SURFACE ( 'NONE', #64130, 0.3937007874015748254 ) ;
#8829 = CARTESIAN_POINT ( 'NONE',  ( -0.6889763779527552368, -0.5400638737290845981, -0.3530559997133363437 ) ) ;
#8830 = CARTESIAN_POINT ( 'NONE',  ( -0.4986876640419939388, 0.2306618581243847221, -0.2411417322834647770 ) ) ;
#8831 = CARTESIAN_POINT ( 'NONE',  ( 0.09842519685039434474, 0.1660481256975885056, 0.3530559997133364547 ) ) ;
#8832 = CARTESIAN_POINT ( 'NONE',  ( -0.3996062992125985480, -7.340648628747423112E-17, -2.635826771653543066 ) ) ;
#8833 = CARTESIAN_POINT ( 'NONE',  ( 0.1958661417322836162, -0.3392501089628018329, -2.219140789205037656 ) ) ;
#8834 = VECTOR ( 'NONE', #20180, 39.37007874015748143 ) ;
#8835 = DIRECTION ( 'NONE',  ( -0.2810846377148240594, -0.6785983445458320107, 0.6785983445458603214 ) ) ;
#8836 = CARTESIAN_POINT ( 'NONE',  ( 0.2952755905511819101, 0.07958543189024071263, -0.2665933059059888421 ) ) ;
#8837 = CARTESIAN_POINT ( 'NONE',  ( 1.010498687664042716, 0.05413385826771626580, -0.4176697321401330321 ) ) ;
#8838 = CARTESIAN_POINT ( 'NONE',  ( -1.272965879265091305, -0.3690944881889763329, 0.3153832671262228327 ) ) ;
#8839 = CARTESIAN_POINT ( 'NONE',  ( 1.364829396325460076, 0.2306618581243848609, 0.2411417322834645549 ) ) ;
#8840 = CARTESIAN_POINT ( 'NONE',  ( -1.279527559055116948, -0.4536011799217367080, 0.2665933059059888421 ) ) ;
#8841 = CARTESIAN_POINT ( 'NONE',  ( -0.3543307086614165824, -0.6692913385826771977, 8.415575281601705876E-17 ) ) ;
#8842 = CARTESIAN_POINT ( 'NONE',  ( 0.2493438320209980519, -0.004921259842519576551, 0.3153832671262227771 ) ) ;
#8843 = CARTESIAN_POINT ( 'NONE',  ( 0.000000000000000000, 0.04488074079120461107, -1.244489337948955221 ) ) ;
#8844 = CARTESIAN_POINT ( 'NONE',  ( 0.6627296587926515548, 0.1771653543307087630, 0.09757992244046791164 ) ) ;
#8845 = CARTESIAN_POINT ( 'NONE',  ( 0.1443569553805781891, 0.05413385826771626580, -0.4176697321401330321 ) ) ;
#8846 = CARTESIAN_POINT ( 'NONE',  ( 4.893765752498283308E-17, -0.3996062992125985480, -0.1555118110236220763 ) ) ;
#8847 = CARTESIAN_POINT ( 'NONE',  ( -0.6627296587926503335, -0.6692913385826771977, 0.1292274648535927661 ) ) ;
#8848 = CARTESIAN_POINT ( 'NONE',  ( -0.2867679344610365999, 0.2867679344610364889, -1.994094488188976610 ) ) ;
#8849 = CARTESIAN_POINT ( 'NONE',  ( 1.122047244094488860, 0.07958543189024085140, 0.2665933059059887866 ) ) ;
#8850 = CARTESIAN_POINT ( 'NONE',  ( -0.01968503937007793844, 0.1660481256975883668, -0.3530559997133364547 ) ) ;
#8851 = CARTESIAN_POINT ( 'NONE',  ( -0.4527559055118102749, -0.5400638737290845981, -0.3530559997133363437 ) ) ;
#8852 = CARTESIAN_POINT ( 'NONE',  ( -0.3937007874015740483, -0.1870078740157479769, 0.3641732283464567677 ) ) ;
#8853 = CARTESIAN_POINT ( 'NONE',  ( 0.5971128608923891301, 0.2066929133858267098, -0.1054918080437494132 ) ) ;
#8854 = CARTESIAN_POINT ( 'NONE',  ( -0.04593175853018302557, 0.1771653543307087630, 0.09757992244046791164 ) ) ;
#8855 = CARTESIAN_POINT ( 'NONE',  ( 0.4790026246719168435, -0.3162353388693409650, -0.4822834645669289433 ) ) ;
#8856 = CARTESIAN_POINT ( 'NONE',  ( -0.6627296587926503335, -0.5511811023622046335, 0.09757992244046803654 ) ) ;
#8857 = CARTESIAN_POINT ( 'NONE',  ( 4.893765752498283308E-17, -0.3996062992125985480, -1.100393700787401619 ) ) ;
#8858 = CARTESIAN_POINT ( 'NONE',  ( -1.233595800524933894, -0.6046776061558809534, -0.2411417322834644161 ) ) ;
#8859 = DIRECTION ( 'NONE',  ( -0.000000000000000000, -1.000000000000000000, -0.000000000000000000 ) ) ;
#8860 = ORIENTED_EDGE ( 'NONE', *, *, #32904, .F. ) ;
#8861 = CARTESIAN_POINT ( 'NONE',  ( -1.043307086614172707, 0.07958543189024071263, -0.2665933059059888421 ) ) ;
#8862 = CARTESIAN_POINT ( 'NONE',  ( -0.2427821522309703550, -0.05778040916215560624, -0.4822834645669293319 ) ) ;
#8863 = CARTESIAN_POINT ( 'NONE',  ( -1.601049868766403650, -0.6046776061558807314, 0.2411417322834647770 ) ) ;
#8864 = CARTESIAN_POINT ( 'NONE',  ( -0.6299212598425188991, -0.1870078740157480879, -0.4822834645669291653 ) ) ;
#8865 = DIRECTION ( 'NONE',  ( 0.000000000000000000, 0.000000000000000000, -1.000000000000000000 ) ) ;
#8866 = CARTESIAN_POINT ( 'NONE',  ( 1.233595800524935227, 0.2306618581243847221, -0.2411417322834647770 ) ) ;
#8867 = CARTESIAN_POINT ( 'NONE',  ( 0.9776902887139113929, -0.6692913385826773087, -0.1292274648535924053 ) ) ;
#8868 = CARTESIAN_POINT ( 'NONE',  ( 0.000000000000000000, 2.755905511811024056, 0.000000000000000000 ) ) ;
#8869 = CARTESIAN_POINT ( 'NONE',  ( -0.5314960629921122726, 2.755905511811024056, -3.937007874015763687 ) ) ;
#8870 = AXIS2_PLACEMENT_3D ( 'NONE', #68164, #42464, #17244 ) ;
#8872 = VECTOR ( 'NONE', #78927, 39.37007874015748143 ) ;
#8871 = CARTESIAN_POINT ( 'NONE',  ( 0.2845351084527213970, -0.07967650482972132853, 5.860631297047876664 ) ) ;
#8873 = CARTESIAN_POINT ( 'NONE',  ( 1.450131233595801428, 0.1771653543307087630, 0.09757992244046791164 ) ) ;
#8874 = CARTESIAN_POINT ( 'NONE',  ( 0.1070741851644053527, 0.3996062992125986590, -0.6233595800524933672 ) ) ;
#8875 = ORIENTED_EDGE ( 'NONE', *, *, #68645, .T. ) ;
#8876 = CARTESIAN_POINT ( 'NONE',  ( -0.4593175853018364174, -0.3690944881889765550, -0.3153832671262227771 ) ) ;
#8877 = CARTESIAN_POINT ( 'NONE',  ( -9.594673741351313045E-17, 0.3917322834645670104, -2.039370078740157410 ) ) ;
#8878 = ORIENTED_EDGE ( 'NONE', *, *, #60399, .T. ) ;
#8879 = CARTESIAN_POINT ( 'NONE',  ( 0.7808398950131240079, -0.3162353388693405765, 0.4822834645669290543 ) ) ;
#8880 = CARTESIAN_POINT ( 'NONE',  ( 0.2427821522309716595, -0.3162353388693409650, -0.4822834645669289433 ) ) ;
#8881 = CARTESIAN_POINT ( 'NONE',  ( -0.7742782152230962556, -0.4281496062992127816, -0.4176697321401328100 ) ) ;
#8882 = CARTESIAN_POINT ( 'NONE',  ( 1.561679790026247350, 0.05413385826771626580, -0.4176697321401330321 ) ) ;
#8883 = CARTESIAN_POINT ( 'NONE',  ( -0.6758530183727028406, 0.1771653543307087630, 0.09757992244046791164 ) ) ;
#8884 = DIRECTION ( 'NONE',  ( 0.000000000000000000, 0.000000000000000000, -1.000000000000000000 ) ) ;
#8885 = CARTESIAN_POINT ( 'NONE',  ( 0.4461942257217856311, 0.2306618581243847221, -0.2411417322834647770 ) ) ;
#8886 = CARTESIAN_POINT ( 'NONE',  ( 0.4855643044619428750, -0.004921259842519576551, 0.3153832671262227771 ) ) ;
#8887 = CARTESIAN_POINT ( 'NONE',  ( -1.036745406824146176, -0.4281496062992124485, 0.4176697321401328655 ) ) ;
#8888 = CARTESIAN_POINT ( 'NONE',  ( -0.2867679344610364334, -0.2867679344610368219, -1.713891445373016520 ) ) ;
#8889 = CARTESIAN_POINT ( 'NONE',  ( -1.233595800524933894, -0.6046776061558809534, -0.2411417322834644161 ) ) ;
#8890 = CARTESIAN_POINT ( 'NONE',  ( -1.660104986876639543, -0.08942795157528024563, -0.3641732283464568787 ) ) ;
#8891 = CARTESIAN_POINT ( 'NONE',  ( 0.9776902887139113929, -0.6692913385826773087, -0.1292274648535924053 ) ) ;
#8892 = CARTESIAN_POINT ( 'NONE',  ( 1.167979002624672580, -0.3690944881889763329, 0.3153832671262228327 ) ) ;
#8893 = ORIENTED_EDGE ( 'NONE', *, *, #15339, .T. ) ;
#8894 = CARTESIAN_POINT ( 'NONE',  ( 0.3420746716998660508, -0.1974969037888703871, 0.05249343832020991057 ) ) ;
#8895 = CARTESIAN_POINT ( 'NONE',  ( -0.4002624671916004129, -0.3162353388693405765, 0.4822834645669290543 ) ) ;
#8896 = ORIENTED_EDGE ( 'NONE', *, *, #64509, .T. ) ;
#8898 = CIRCLE ( 'NONE', #66700, 0.1190944881889763746 ) ;
#8897 = CARTESIAN_POINT ( 'NONE',  ( 0.5839895013123367340, -0.5511811023622048555, -0.09757992244046775898 ) ) ;
#8899 = CARTESIAN_POINT ( 'NONE',  ( -1.364829396325458521, 0.2306618581243847221, -0.2411417322834647770 ) ) ;
#8900 = CARTESIAN_POINT ( 'NONE',  ( 1.089238845144357537, -0.4281496062992124485, 0.4176697321401328655 ) ) ;
#8901 = CARTESIAN_POINT ( 'NONE',  ( 0.8333333333333340365, 0.2952755905511810774, -0.1292274648535930714 ) ) ;
#8902 = CARTESIAN_POINT ( 'NONE',  ( -0.2952755905511804668, 0.1660481256975885056, 0.3530559997133364547 ) ) ;
#8903 = CARTESIAN_POINT ( 'NONE',  ( -0.2559055118110227234, -0.5400638737290844871, 0.3530559997133364547 ) ) ;
#8904 = CARTESIAN_POINT ( 'NONE',  ( -0.2867679344610365999, 0.2867679344610364889, -2.309055118110235671 ) ) ;
#8905 = CARTESIAN_POINT ( 'NONE',  ( -1.607611548556429737, -0.6692913385826771977, 0.1292274648535927661 ) ) ;
#8906 = CARTESIAN_POINT ( 'NONE',  ( -0.6758530183727028406, 0.2952755905511811885, 0.1292274648535926551 ) ) ;
#8907 = CARTESIAN_POINT ( 'NONE',  ( -0.6496062992125976043, 0.07958543189024071263, -0.2665933059059888421 ) ) ;
#8908 = CARTESIAN_POINT ( 'NONE',  ( 1.292650918635171564, -0.6692913385826773087, -0.1292274648535924053 ) ) ;
#8909 = DIRECTION ( 'NONE',  ( -0.000000000000000000, -0.000000000000000000, -1.000000000000000000 ) ) ;
#8910 = ADVANCED_FACE ( 'NONE', ( #65350 ), #16332, .F. ) ;
#8911 = CARTESIAN_POINT ( 'NONE',  ( -1.036745406824146176, 0.05413385826771626580, -0.4176697321401330321 ) ) ;
#8912 = CARTESIAN_POINT ( 'NONE',  ( -0.2925321140481932369, 0.2925321140481931259, 0.06102362204724409017 ) ) ;
#8913 = CARTESIAN_POINT ( 'NONE',  ( 0.5446194225721792126, -0.05778040916215560624, -0.4822834645669293319 ) ) ;
#8914 = CARTESIAN_POINT ( 'NONE',  ( -0.3996062992125986035, -0.1070741851644056997, -1.778215223097112663 ) ) ;
#8915 = CARTESIAN_POINT ( 'NONE',  ( -0.6575345472709128725, 1.929133858267715773, -0.5309055118110235227 ) ) ;
#8916 = EDGE_CURVE ( 'NONE', #64866, #31453, #1542, .T. ) ;
#8917 = CARTESIAN_POINT ( 'NONE',  ( -0.2165354330708654795, 0.1660481256975885056, 0.3530559997133364547 ) ) ;
#8918 = CARTESIAN_POINT ( 'NONE',  ( -1.332020997375327642, -0.08942795157527998196, 0.3641732283464567121 ) ) ;
#8920 = CARTESIAN_POINT ( 'NONE',  ( -0.4623158380715545746, 0.02617651024168223331, 2.142213561789874543 ) ) ;
#8919 = CARTESIAN_POINT ( 'NONE',  ( 1.167979002624672580, -0.3690944881889763329, 0.3153832671262228327 ) ) ;
#8921 = CARTESIAN_POINT ( 'NONE',  ( 0.4091458600556403535, 0.2362204724409449896, -0.8379265091863516979 ) ) ;
#8922 = CARTESIAN_POINT ( 'NONE',  ( 1.259842519685040019, -0.1870078740157480601, -0.3641732283464567677 ) ) ;
#8923 = CARTESIAN_POINT ( 'NONE',  ( 1.417322834645670104, -0.1870078740157479769, 0.4822834645669291653 ) ) ;
#8924 = CARTESIAN_POINT ( 'NONE',  ( -0.1974969037888704149, -0.3420746716998661063, -0.2998687664041995715 ) ) ;
#8925 = CARTESIAN_POINT ( 'NONE',  ( -0.2493438320209966919, 0.05413385826771626580, -0.4176697321401330321 ) ) ;
#8926 = CARTESIAN_POINT ( 'NONE',  ( -0.5314960629921122726, 2.755905511811024056, -3.937007874015763687 ) ) ;
#8927 = CARTESIAN_POINT ( 'NONE',  ( 1.561679790026247350, -0.3690944881889763329, 0.3153832671262228327 ) ) ;
#8928 = CARTESIAN_POINT ( 'NONE',  ( -0.2165354330708654795, -0.5400638737290845981, -0.3530559997133363437 ) ) ;
#8929 = CARTESIAN_POINT ( 'NONE',  ( -0.2891555358219909388, -0.2891555358219912164, -0.2933070866141732624 ) ) ;
#8930 = CARTESIAN_POINT ( 'NONE',  ( 1.187664041994751285, -0.05778040916215522460, 0.4822834645669289988 ) ) ;
#8931 = CARTESIAN_POINT ( 'NONE',  ( 0.3674540682414705883, 0.2306618581243847221, -0.2411417322834647770 ) ) ;
#8932 = CARTESIAN_POINT ( 'NONE',  ( 0.4396325459317593221, 0.1771653543307087075, -0.09757992244046823083 ) ) ;
#8933 = PLANE ( 'NONE',  #11755 ) ;
#8934 = CARTESIAN_POINT ( 'NONE',  ( 0.2755905511811031494, 0.1771653543307087630, 0.000000000000000000 ) ) ;
#8935 = CARTESIAN_POINT ( 'NONE',  ( -0.3996062992125986590, 0.1070741851644051723, -1.526902887139107490 ) ) ;
#8936 = CARTESIAN_POINT ( 'NONE',  ( 0.5839895013123367340, 0.2952755905511811885, 0.1292274648535926551 ) ) ;
#8937 = EDGE_CURVE ( 'NONE', #6163, #59008, #25792, .T. ) ;
#8938 = CARTESIAN_POINT ( 'NONE',  ( -0.1049643490035302024, -0.3917322834645671215, -1.009186351706036433 ) ) ;
#8939 = CIRCLE ( 'NONE', #74851, 0.1937007874015748143 ) ;
#8940 = VECTOR ( 'NONE', #5443, 39.37007874015748143 ) ;
#8941 = CARTESIAN_POINT ( 'NONE',  ( 5.785732909357575061E-17, -0.4724409448818898682, -0.4704724409448819422 ) ) ;
#8942 = DIRECTION ( 'NONE',  ( 0.000000000000000000, -1.000000000000000000, -0.000000000000000000 ) ) ;
#8943 = CARTESIAN_POINT ( 'NONE',  ( 0.1049868766404206816, -0.5023911411419708095, -0.1820866141732282451 ) ) ;
#8944 = CARTESIAN_POINT ( 'NONE',  ( -0.09842519685039295696, -0.5400638737290844871, 0.3530559997133364547 ) ) ;
#8945 = CARTESIAN_POINT ( 'NONE',  ( 1.200787401574803681, 0.07958543189024085140, 0.2665933059059887866 ) ) ;
#8946 = CARTESIAN_POINT ( 'NONE',  ( -1.272965879265091305, -0.3690944881889763329, 0.3153832671262228327 ) ) ;
#8947 = CARTESIAN_POINT ( 'NONE',  ( -1.437007874015747477, -0.5400638737290844871, 0.3530559997133364547 ) ) ;
#8948 = CARTESIAN_POINT ( 'NONE',  ( 0.5774278215223104249, 0.2306618581243848609, 0.2411417322834645549 ) ) ;
#8949 = B_SPLINE_CURVE_WITH_KNOTS ( 'NONE', 3,
 ( #49882, #49476, #43971, #11189 ),
 .UNSPECIFIED., .F., .F.,
 ( 4, 4 ),
 ( 0.02789255478306693070, 0.02946499057610776906 ),
 .UNSPECIFIED. ) ;
#8950 = CARTESIAN_POINT ( 'NONE',  ( -1.627296587926508442, 0.1283753931104748280, 0.1820866141732283561 ) ) ;
#8951 = DIRECTION ( 'NONE',  ( -3.096699300667737957E-16, 1.000000000000000000, -0.000000000000000000 ) ) ;
#8952 = CARTESIAN_POINT ( 'NONE',  ( 0.4199475065616803948, -0.6046776061558809534, -0.2411417322834644161 ) ) ;
#8953 = CARTESIAN_POINT ( 'NONE',  ( -0.3996062992125986590, 0.1070741851644051723, 0.2053805774278214813 ) ) ;
#8954 = VECTOR ( 'NONE', #38090, 39.37007874015748143 ) ;
#8955 = CARTESIAN_POINT ( 'NONE',  ( 1.548556430446194954, 0.2306618581243847221, -0.2411417322834647770 ) ) ;
#8956 = CARTESIAN_POINT ( 'NONE',  ( 1.089238845144357759, 0.05413385826771626580, -0.4176697321401330321 ) ) ;
#8957 = CARTESIAN_POINT ( 'NONE',  ( -1.528871391076114250, 0.1771653543307087075, -0.09757992244046823083 ) ) ;
#8958 = CARTESIAN_POINT ( 'NONE',  ( 1.279527559055118724, -0.4536011799217368745, -0.2665933059059886201 ) ) ;
#8959 = CARTESIAN_POINT ( 'NONE',  ( 1.574803149606299746, -0.1870078740157480879, -0.4822834645669291653 ) ) ;
#8960 = CARTESIAN_POINT ( 'NONE',  ( -0.9120734908136475250, -0.5511811023622048555, -0.09757992244046775898 ) ) ;
#8961 = CARTESIAN_POINT ( 'NONE',  ( -0.2362204724409451284, 0.4091458600556402425, -2.060367454068241511 ) ) ;
#8962 = CARTESIAN_POINT ( 'NONE',  ( 0.6561679790026253567, 0.1283753931104748280, 0.1820866141732283561 ) ) ;
#8963 = CARTESIAN_POINT ( 'NONE',  ( 0.2755905511811031494, 0.2952755905511811885, 0.000000000000000000 ) ) ;
#8964 = CARTESIAN_POINT ( 'NONE',  ( 1.213910761154856299, -0.6692913385826773087, -0.1292274648535924053 ) ) ;
#8965 = CARTESIAN_POINT ( 'NONE',  ( -0.2821522309711278487, -0.6692913385826773087, -0.1292274648535924053 ) ) ;
#8966 = CARTESIAN_POINT ( 'NONE',  ( 0.1837270341207354329, 0.1283753931104748280, 0.1820866141732283561 ) ) ;
#8967 = CARTESIAN_POINT ( 'NONE',  ( 1.417322834645670104, -0.1870078740157479769, 0.4822834645669291653 ) ) ;
#8968 = CARTESIAN_POINT ( 'NONE',  ( -0.2238009295390064879, -2.294479370626195693E-15, 0.3464511005275217603 ) ) ;
#8969 = CARTESIAN_POINT ( 'NONE',  ( -1.076115485564303809, 0.2306618581243848609, 0.2411417322834645549 ) ) ;
#8971 = CARTESIAN_POINT ( 'NONE',  ( -0.1070741851644051862, -0.3996062992125986590, -0.8595800524934383846 ) ) ;
#8970 = CARTESIAN_POINT ( 'NONE',  ( -1.443569553805773564, -0.5023911411419708095, 0.1820866141732285504 ) ) ;
#8972 = CARTESIAN_POINT ( 'NONE',  ( 1.013282927784340259, -2.226000259411765883E-16, -0.4281993546915530136 ) ) ;
#8973 = CARTESIAN_POINT ( 'NONE',  ( -0.9055118110236215490, -0.6692913385826771977, 8.415575281601705876E-17 ) ) ;
#8974 = EDGE_CURVE ( 'NONE', #41616, #66374, #33355, .T. ) ;
#8975 = CARTESIAN_POINT ( 'NONE',  ( -0.1181102362204717315, 0.2952755905511811885, 0.000000000000000000 ) ) ;
#8976 =( BOUNDED_CURVE ( )  B_SPLINE_CURVE ( 2, ( #55230, #82574, #76265, #31213, #24893, #50156, #10644, #11047, #80937, #23253, #23664, #11464, #49745 ),
 .UNSPECIFIED., .F., .F. ) 
 B_SPLINE_CURVE_WITH_KNOTS ( ( 3, 2, 2, 2, 2, 2, 3 ),
 ( 0.5369674582711644328, 0.5378787878787878451, 0.5416666666666666297, 0.5454545454545454142, 0.5492424242424241987, 0.5530303030303029832, 0.5539416326379265065 ),
 .UNSPECIFIED. ) 
 CURVE ( )  GEOMETRIC_REPRESENTATION_ITEM ( )  RATIONAL_B_SPLINE_CURVE ( ( 0.9875488213027523443, 0.9918020599134680371, 1.000000000000000000, 0.9659258262890683122, 1.000000000000000000, 0.9659258262890683122, 1.000000000000000000, 0.9659258262890683122, 1.000000000000000000, 0.9659258262890683122, 1.000000000000000000, 0.9918020599134671489, 0.9875488213027514561 ) ) 
 REPRESENTATION_ITEM ( '' )  );
#8977 = CARTESIAN_POINT ( 'NONE',  ( -0.1070741851644051862, -0.3996062992125987146, -2.906824146981627610 ) ) ;
#8978 = CARTESIAN_POINT ( 'NONE',  ( 0.2891555358219910499, 0.2891555358219910499, -2.342519685039370358 ) ) ;
#8979 = ORIENTED_EDGE ( 'NONE', *, *, #57961, .T. ) ;
#8980 = CARTESIAN_POINT ( 'NONE',  ( 0.7152230971128616943, -0.08942795157527998196, 0.3641732283464567121 ) ) ;
#8981 = CARTESIAN_POINT ( 'NONE',  ( 0.1958661417322836440, -0.3392501089628017219, -1.028871391076115360 ) ) ;
#8982 = CARTESIAN_POINT ( 'NONE',  ( 0.9448818897637802916, -0.1870078740157479769, 0.4822834645669291653 ) ) ;
#8983 = DIRECTION ( 'NONE',  ( 1.000000000000000000, -0.000000000000000000, -0.000000000000000000 ) ) ;
#8984 = CARTESIAN_POINT ( 'NONE',  ( -1.384514435695537005, 0.1771653543307087630, 0.09757992244046791164 ) ) ;
#8985 = CARTESIAN_POINT ( 'NONE',  ( 1.404199475065617708, 0.05413385826771626580, -0.4176697321401330321 ) ) ;
#8986 = CARTESIAN_POINT ( 'NONE',  ( -1.430446194225721390, -0.4281496062992124485, 0.4176697321401328655 ) ) ;
#8987 = CARTESIAN_POINT ( 'NONE',  ( 0.2867679344610365999, -0.2867679344610365999, -0.4934190044281346332 ) ) ;
#8988 = EDGE_CURVE ( 'NONE', #3939, #18816, #67404, .T. ) ;
#8989 = CARTESIAN_POINT ( 'NONE',  ( 0.1443569553805781891, 0.05413385826771626580, -0.4176697321401330321 ) ) ;
#8990 = CARTESIAN_POINT ( 'NONE',  ( -0.2821522309711278487, 0.1771653543307087630, 0.09757992244046791164 ) ) ;
#8991 = CARTESIAN_POINT ( 'NONE',  ( 0.6561679790026253567, 0.2306618581243848609, 0.2411417322834645549 ) ) ;
#8992 = CARTESIAN_POINT ( 'NONE',  ( 0.3937007874015754361, -0.1870078740157480879, -0.4822834645669291653 ) ) ;
#8993 = DIRECTION ( 'NONE',  ( 0.000000000000000000, 0.000000000000000000, 1.000000000000000000 ) ) ;
#8994 = CIRCLE ( 'NONE', #6260, 3.228346456692913424 ) ;
#8995 = CARTESIAN_POINT ( 'NONE',  ( -1.614173228346456712, 1.543375672658095610, -0.1372047244094478091 ) ) ;
#8996 = CARTESIAN_POINT ( 'NONE',  ( 0.2867679344610366554, -0.2867679344610365999, -1.669966822343518897 ) ) ;
#8997 = CARTESIAN_POINT ( 'NONE',  ( 0.9186351706036752773, 0.2306618581243847221, -0.2411417322834647770 ) ) ;
#8998 = CIRCLE ( 'NONE', #21133, 0.1771653543307086798 ) ;
#8999 = CARTESIAN_POINT ( 'NONE',  ( 5.463695987328526437E-16, -0.1870078740157479769, 0.4822834645669291653 ) ) ;
#9000 = CARTESIAN_POINT ( 'NONE',  ( -1.161417322834644716, 0.1660481256975885056, 0.3530559997133364547 ) ) ;
#9001 = CARTESIAN_POINT ( 'NONE',  ( 1.496062992125984703, -0.1870078740157480879, -0.4822834645669291653 ) ) ;
#9002 = CARTESIAN_POINT ( 'NONE',  ( 0.6824146981627303710, -0.6046776061558807314, 0.2411417322834647770 ) ) ;
#9003 = CARTESIAN_POINT ( 'NONE',  ( 0.1049643490035303689, 0.3917322834645670104, -0.7080052493438320216 ) ) ;
#9004 = CARTESIAN_POINT ( 'NONE',  ( -0.2230971128608915943, -0.4281496062992127816, -0.4176697321401328100 ) ) ;
#9005 = CARTESIAN_POINT ( 'NONE',  ( 0.7349081364829403995, 0.2306618581243848609, 0.2411417322834645549 ) ) ;
#9006 = CARTESIAN_POINT ( 'NONE',  ( 0.04593175853018440641, -0.6692913385826771977, 0.1292274648535927661 ) ) ;
#9007 = CARTESIAN_POINT ( 'NONE',  ( 0.5511811023622055217, -0.1870078740157479769, 0.3641732283464567677 ) ) ;
#9008 = CARTESIAN_POINT ( 'NONE',  ( -1.358267716535432434, 0.1660481256975883668, -0.3530559997133364547 ) ) ;
#9009 = CARTESIAN_POINT ( 'NONE',  ( -1.482939632545930975, -0.4281496062992127816, -0.4176697321401328100 ) ) ;
#9010 = CARTESIAN_POINT ( 'NONE',  ( 0.9448818897637802916, -0.1870078740157479769, 0.4822834645669291653 ) ) ;
#9011 = CARTESIAN_POINT ( 'NONE',  ( -3.937007874015748143, 1.537401574803149984, 0.4744094488188970171 ) ) ;
#9012 = CARTESIAN_POINT ( 'NONE',  ( -0.3392501089628017219, -0.1958661417322836718, -2.406824146981627166 ) ) ;
#9013 = VERTEX_POINT ( 'NONE', #3854 ) ;
#9014 = ORIENTED_EDGE ( 'NONE', *, *, #27043, .T. ) ;
#9015 = CARTESIAN_POINT ( 'NONE',  ( 1.200787401574803681, 0.1660481256975885056, 0.3530559997133364547 ) ) ;
#9016 = CARTESIAN_POINT ( 'NONE',  ( 0.6692913385826777528, 0.1771653543307087630, 0.000000000000000000 ) ) ;
#9017 = FACE_OUTER_BOUND ( 'NONE', #36036, .T. ) ;
#9018 = DIRECTION ( 'NONE',  ( -0.8660254037844433705, 0.000000000000000000, 0.4999999999999920064 ) ) ;
#9019 = CARTESIAN_POINT ( 'NONE',  ( 0.3977953519386753789, 0.03143970413924940949, -1.929133858267772839 ) ) ;
#9020 = CARTESIAN_POINT ( 'NONE',  ( 0.3392501089628018884, -0.1958661417322834220, -1.449475065616798064 ) ) ;
#9021 = CARTESIAN_POINT ( 'NONE',  ( 0.1998031496062994128, -0.3460692066303957537, -2.058398950131233640 ) ) ;
#9022 = CARTESIAN_POINT ( 'NONE',  ( 0.000000000000000000, 0.000000000000000000, 0.1574803149606299191 ) ) ;
#9023 = CARTESIAN_POINT ( 'NONE',  ( -0.9383202099737524282, -0.05778040916215522460, 0.4822834645669289988 ) ) ;
#9024 = CARTESIAN_POINT ( 'NONE',  ( 1.240157480314961314, -0.5400638737290844871, 0.3530559997133364547 ) ) ;
#9025 = VERTEX_POINT ( 'NONE', #28692 ) ;
#9026 = CARTESIAN_POINT ( 'NONE',  ( 1.607611548556431069, 0.2952755905511811885, 0.1292274648535926551 ) ) ;
#9027 = CARTESIAN_POINT ( 'NONE',  ( 1.587926509186352586, -0.3690944881889765550, -0.3153832671262227771 ) ) ;
#9028 = CONTEXT_DEPENDENT_SHAPE_REPRESENTATION ( #78331, #48041 ) ;
#9029 = CYLINDRICAL_SURFACE ( 'NONE', #80230, 0.3937007874015748254 ) ;
#9030 = CARTESIAN_POINT ( 'NONE',  ( 0.1070741851644053527, 0.3996062992125985480, -1.959973753280839892 ) ) ;
#9031 = CARTESIAN_POINT ( 'NONE',  ( -1.292650918635170010, 0.1771653543307087075, -0.09757992244046823083 ) ) ;
#9032 = CARTESIAN_POINT ( 'NONE',  ( 0.2017716535433070613, -0.2017716535433070890, 0.000000000000000000 ) ) ;
#9033 = CARTESIAN_POINT ( 'NONE',  ( 0.3805774278215230400, -0.4281496062992124485, 0.4176697321401328655 ) ) ;
#9035 = DIRECTION ( 'NONE',  ( 0.000000000000000000, 0.000000000000000000, -1.000000000000000000 ) ) ;
#9034 = CARTESIAN_POINT ( 'NONE',  ( 1.515748031496063408, 0.1660481256975885056, 0.3530559997133364547 ) ) ;
#9036 = CARTESIAN_POINT ( 'NONE',  ( -0.6627296587926503335, -0.5511811023622046335, 0.09757992244046803654 ) ) ;
#9037 = CARTESIAN_POINT ( 'NONE',  ( 0.6364829396325465405, -0.3162353388693409650, -0.4822834645669289433 ) ) ;
#9038 = CARTESIAN_POINT ( 'NONE',  ( 1.325459317585302665, -0.004921259842519870586, -0.3153832671262229437 ) ) ;
#9039 = CARTESIAN_POINT ( 'NONE',  ( -0.3917322834645668994, -0.1049643490035306742, -1.385807455871704175 ) ) ;
#9040 = CARTESIAN_POINT ( 'NONE',  ( -0.7611548556430438595, 0.1283753931104748280, 0.1820866141732283561 ) ) ;
#9041 = CARTESIAN_POINT ( 'NONE',  ( 1.509186351706037543, 0.05413385826771666132, 0.4176697321401328100 ) ) ;
#9042 = DIRECTION ( 'NONE',  ( -0.000000000000000000, 1.000000000000000000, -0.000000000000000000 ) ) ;
#9043 = CARTESIAN_POINT ( 'NONE',  ( 0.3674540682414705883, 0.2306618581243847221, -0.2411417322834647770 ) ) ;
#9044 = CARTESIAN_POINT ( 'NONE',  ( -0.8070866141732276899, 0.07958543189024071263, -0.2665933059059888421 ) ) ;
#9045 = CARTESIAN_POINT ( 'NONE',  ( -0.1181102362204717315, 0.1771653543307087630, 0.000000000000000000 ) ) ;
#9046 = CARTESIAN_POINT ( 'NONE',  ( -0.09842519685039295696, 0.1660481256975883668, -0.3530559997133364547 ) ) ;
#9047 = CARTESIAN_POINT ( 'NONE',  ( 1.653543307086614789, -0.1870078740157479769, 0.4822834645669291653 ) ) ;
#9048 = CARTESIAN_POINT ( 'NONE',  ( 0.1049643490035304799, -0.3917322834645670104, 0.07544000180346267792 ) ) ;
#9049 = CARTESIAN_POINT ( 'NONE',  ( 0.7874015748031503170, -0.1870078740157479769, 0.4822834645669291653 ) ) ;
#9050 = VECTOR ( 'NONE', #11045, 39.37007874015748143 ) ;
#9051 = VECTOR ( 'NONE', #9661, 39.37007874015748143 ) ;
#9052 = CARTESIAN_POINT ( 'NONE',  ( 0.000000000000000000, 1.724409448818897905, 0.000000000000000000 ) ) ;
#9053 = VECTOR ( 'NONE', #63209, 39.37007874015748143 ) ;
#9054 = CARTESIAN_POINT ( 'NONE',  ( -0.1265901696524986964, -0.4724409448818899238, -1.723753280839894986 ) ) ;
#9055 = CARTESIAN_POINT ( 'NONE',  ( -0.6955380577427815458, -0.4281496062992127816, -0.4176697321401328100 ) ) ;
#9056 = CARTESIAN_POINT ( 'NONE',  ( -0.1771653543307080136, -0.4536011799217367080, 0.2665933059059888421 ) ) ;
#9057 = ADVANCED_FACE ( 'NONE', ( #55583 ), #73744, .F. ) ;
#9058 = CARTESIAN_POINT ( 'NONE',  ( -1.502624671916009680, -0.3162353388693405765, 0.4822834645669290543 ) ) ;
#9059 = CARTESIAN_POINT ( 'NONE',  ( 0.3477690288713918276, -0.5511811023622048555, -0.09757992244046775898 ) ) ;
#9060 = CARTESIAN_POINT ( 'NONE',  ( -0.5905511811023615998, 0.1771653543307087630, 0.000000000000000000 ) ) ;
#9061 = CARTESIAN_POINT ( 'NONE',  ( -1.082677165354329896, 0.1660481256975885056, 0.3530559997133364547 ) ) ;
#9062 = CARTESIAN_POINT ( 'NONE',  ( -1.627296587926508442, -0.6046776061558809534, -0.2411417322834644161 ) ) ;
#9063 = CARTESIAN_POINT ( 'NONE',  ( 1.384514435695538559, 0.2952755905511810774, -0.1292274648535930714 ) ) ;
#9064 = CARTESIAN_POINT ( 'NONE',  ( 1.036394771582350938, 0.004960608223779470680, 0.3437734562760185741 ) ) ;
#9065 = CARTESIAN_POINT ( 'NONE',  ( 0.8464566929133866546, -0.4536011799217367080, 0.2665933059059888421 ) ) ;
#9066 = CARTESIAN_POINT ( 'NONE',  ( 0.5971128608923891301, 0.2952755905511810774, -0.1292274648535930714 ) ) ;
#9067 = EDGE_CURVE ( 'NONE', #31420, #71641, #54353, .T. ) ;
#9068 = CARTESIAN_POINT ( 'NONE',  ( 1.403614904275686858E-14, 1.537401574803149984, -3.937007874015761910 ) ) ;
#9069 = CARTESIAN_POINT ( 'NONE',  ( 1.292650918635171564, 0.1771653543307087630, 0.09757992244046791164 ) ) ;
#9070 = VERTEX_POINT ( 'NONE', #21965 ) ;
#9071 = B_SPLINE_CURVE_WITH_KNOTS ( 'NONE', 3,
 ( #61008, #3357, #72818, #15168, #74069, #16415, #68570 ),
 .UNSPECIFIED., .F., .F.,
 ( 4, 3, 4 ),
 ( 7.285838599102589797E-17, 0.001246232571205252914, 0.002492492258783168303 ),
 .UNSPECIFIED. ) ;
#9072 = CARTESIAN_POINT ( 'NONE',  ( -0.3996062992125985480, -7.340648628747423112E-17, -2.793307086614173151 ) ) ;
#9073 = CARTESIAN_POINT ( 'NONE',  ( -1.181102362204723644, -0.1870078740157479769, 0.3641732283464567677 ) ) ;
#9074 = CARTESIAN_POINT ( 'NONE',  ( -0.3149606299212590610, -0.1870078740157480879, -0.4822834645669291653 ) ) ;
#9075 = CARTESIAN_POINT ( 'NONE',  ( 0.4396325459317590445, -0.6692913385826771977, 0.1292274648535927661 ) ) ;
#9076 = CARTESIAN_POINT ( 'NONE',  ( -1.482939632545930975, -0.3690944881889765550, -0.3153832671262227771 ) ) ;
#9077 = CARTESIAN_POINT ( 'NONE',  ( -0.1998031496062991630, -0.3460692066303959202, -2.189632545931758489 ) ) ;
#9078 = CARTESIAN_POINT ( 'NONE',  ( -1.240157480314959759, 0.1660481256975885056, 0.3530559997133364547 ) ) ;
#9079 = CARTESIAN_POINT ( 'NONE',  ( 0.6299212598425204535, -0.1870078740157480879, -0.4822834645669291653 ) ) ;
#9080 = CARTESIAN_POINT ( 'NONE',  ( -0.09186351706036663400, -0.4281496062992124485, 0.4176697321401328655 ) ) ;
#9081 = CARTESIAN_POINT ( 'NONE',  ( 1.010498687664042716, 0.05413385826771626580, -0.4176697321401330321 ) ) ;
#9082 = CARTESIAN_POINT ( 'NONE',  ( 1.692913385826772421, 0.2952755905511811885, 0.000000000000000000 ) ) ;
#9083 = CARTESIAN_POINT ( 'NONE',  ( -0.3996062992125987146, 0.1070741851644051862, -1.292650918635170454 ) ) ;
#9084 = CARTESIAN_POINT ( 'NONE',  ( -0.2891555358219908833, -0.2891555358219912164, -1.161417322834645827 ) ) ;
#9085 = CARTESIAN_POINT ( 'NONE',  ( 0.3996062992125986035, 0.1070741851644054776, -2.329396325459317296 ) ) ;
#9086 = CARTESIAN_POINT ( 'NONE',  ( 0.2867679344610366554, 0.2867679344610366554, -0.1299212598425196485 ) ) ;
#9087 = CARTESIAN_POINT ( 'NONE',  ( 0.07217847769028949700, -0.08942795157528024563, -0.3641732283464568787 ) ) ;
#9088 = CARTESIAN_POINT ( 'NONE',  ( -0.5183727034120726440, -0.6692913385826773087, -0.1292274648535924053 ) ) ;
#9089 = CARTESIAN_POINT ( 'NONE',  ( 1.017060367454068581, -0.05778040916215560624, -0.4822834645669293319 ) ) ;
#9090 = CARTESIAN_POINT ( 'NONE',  ( -0.3420746716998660508, -0.1974969037888706924, -1.704068241469815836 ) ) ;
#9091 = CARTESIAN_POINT ( 'NONE',  ( -0.2230971128608915943, -0.004921259842519576551, 0.3153832671262227771 ) ) ;
#9092 = CARTESIAN_POINT ( 'NONE',  ( -1.049868766404198794, -0.6046776061558807314, 0.2411417322834647770 ) ) ;
#9093 = CARTESIAN_POINT ( 'NONE',  ( -1.469816272965878357, 0.2306618581243848609, 0.2411417322834645549 ) ) ;
#9094 = CARTESIAN_POINT ( 'NONE',  ( 0.2362204724409451007, -0.4091458600556402980, -1.824146981627296604 ) ) ;
#9095 = CARTESIAN_POINT ( 'NONE',  ( 0.3285422586334079686, 0.2143816077119419516, -2.755905511811022723 ) ) ;
#9096 = EDGE_LOOP ( 'NONE', ( #28412, #46874, #14400, #76473, #66041, #66129, #8076 ) ) ;
#9097 = ORIENTED_EDGE ( 'NONE', *, *, #13640, .T. ) ;
#9098 = CARTESIAN_POINT ( 'NONE',  ( 1.076115485564305141, -0.6046776061558807314, 0.2411417322834647770 ) ) ;
#9099 = CARTESIAN_POINT ( 'NONE',  ( 1.482939632545932307, -0.004921259842519870586, -0.3153832671262229437 ) ) ;
#9101 = CARTESIAN_POINT ( 'NONE',  ( -1.187664041994749731, -0.3162353388693405765, 0.4822834645669290543 ) ) ;
#9100 = CARTESIAN_POINT ( 'NONE',  ( -1.305774278215222184, 0.1771653543307087630, 0.09757992244046791164 ) ) ;
#9102 = CARTESIAN_POINT ( 'NONE',  ( -0.2867679344610364334, -0.2867679344610368219, -2.501293020176166504 ) ) ;
#9103 = CARTESIAN_POINT ( 'NONE',  ( 1.033630966599880630, -4.927456884911482678E-16, 0.4445507791589062840 ) ) ;
#9104 = CARTESIAN_POINT ( 'NONE',  ( 1.286089238845145033, -0.6046776061558809534, -0.2411417322834644161 ) ) ;
#9105 = CARTESIAN_POINT ( 'NONE',  ( -1.712598425196849572, 0.1660481256975885056, 0.3530559997133364547 ) ) ;
#9106 = CARTESIAN_POINT ( 'NONE',  ( -0.2099737532808391705, -0.6046776061558809534, -0.2411417322834644161 ) ) ;
#9107 = CARTESIAN_POINT ( 'NONE',  ( 0.01968503937007930540, 0.1660481256975885056, 0.3530559997133364547 ) ) ;
#9108 = CARTESIAN_POINT ( 'NONE',  ( -1.351706036745406347, -0.4281496062992124485, 0.4176697321401328655 ) ) ;
#9109 = CARTESIAN_POINT ( 'NONE',  ( 0.3917322834645669549, 0.1049643490035304660, 0.1056430446194224632 ) ) ;
#9110 = CARTESIAN_POINT ( 'NONE',  ( 0.2099737532808405305, 0.2306618581243847221, -0.2411417322834647770 ) ) ;
#9111 =( BOUNDED_CURVE ( )  B_SPLINE_CURVE ( 2, ( #66054, #7130, #21016, #34056, #59720, #52980, #65651 ),
 .UNSPECIFIED., .F., .F. ) 
 B_SPLINE_CURVE_WITH_KNOTS ( ( 3, 2, 2, 3 ),
 ( 0.9125000000000000888, 0.9166666666666667407, 0.9208333333333332815, 0.9250000000000000444 ),
 .UNSPECIFIED. ) 
 CURVE ( )  GEOMETRIC_REPRESENTATION_ITEM ( )  RATIONAL_B_SPLINE_CURVE ( ( 0.9999999999999991118, 0.9659258262890692004, 1.000000000000000000, 0.9659258262890683122, 1.000000000000000000, 0.9659258262890683122, 1.000000000000000000 ) ) 
 REPRESENTATION_ITEM ( '' )  );
#9112 = CARTESIAN_POINT ( 'NONE',  ( 0.2867679344610365999, -0.2867679344610365444, -1.665354330708661124 ) ) ;
#9113 = CARTESIAN_POINT ( 'NONE',  ( -1.397637795275589623, -0.4536011799217368745, -0.2665933059059886201 ) ) ;
#9114 = VERTEX_POINT ( 'NONE', #80065 ) ;
#9115 = CARTESIAN_POINT ( 'NONE',  ( 0.1974969037888706369, -0.3420746716998659953, -2.296587926509186417 ) ) ;
#9116 = ORIENTED_EDGE ( 'NONE', *, *, #12655, .F. ) ;
#9117 = CARTESIAN_POINT ( 'NONE',  ( -1.600194884102785764, 1.375860811871311373, 0.4460756753617342030 ) ) ;
#9118 = AXIS2_PLACEMENT_3D ( 'NONE', #80440, #66551, #8884 ) ;
#9119 = CARTESIAN_POINT ( 'NONE',  ( -1.469816272965878357, -0.6046776061558809534, -0.2411417322834644161 ) ) ;
#9120 = CARTESIAN_POINT ( 'NONE',  ( -1.574803149606298192, -0.1870078740157480879, -0.4822834645669291653 ) ) ;
#9121 = CARTESIAN_POINT ( 'NONE',  ( 0.3996062992125986035, 0.1070741851644054776, -0.4396325459317584339 ) ) ;
#9122 = CARTESIAN_POINT ( 'NONE',  ( -1.482939632545930975, -0.4281496062992127816, -0.4176697321401328100 ) ) ;
#9123 = CARTESIAN_POINT ( 'NONE',  ( -1.607611548556429737, -0.6692913385826771977, 0.1292274648535927661 ) ) ;
#9124 = CARTESIAN_POINT ( 'NONE',  ( -0.9645669291338576645, 0.1660481256975883391, -0.3530559997133364547 ) ) ;
#9125 = CARTESIAN_POINT ( 'NONE',  ( -1.076935383196057305, 2.559055118110236560, -0.3149606299212599492 ) ) ;
#9126 = CARTESIAN_POINT ( 'NONE',  ( -0.1049643490035302024, -0.3917322834645671215, 0.0006561679790025351077 ) ) ;
#9127 = CARTESIAN_POINT ( 'NONE',  ( -0.3608923884514428360, 0.1771653543307087630, 0.09757992244046791164 ) ) ;
#9128 = CARTESIAN_POINT ( 'NONE',  ( -0.6496062992125976043, -0.4536011799217367080, 0.2665933059059888421 ) ) ;
#9129 = CARTESIAN_POINT ( 'NONE',  ( -1.299212598425196097, 0.2952755905511811885, 0.000000000000000000 ) ) ;
#9130 = CARTESIAN_POINT ( 'NONE',  ( 0.9514435695538062676, -0.05778040916215522460, 0.4822834645669289988 ) ) ;
#9131 = CARTESIAN_POINT ( 'NONE',  ( -0.8464566929133852113, 0.1660481256975885056, 0.3530559997133364547 ) ) ;
#9132 = CARTESIAN_POINT ( 'NONE',  ( -0.3392501089628017219, -0.1958661417322836718, -0.04461942257217842850 ) ) ;
#9133 = ORIENTED_EDGE ( 'NONE', *, *, #19008, .F. ) ;
#9134 = CARTESIAN_POINT ( 'NONE',  ( -1.351706036745406347, -0.4281496062992124485, 0.4176697321401328655 ) ) ;
#9135 = CARTESIAN_POINT ( 'NONE',  ( -0.7773926554473638006, -2.191421614605370878E-15, 0.4445507791589071167 ) ) ;
#9136 = CARTESIAN_POINT ( 'NONE',  ( 0.000000000000000000, 0.000000000000000000, 0.000000000000000000 ) ) ;
#9137 = CARTESIAN_POINT ( 'NONE',  ( -0.4091458600556402980, -0.2362204724409451284, -1.312335958005249381 ) ) ;
#9138 = CARTESIAN_POINT ( 'NONE',  ( 1.882930639362819347, 1.098283573398303403, -0.1802708669123839202 ) ) ;
#9139 = CARTESIAN_POINT ( 'NONE',  ( 0.1958661417322836440, -0.3392501089628017219, -0.7139107611548556331 ) ) ;
#9140 = CARTESIAN_POINT ( 'NONE',  ( 0.1958661417322836440, -0.3392501089628017219, -2.223753280839895208 ) ) ;
#9141 = CARTESIAN_POINT ( 'NONE',  ( -0.3149606299212590610, -0.1870078740157480879, -0.4822834645669291653 ) ) ;
#9142 = CARTESIAN_POINT ( 'NONE',  ( 1.259842519685040019, -0.1870078740157480879, -0.4822834645669291653 ) ) ;
#9143 = CARTESIAN_POINT ( 'NONE',  ( -0.3996062992125986590, 0.1070741851644051723, 0.04790026246719156916 ) ) ;
#9145 = DIRECTION ( 'NONE',  ( -0.000000000000000000, 1.000000000000000000, -0.000000000000000000 ) ) ;
#9144 = CARTESIAN_POINT ( 'NONE',  ( -1.522309711286088607, 0.2306618581243847221, -0.2411417322834647770 ) ) ;
#9146 = CARTESIAN_POINT ( 'NONE',  ( -1.272965879265091305, -0.4281496062992124485, 0.4176697321401328655 ) ) ;
#9147 = CARTESIAN_POINT ( 'NONE',  ( -0.9645669291338575535, -0.5400638737290844871, 0.3530559997133364547 ) ) ;
#9148 = CARTESIAN_POINT ( 'NONE',  ( -0.2867679344610366554, 0.2867679344610365444, -0.09971821702655986330 ) ) ;
#9149 = CARTESIAN_POINT ( 'NONE',  ( 0.4396325459317590445, -0.5511811023622046335, 0.09757992244046803654 ) ) ;
#9150 = CARTESIAN_POINT ( 'NONE',  ( -0.1049643490035301885, -0.3917322834645671215, -0.6292650918635172008 ) ) ;
#9151 = CARTESIAN_POINT ( 'NONE',  ( 0.3018372703412079971, -0.004921259842519870586, -0.3153832671262229437 ) ) ;
#9152 = CARTESIAN_POINT ( 'NONE',  ( 1.076115485564305141, -0.5023911411419708095, 0.1820866141732285504 ) ) ;
#9153 = CARTESIAN_POINT ( 'NONE',  ( 0.8792650918635177559, -0.4281496062992127816, -0.4176697321401328100 ) ) ;
#9154 = CARTESIAN_POINT ( 'NONE',  ( -0.4724409448818890911, -0.1870078740157480601, -0.3641732283464567677 ) ) ;
#9155 = CARTESIAN_POINT ( 'NONE',  ( 0.2867679344610365999, -0.2867679344610365444, -1.822834645669291653 ) ) ;
#9156 = CARTESIAN_POINT ( 'NONE',  ( -1.115485564304461219, 0.05413385826771626580, -0.4176697321401330321 ) ) ;
#9157 = CARTESIAN_POINT ( 'NONE',  ( -1.299212598425196097, 0.1771653543307087630, 0.000000000000000000 ) ) ;
#9158 = CARTESIAN_POINT ( 'NONE',  ( 0.3458507752293908943, 0.3458507752293908943, -0.5295275590551181688 ) ) ;
#9159 = CARTESIAN_POINT ( 'NONE',  ( -0.8989501312335946848, -0.5511811023622046335, 0.09757992244046803654 ) ) ;
#9160 = EDGE_CURVE ( 'NONE', #28368, #3377, #48571, .T. ) ;
#9161 = CARTESIAN_POINT ( 'NONE',  ( -0.2624671916010490880, -0.6046776061558807314, 0.2411417322834647770 ) ) ;
#9162 = CARTESIAN_POINT ( 'NONE',  ( -3.937007874015748143, 1.537401574803149984, -2.901595197523589142E-16 ) ) ;
#9163 = CARTESIAN_POINT ( 'NONE',  ( 0.5380577427821529035, -0.004921259842519870586, -0.3153832671262229437 ) ) ;
#9164 = CARTESIAN_POINT ( 'NONE',  ( -0.4461942257217840213, 0.1283753931104748280, 0.1820866141732283561 ) ) ;
#9165 = CARTESIAN_POINT ( 'NONE',  ( -0.8858267716535425107, -0.5400638737290844871, 0.3530559997133364547 ) ) ;
#9166 = CARTESIAN_POINT ( 'NONE',  ( -1.574803149606298636, -0.1870078740157479769, 0.4822834645669291653 ) ) ;
#9167 = CARTESIAN_POINT ( 'NONE',  ( 0.2362204724409449064, 0.4091458600556404646, -1.953412073490813805 ) ) ;
#9168 = CARTESIAN_POINT ( 'NONE',  ( 0.006561679790026889343, -0.3162353388693409650, -0.4822834645669289433 ) ) ;
#9169 = EDGE_LOOP ( 'NONE', ( #16679, #10460, #9228, #11234 ) ) ;
#9170 = CARTESIAN_POINT ( 'NONE',  ( 0.1998031496062994128, -0.3460692066303957537, -1.428477690288713964 ) ) ;
#9171 = CARTESIAN_POINT ( 'NONE',  ( 1.437007874015748810, 0.1660481256975885056, 0.3530559997133364547 ) ) ;
#9172 = CARTESIAN_POINT ( 'NONE',  ( -0.4199475065616791736, 0.1283753931104746893, -0.1820866141732285504 ) ) ;
#9173 = CARTESIAN_POINT ( 'NONE',  ( -0.2230971128608915943, -0.4281496062992127816, -0.4176697321401328100 ) ) ;
#9174 = CARTESIAN_POINT ( 'NONE',  ( -1.456692913385826182, 0.2952755905511811885, 0.000000000000000000 ) ) ;
#9175 = CARTESIAN_POINT ( 'NONE',  ( 1.673228346456693494, 0.1660481256975885056, 0.3530559997133364547 ) ) ;
#9176 = CARTESIAN_POINT ( 'NONE',  ( 1.345144356955381593, -0.05778040916215522460, 0.4822834645669289988 ) ) ;
#9177 = CARTESIAN_POINT ( 'NONE',  ( -0.6233595800524928121, -0.08942795157527998196, 0.3641732283464567121 ) ) ;
#9178 = CARTESIAN_POINT ( 'NONE',  ( -1.090429162302622101, -1.142320075227303543E-15, 0.3627985898453523483 ) ) ;
#9179 = CARTESIAN_POINT ( 'NONE',  ( -0.3996062992125987146, 0.1070741851644051862, -0.1902887139107611314 ) ) ;
#9180 = CARTESIAN_POINT ( 'NONE',  ( 0.3392501089628018884, -0.1958661417322833942, -2.936371021818584115 ) ) ;
#9181 = FACE_BOUND ( 'NONE', #58252, .T. ) ;
#9182 = CARTESIAN_POINT ( 'NONE',  ( 1.358267716535433323, -0.4536011799217368745, -0.2665933059059886201 ) ) ;
#9183 = CARTESIAN_POINT ( 'NONE',  ( -1.627296587926508442, -0.6046776061558809534, -0.2411417322834644161 ) ) ;
#9184 = CARTESIAN_POINT ( 'NONE',  ( 1.023622047244095112, -0.1870078740157480879, -0.4822834645669291653 ) ) ;
#9185 = CARTESIAN_POINT ( 'NONE',  ( 0.2867679344610365999, -0.2867679344610365444, -2.230314960629921295 ) ) ;
#9186 = CARTESIAN_POINT ( 'NONE',  ( 1.161417322834646493, -0.4536011799217367080, 0.2665933059059888421 ) ) ;
#9187 = CARTESIAN_POINT ( 'NONE',  ( 0.1246719160104994284, 0.2952755905511810774, -0.1292274648535930714 ) ) ;
#9188 = CARTESIAN_POINT ( 'NONE',  ( -0.2493438320209966919, -0.4281496062992124485, 0.4176697321401328655 ) ) ;
#9189 = CARTESIAN_POINT ( 'NONE',  ( -3.908320185825792326, 1.537401574803149984, 0.4744094488188970171 ) ) ;
#9190 = CARTESIAN_POINT ( 'NONE',  ( -0.4724409448818898682, -8.678599364036362592E-17, -0.6692913385826770867 ) ) ;
#9191 = CARTESIAN_POINT ( 'NONE',  ( 0.06840103802056105020, -1.283732188437465593E-15, -0.4281993546915538462 ) ) ;
#9192 = CARTESIAN_POINT ( 'NONE',  ( 0.1443569553805781891, -0.3690944881889763329, 0.3153832671262228327 ) ) ;
#9193 = ORIENTED_EDGE ( 'NONE', *, *, #49555, .F. ) ;
#9194 = CARTESIAN_POINT ( 'NONE',  ( 0.2867679344610366554, -0.2867679344610365999, -0.4101243026584795448 ) ) ;
#9195 = ORIENTED_EDGE ( 'NONE', *, *, #9262, .T. ) ;
#9196 = CARTESIAN_POINT ( 'NONE',  ( -0.4002624671916004129, -0.05778040916215560624, -0.4822834645669293319 ) ) ;
#9197 = CARTESIAN_POINT ( 'NONE',  ( 1.161417322834646271, 0.1660481256975883668, -0.3530559997133364547 ) ) ;
#9198 = CARTESIAN_POINT ( 'NONE',  ( 0.2099737532808405305, -0.6046776061558807314, 0.2411417322834647770 ) ) ;
#9199 = CARTESIAN_POINT ( 'NONE',  ( -0.1706036745406816491, -0.004921259842519870586, -0.3153832671262229437 ) ) ;
#9200 = CARTESIAN_POINT ( 'NONE',  ( 0.6627296587926517768, -0.6692913385826773087, -0.1292274648535924053 ) ) ;
#9201 = CARTESIAN_POINT ( 'NONE',  ( -1.089238845144356427, -0.4281496062992127816, -0.4176697321401328100 ) ) ;
#9202 = CARTESIAN_POINT ( 'NONE',  ( -0.5446194225721777693, -0.3162353388693409650, -0.4822834645669289433 ) ) ;
#9203 = CARTESIAN_POINT ( 'NONE',  ( -0.9580052493438311334, -0.4281496062992124485, 0.4176697321401328655 ) ) ;
#9204 = CARTESIAN_POINT ( 'NONE',  ( 1.141732283464567566, 0.2952755905511811885, 0.000000000000000000 ) ) ;
#9205 = CARTESIAN_POINT ( 'NONE',  ( 0.8464566929133865436, 0.1660481256975883668, -0.3530559997133364547 ) ) ;
#9206 = CARTESIAN_POINT ( 'NONE',  ( 0.7677165354330716118, 0.1660481256975883668, -0.3530559997133364547 ) ) ;
#9207 = CARTESIAN_POINT ( 'NONE',  ( -0.3392501089628017219, -0.1958661417322836718, -0.6745406824146981117 ) ) ;
#9208 = CARTESIAN_POINT ( 'NONE',  ( -0.07217847769028787330, -0.08942795157527998196, 0.3641732283464567121 ) ) ;
#9209 = ORIENTED_EDGE ( 'NONE', *, *, #76941, .F. ) ;
#9210 = CARTESIAN_POINT ( 'NONE',  ( 0.1058382717557499880, 0.3949938075777411073, -0.9383202099737534274 ) ) ;
#9211 = ORIENTED_EDGE ( 'NONE', *, *, #61964, .F. ) ;
#9212 = CARTESIAN_POINT ( 'NONE',  ( -0.8595800524934373854, -0.2845877964562161244, -0.3641732283464567121 ) ) ;
#9213 = CARTESIAN_POINT ( 'NONE',  ( -0.6364829396325453192, -0.05778040916215560624, -0.4822834645669293319 ) ) ;
#9214 = CARTESIAN_POINT ( 'NONE',  ( 2.869792031447826908, 1.067551433859866616, 0.06782095098396989652 ) ) ;
#9215 = CARTESIAN_POINT ( 'NONE',  ( -0.2362204724409442680, -0.1870078740157480879, -0.4822834645669291653 ) ) ;
#9216 = CARTESIAN_POINT ( 'NONE',  ( -0.2296587926509179312, -0.3162353388693409650, -0.4822834645669289433 ) ) ;
#9217 = CARTESIAN_POINT ( 'NONE',  ( -1.364829396325458521, -0.6046776061558807314, 0.2411417322834647770 ) ) ;
#9218 = CARTESIAN_POINT ( 'NONE',  ( -1.391076115485563758, 0.2306618581243848609, 0.2411417322834645549 ) ) ;
#9219 = CARTESIAN_POINT ( 'NONE',  ( 1.128608923884515169, -0.5023911411419708095, -0.1820866141732282451 ) ) ;
#9220 = CARTESIAN_POINT ( 'NONE',  ( -1.157146581871515012E-16, 0.4724409448818898682, -0.3917322834645669549 ) ) ;
#9221 = CARTESIAN_POINT ( 'NONE',  ( 0.2747288752779719623, 0.1086799599621180723, 5.842342907282080056 ) ) ;
#9222 = CARTESIAN_POINT ( 'NONE',  ( 0.3740157480314966754, 0.07958543189024071263, -0.2665933059059888421 ) ) ;
#9223 = CARTESIAN_POINT ( 'NONE',  ( 0.2296587926509192634, -0.3162353388693405765, 0.4822834645669290543 ) ) ;
#9224 = CARTESIAN_POINT ( 'NONE',  ( 0.1837270341207357105, -0.6046776061558809534, -0.2411417322834644161 ) ) ;
#9225 = ORIENTED_EDGE ( 'NONE', *, *, #69615, .T. ) ;
#9226 = CARTESIAN_POINT ( 'NONE',  ( 0.3996062992125986035, 0.1070741851644054776, -1.699475065616798064 ) ) ;
#9227 = CARTESIAN_POINT ( 'NONE',  ( -1.604771003085130321, 1.002618919725274393, 0.1466069496707742281 ) ) ;
#9228 = ORIENTED_EDGE ( 'NONE', *, *, #53323, .F. ) ;
#9229 = CARTESIAN_POINT ( 'NONE',  ( -0.3460692066303957537, -0.1998031496062994405, -1.231627296587926468 ) ) ;
#9230 = CARTESIAN_POINT ( 'NONE',  ( 0.3996062992125986035, -0.1070741851644052972, -0.6607611548556431291 ) ) ;
#9231 = CARTESIAN_POINT ( 'NONE',  ( -0.3871391076115479057, -0.3162353388693409650, -0.4822834645669289433 ) ) ;
#9232 = CARTESIAN_POINT ( 'NONE',  ( 0.4724409448818897572, -0.1265901696524988906, -0.1115485564304461719 ) ) ;
#9233 = B_SPLINE_CURVE_WITH_KNOTS ( 'NONE', 3,
 ( #16723, #61316, #15902, #60904 ),
 .UNSPECIFIED., .F., .F.,
 ( 4, 4 ),
 ( 0.000000000000000000, 0.0007402370886711635454 ),
 .UNSPECIFIED. ) ;
#9234 = CARTESIAN_POINT ( 'NONE',  ( -0.3917322834645671215, 0.1049643490035301469, -2.637139107611548461 ) ) ;
#9235 = CARTESIAN_POINT ( 'NONE',  ( 1.666666666666667185, 0.05413385826771666132, 0.4176697321401328100 ) ) ;
#9236 = CARTESIAN_POINT ( 'NONE',  ( 1.036745406824147508, -0.4281496062992127816, -0.4176697321401328100 ) ) ;
#9237 = CARTESIAN_POINT ( 'NONE',  ( 0.8333333333333340365, -0.6692913385826771977, 0.1292274648535927661 ) ) ;
#9238 = CARTESIAN_POINT ( 'NONE',  ( -0.7742782152230962556, -0.3690944881889765550, -0.3153832671262227771 ) ) ;
#9239 = CARTESIAN_POINT ( 'NONE',  ( -0.1443569553805768291, 0.05413385826771666132, 0.4176697321401328100 ) ) ;
#9240 = CARTESIAN_POINT ( 'NONE',  ( 0.4724409448818896462, 0.1265901696524990294, -2.091207349081364519 ) ) ;
#9241 = CARTESIAN_POINT ( 'NONE',  ( 0.1049868766404206816, 0.1283753931104748280, 0.1820866141732283561 ) ) ;
#9242 = CARTESIAN_POINT ( 'NONE',  ( -0.3083989501312330295, -0.05778040916215522460, 0.4822834645669289988 ) ) ;
#9244 = B_SPLINE_CURVE_WITH_KNOTS ( 'NONE', 3,
 ( #71082, #52114, #45802, #57599 ),
 .UNSPECIFIED., .F., .F.,
 ( 4, 4 ),
 ( 9.341771812940338307E-18, 0.001510660848364197726 ),
 .UNSPECIFIED. ) ;
#9243 = CARTESIAN_POINT ( 'NONE',  ( 0.3949938075777408852, 0.1058382717557500435, -1.776246719160105236 ) ) ;
#9245 = CARTESIAN_POINT ( 'NONE',  ( 1.574803149606299746, -0.1870078740157479769, 0.3641732283464567677 ) ) ;
#9246 = CARTESIAN_POINT ( 'NONE',  ( 0.09186351706036799403, -0.3690944881889765550, -0.3153832671262227771 ) ) ;
#9247 = CARTESIAN_POINT ( 'NONE',  ( 1.666666666666667185, -0.004921259842519576551, 0.3153832671262227771 ) ) ;
#9248 = CARTESIAN_POINT ( 'NONE',  ( -1.207349081364828880, 0.2306618581243847221, -0.2411417322834647770 ) ) ;
#9249 = CARTESIAN_POINT ( 'NONE',  ( -0.9120734908136475250, -0.5511811023622048555, -0.09757992244046775898 ) ) ;
#9250 = CARTESIAN_POINT ( 'NONE',  ( -0.2362204724409451284, 0.4091458600556402425, -2.294619422572178102 ) ) ;
#9251 = CARTESIAN_POINT ( 'NONE',  ( -1.056430446194224881, 0.2952755905511810774, -0.1292274648535930714 ) ) ;
#9252 = CARTESIAN_POINT ( 'NONE',  ( -0.05249343832020911260, 0.2306618581243848609, 0.2411417322834645549 ) ) ;
#9253 = CARTESIAN_POINT ( 'NONE',  ( -0.3996062992125985480, -7.340648628747423112E-17, -2.478346456692913868 ) ) ;
#9254 = ADVANCED_FACE ( 'NONE', ( #22383 ), #52586, .F. ) ;
#9255 = CARTESIAN_POINT ( 'NONE',  ( 0.3392501089628018329, 0.1958661417322835052, -2.415991182905824708 ) ) ;
#9256 = CARTESIAN_POINT ( 'NONE',  ( 0.5314960629920859603, 2.755905511811024056, 3.821484228344198986 ) ) ;
#9257 = CARTESIAN_POINT ( 'NONE',  ( 0.2427821522309719648, -0.08942795157527998196, 0.3641732283464567121 ) ) ;
#9258 = CARTESIAN_POINT ( 'NONE',  ( 0.9908136482939640111, 0.2952755905511810774, -0.1292274648535930714 ) ) ;
#9259 = CARTESIAN_POINT ( 'NONE',  ( -1.030183727034119867, -0.08942795157528024563, -0.3641732283464568787 ) ) ;
#9260 = CARTESIAN_POINT ( 'NONE',  ( 1.194225721784777594, 0.05413385826771666132, 0.4176697321401328100 ) ) ;
#9261 = CARTESIAN_POINT ( 'NONE',  ( -1.423884514435694859, -0.2845877964562159024, 0.3641732283464567677 ) ) ;
#9262 = EDGE_CURVE ( 'NONE', #71339, #38980, #26293, .T. ) ;
#9263 = CARTESIAN_POINT ( 'NONE',  ( -0.4199475065616791736, 0.2306618581243847221, -0.2411417322834647770 ) ) ;
#9264 = CARTESIAN_POINT ( 'NONE',  ( 0.06561679790026316017, -0.3690944881889763329, 0.3153832671262228327 ) ) ;
#9265 = DIRECTION ( 'NONE',  ( 1.000000000000000000, 0.000000000000000000, -0.000000000000000000 ) ) ;
#9266 = CARTESIAN_POINT ( 'NONE',  ( 0.6496062992125991586, 0.07958543189024085140, 0.2665933059059887866 ) ) ;
#9267 = CARTESIAN_POINT ( 'NONE',  ( -0.05249343832020911260, 0.2306618581243848609, 0.2411417322834645549 ) ) ;
#9268 = CARTESIAN_POINT ( 'NONE',  ( -0.3996062992125985480, -7.340648628747423112E-17, -0.2736220472440945017 ) ) ;
#9269 = CARTESIAN_POINT ( 'NONE',  ( -0.8595800524934373854, -0.3162353388693409650, -0.4822834645669289433 ) ) ;
#9270 = CARTESIAN_POINT ( 'NONE',  ( -0.2867679344610364334, -0.2867679344610367109, -1.718503937007874072 ) ) ;
#9271 = CARTESIAN_POINT ( 'NONE',  ( 0.9055118110236227702, -0.5511811023622047445, 6.969142054262312111E-17 ) ) ;
#9272 = CARTESIAN_POINT ( 'NONE',  ( 0.1837270341207357105, -0.6046776061558809534, -0.2411417322834644161 ) ) ;
#9273 = CARTESIAN_POINT ( 'NONE',  ( -0.2165354330708654795, 0.1660481256975885056, 0.3530559997133364547 ) ) ;
#9274 = CARTESIAN_POINT ( 'NONE',  ( -0.5052493438320203589, 0.1771653543307087075, -0.09757992244046823083 ) ) ;
#9275 = LINE ( 'NONE', #41257, #44043 ) ;
#9276 = CARTESIAN_POINT ( 'NONE',  ( -0.6496062992125976043, 0.07958543189024071263, -0.2665933059059888421 ) ) ;
#9277 = CARTESIAN_POINT ( 'NONE',  ( 0.3280839895013130669, -0.4281496062992127816, -0.4176697321401328100 ) ) ;
#9278 = CARTESIAN_POINT ( 'NONE',  ( -0.9055118110236215490, 0.1771653543307087630, 0.000000000000000000 ) ) ;
#9279 = CARTESIAN_POINT ( 'NONE',  ( 0.3996062992125986035, -0.1070741851644052972, -0.9757217847769029673 ) ) ;
#9280 = CARTESIAN_POINT ( 'NONE',  ( -1.115485564304461219, 0.05413385826771626580, -0.4176697321401330321 ) ) ;
#9281 = LINE ( 'NONE', #8447, #78434 ) ;
#9282 = VERTEX_POINT ( 'NONE', #60268 ) ;
#9283 = CARTESIAN_POINT ( 'NONE',  ( -1.167979002624671470, -0.3690944881889765550, -0.3153832671262227771 ) ) ;
#9284 = CARTESIAN_POINT ( 'NONE',  ( -0.3937007874015740483, -0.1870078740157480879, -0.4822834645669291653 ) ) ;
#9285 = CARTESIAN_POINT ( 'NONE',  ( 0.3964540044758441684, 0.009627693921947956882, -1.220472440942466541 ) ) ;
#9286 = CARTESIAN_POINT ( 'NONE',  ( -1.187664041994749731, -0.3162353388693405765, 0.4822834645669290543 ) ) ;
#9287 = CARTESIAN_POINT ( 'NONE',  ( 2.795275590551181466, 2.793565526369266916, 0.000000000000000000 ) ) ;
#9288 = CARTESIAN_POINT ( 'NONE',  ( 1.476377952755906442, -0.5400638737290844871, 0.3530559997133364547 ) ) ;
#9289 = CARTESIAN_POINT ( 'NONE',  ( 0.7086614173228353852, -0.1870078740157479769, 0.4822834645669291653 ) ) ;
#9290 = DIRECTION ( 'NONE',  ( 0.000000000000000000, -1.000000000000000000, 0.000000000000000000 ) ) ;
#9291 = DIRECTION ( 'NONE',  ( -3.096699300667737957E-16, 1.000000000000000000, -0.000000000000000000 ) ) ;
#9292 = B_SPLINE_CURVE_WITH_KNOTS ( 'NONE', 3,
 ( #26792, #52449, #71839, #14188, #7868, #33532, #22568 ),
 .UNSPECIFIED., .F., .F.,
 ( 4, 3, 4 ),
 ( 5.551115123125782702E-17, 0.001246230184515611638, 0.002492489877932689731 ),
 .UNSPECIFIED. ) ;
#9293 = CARTESIAN_POINT ( 'NONE',  ( 1.456692913385827515, 0.1771653543307087630, 0.000000000000000000 ) ) ;
#9294 = CARTESIAN_POINT ( 'NONE',  ( 0.1998031496062992740, 0.3460692066303959757, -0.3018372703412073865 ) ) ;
#9295 = VERTEX_POINT ( 'NONE', #3440 ) ;
#9296 = CARTESIAN_POINT ( 'NONE',  ( -0.6627296587926501115, 0.1771653543307087075, -0.09757992244046823083 ) ) ;
#9297 = CARTESIAN_POINT ( 'NONE',  ( -0.3392501089628017219, -0.1958661417322836718, -2.406824146981627166 ) ) ;
#9298 = EDGE_LOOP ( 'NONE', ( #39317, #3639, #72459, #73369 ) ) ;
#9299 = CARTESIAN_POINT ( 'NONE',  ( 0.9251968503937015864, -0.5400638737290844871, 0.3530559997133364547 ) ) ;
#9300 = CARTESIAN_POINT ( 'NONE',  ( -0.006561679790025524116, -0.3162353388693405765, 0.4822834645669290543 ) ) ;
#9301 = CARTESIAN_POINT ( 'NONE',  ( -0.5905511811023613777, -0.6692913385826771977, 8.415575281601705876E-17 ) ) ;
#9302 = CARTESIAN_POINT ( 'NONE',  ( 1.286089238845145033, -0.6046776061558809534, -0.2411417322834644161 ) ) ;
#9303 = CARTESIAN_POINT ( 'NONE',  ( -1.496062992125983815, -0.1870078740157479769, 0.3641732283464567677 ) ) ;
#9304 = CARTESIAN_POINT ( 'NONE',  ( -0.7478466213799872531, 2.204724409448818978, -0.5309055118110235227 ) ) ;
#9305 = CARTESIAN_POINT ( 'NONE',  ( 0.4658792650918641698, -0.05778040916215560624, -0.4822834645669293319 ) ) ;
#9306 = CARTESIAN_POINT ( 'NONE',  ( -0.7480314960629914633, -0.6692913385826771977, 8.415575281601705876E-17 ) ) ;
#9307 = CARTESIAN_POINT ( 'NONE',  ( 0.1049643490035304522, -0.3917322834645668994, -1.425177534611861585 ) ) ;
#9308 = CARTESIAN_POINT ( 'NONE',  ( -1.312335958005248715, 0.2306618581243848609, 0.2411417322834645549 ) ) ;
#9309 = CARTESIAN_POINT ( 'NONE',  ( 0.1180926326102879620, 1.077616795999332133, -2.860488110875698542 ) ) ;
#9310 = CARTESIAN_POINT ( 'NONE',  ( 1.122047244094488860, -0.5400638737290845981, -0.3530559997133363437 ) ) ;
#9311 = CARTESIAN_POINT ( 'NONE',  ( 1.200787401574803681, 0.07958543189024085140, 0.2665933059059887866 ) ) ;
#9312 = ORIENTED_EDGE ( 'NONE', *, *, #38110, .T. ) ;
#9313 = CARTESIAN_POINT ( 'NONE',  ( 0.3949938075777409963, 2.418639510665530435E-17, 0.03937007874015741732 ) ) ;
#9314 = CARTESIAN_POINT ( 'NONE',  ( -0.4199475065616791736, -0.6046776061558807314, 0.2411417322834647770 ) ) ;
#9315 = ORIENTED_EDGE ( 'NONE', *, *, #25445, .T. ) ;
#9316 = CARTESIAN_POINT ( 'NONE',  ( 0.2296587926509192634, -0.08942795157528024563, -0.3641732283464568787 ) ) ;
#9317 = CARTESIAN_POINT ( 'NONE',  ( -1.259842519685038686, -0.1870078740157479769, 0.4822834645669291653 ) ) ;
#9318 = CARTESIAN_POINT ( 'NONE',  ( 1.115485564304462551, 0.05413385826771666132, 0.4176697321401328100 ) ) ;
#9319 = CARTESIAN_POINT ( 'NONE',  ( 0.7217847769028878924, -0.4281496062992127816, -0.4176697321401328100 ) ) ;
#9320 = CARTESIAN_POINT ( 'NONE',  ( -0.1706036745406816491, -0.4281496062992124485, 0.4176697321401328655 ) ) ;
#9321 = CARTESIAN_POINT ( 'NONE',  ( -0.8923884514435688198, -0.6046776061558807314, 0.2411417322834647770 ) ) ;
#9322 = CARTESIAN_POINT ( 'NONE',  ( -0.3917322834645671215, 0.1049643490035301469, -2.322178477690288734 ) ) ;
#9323 = CARTESIAN_POINT ( 'NONE',  ( -1.469816272965878357, -0.6046776061558809534, -0.2411417322834644161 ) ) ;
#9324 = CARTESIAN_POINT ( 'NONE',  ( -0.6299212598425188991, -0.1870078740157480879, -0.4822834645669291653 ) ) ;
#9325 = CARTESIAN_POINT ( 'NONE',  ( -0.5249343832020990641, 0.1283753931104748280, 0.1820866141732283561 ) ) ;
#9326 = CARTESIAN_POINT ( 'NONE',  ( 1.279527559055118724, -0.5400638737290845981, -0.3530559997133363437 ) ) ;
#9327 = DIRECTION ( 'NONE',  ( 0.000000000000000000, 0.000000000000000000, 1.000000000000000000 ) ) ;
#9328 = CARTESIAN_POINT ( 'NONE',  ( -0.9908136482939626788, -0.6692913385826773087, -0.1292274648535924053 ) ) ;
#9329 = CARTESIAN_POINT ( 'NONE',  ( -0.1998031496062994405, 0.3460692066303957537, -0.08989501312335958227 ) ) ;
#9330 = CARTESIAN_POINT ( 'NONE',  ( 0.6758530183727039509, 0.2952755905511810774, -0.1292274648535930714 ) ) ;
#9331 = CARTESIAN_POINT ( 'NONE',  ( 0.3996062992125986035, 0.1070741851644054776, -1.699475065616798064 ) ) ;
#9332 = CARTESIAN_POINT ( 'NONE',  ( -0.6743677390038179675, 1.919528098118540305, -0.5309055118110235227 ) ) ;
#9333 = CARTESIAN_POINT ( 'NONE',  ( -0.04593175853018302557, 0.2952755905511811885, 0.1292274648535926551 ) ) ;
#9334 = CARTESIAN_POINT ( 'NONE',  ( -1.017060367454067249, -0.08942795157527998196, 0.3641732283464567121 ) ) ;
#9335 = CARTESIAN_POINT ( 'NONE',  ( 1.115485564304462551, -0.3690944881889765550, -0.3153832671262227771 ) ) ;
#9336 = CARTESIAN_POINT ( 'NONE',  ( -1.157146581871515012E-16, 0.4724409448818898682, -0.7066929133858268486 ) ) ;
#9337 = CARTESIAN_POINT ( 'NONE',  ( 1.122047244094488860, -0.4536011799217368745, -0.2665933059059886201 ) ) ;
#9338 = VECTOR ( 'NONE', #52257, 39.37007874015748143 ) ;
#9339 = CARTESIAN_POINT ( 'NONE',  ( 0.7939632545931766261, -0.05778040916215522460, 0.4822834645669289988 ) ) ;
#9340 = CARTESIAN_POINT ( 'NONE',  ( -0.1974969037888704149, -0.3420746716998661063, -0.6148293963254595207 ) ) ;
#9341 = CARTESIAN_POINT ( 'NONE',  ( -0.4002624671916004129, -0.05778040916215560624, -0.4822834645669293319 ) ) ;
#9342 = DIRECTION ( 'NONE',  ( -1.000000000000000000, -8.805702923740138355E-17, 0.000000000000000000 ) ) ;
#9343 = CARTESIAN_POINT ( 'NONE',  ( 1.502624671916010790, -0.2845877964562161244, -0.3641732283464567121 ) ) ;
#9344 = CARTESIAN_POINT ( 'NONE',  ( -0.6758530183727028406, -0.6692913385826773087, -0.1292274648535924053 ) ) ;
#9345 = CARTESIAN_POINT ( 'NONE',  ( 0.3949938075777408852, 0.1058382717557500435, -0.3589238845144356871 ) ) ;
#9346 = CARTESIAN_POINT ( 'NONE',  ( 1.463254593175853824, -0.6692913385826771977, 0.1292274648535927661 ) ) ;
#9347 = CARTESIAN_POINT ( 'NONE',  ( 0.2493438320209980519, -0.4281496062992127816, -0.4176697321401328100 ) ) ;
#9348 = CARTESIAN_POINT ( 'NONE',  ( 0.4461942257217856311, 0.1283753931104746893, -0.1820866141732285504 ) ) ;
#9349 = PLANE ( 'NONE',  #53314 ) ;
#9350 = CARTESIAN_POINT ( 'NONE',  ( 0.6036745406824154392, 0.1283753931104746893, -0.1820866141732285504 ) ) ;
#9351 = DIRECTION ( 'NONE',  ( 0.000000000000000000, 0.000000000000000000, 1.000000000000000000 ) ) ;
#9352 = CARTESIAN_POINT ( 'NONE',  ( 0.3460692066303959202, -0.1998031496062991630, -1.126640419947506633 ) ) ;
#9353 = CARTESIAN_POINT ( 'NONE',  ( 0.6824146981627303710, -0.6046776061558807314, 0.2411417322834647770 ) ) ;
#9354 = CARTESIAN_POINT ( 'NONE',  ( -0.1958661417322836718, 0.3392501089628017219, -1.107611548556430403 ) ) ;
#9355 = CARTESIAN_POINT ( 'NONE',  ( 0.2255212960314322279, -4.135162568743707313E-16, -0.4118484887281965712 ) ) ;
#9356 = CARTESIAN_POINT ( 'NONE',  ( 0.9324623468618423727, 2.784432375088962958E-17, -0.3464511005275205946 ) ) ;
#9357 = CARTESIAN_POINT ( 'NONE',  ( -0.006561679790025524116, -0.2845877964562159024, 0.3641732283464567677 ) ) ;
#9358 = CARTESIAN_POINT ( 'NONE',  ( 0.01968503937007957949, -0.5400638737290845981, -0.3530559997133363437 ) ) ;
#9359 = CARTESIAN_POINT ( 'NONE',  ( 1.476377952755906442, -0.4536011799217367080, 0.2665933059059888421 ) ) ;
#9360 = CARTESIAN_POINT ( 'NONE',  ( -1.371391076115484831, 0.1771653543307087075, -0.09757992244046823083 ) ) ;
#9361 = CARTESIAN_POINT ( 'NONE',  ( -1.305774278215222184, -0.6692913385826773087, -0.1292274648535924053 ) ) ;
#9362 = CARTESIAN_POINT ( 'NONE',  ( 0.5314960629921267055, -0.5400638737290844871, 0.3530559997133364547 ) ) ;
#9363 = CARTESIAN_POINT ( 'NONE',  ( 1.076115485564305141, 0.2306618581243847221, -0.2411417322834647770 ) ) ;
#9364 = FACE_OUTER_BOUND ( 'NONE', #76910, .T. ) ;
#9365 = CARTESIAN_POINT ( 'NONE',  ( 0.6627296587926515548, 0.2952755905511811885, 0.1292274648535926551 ) ) ;
#9366 = CARTESIAN_POINT ( 'NONE',  ( 1.358267716535433323, 0.1660481256975885056, 0.3530559997133364547 ) ) ;
#9367 = CARTESIAN_POINT ( 'NONE',  ( 1.069553805774278832, 0.2952755905511810774, -0.1292274648535930714 ) ) ;
#9368 = CARTESIAN_POINT ( 'NONE',  ( 0.5314960629921396951, 2.755905511811024056, -3.937007874015760578 ) ) ;
#9369 = CARTESIAN_POINT ( 'NONE',  ( 0.6627296587926517768, -0.5511811023622048555, -0.09757992244046775898 ) ) ;
#9370 = CARTESIAN_POINT ( 'NONE',  ( -1.607611548556429737, 0.1771653543307087075, -0.09757992244046823083 ) ) ;
#9371 = CARTESIAN_POINT ( 'NONE',  ( -0.9645669291338575535, 0.07958543189024071263, -0.2665933059059888421 ) ) ;
#9372 = CARTESIAN_POINT ( 'NONE',  ( 0.4002624671916016896, -0.2845877964562161244, -0.3641732283464567121 ) ) ;
#9373 = CARTESIAN_POINT ( 'NONE',  ( -0.01312335958005186876, 0.05413385826771626580, -0.4176697321401330321 ) ) ;
#9374 = CARTESIAN_POINT ( 'NONE',  ( 0.6758530183727039509, 0.2952755905511810774, -0.1292274648535930714 ) ) ;
#9375 = CARTESIAN_POINT ( 'NONE',  ( -0.2296587926509179312, -0.05778040916215522460, 0.4822834645669289988 ) ) ;
#9376 = EDGE_CURVE ( 'NONE', #51564, #6368, #44798, .T. ) ;
#9377 = CARTESIAN_POINT ( 'NONE',  ( 0.3215223097112867578, -0.08942795157527998196, 0.3641732283464567121 ) ) ;
#9378 = CARTESIAN_POINT ( 'NONE',  ( 1.423884514435696191, -0.05778040916215522460, 0.4822834645669289988 ) ) ;
#9379 = CARTESIAN_POINT ( 'NONE',  ( -1.713362436456637550, 1.196869643373675407, 0.3303709977379641893 ) ) ;
#9380 = CARTESIAN_POINT ( 'NONE',  ( -0.8464566929133852113, -0.5400638737290845981, -0.3530559997133363437 ) ) ;
#9382 = CARTESIAN_POINT ( 'NONE',  ( -9.787531504996567848E-17, 0.3996062992125986035, -0.7874015748031496509 ) ) ;
#9381 = CARTESIAN_POINT ( 'NONE',  ( 0.000000000000000000, 0.000000000000000000, 0.000000000000000000 ) ) ;
#9383 = CARTESIAN_POINT ( 'NONE',  ( -0.7535225988626923499, 2.401574803149606474, 0.4915354330708645025 ) ) ;
#9384 = CARTESIAN_POINT ( 'NONE',  ( -0.8858267716535425107, -0.5400638737290844871, 0.3530559997133364547 ) ) ;
#9385 = CARTESIAN_POINT ( 'NONE',  ( -0.6167979002624665030, 0.05413385826771666132, 0.4176697321401328100 ) ) ;
#9386 = CARTESIAN_POINT ( 'NONE',  ( -0.1998031496062991907, -0.3460692066303959757, -2.900262467191600635 ) ) ;
#9387 = CARTESIAN_POINT ( 'NONE',  ( 0.3949938075777409963, 2.418639510665530435E-17, -2.480314960629921295 ) ) ;
#9388 = ORIENTED_EDGE ( 'NONE', *, *, #16612, .T. ) ;
#9389 = CARTESIAN_POINT ( 'NONE',  ( 0.6167979002624679463, -0.004921259842519870586, -0.3153832671262229437 ) ) ;
#9390 = CARTESIAN_POINT ( 'NONE',  ( -0.3392501089628017219, -0.1958661417322836718, -1.146981627296587813 ) ) ;
#9391 = CARTESIAN_POINT ( 'NONE',  ( 1.259842519685040019, -0.1870078740157479769, 0.4822834645669291653 ) ) ;
#9392 = CARTESIAN_POINT ( 'NONE',  ( 0.4996603849959059263, 1.493546695847427719, 0.5309055118110234117 ) ) ;
#9393 = CARTESIAN_POINT ( 'NONE',  ( -1.351706036745406347, -0.004921259842519870586, -0.3153832671262229437 ) ) ;
#9394 = CARTESIAN_POINT ( 'NONE',  ( 1.594488188976378673, -0.5400638737290845981, -0.3530559997133363437 ) ) ;
#9395 = CARTESIAN_POINT ( 'NONE',  ( -1.548556430446193399, 0.2306618581243848609, 0.2411417322834645549 ) ) ;
#9396 = CARTESIAN_POINT ( 'NONE',  ( -0.3917322834645670659, 0.1049643490035301607, -0.1128415766066123566 ) ) ;
#9397 = CARTESIAN_POINT ( 'NONE',  ( 0.1509186351706045259, -0.05778040916215560624, -0.4822834645669293319 ) ) ;
#9398 = CARTESIAN_POINT ( 'NONE',  ( -0.4396325459317579898, 0.1771653543307087630, 0.09757992244046791164 ) ) ;
#9399 = EDGE_CURVE ( 'NONE', #78980, #67465, #35125, .T. ) ;
#9400 = CARTESIAN_POINT ( 'NONE',  ( 0.7808398950131240079, -0.3162353388693405765, 0.4822834645669290543 ) ) ;
#9401 = CARTESIAN_POINT ( 'NONE',  ( 0.06561679790026316017, 0.05413385826771626580, -0.4176697321401330321 ) ) ;
#9402 = CARTESIAN_POINT ( 'NONE',  ( -1.192598508356889520, -5.582469467804009507E-15, -0.3791483426435192650 ) ) ;
#9403 = CARTESIAN_POINT ( 'NONE',  ( -1.157146581871515012E-16, 0.4724409448818898682, -1.102362204724409489 ) ) ;
#9404 = CARTESIAN_POINT ( 'NONE',  ( 0.1958661417322836718, -0.3392501089628017219, -1.505924827592862503 ) ) ;
#9405 = CARTESIAN_POINT ( 'NONE',  ( 0.7217847769028878924, 0.05413385826771666132, 0.4176697321401328100 ) ) ;
#9406 = CARTESIAN_POINT ( 'NONE',  ( 0.1312335958005255154, -0.6046776061558807314, 0.2411417322834647770 ) ) ;
#9407 = CARTESIAN_POINT ( 'NONE',  ( -0.8530183727034112984, 0.05413385826771666132, 0.4176697321401328100 ) ) ;
#9408 = CARTESIAN_POINT ( 'NONE',  ( 1.161417322834646271, 0.1660481256975883668, -0.3530559997133364547 ) ) ;
#9409 = CARTESIAN_POINT ( 'NONE',  ( 0.8070866141732289112, -0.5400638737290845981, -0.3530559997133363437 ) ) ;
#9410 = CARTESIAN_POINT ( 'NONE',  ( 4.797336870675656522E-17, -0.3917322834645670104, -1.108267716535433101 ) ) ;
#9411 = CARTESIAN_POINT ( 'NONE',  ( -0.1771653543307080136, -0.5400638737290844871, 0.3530559997133364547 ) ) ;
#9412 = CARTESIAN_POINT ( 'NONE',  ( 0.5314960629921267055, -0.5400638737290844871, 0.3530559997133364547 ) ) ;
#9413 = CARTESIAN_POINT ( 'NONE',  ( 0.03937007874015833325, -0.6692913385826771977, 8.415575281601705876E-17 ) ) ;
#9414 = CARTESIAN_POINT ( 'NONE',  ( 0.6889763779527566800, -0.4536011799217367080, 0.2665933059059888421 ) ) ;
#9415 = CARTESIAN_POINT ( 'NONE',  ( -1.240157480314959759, 0.1660481256975885056, 0.3530559997133364547 ) ) ;
#9416 = CARTESIAN_POINT ( 'NONE',  ( -0.2248261898302304773, 1.118407866122133276, -2.823087432092973081 ) ) ;
#9417 = CARTESIAN_POINT ( 'NONE',  ( 0.1312335958005255154, -0.6046776061558807314, 0.2411417322834647770 ) ) ;
#9418 = DIRECTION ( 'NONE',  ( -3.491481338843132961E-15, -0.000000000000000000, 1.000000000000000000 ) ) ;
#9419 = EDGE_CURVE ( 'NONE', #44018, #69029, #41725, .T. ) ;
#9420 = CARTESIAN_POINT ( 'NONE',  ( -0.3392501089628019995, 0.1958661417322832277, -2.380577427821522374 ) ) ;
#9421 = ORIENTED_EDGE ( 'NONE', *, *, #16548, .F. ) ;
#9422 = ORIENTED_EDGE ( 'NONE', *, *, #79479, .T. ) ;
#9423 = CARTESIAN_POINT ( 'NONE',  ( 1.292650918635171564, -0.6692913385826773087, -0.1292274648535924053 ) ) ;
#9424 = CARTESIAN_POINT ( 'NONE',  ( 0.4724409448818904789, -0.1870078740157479769, 0.3641732283464567677 ) ) ;
#9426 = DIRECTION ( 'NONE',  ( 0.000000000000000000, 0.000000000000000000, -1.000000000000000000 ) ) ;
#9425 = CARTESIAN_POINT ( 'NONE',  ( -1.220472440944882386, -3.283890673957456492E-15, 0.4445507791589070057 ) ) ;
#9427 = LINE ( 'NONE', #72984, #81312 ) ;
#9428 = CARTESIAN_POINT ( 'NONE',  ( -0.03443470937339728616, 0.2755905511811023723, -1.537015892239756099 ) ) ;
#9429 = CARTESIAN_POINT ( 'NONE',  ( -0.1958661417322836718, 0.3392501089628017219, -1.357611548556430625 ) ) ;
#9430 = CARTESIAN_POINT ( 'NONE',  ( 0.2925321140481932369, 0.2925321140481932369, -2.419291338582676865 ) ) ;
#9431 = CARTESIAN_POINT ( 'NONE',  ( -0.8923884514435688198, -0.6046776061558807314, 0.2411417322834647770 ) ) ;
#9432 = CARTESIAN_POINT ( 'NONE',  ( -0.6496062992125976043, -0.5400638737290844871, 0.3530559997133364547 ) ) ;
#9433 = CARTESIAN_POINT ( 'NONE',  ( 0.6627296587926515548, 0.2952755905511811885, 0.1292274648535926551 ) ) ;
#9434 = ORIENTED_EDGE ( 'NONE', *, *, #69637, .T. ) ;
#9435 = CARTESIAN_POINT ( 'NONE',  ( 1.391076115485564868, -0.6046776061558807314, 0.2411417322834647770 ) ) ;
#9436 = CARTESIAN_POINT ( 'NONE',  ( -1.169169330835493126, -3.926852850522101851E-15, 0.3627989612356165572 ) ) ;
#9437 = DIRECTION ( 'NONE',  ( 0.000000000000000000, -1.000000000000000000, 0.000000000000000000 ) ) ;
#9438 = CARTESIAN_POINT ( 'NONE',  ( -0.3460692066303960313, 0.1998031496062989965, -2.150262467191601079 ) ) ;
#9439 = CARTESIAN_POINT ( 'NONE',  ( -1.535433070866141225, -0.5511811023622047445, 6.969142054262312111E-17 ) ) ;
#9440 = DIRECTION ( 'NONE',  ( -0.000000000000000000, -1.000000000000000000, 0.000000000000000000 ) ) ;
#9441 = CARTESIAN_POINT ( 'NONE',  ( 0.3018372703412079971, 0.05413385826771626580, -0.4176697321401330321 ) ) ;
#9443 = CARTESIAN_POINT ( 'NONE',  ( 0.000000000000000000, 2.755905511811024056, 0.000000000000000000 ) ) ;
#9442 = CARTESIAN_POINT ( 'NONE',  ( 1.673228346456693494, 0.1660481256975885056, 0.3530559997133364547 ) ) ;
#9444 = CARTESIAN_POINT ( 'NONE',  ( -1.076115485564303809, 0.1283753931104748280, 0.1820866141732283561 ) ) ;
#9445 = CARTESIAN_POINT ( 'NONE',  ( 0.9776902887139113929, -0.6692913385826773087, -0.1292274648535924053 ) ) ;
#9446 = CARTESIAN_POINT ( 'NONE',  ( 1.240157480314961314, -0.4536011799217367080, 0.2665933059059888421 ) ) ;
#9447 = CARTESIAN_POINT ( 'NONE',  ( -0.1958661417322836440, 0.3392501089628016664, -1.038038427000312902 ) ) ;
#9448 = CARTESIAN_POINT ( 'NONE',  ( -0.9514435695538050464, -0.2845877964562159024, 0.3641732283464567677 ) ) ;
#9449 = CARTESIAN_POINT ( 'NONE',  ( 1.437007874015748810, -0.5400638737290845981, -0.3530559997133363437 ) ) ;
#9450 = CARTESIAN_POINT ( 'NONE',  ( 2.557182324916567495, 1.572090529166660922, -0.4732185887570796723 ) ) ;
#9451 = CARTESIAN_POINT ( 'NONE',  ( -0.2821522309711278487, 0.2952755905511811885, 0.1292274648535926551 ) ) ;
#9452 = CARTESIAN_POINT ( 'NONE',  ( -1.318897637795274802, 0.07958543189024085140, 0.2665933059059887866 ) ) ;
#9453 = CARTESIAN_POINT ( 'NONE',  ( -0.2493438320209966919, -0.004921259842519870586, -0.3153832671262229437 ) ) ;
#9454 = CARTESIAN_POINT ( 'NONE',  ( -0.2952755905511804668, 0.1660481256975885056, 0.3530559997133364547 ) ) ;
#9455 = CARTESIAN_POINT ( 'NONE',  ( -1.463254593175852492, 0.1771653543307087630, 0.09757992244046791164 ) ) ;
#9456 = CARTESIAN_POINT ( 'NONE',  ( -0.3917322834645670104, -0.1049643490035307020, -0.3576308643382697383 ) ) ;
#9457 = CARTESIAN_POINT ( 'NONE',  ( 0.4790026246719167324, -0.05778040916215522460, 0.4822834645669289988 ) ) ;
#9458 = CARTESIAN_POINT ( 'NONE',  ( 0.4040399068613302891, -1.094630224652485432E-15, 0.4281993546915535687 ) ) ;
#9459 = CARTESIAN_POINT ( 'NONE',  ( 5.785732909357575061E-17, -0.4724409448818898682, -1.730314960629921517 ) ) ;
#9460 = CARTESIAN_POINT ( 'NONE',  ( -1.253280839895012377, -0.05778040916215522460, 0.4822834645669289988 ) ) ;
#9461 = CARTESIAN_POINT ( 'NONE',  ( -0.5577427821522301654, -0.08942795157528024563, -0.3641732283464568787 ) ) ;
#9462 = CARTESIAN_POINT ( 'NONE',  ( -1.167979002624671470, 0.05413385826771666132, 0.4176697321401328100 ) ) ;
#9463 = CARTESIAN_POINT ( 'NONE',  ( -0.07217847769028787330, -0.05778040916215522460, 0.4822834645669289988 ) ) ;
#9464 = CARTESIAN_POINT ( 'NONE',  ( 0.5905511811023629321, 0.1771653543307087630, 0.000000000000000000 ) ) ;
#9465 = CARTESIAN_POINT ( 'NONE',  ( -0.7217847769028863381, -0.004921259842519870586, -0.3153832671262229437 ) ) ;
#9466 = CARTESIAN_POINT ( 'NONE',  ( -0.9448818897637790704, -0.1870078740157479769, 0.4822834645669291653 ) ) ;
#9467 = CARTESIAN_POINT ( 'NONE',  ( 1.568241469816273437, -0.2845877964562159024, 0.3641732283464567677 ) ) ;
#9468 = CARTESIAN_POINT ( 'NONE',  ( 1.482939632545932307, -0.4281496062992124485, 0.4176697321401328655 ) ) ;
#9469 = PLANE ( 'NONE',  #56857 ) ;
#9470 = CARTESIAN_POINT ( 'NONE',  ( 0.6692913385826778638, -0.5511811023622047445, 6.969142054262312111E-17 ) ) ;
#9471 = CARTESIAN_POINT ( 'NONE',  ( 0.9317585301837276734, 0.05413385826771626580, -0.4176697321401330321 ) ) ;
#9472 = ADVANCED_FACE ( 'NONE', ( #15667 ), #2618, .F. ) ;
#9473 = CARTESIAN_POINT ( 'NONE',  ( -1.291027602697912169, 0.1377952755905511861, 0.5830028338522512676 ) ) ;
#9474 = CARTESIAN_POINT ( 'NONE',  ( 1.482939632545932307, -0.004921259842519870586, -0.3153832671262229437 ) ) ;
#9475 = VERTEX_POINT ( 'NONE', #60677 ) ;
#9476 = CARTESIAN_POINT ( 'NONE',  ( -0.8792650918635160906, -0.4281496062992124485, 0.4176697321401328655 ) ) ;
#9477 = CARTESIAN_POINT ( 'NONE',  ( -0.3460692066303960313, 0.1998031496062989965, -2.622703412073490892 ) ) ;
#9478 = CARTESIAN_POINT ( 'NONE',  ( -1.404199475065615932, -0.3690944881889765550, -0.3153832671262227771 ) ) ;
#9479 = CARTESIAN_POINT ( 'NONE',  ( -0.7480314960629914633, -0.6692913385826771977, 8.415575281601705876E-17 ) ) ;
#9480 = CARTESIAN_POINT ( 'NONE',  ( 0.3937007874015754361, -0.1870078740157480879, -0.4822834645669291653 ) ) ;
#9481 = CARTESIAN_POINT ( 'NONE',  ( -1.463254593175852492, -0.5511811023622048555, -0.09757992244046775898 ) ) ;
#9482 = CARTESIAN_POINT ( 'NONE',  ( -0.1998031496062991630, -0.3460692066303959202, -2.032152230971128848 ) ) ;
#9483 = CARTESIAN_POINT ( 'NONE',  ( -1.528871391076114250, 0.2952755905511810774, -0.1292274648535930714 ) ) ;
#9484 = CARTESIAN_POINT ( 'NONE',  ( 0.4068241469816281097, 0.05413385826771666132, 0.4176697321401328100 ) ) ;
#9485 = CARTESIAN_POINT ( 'NONE',  ( 0.03937007874015833325, -0.6692913385826771977, 8.415575281601705876E-17 ) ) ;
#9486 = CARTESIAN_POINT ( 'NONE',  ( 0.8989501312335963501, -0.6692913385826773087, -0.1292274648535924053 ) ) ;
#9487 = DIRECTION ( 'NONE',  ( 1.000000000000000000, 3.096699300667737957E-16, -1.692413147294446216E-16 ) ) ;
#9488 = CARTESIAN_POINT ( 'NONE',  ( 0.3996062992125986590, -0.1070741851644053111, -1.686351706036745446 ) ) ;
#9489 = CARTESIAN_POINT ( 'NONE',  ( 0.2891555358219910499, 0.2891555358219910499, -1.240157480314960869 ) ) ;
#9490 = CARTESIAN_POINT ( 'NONE',  ( 0.2925321140481932369, -0.2925321140481932369, -2.460629921259842146 ) ) ;
#9491 = LINE ( 'NONE', #34757, #17063 ) ;
#9492 = APPLICATION_CONTEXT ( 'automotive_design' ) ;
#9493 = CARTESIAN_POINT ( 'NONE',  ( 4.218763579739897660E-16, 0.000000000000000000, 3.444881889763779625 ) ) ;
#9494 = CARTESIAN_POINT ( 'NONE',  ( -0.09186351706036689768, -0.004921259842519870586, -0.3153832671262229437 ) ) ;
#9495 = CARTESIAN_POINT ( 'NONE',  ( -0.2755905511811018171, 0.2952755905511811885, 0.000000000000000000 ) ) ;
#9496 = CARTESIAN_POINT ( 'NONE',  ( 1.069553805774278610, -0.6692913385826771977, 0.1292274648535927661 ) ) ;
#9497 = CARTESIAN_POINT ( 'NONE',  ( -9.674558042662122972E-17, 0.3949938075777409963, -1.966535433070866423 ) ) ;
#9498 = CARTESIAN_POINT ( 'NONE',  ( 0.1181102362204730916, 0.1771653543307087630, 0.000000000000000000 ) ) ;
#9499 = CARTESIAN_POINT ( 'NONE',  ( -1.240157480314959759, -0.5400638737290845981, -0.3530559997133363437 ) ) ;
#9500 = CARTESIAN_POINT ( 'NONE',  ( 1.227034120734908917, -0.6692913385826771977, 0.1292274648535927661 ) ) ;
#9501 = CARTESIAN_POINT ( 'NONE',  ( 0.2362204724409451007, -0.4091458600556402980, -2.296587926509186417 ) ) ;
#9502 = CARTESIAN_POINT ( 'NONE',  ( 0.1070741851644054915, -0.3996062992125986035, -1.660104986876640210 ) ) ;
#9503 = CARTESIAN_POINT ( 'NONE',  ( 1.161417322834646271, 0.1660481256975883391, -0.3530559997133364547 ) ) ;
#9504 = VERTEX_POINT ( 'NONE', #15250 ) ;
#9505 = ORIENTED_EDGE ( 'NONE', *, *, #35324, .F. ) ;
#9506 = CARTESIAN_POINT ( 'NONE',  ( 1.069553805774278610, -0.6692913385826771977, 0.1292274648535927661 ) ) ;
#9507 = CARTESIAN_POINT ( 'NONE',  ( -1.686351706036744558, 0.2952755905511810774, -0.1292274648535930714 ) ) ;
#9509 = CARTESIAN_POINT ( 'NONE',  ( -1.220472440944881054, -0.6692913385826771977, 8.415575281601705876E-17 ) ) ;
#9508 = CARTESIAN_POINT ( 'NONE',  ( -1.049868766404198794, -0.5023911411419708095, 0.1820866141732285504 ) ) ;
#9510 = CARTESIAN_POINT ( 'NONE',  ( 0.1049643490035304938, -0.3917322834645669549, 0.1450131233595799429 ) ) ;
#9511 = CARTESIAN_POINT ( 'NONE',  ( -0.9908136482939625678, 0.2066929133858267931, 0.1054918080437490802 ) ) ;
#9512 = CARTESIAN_POINT ( 'NONE',  ( 1.095800524934383846, -0.05778040916215560624, -0.4822834645669293319 ) ) ;
#9513 = CARTESIAN_POINT ( 'NONE',  ( 3.924389226575468737, 2.755905511811024056, 0.3149606299212598381 ) ) ;
#9514 = CARTESIAN_POINT ( 'NONE',  ( -0.1443569553805768291, 0.05413385826771666132, 0.4176697321401328100 ) ) ;
#9515 = CARTESIAN_POINT ( 'NONE',  ( -0.5118110236220466680, -0.6692913385826771977, 8.415575281601705876E-17 ) ) ;
#9516 = AXIS2_PLACEMENT_3D ( 'NONE', #49779, #62840, #9838 ) ;
#9517 = CARTESIAN_POINT ( 'NONE',  ( -1.640419947506561060, 0.05413385826771666132, 0.4176697321401328100 ) ) ;
#9518 = CARTESIAN_POINT ( 'NONE',  ( 0.3917322834645670104, -0.1049643490035303411, -0.3536745406824148286 ) ) ;
#9519 = CARTESIAN_POINT ( 'NONE',  ( 0.2952755905511816326, -0.5400638737290844871, 0.3530559997133364547 ) ) ;
#9520 = CARTESIAN_POINT ( 'NONE',  ( 0.1958661417322836440, -0.3392501089628017219, -2.131233595800524849 ) ) ;
#9521 = CARTESIAN_POINT ( 'NONE',  ( -1.423884514435694859, -0.08942795157528024563, -0.3641732283464568787 ) ) ;
#9522 = ORIENTED_EDGE ( 'NONE', *, *, #26035, .F. ) ;
#9523 = CARTESIAN_POINT ( 'NONE',  ( -0.1058382717557497937, -0.3949938075777411628, -2.434383202099737353 ) ) ;
#9524 = ORIENTED_EDGE ( 'NONE', *, *, #65450, .F. ) ;
#9525 = CARTESIAN_POINT ( 'NONE',  ( 0.5419760673063066525, 1.535433070866141447, 0.4915354330708653907 ) ) ;
#9526 = CARTESIAN_POINT ( 'NONE',  ( -1.515748031496062076, 0.1660481256975883668, -0.3530559997133364547 ) ) ;
#9527 = CARTESIAN_POINT ( 'NONE',  ( -0.2925321140481930704, -0.2925321140481933480, -1.003937007874015741 ) ) ;
#9528 = CARTESIAN_POINT ( 'NONE',  ( -1.692913385826770645, 0.2952755905511811885, 0.000000000000000000 ) ) ;
#9529 = CARTESIAN_POINT ( 'NONE',  ( 1.854472803289052507, 2.716535433070866645, -0.5314960629921260393 ) ) ;
#9530 = CARTESIAN_POINT ( 'NONE',  ( 0.000000000000000000, 0.000000000000000000, 6.043307086614173151 ) ) ;
#9531 = CARTESIAN_POINT ( 'NONE',  ( -0.3805774278215216522, 0.05413385826771666132, 0.4176697321401328100 ) ) ;
#9532 = ADVANCED_FACE ( 'NONE', ( #16497 ), #28274, .F. ) ;
#9533 = CARTESIAN_POINT ( 'NONE',  ( 0.2867679344610365999, 0.2867679344610365999, -0.06496062992125994917 ) ) ;
#9534 = CARTESIAN_POINT ( 'NONE',  ( -0.4593175853018364174, -0.3690944881889765550, -0.3153832671262227771 ) ) ;
#9535 = CARTESIAN_POINT ( 'NONE',  ( -0.5839895013123351797, 0.1771653543307087075, -0.09757992244046823083 ) ) ;
#9536 = CARTESIAN_POINT ( 'NONE',  ( -1.194225721784776262, -0.4281496062992124485, 0.4176697321401328655 ) ) ;
#9537 = ADVANCED_FACE ( 'NONE', ( #47625 ), #41329, .F. ) ;
#9538 = CARTESIAN_POINT ( 'NONE',  ( 0.6299212598425204535, -0.1870078740157479769, 0.4822834645669291653 ) ) ;
#9539 = CARTESIAN_POINT ( 'NONE',  ( -0.9120734908136475250, -0.6692913385826773087, -0.1292274648535924053 ) ) ;
#9540 = VECTOR ( 'NONE', #69101, 39.37007874015748143 ) ;
#9541 = FACE_OUTER_BOUND ( 'NONE', #735, .T. ) ;
#9542 = ORIENTED_EDGE ( 'NONE', *, *, #81853, .T. ) ;
#9543 = CARTESIAN_POINT ( 'NONE',  ( -1.279527559055116948, 0.1660481256975883668, -0.3530559997133364547 ) ) ;
#9544 = LINE ( 'NONE', #80268, #7089 ) ;
#9545 = CARTESIAN_POINT ( 'NONE',  ( 0.2362204724409449064, 0.4091458600556404646, -1.561679790026246684 ) ) ;
#9546 = DIRECTION ( 'NONE',  ( 0.6236670536615054328, 0.6323634944239198141, -0.4595169388576945124 ) ) ;
#9547 = CARTESIAN_POINT ( 'NONE',  ( -0.1049643490035307020, 0.3917322834645669549, -0.6286089238845143923 ) ) ;
#9548 = CARTESIAN_POINT ( 'NONE',  ( 0.3917322834645669549, 0.1049643490035304660, -2.414041994750655729 ) ) ;
#9549 = CARTESIAN_POINT ( 'NONE',  ( -0.8136482939632537770, 0.2306618581243847221, -0.2411417322834647770 ) ) ;
#9550 = CARTESIAN_POINT ( 'NONE',  ( 1.266404199475066328, -0.3162353388693409650, -0.4822834645669289433 ) ) ;
#9551 = CARTESIAN_POINT ( 'NONE',  ( -0.2925321140481932369, 0.2925321140481931259, -0.4114173228346455491 ) ) ;
#9553 = CARTESIAN_POINT ( 'NONE',  ( -0.6692913385826764205, 0.2066929133858268208, 0.000000000000000000 ) ) ;
#9552 = CARTESIAN_POINT ( 'NONE',  ( -1.699475065616797398, 0.2952755905511811885, 0.1292274648535926551 ) ) ;
#9554 = CARTESIAN_POINT ( 'NONE',  ( -1.423884514435694859, -0.3162353388693405765, 0.4822834645669290543 ) ) ;
#9555 = CARTESIAN_POINT ( 'NONE',  ( -0.9711286089238838626, -0.6046776061558807314, 0.2411417322834647770 ) ) ;
#9556 = CARTESIAN_POINT ( 'NONE',  ( 0.2867679344610365999, -0.2867679344610365999, -0.1784583745068747673 ) ) ;
#9557 = CARTESIAN_POINT ( 'NONE',  ( 0.3083989501312343062, -0.2845877964562159024, 0.3641732283464567677 ) ) ;
#9558 = CARTESIAN_POINT ( 'NONE',  ( 0.3392501089628018329, 0.1958661417322835607, -0.3733595800524935338 ) ) ;
#9559 = CARTESIAN_POINT ( 'NONE',  ( 0.1377952755905518800, 0.07958543189024071263, -0.2665933059059888421 ) ) ;
#9560 = CARTESIAN_POINT ( 'NONE',  ( 0.9908136482939640111, 0.1771653543307087075, -0.09757992244046823083 ) ) ;
#9561 = CARTESIAN_POINT ( 'NONE',  ( 0.9120734908136489683, -0.6692913385826771977, 0.1292274648535927661 ) ) ;
#9562 = CARTESIAN_POINT ( 'NONE',  ( -0.1049868766404193215, -0.5023911411419708095, 0.1820866141732285504 ) ) ;
#9563 = CARTESIAN_POINT ( 'NONE',  ( 0.3392501089628018329, 0.1958661417322835607, -2.170603674540682260 ) ) ;
#9564 = CARTESIAN_POINT ( 'NONE',  ( -1.614173228346455824, 0.2952755905511811885, 0.000000000000000000 ) ) ;
#9565 = EDGE_CURVE ( 'NONE', #9606, #7036, #30669, .T. ) ;
#9566 = CARTESIAN_POINT ( 'NONE',  ( -1.358267716535432434, -0.4536011799217367080, 0.2665933059059888421 ) ) ;
#9567 = CARTESIAN_POINT ( 'NONE',  ( 0.2362204724409449064, 0.4091458600556404646, -0.2211286089238845010 ) ) ;
#9568 = CARTESIAN_POINT ( 'NONE',  ( -0.2952755905511803003, -0.5400638737290845981, -0.3530559997133363437 ) ) ;
#9569 = CARTESIAN_POINT ( 'NONE',  ( 1.640419947506562393, -0.3690944881889763329, 0.3153832671262228327 ) ) ;
#9570 = EDGE_CURVE ( 'NONE', #79188, #18348, #35424, .T. ) ;
#9571 = CARTESIAN_POINT ( 'NONE',  ( 0.5708661417322841158, -0.4536011799217368745, -0.2665933059059886201 ) ) ;
#9572 = CARTESIAN_POINT ( 'NONE',  ( -0.3280839895013117347, -0.3690944881889763329, 0.3153832671262228327 ) ) ;
#9573 = CARTESIAN_POINT ( 'NONE',  ( -0.9251968503937002541, -0.5400638737290845981, -0.3530559997133363437 ) ) ;
#9574 = CARTESIAN_POINT ( 'NONE',  ( -1.594488188976377563, -0.5400638737290844871, 0.3530559997133364547 ) ) ;
#9575 = DIRECTION ( 'NONE',  ( 0.000000000000000000, 0.000000000000000000, -1.000000000000000000 ) ) ;
#9576 = CARTESIAN_POINT ( 'NONE',  ( 0.2034120734908144990, -0.6692913385826771977, 0.1292274648535927661 ) ) ;
#9577 = EDGE_LOOP ( 'NONE', ( #12413, #57116, #63450, #41679 ) ) ;
#9578 = CARTESIAN_POINT ( 'NONE',  ( 0.1998031496062994128, -0.3460692066303957537, -1.743438320209973469 ) ) ;
#9579 = EDGE_CURVE ( 'NONE', #20803, #6972, #6657, .T. ) ;
#9580 = CARTESIAN_POINT ( 'NONE',  ( 1.601049868766404982, 0.2306618581243848609, 0.2411417322834645549 ) ) ;
#9581 = CARTESIAN_POINT ( 'NONE',  ( -0.1377952755905504645, 0.07958543189024085140, 0.2665933059059887866 ) ) ;
#9582 = CARTESIAN_POINT ( 'NONE',  ( -0.1837270341207343505, -0.6046776061558807314, 0.2411417322834647770 ) ) ;
#9583 = CARTESIAN_POINT ( 'NONE',  ( -1.548556430446193399, -0.6046776061558809534, -0.2411417322834644161 ) ) ;
#9584 = CARTESIAN_POINT ( 'NONE',  ( -1.482939632545930975, -0.004921259842519576551, 0.3153832671262227771 ) ) ;
#9585 = CARTESIAN_POINT ( 'NONE',  ( 1.423884514435696413, -0.3162353388693409650, -0.4822834645669289433 ) ) ;
#9586 = CARTESIAN_POINT ( 'NONE',  ( -1.305774278215222184, 0.2952755905511811885, 0.1292274648535926551 ) ) ;
#9587 = CARTESIAN_POINT ( 'NONE',  ( -0.7874015748031489847, -0.1870078740157479769, 0.3641732283464567677 ) ) ;
#9588 = CARTESIAN_POINT ( 'NONE',  ( -0.3460692066303960313, 0.1998031496062989965, -0.2604986876640419946 ) ) ;
#9589 = CARTESIAN_POINT ( 'NONE',  ( -0.3460692066303958092, -0.1998031496062994683, -0.5249343832020997302 ) ) ;
#9590 = CARTESIAN_POINT ( 'NONE',  ( 0.3917322834645670104, 0.1049643490035304660, -2.798575746228034067 ) ) ;
#9591 = VECTOR ( 'NONE', #72487, 39.37007874015748143 ) ;
#9592 = CARTESIAN_POINT ( 'NONE',  ( 1.482939632545932307, -0.3690944881889763329, 0.3153832671262228327 ) ) ;
#9593 = CARTESIAN_POINT ( 'NONE',  ( 1.122047244094488860, 0.07958543189024085140, 0.2665933059059887866 ) ) ;
#9594 = CARTESIAN_POINT ( 'NONE',  ( 0.4068241469816281097, 0.009842519685039467087, 0.3409548833797002021 ) ) ;
#9595 = CARTESIAN_POINT ( 'NONE',  ( 0.9055118110236227702, -0.6692913385826771977, 8.415575281601705876E-17 ) ) ;
#9596 = CARTESIAN_POINT ( 'NONE',  ( -0.3949938075777408852, -0.1058382717557502933, -0.9101049868766403206 ) ) ;
#9597 = CARTESIAN_POINT ( 'NONE',  ( 1.423884514435696413, -0.2845877964562161244, -0.3641732283464567121 ) ) ;
#9598 = CARTESIAN_POINT ( 'NONE',  ( 0.1771653543307093182, -0.5400638737290845981, -0.3530559997133363437 ) ) ;
#9599 = CARTESIAN_POINT ( 'NONE',  ( -0.8267716535433065062, 0.2952755905511811885, 0.000000000000000000 ) ) ;
#9600 = CARTESIAN_POINT ( 'NONE',  ( 1.673228346456693494, 0.1660481256975885056, 0.3530559997133364547 ) ) ;
#9601 = CARTESIAN_POINT ( 'NONE',  ( 0.4724409448818898682, 2.892866454678787531E-17, -0.5905511811023621549 ) ) ;
#9602 = CARTESIAN_POINT ( 'NONE',  ( -9.787531504996567848E-17, 0.3996062992125986035, -2.204724409448818978 ) ) ;
#9603 = CARTESIAN_POINT ( 'NONE',  ( 0.4724409448818904789, -0.1870078740157479769, 0.3641732283464567677 ) ) ;
#9604 = EDGE_LOOP ( 'NONE', ( #75883, #39629, #28440, #67089, #1139, #78158 ) ) ;
#9605 = CARTESIAN_POINT ( 'NONE',  ( -0.1958661417322836995, 0.3392501089628017219, -0.4823027803487682785 ) ) ;
#9606 = VERTEX_POINT ( 'NONE', #29514 ) ;
#9607 = CARTESIAN_POINT ( 'NONE',  ( -0.4461942257217840213, 0.2306618581243848609, 0.2411417322834645549 ) ) ;
#9608 = CARTESIAN_POINT ( 'NONE',  ( 0.7808398950131240079, -0.3162353388693405765, 0.4822834645669290543 ) ) ;
#9609 = CARTESIAN_POINT ( 'NONE',  ( -0.3280839895013117347, 0.05413385826771626580, -0.4176697321401330321 ) ) ;
#9610 = CARTESIAN_POINT ( 'NONE',  ( -0.1968503937007867743, 0.1771653543307087630, 0.000000000000000000 ) ) ;
#9611 = CARTESIAN_POINT ( 'NONE',  ( 0.8267716535433078384, -0.6692913385826771977, 8.415575281601705876E-17 ) ) ;
#9612 = CARTESIAN_POINT ( 'NONE',  ( -0.9055118110236215490, -0.6692913385826771977, 8.415575281601705876E-17 ) ) ;
#9613 = CARTESIAN_POINT ( 'NONE',  ( -0.2493438320209966919, 0.05413385826771626580, -0.4176697321401330321 ) ) ;
#9614 = CARTESIAN_POINT ( 'NONE',  ( 1.299212598425197429, 0.2952755905511811885, 0.000000000000000000 ) ) ;
#9615 = CARTESIAN_POINT ( 'NONE',  ( 1.102362204724410155, -0.1870078740157479769, 0.4822834645669291653 ) ) ;
#9616 = CARTESIAN_POINT ( 'NONE',  ( 0.7217847769028878924, 0.05413385826771666132, 0.4176697321401328100 ) ) ;
#9617 = CARTESIAN_POINT ( 'NONE',  ( 0.3392501089628018329, 0.1958661417322835607, -0.5958005249343831800 ) ) ;
#9618 = CARTESIAN_POINT ( 'NONE',  ( -0.1443569553805765515, -0.3690944881889765550, -0.3153832671262227771 ) ) ;
#9619 = ORIENTED_EDGE ( 'NONE', *, *, #44498, .T. ) ;
#9620 = CARTESIAN_POINT ( 'NONE',  ( 0.1974969037888704704, 0.3420746716998660508, -0.9317585301837268963 ) ) ;
#9621 = ORIENTED_EDGE ( 'NONE', *, *, #27502, .F. ) ;
#9622 = CARTESIAN_POINT ( 'NONE',  ( -1.056430446194224881, 0.1771653543307087075, -0.09757992244046823083 ) ) ;
#9623 = CARTESIAN_POINT ( 'NONE',  ( -0.3149606299212590610, -0.1870078740157480879, -0.4822834645669291653 ) ) ;
#9624 = CARTESIAN_POINT ( 'NONE',  ( -0.3996062992125987146, 0.1070741851644051862, 0.1246719160104986790 ) ) ;
#9625 = CARTESIAN_POINT ( 'NONE',  ( -0.4790026246719154557, -0.3162353388693405765, 0.4822834645669290543 ) ) ;
#9626 = CARTESIAN_POINT ( 'NONE',  ( -0.6036745406824141069, 0.2306618581243848609, 0.2411417322834645549 ) ) ;
#9627 = CARTESIAN_POINT ( 'NONE',  ( -1.174540682414697335, -0.05778040916215522460, 0.4822834645669289988 ) ) ;
#9628 = EDGE_CURVE ( 'NONE', #56091, #63201, #69474, .T. ) ;
#9629 = CARTESIAN_POINT ( 'NONE',  ( -1.345144356955379816, -0.05778040916215560624, -0.4822834645669293319 ) ) ;
#9630 = CARTESIAN_POINT ( 'NONE',  ( 0.9251968503937015864, 0.07958543189024071263, -0.2665933059059888421 ) ) ;
#9631 = DIRECTION ( 'NONE',  ( -0.4999999999999965028, 0.8660254037844405950, 0.000000000000000000 ) ) ;
#9632 = CARTESIAN_POINT ( 'NONE',  ( 0.4724409448818898682, 2.892866454678787531E-17, -0.6673228346456693272 ) ) ;
#9633 = CARTESIAN_POINT ( 'NONE',  ( 0.6496062992125991586, 0.07958543189024085140, 0.2665933059059887866 ) ) ;
#9634 = CARTESIAN_POINT ( 'NONE',  ( 0.1181102362204730916, 0.2952755905511811885, 0.000000000000000000 ) ) ;
#9635 = CARTESIAN_POINT ( 'NONE',  ( 0.4593175853018380828, 0.05413385826771626580, -0.4176697321401330321 ) ) ;
#9636 = EDGE_LOOP ( 'NONE', ( #65638, #34482, #32642, #31123 ) ) ;
#9637 = AXIS2_PLACEMENT_3D ( 'NONE', #22880, #28780, #47296 ) ;
#9638 = CARTESIAN_POINT ( 'NONE',  ( -0.3996062992125986035, -0.1070741851644056997, -1.778215223097112663 ) ) ;
#9639 = DIRECTION ( 'NONE',  ( 0.000000000000000000, -1.000000000000000000, 0.000000000000000000 ) ) ;
#9640 = ORIENTED_EDGE ( 'NONE', *, *, #14239, .F. ) ;
#9641 = CARTESIAN_POINT ( 'NONE',  ( -9.787531504996566615E-17, 0.3996062992125985480, -1.179133858267716661 ) ) ;
#9642 = CARTESIAN_POINT ( 'NONE',  ( 0.1998031496062992463, 0.3460692066303959202, -0.6935695538057742304 ) ) ;
#9643 = CARTESIAN_POINT ( 'NONE',  ( -0.6889763779527552368, -0.4536011799217368745, -0.2665933059059886201 ) ) ;
#9644 = CARTESIAN_POINT ( 'NONE',  ( -1.082677165354329896, 0.1660481256975885056, 0.3530559997133364547 ) ) ;
#9645 = CARTESIAN_POINT ( 'NONE',  ( -1.157146581871515012E-16, 0.4724409448818898682, 0.000000000000000000 ) ) ;
#9646 = CARTESIAN_POINT ( 'NONE',  ( -0.2867679344610365999, 0.2867679344610364889, -2.466535433070865757 ) ) ;
#9647 = CARTESIAN_POINT ( 'NONE',  ( -1.614173228346455824, 0.1771653543307087630, 0.000000000000000000 ) ) ;
#9648 = CARTESIAN_POINT ( 'NONE',  ( 1.010498687664042716, 0.05413385826771626580, -0.4176697321401330321 ) ) ;
#9649 = CARTESIAN_POINT ( 'NONE',  ( 0.3149606299212606708, -0.1870078740157480879, -0.4822834645669291653 ) ) ;
#9650 = CARTESIAN_POINT ( 'NONE',  ( -0.6036745406824141069, -0.5023911411419708095, -0.1820866141732282451 ) ) ;
#9651 = CARTESIAN_POINT ( 'NONE',  ( 0.2624671916010504757, -0.6046776061558809534, -0.2411417322834644161 ) ) ;
#9652 = CARTESIAN_POINT ( 'NONE',  ( 0.4724409448818897572, -0.1265901696524988906, -2.078083989501312345 ) ) ;
#9653 = CARTESIAN_POINT ( 'NONE',  ( -0.1706036745406816491, -0.004921259842519870586, -0.3153832671262229437 ) ) ;
#9654 = CARTESIAN_POINT ( 'NONE',  ( -0.3937007874015740483, -0.1870078740157480879, -0.4822834645669291653 ) ) ;
#9655 = CARTESIAN_POINT ( 'NONE',  ( 0.3420746716998660508, -0.1974969037888704149, -1.914041994750656395 ) ) ;
#9656 = CARTESIAN_POINT ( 'NONE',  ( -1.450131233595799651, -0.6692913385826771977, 0.1292274648535927661 ) ) ;
#9657 = CARTESIAN_POINT ( 'NONE',  ( 0.2755905511811031494, -0.5511811023622047445, 6.969142054262312111E-17 ) ) ;
#9658 = DIRECTION ( 'NONE',  ( 0.000000000000000000, -1.601283208593975810E-15, -1.000000000000000000 ) ) ;
#9659 = CARTESIAN_POINT ( 'NONE',  ( -1.266404199475064773, -0.3162353388693405765, 0.4822834645669290543 ) ) ;
#9660 = CARTESIAN_POINT ( 'NONE',  ( -0.8267716535433065062, 0.1771653543307087630, 0.000000000000000000 ) ) ;
#9661 = DIRECTION ( 'NONE',  ( 0.000000000000000000, 1.000000000000000000, -1.734723475976805862E-16 ) ) ;
#9662 = CARTESIAN_POINT ( 'NONE',  ( -1.213910761154854745, 0.2952755905511810774, -0.1292274648535930714 ) ) ;
#9663 = CARTESIAN_POINT ( 'NONE',  ( -0.5118110236220466680, 0.2952755905511811885, 0.000000000000000000 ) ) ;
#9664 = CARTESIAN_POINT ( 'NONE',  ( 0.1998031496062994128, -0.3460692066303957537, -2.688320209973753538 ) ) ;
#9665 = CARTESIAN_POINT ( 'NONE',  ( 0.2427821522309719648, -0.05778040916215522460, 0.4822834645669289988 ) ) ;
#9666 = CARTESIAN_POINT ( 'NONE',  ( -0.3392501089628019439, 0.1958661417322832554, -2.311004306265404651 ) ) ;
#9667 = CARTESIAN_POINT ( 'NONE',  ( 0.5314960629920849611, 2.697625129285034618, 3.898413161119336223 ) ) ;
#9668 = CARTESIAN_POINT ( 'NONE',  ( 0.1706036745406830368, -0.3690944881889765550, -0.3153832671262227771 ) ) ;
#9669 = CARTESIAN_POINT ( 'NONE',  ( 1.135170603674541256, 0.2952755905511811885, 0.1292274648535926551 ) ) ;
#9670 = CARTESIAN_POINT ( 'NONE',  ( -1.135170603674539924, -0.5511811023622046335, 0.09757992244046803654 ) ) ;
#9671 = CARTESIAN_POINT ( 'NONE',  ( 1.115485564304462551, -0.4281496062992127816, -0.4176697321401328100 ) ) ;
#9672 = CYLINDRICAL_SURFACE ( 'NONE', #8870, 0.1968503937007874405 ) ;
#9673 = CARTESIAN_POINT ( 'NONE',  ( -0.3346456692913377662, -0.5400638737290844871, 0.3530559997133364547 ) ) ;
#9674 = CARTESIAN_POINT ( 'NONE',  ( 0.1968503937007881344, -0.5511811023622047445, 6.969142054262312111E-17 ) ) ;
#9675 = CARTESIAN_POINT ( 'NONE',  ( 1.614173228346457378, 0.2753471884572480932, -0.1372047244094471152 ) ) ;
#9676 = CARTESIAN_POINT ( 'NONE',  ( 0.4527559055118117182, -0.4536011799217367080, 0.2665933059059888421 ) ) ;
#9677 = CARTESIAN_POINT ( 'NONE',  ( -0.1246719160104980823, -0.6692913385826773087, -0.1292274648535924053 ) ) ;
#9678 = CARTESIAN_POINT ( 'NONE',  ( -0.1998031496062991630, -0.3460692066303959202, -0.1423884514435695414 ) ) ;
#9679 = CARTESIAN_POINT ( 'NONE',  ( -0.9776902887139098386, -0.6692913385826771977, 0.1292274648535927661 ) ) ;
#9680 = CARTESIAN_POINT ( 'NONE',  ( -0.3917322834645671215, 0.1049643490035301469, -1.849737532808399143 ) ) ;
#9681 = CARTESIAN_POINT ( 'NONE',  ( 0.9711286089238851948, 0.1283753931104748280, 0.1820866141732283561 ) ) ;
#9682 = CARTESIAN_POINT ( 'NONE',  ( 0.1706036745406830368, -0.4281496062992127816, -0.4176697321401328100 ) ) ;
#9683 = CARTESIAN_POINT ( 'NONE',  ( -0.2099737532808391705, 0.2306618581243848609, 0.2411417322834645549 ) ) ;
#9684 = CARTESIAN_POINT ( 'NONE',  ( -0.2099737532808391705, 0.1283753931104748280, 0.1820866141732283561 ) ) ;
#9685 = DIRECTION ( 'NONE',  ( 0.000000000000000000, 0.000000000000000000, 1.000000000000000000 ) ) ;
#9686 = CARTESIAN_POINT ( 'NONE',  ( -0.6364829396325453192, -0.08942795157528024563, -0.3641732283464568787 ) ) ;
#9687 = CARTESIAN_POINT ( 'NONE',  ( 0.1837270341207357105, -0.6046776061558809534, -0.2411417322834644161 ) ) ;
#9688 = CARTESIAN_POINT ( 'NONE',  ( -1.312335958005248715, -0.5023911411419708095, -0.1820866141732282451 ) ) ;
#9689 = CARTESIAN_POINT ( 'NONE',  ( 0.1070741851644053388, 0.3996062992125986035, -1.015091863517060267 ) ) ;
#9690 = CARTESIAN_POINT ( 'NONE',  ( -0.9908136482939626788, 0.2952755905511811885, 0.1292274648535926551 ) ) ;
#9691 = CARTESIAN_POINT ( 'NONE',  ( -1.436417322834644850, 0.8346805926620876059, 0.3149606299212598381 ) ) ;
#9692 = ORIENTED_EDGE ( 'NONE', *, *, #55305, .F. ) ;
#9693 = CARTESIAN_POINT ( 'NONE',  ( -1.732283464566928277, -0.1870078740157479769, 0.3641732283464567677 ) ) ;
#9694 = VECTOR ( 'NONE', #5943, 39.37007874015748143 ) ;
#9695 = CARTESIAN_POINT ( 'NONE',  ( -0.4461942257217840213, 0.2306618581243848609, 0.2411417322834645549 ) ) ;
#9696 = CARTESIAN_POINT ( 'NONE',  ( 0.2981046825593872684, 1.168156273747579688, -1.428012540953041976 ) ) ;
#9697 = CARTESIAN_POINT ( 'NONE',  ( -1.286089238845143479, 0.2306618581243847221, -0.2411417322834647770 ) ) ;
#9698 = CARTESIAN_POINT ( 'NONE',  ( 0.3392501089628018329, 0.1958661417322835607, -1.633202099737532942 ) ) ;
#9699 = DIRECTION ( 'NONE',  ( 0.000000000000000000, -1.000000000000000000, 0.000000000000000000 ) ) ;
#9700 = CARTESIAN_POINT ( 'NONE',  ( 1.430446194225722500, -0.4281496062992127816, -0.4176697321401328100 ) ) ;
#9701 = CARTESIAN_POINT ( 'NONE',  ( 1.017060367454068803, -0.3162353388693405765, 0.4822834645669290543 ) ) ;
#9702 = CARTESIAN_POINT ( 'NONE',  ( -0.2624671916010490880, 0.1539470093639521697, -0.1968503937007875793 ) ) ;
#9703 = CARTESIAN_POINT ( 'NONE',  ( 0.2407525580057140735, -0.1709688663325618085, 5.655154502652835369 ) ) ;
#9704 = CARTESIAN_POINT ( 'NONE',  ( 1.404199475065617264, -0.3690944881889763329, 0.3153832671262228327 ) ) ;
#9705 = CARTESIAN_POINT ( 'NONE',  ( -0.3996062992125987146, 0.1070741851644051862, -0.5052493438320209140 ) ) ;
#9706 = EDGE_LOOP ( 'NONE', ( #61651, #70902, #69739, #73099, #58548, #48638, #35177 ) ) ;
#9707 = CARTESIAN_POINT ( 'NONE',  ( -0.5511811023622038563, -0.1870078740157479769, 0.3641732283464567677 ) ) ;
#9708 = CARTESIAN_POINT ( 'NONE',  ( -0.3392501089628019995, 0.1958661417322832277, -2.065616797900262647 ) ) ;
#9709 = VERTEX_POINT ( 'NONE', #42955 ) ;
#9710 = CARTESIAN_POINT ( 'NONE',  ( 0.7742782152230978099, -0.4281496062992124485, 0.4176697321401328655 ) ) ;
#9711 = CARTESIAN_POINT ( 'NONE',  ( -0.2427821522309703550, -0.05778040916215560624, -0.4822834645669293319 ) ) ;
#9712 = CARTESIAN_POINT ( 'NONE',  ( -1.148293963254592542, 0.2952755905511811885, 0.1292274648535926551 ) ) ;
#9713 = CARTESIAN_POINT ( 'NONE',  ( 1.646981627296588035, -0.3162353388693405765, 0.4822834645669290543 ) ) ;
#9714 = CARTESIAN_POINT ( 'NONE',  ( -1.469816272965878357, 0.1283753931104748280, 0.1820866141732283561 ) ) ;
#9715 = CARTESIAN_POINT ( 'NONE',  ( -0.4741708390789116656, 1.554782515222133510, -2.554855015577685240 ) ) ;
#9716 = CARTESIAN_POINT ( 'NONE',  ( 0.2099737532808405305, -0.6046776061558807314, 0.2411417322834647770 ) ) ;
#9717 = CARTESIAN_POINT ( 'NONE',  ( -0.7742782152230962556, -0.4281496062992127816, -0.4176697321401328100 ) ) ;
#9718 = CARTESIAN_POINT ( 'NONE',  ( 0.1049643490035303689, 0.3917322834645668994, -1.490794332512124010 ) ) ;
#9719 = CARTESIAN_POINT ( 'NONE',  ( -1.332020997375327642, -0.05778040916215522460, 0.4822834645669289988 ) ) ;
#9720 = CARTESIAN_POINT ( 'NONE',  ( 0.06818963398612189197, 1.067605756753703172, -2.869741741654902256 ) ) ;
#9721 = CARTESIAN_POINT ( 'NONE',  ( 1.135170603674541256, -0.6692913385826773087, -0.1292274648535924053 ) ) ;
#9722 = CARTESIAN_POINT ( 'NONE',  ( 1.181102362204725198, -0.1870078740157479769, 0.3641732283464567677 ) ) ;
#9723 = ORIENTED_EDGE ( 'NONE', *, *, #7244, .F. ) ;
#9724 = CARTESIAN_POINT ( 'NONE',  ( -0.1049643490035302301, -0.3917322834645671770, -2.903562622868453680 ) ) ;
#9725 = CARTESIAN_POINT ( 'NONE',  ( -0.4265091863517051496, -0.6692913385826771977, 0.1292274648535927661 ) ) ;
#9726 = ORIENTED_EDGE ( 'NONE', *, *, #5310, .F. ) ;
#9727 = CARTESIAN_POINT ( 'NONE',  ( 0.4199475065616803948, -0.5023911411419708095, -0.1820866141732282451 ) ) ;
#9728 = CARTESIAN_POINT ( 'NONE',  ( -1.279527559055116948, -0.5400638737290844871, 0.3530559997133364547 ) ) ;
#9729 = CARTESIAN_POINT ( 'NONE',  ( 0.9120734908136489683, -0.6692913385826771977, 0.1292274648535927661 ) ) ;
#9730 = CARTESIAN_POINT ( 'NONE',  ( 0.8989501312335963501, -0.6692913385826773087, -0.1292274648535924053 ) ) ;
#9731 = EDGE_CURVE ( 'NONE', #65535, #64697, #30334, .T. ) ;
#9732 = CARTESIAN_POINT ( 'NONE',  ( -0.2493438320209966919, 0.05413385826771626580, -0.4176697321401330321 ) ) ;
#9733 = CARTESIAN_POINT ( 'NONE',  ( 0.2867679344610366554, 0.2867679344610366554, -1.394376271162416359 ) ) ;
#9734 = CARTESIAN_POINT ( 'NONE',  ( -0.8136482939632537770, 0.2306618581243847221, -0.2411417322834647770 ) ) ;
#9735 = CARTESIAN_POINT ( 'NONE',  ( 0.3917322834645669549, 0.1049643490035304660, -2.256561679790026531 ) ) ;
#9736 = CARTESIAN_POINT ( 'NONE',  ( -1.561679790026246017, 0.05413385826771666132, 0.4176697321401328100 ) ) ;
#9737 = CARTESIAN_POINT ( 'NONE',  ( -0.6692913385826764205, 0.2952755905511811885, 0.000000000000000000 ) ) ;
#9738 = CARTESIAN_POINT ( 'NONE',  ( 1.332020997375329197, -0.3162353388693405765, 0.4822834645669290543 ) ) ;
#9739 = CARTESIAN_POINT ( 'NONE',  ( 1.404199475065617708, 0.05413385826771626580, -0.4176697321401330321 ) ) ;
#9740 = CARTESIAN_POINT ( 'NONE',  ( -0.9448818897637790704, -0.1870078740157479769, 0.4822834645669291653 ) ) ;
#9741 = CARTESIAN_POINT ( 'NONE',  ( 0.2925321140481932369, 0.2925321140481932369, 0.1003937007874015769 ) ) ;
#9742 = CARTESIAN_POINT ( 'NONE',  ( 0.6889763779527563470, 0.1660481256975883668, -0.3530559997133364547 ) ) ;
#9743 = CARTESIAN_POINT ( 'NONE',  ( 0.3460692066303959757, -0.1998031496062991907, -1.837270341207349000 ) ) ;
#9744 = CARTESIAN_POINT ( 'NONE',  ( -0.4593175853018364174, -0.4281496062992127816, -0.4176697321401328100 ) ) ;
#9745 = CARTESIAN_POINT ( 'NONE',  ( -1.430446194225720724, -0.004921259842519870586, -0.3153832671262229437 ) ) ;
#9746 = CARTESIAN_POINT ( 'NONE',  ( 0.6167979002624679463, -0.004921259842519870586, -0.3153832671262229437 ) ) ;
#9747 = CARTESIAN_POINT ( 'NONE',  ( 0.2362204724409451007, -0.4091458600556402980, -0.6410761154855643129 ) ) ;
#9748 = CARTESIAN_POINT ( 'NONE',  ( 1.049868766404200349, 0.1283753931104748280, 0.1820866141732283561 ) ) ;
#9749 = CARTESIAN_POINT ( 'NONE',  ( 0.8923884514435701520, -0.6046776061558809534, -0.2411417322834644161 ) ) ;
#9750 = CARTESIAN_POINT ( 'NONE',  ( -0.1974969037888706924, 0.3420746716998658843, -0.5623359580052492701 ) ) ;
#9751 = CARTESIAN_POINT ( 'NONE',  ( -0.4396325459317579898, 0.2952755905511811885, 0.1292274648535926551 ) ) ;
#9752 = DIRECTION ( 'NONE',  ( -1.000000000000000000, 0.000000000000000000, -3.491481338843132961E-15 ) ) ;
#9753 = CARTESIAN_POINT ( 'NONE',  ( 1.410761154855643795, -0.2845877964562159024, 0.3641732283464567677 ) ) ;
#9754 = CARTESIAN_POINT ( 'NONE',  ( -0.5971128608923877978, 0.2952755905511811885, 0.1292274648535926551 ) ) ;
#9755 = CARTESIAN_POINT ( 'NONE',  ( 0.1974969037888706092, -0.3420746716998660508, -0.4835958005249345049 ) ) ;
#9756 = CARTESIAN_POINT ( 'NONE',  ( 1.371391076115485941, 0.2952755905511811885, 0.1292274648535926551 ) ) ;
#9757 = CARTESIAN_POINT ( 'NONE',  ( 0.2755905511811031494, -0.6692913385826771977, 8.415575281601705876E-17 ) ) ;
#9758 = AXIS2_PLACEMENT_3D ( 'NONE', #68690, #23649, #53976 ) ;
#9759 = CARTESIAN_POINT ( 'NONE',  ( 0.6955380577427828781, -0.3690944881889763329, 0.3153832671262228327 ) ) ;
#9760 = CARTESIAN_POINT ( 'NONE',  ( 0.4724409448818898682, 2.892866454678787531E-17, -0.1948818897637795422 ) ) ;
#9761 = CARTESIAN_POINT ( 'NONE',  ( 0.07874015748031558404, -0.1870078740157479769, 0.3641732283464567677 ) ) ;
#9762 = CARTESIAN_POINT ( 'NONE',  ( -1.502624671916009680, -0.3162353388693405765, 0.4822834645669290543 ) ) ;
#9763 = CARTESIAN_POINT ( 'NONE',  ( 0.3996062992125985480, 2.446882876249141654E-17, -1.139763779527559029 ) ) ;
#9764 = CARTESIAN_POINT ( 'NONE',  ( 0.8464566929133866546, -0.5400638737290844871, 0.3530559997133364547 ) ) ;
#9765 = CARTESIAN_POINT ( 'NONE',  ( -0.3392501089628019995, 0.1958661417322832277, -1.120734908136482799 ) ) ;
#9766 = CARTESIAN_POINT ( 'NONE',  ( 1.489501312335958172, -0.2845877964562159024, 0.3641732283464567677 ) ) ;
#9767 = CARTESIAN_POINT ( 'NONE',  ( -0.3285422586334152406, -0.2143816077119310159, -5.947530023412593222E-17 ) ) ;
#9768 = CARTESIAN_POINT ( 'NONE',  ( -0.07874015748031421014, -0.1870078740157480601, -0.3641732283464567677 ) ) ;
#9769 = CARTESIAN_POINT ( 'NONE',  ( 0.09842519685039434474, 0.1660481256975885056, 0.3530559997133364547 ) ) ;
#9770 = CARTESIAN_POINT ( 'NONE',  ( 1.272965879265092637, -0.3690944881889765550, -0.3153832671262227771 ) ) ;
#9771 = CARTESIAN_POINT ( 'NONE',  ( -1.305774278215222184, -0.5511811023622048555, -0.09757992244046775898 ) ) ;
#9772 = CARTESIAN_POINT ( 'NONE',  ( -1.587926509186350810, -0.4281496062992124485, 0.4176697321401328655 ) ) ;
#9773 = CARTESIAN_POINT ( 'NONE',  ( 0.4330708661417329575, 0.2952755905511811885, 0.000000000000000000 ) ) ;
#9774 = CARTESIAN_POINT ( 'NONE',  ( 1.358267716535433323, 0.1660481256975885056, 0.3530559997133364547 ) ) ;
#9775 = CARTESIAN_POINT ( 'NONE',  ( -2.630268417803885317, 1.724409448818897905, 0.4359958488159718093 ) ) ;
#9776 = CARTESIAN_POINT ( 'NONE',  ( -0.03937007874015669567, -0.6692913385826771977, 8.415575281601705876E-17 ) ) ;
#9777 = CARTESIAN_POINT ( 'NONE',  ( 1.181102362204725198, -0.1870078740157479769, 0.4822834645669291653 ) ) ;
#9778 = CARTESIAN_POINT ( 'NONE',  ( 0.9645669291338591078, -0.5400638737290845981, -0.3530559997133363437 ) ) ;
#9779 = AXIS2_PLACEMENT_3D ( 'NONE', #16282, #66373, #29306 ) ;
#9780 = DIRECTION ( 'NONE',  ( 0.000000000000000000, 0.000000000000000000, 1.000000000000000000 ) ) ;
#9781 = CARTESIAN_POINT ( 'NONE',  ( 0.8267716535433078384, -0.5511811023622047445, 6.969142054262312111E-17 ) ) ;
#9782 = CARTESIAN_POINT ( 'NONE',  ( 1.443569553805774897, -0.6046776061558809534, -0.2411417322834644161 ) ) ;
#9783 = CARTESIAN_POINT ( 'NONE',  ( -0.8792650918635160906, -0.3690944881889763329, 0.3153832671262228327 ) ) ;
#9784 = CARTESIAN_POINT ( 'NONE',  ( 0.3608923884514443348, 0.1771653543307087075, -0.09757992244046823083 ) ) ;
#9785 = CARTESIAN_POINT ( 'NONE',  ( -0.02624671916010428221, 0.2306618581243847221, -0.2411417322834647770 ) ) ;
#9786 = CARTESIAN_POINT ( 'NONE',  ( 0.7086614173228352742, -0.1870078740157480879, -0.4822834645669291653 ) ) ;
#9787 = CARTESIAN_POINT ( 'NONE',  ( -0.2559055118110227234, -0.5400638737290844871, 0.3530559997133364547 ) ) ;
#9788 = CARTESIAN_POINT ( 'NONE',  ( 0.03280839895013198948, 0.1771653543307087630, 0.09757992244046791164 ) ) ;
#9789 = CARTESIAN_POINT ( 'NONE',  ( 0.8464566929133865436, 0.1660481256975883668, -0.3530559997133364547 ) ) ;
#9790 = CARTESIAN_POINT ( 'NONE',  ( 2.787279214012418738, 0.000000000000000000, 0.000000000000000000 ) ) ;
#9791 = CARTESIAN_POINT ( 'NONE',  ( -0.8398950131233589023, -0.6046776061558809534, -0.2411417322834644161 ) ) ;
#9793 = DIRECTION ( 'NONE',  ( -0.000000000000000000, -1.000000000000000000, -0.000000000000000000 ) ) ;
#9792 = CARTESIAN_POINT ( 'NONE',  ( 0.000000000000000000, 2.165354330708661568, 0.000000000000000000 ) ) ;
#9794 = DIRECTION ( 'NONE',  ( 0.000000000000000000, 0.000000000000000000, 1.000000000000000000 ) ) ;
#9795 = CARTESIAN_POINT ( 'NONE',  ( -1.338582677165353729, -0.1870078740157479769, 0.4822834645669291653 ) ) ;
#9796 = CARTESIAN_POINT ( 'NONE',  ( -0.6692913385826764205, -0.6692913385826771977, 8.415575281601705876E-17 ) ) ;
#9797 = CARTESIAN_POINT ( 'NONE',  ( 0.1998031496062994405, -0.3460692066303958092, -2.926509186351706315 ) ) ;
#9798 = CARTESIAN_POINT ( 'NONE',  ( 0.2891555358219910499, -0.2891555358219909944, -2.145669291338582862 ) ) ;
#9799 = VERTEX_POINT ( 'NONE', #33148 ) ;
#9800 = CARTESIAN_POINT ( 'NONE',  ( 0.7480314960629927956, 0.1771653543307087630, 0.000000000000000000 ) ) ;
#9802 = CARTESIAN_POINT ( 'NONE',  ( 0.1958661417322836440, -0.3392501089628017219, -0.8713910761154854967 ) ) ;
#9801 = VECTOR ( 'NONE', #4463, 39.37007874015748854 ) ;
#9803 = CARTESIAN_POINT ( 'NONE',  ( 1.003937007874016185, 0.1660481256975883668, -0.3530559997133364547 ) ) ;
#9804 = DIRECTION ( 'NONE',  ( -3.096699300667737957E-16, 1.000000000000000000, -0.000000000000000000 ) ) ;
#9805 = CARTESIAN_POINT ( 'NONE',  ( -1.423884514435694859, -0.2845877964562159024, 0.3641732283464567677 ) ) ;
#9806 = CARTESIAN_POINT ( 'NONE',  ( -0.01585754980764347150, 1.062992125984252745, 1.122047244094488638 ) ) ;
#9807 = CARTESIAN_POINT ( 'NONE',  ( -1.555118110236219930, 0.1660481256975885056, 0.3530559997133364547 ) ) ;
#9808 = CARTESIAN_POINT ( 'NONE',  ( 0.2624671916010504757, 0.2306618581243848609, 0.2411417322834645549 ) ) ;
#9809 = CARTESIAN_POINT ( 'NONE',  ( 0.1049643490035304522, -0.3917322834645668994, -0.3228153298874523180 ) ) ;
#9810 = CARTESIAN_POINT ( 'NONE',  ( 0.1706036745406830368, -0.4281496062992127816, -0.4176697321401328100 ) ) ;
#9811 = CARTESIAN_POINT ( 'NONE',  ( -0.9842519685039365918, -0.5511811023622047445, 6.969142054262312111E-17 ) ) ;
#9813 = EDGE_CURVE ( 'NONE', #59522, #83292, #80656, .T. ) ;
#9812 = CARTESIAN_POINT ( 'NONE',  ( 0.9711286089238851948, 0.2306618581243848609, 0.2411417322834645549 ) ) ;
#9814 = CARTESIAN_POINT ( 'NONE',  ( -0.1181102362204717315, 0.2952755905511811885, 0.000000000000000000 ) ) ;
#9815 = CARTESIAN_POINT ( 'NONE',  ( -1.603475055217291612, 2.094628720676861011, -0.04573490813648263542 ) ) ;
#9816 = CARTESIAN_POINT ( 'NONE',  ( -0.01241954290193713825, 2.784432375088962958E-17, -0.3464511005275205946 ) ) ;
#9817 = CARTESIAN_POINT ( 'NONE',  ( -0.3392501089628017219, -0.1958661417322836995, -1.624035063813334956 ) ) ;
#9818 = CARTESIAN_POINT ( 'NONE',  ( 0.7874015748031503170, -0.1870078740157480879, -0.4822834645669291653 ) ) ;
#9819 = CARTESIAN_POINT ( 'NONE',  ( 0.1246719160104994284, -0.6692913385826771977, 0.1292274648535927661 ) ) ;
#9820 = CARTESIAN_POINT ( 'NONE',  ( -0.8727034120734901146, -0.3162353388693405765, 0.4822834645669290543 ) ) ;
#9821 = CARTESIAN_POINT ( 'NONE',  ( 1.056430446194226436, -0.6692913385826773087, -0.1292274648535924053 ) ) ;
#9822 = ADVANCED_FACE ( 'NONE', ( #5084 ), #17730, .F. ) ;
#9823 = CARTESIAN_POINT ( 'NONE',  ( 0.3674540682414705883, -0.6046776061558807314, 0.2411417322834647770 ) ) ;
#9824 = CARTESIAN_POINT ( 'NONE',  ( -0.1958661417322836718, 0.3392501089628017219, -0.8851706036745407014 ) ) ;
#9825 = CARTESIAN_POINT ( 'NONE',  ( -0.3149606299212590610, -0.1870078740157479769, 0.4822834645669291653 ) ) ;
#9826 = CARTESIAN_POINT ( 'NONE',  ( 0.6102362204724416372, 0.1660481256975883668, -0.3530559997133364547 ) ) ;
#9827 = CARTESIAN_POINT ( 'NONE',  ( -0.1181102362204717315, -0.6692913385826771977, 8.415575281601705876E-17 ) ) ;
#9828 = CARTESIAN_POINT ( 'NONE',  ( 0.6167979002624679463, -0.004921259842519870586, -0.3153832671262229437 ) ) ;
#9829 = CARTESIAN_POINT ( 'NONE',  ( -1.443569553805773564, -0.6046776061558807314, 0.2411417322834647770 ) ) ;
#9830 = CARTESIAN_POINT ( 'NONE',  ( -0.6299212598425230070, 0.000000000000000000, 0.9285414500055690912 ) ) ;
#9831 = CARTESIAN_POINT ( 'NONE',  ( 0.1706036745406830368, 0.05413385826771666132, 0.4176697321401328100 ) ) ;
#9832 = CARTESIAN_POINT ( 'NONE',  ( -0.4724409448818896462, -0.1265901696524993070, -0.9101049868766404316 ) ) ;
#9833 = CARTESIAN_POINT ( 'NONE',  ( -0.1049643490035307020, 0.3917322834645669549, -2.203412073490814027 ) ) ;
#9834 = VERTEX_POINT ( 'NONE', #43358 ) ;
#9835 = ORIENTED_EDGE ( 'NONE', *, *, #67540, .T. ) ;
#9836 = CARTESIAN_POINT ( 'NONE',  ( 1.167979002624672580, -0.4281496062992124485, 0.4176697321401328655 ) ) ;
#9837 = CARTESIAN_POINT ( 'NONE',  ( 0.5708661417322841158, -0.4536011799217368745, -0.2665933059059886201 ) ) ;
#9839 = CARTESIAN_POINT ( 'NONE',  ( -3.237502116762790205, 2.729657714433391114, -0.5314960629921260393 ) ) ;
#9838 = DIRECTION ( 'NONE',  ( 0.000000000000000000, 0.000000000000000000, -1.000000000000000000 ) ) ;
#9840 = CARTESIAN_POINT ( 'NONE',  ( 0.1049643490035304938, -0.3917322834645669549, -0.7998687664041995715 ) ) ;
#9841 = FACE_OUTER_BOUND ( 'NONE', #23892, .T. ) ;
#9842 = FILL_AREA_STYLE ('',( #15337 ) ) ;
#9843 = CARTESIAN_POINT ( 'NONE',  ( 0.3917322834645670104, -0.1049643490035303411, -1.456036745406824151 ) ) ;
#9844 = CARTESIAN_POINT ( 'NONE',  ( -0.1998031496062994405, 0.3460692066303957537, -2.452099737532808188 ) ) ;
#9845 = CARTESIAN_POINT ( 'NONE',  ( 0.9645669291338588858, 0.1660481256975885056, 0.3530559997133364547 ) ) ;
#9846 = CARTESIAN_POINT ( 'NONE',  ( -0.8989501312335946848, -0.6692913385826771977, 0.1292274648535927661 ) ) ;
#9847 = VECTOR ( 'NONE', #27578, 39.37007874015748143 ) ;
#9848 = CARTESIAN_POINT ( 'NONE',  ( -0.8989501312335946848, 0.2952755905511810774, -0.1292274648535930714 ) ) ;
#9849 = CARTESIAN_POINT ( 'NONE',  ( 0.5380577427821529035, 0.05413385826771626580, -0.4176697321401330321 ) ) ;
#9850 = ORIENTED_EDGE ( 'NONE', *, *, #10428, .F. ) ;
#9851 = CARTESIAN_POINT ( 'NONE',  ( 1.233595800524935227, -0.6046776061558807314, 0.2411417322834647770 ) ) ;
#9852 = CARTESIAN_POINT ( 'NONE',  ( -1.044082653748674261, 1.299084363779800411, 0.4113579841234183410 ) ) ;
#9853 = CONTEXT_DEPENDENT_SHAPE_REPRESENTATION ( #57266, #53380 ) ;
#9854 = DIRECTION ( 'NONE',  ( 0.000000000000000000, 0.000000000000000000, 1.000000000000000000 ) ) ;
#9855 = CARTESIAN_POINT ( 'NONE',  ( -0.3996062992125986035, 0.1070741851644051584, -1.999343832020997525 ) ) ;
#9856 = CARTESIAN_POINT ( 'NONE',  ( -1.377952755905511140, -0.5511811023622047445, 6.969142054262312111E-17 ) ) ;
#9857 = CARTESIAN_POINT ( 'NONE',  ( 1.840814949217404406, 2.729664702882089067, 0.5314960629921260393 ) ) ;
#9858 = CARTESIAN_POINT ( 'NONE',  ( 0.3608923884514443348, -0.6692913385826771977, 0.1292274648535927661 ) ) ;
#9860 = DIRECTION ( 'NONE',  ( 0.000000000000000000, 0.000000000000000000, -1.000000000000000000 ) ) ;
#9859 = CARTESIAN_POINT ( 'NONE',  ( -1.559171609364246924, 0.3937007874015748254, 0.4177787735906735578 ) ) ;
#9861 = CARTESIAN_POINT ( 'NONE',  ( -1.049868766404198794, 0.1283753931104746893, -0.1820866141732285504 ) ) ;
#9862 = CARTESIAN_POINT ( 'NONE',  ( 0.3215223097112867578, -0.3162353388693409650, -0.4822834645669289433 ) ) ;
#9863 = CARTESIAN_POINT ( 'NONE',  ( 1.253280839895013710, -0.2845877964562159024, 0.3641732283464567677 ) ) ;
#9864 = CARTESIAN_POINT ( 'NONE',  ( -0.2867679344610366554, 0.2867679344610365444, -1.044600106790339433 ) ) ;
#9865 = AXIS2_PLACEMENT_3D ( 'NONE', #70322, #38753, #12677 ) ;
#9866 = CARTESIAN_POINT ( 'NONE',  ( -1.122047244094487306, -0.4536011799217367080, 0.2665933059059888421 ) ) ;
#9867 = CARTESIAN_POINT ( 'NONE',  ( 1.259842519685040019, -0.1870078740157480879, -0.4822834645669291653 ) ) ;
#9868 = CARTESIAN_POINT ( 'NONE',  ( 0.3130345246323552599, 1.559122693537392745, 0.003049358274158167365 ) ) ;
#9869 = CARTESIAN_POINT ( 'NONE',  ( -0.3608923884514428360, -0.6692913385826773087, -0.1292274648535924053 ) ) ;
#9870 = CARTESIAN_POINT ( 'NONE',  ( -1.364829396325458521, -0.5023911411419708095, 0.1820866141732285504 ) ) ;
#9871 = CARTESIAN_POINT ( 'NONE',  ( -0.3346456692913377662, -0.4536011799217367080, 0.2665933059059888421 ) ) ;
#9872 = CARTESIAN_POINT ( 'NONE',  ( -0.7152230971128602510, -0.05778040916215560624, -0.4822834645669293319 ) ) ;
#9873 = CARTESIAN_POINT ( 'NONE',  ( -1.450131233595799651, 0.1771653543307087075, -0.09757992244046823083 ) ) ;
#9874 = CARTESIAN_POINT ( 'NONE',  ( -0.3392501089628017219, -0.1958661417322836995, -0.5216728590889256889 ) ) ;
#9875 = CARTESIAN_POINT ( 'NONE',  ( 0.1771653543307093182, 0.1660481256975885056, 0.3530559997133364547 ) ) ;
#9876 = DIRECTION ( 'NONE',  ( 0.000000000000000000, -1.000000000000000000, 0.000000000000000000 ) ) ;
#9877 = CARTESIAN_POINT ( 'NONE',  ( -0.4724409448818898682, -8.678599364036362592E-17, -1.848425196850393526 ) ) ;
#9878 = CARTESIAN_POINT ( 'NONE',  ( -1.207349081364828880, 0.2306618581243847221, -0.2411417322834647770 ) ) ;
#9879 = CARTESIAN_POINT ( 'NONE',  ( -0.6364829396325453192, -0.2845877964562159024, 0.3641732283464567677 ) ) ;
#9880 = CARTESIAN_POINT ( 'NONE',  ( -1.568241469816272105, -0.3162353388693409650, -0.4822834645669289433 ) ) ;
#9881 = CARTESIAN_POINT ( 'NONE',  ( -0.01968503937007793844, 0.1660481256975883668, -0.3530559997133364547 ) ) ;
#9882 = CARTESIAN_POINT ( 'NONE',  ( 0.2427821522309719648, -0.08942795157527998196, 0.3641732283464567121 ) ) ;
#9883 = CARTESIAN_POINT ( 'NONE',  ( -1.017060367454067249, -0.2845877964562161244, -0.3641732283464567121 ) ) ;
#9884 = CARTESIAN_POINT ( 'NONE',  ( -1.456692913385826182, -0.6692913385826771977, 8.415575281601705876E-17 ) ) ;
#9885 = CARTESIAN_POINT ( 'NONE',  ( -1.469816272965878357, -0.6046776061558809534, -0.2411417322834644161 ) ) ;
#9886 = CARTESIAN_POINT ( 'NONE',  ( 1.312335958005250269, -0.6046776061558807314, 0.2411417322834647770 ) ) ;
#9887 = CARTESIAN_POINT ( 'NONE',  ( 0.2642730939577003224, 1.143123705106234622, 1.923655279115566996 ) ) ;
#9888 = CARTESIAN_POINT ( 'NONE',  ( 0.4658792650918641698, -0.08942795157528024563, -0.3641732283464568787 ) ) ;
#9889 = CARTESIAN_POINT ( 'NONE',  ( 0.7742782152230979209, 0.05413385826771626580, -0.4176697321401330321 ) ) ;
#9890 = DIRECTION ( 'NONE',  ( 3.096699300667737957E-16, -1.000000000000000000, 0.000000000000000000 ) ) ;
#9891 = CARTESIAN_POINT ( 'NONE',  ( 1.332020997375328974, -0.08942795157528024563, -0.3641732283464568787 ) ) ;
#9892 = VERTEX_POINT ( 'NONE', #81711 ) ;
#9893 = CARTESIAN_POINT ( 'NONE',  ( -1.069553805774277722, -0.6692913385826773087, -0.1292274648535924053 ) ) ;
#9894 = CARTESIAN_POINT ( 'NONE',  ( -0.9645669291338575535, 0.1660481256975883668, -0.3530559997133364547 ) ) ;
#9895 = CARTESIAN_POINT ( 'NONE',  ( 0.3871391076115492380, -0.05778040916215560624, -0.4822834645669293319 ) ) ;
#9896 = CARTESIAN_POINT ( 'NONE',  ( -1.423884514435694859, -0.2845877964562159024, 0.3641732283464567677 ) ) ;
#9897 = CARTESIAN_POINT ( 'NONE',  ( 0.3460692066303959202, -0.1998031496062991630, -2.229002624671916344 ) ) ;
#9898 = CARTESIAN_POINT ( 'NONE',  ( 1.574803149606299746, -0.1870078740157479769, 0.3641732283464567677 ) ) ;
#9899 = CARTESIAN_POINT ( 'NONE',  ( 0.2362204724409456558, -0.1870078740157479769, 0.4822834645669291653 ) ) ;
#9900 = CARTESIAN_POINT ( 'NONE',  ( 0.8267716535433077274, 0.2952755905511811885, 0.000000000000000000 ) ) ;
#9901 = DIRECTION ( 'NONE',  ( -0.000000000000000000, -1.000000000000000000, -0.000000000000000000 ) ) ;
#9902 = CARTESIAN_POINT ( 'NONE',  ( 4.893765752498283924E-17, -0.3996062992125986035, -1.653543307086614123 ) ) ;
#9903 = CARTESIAN_POINT ( 'NONE',  ( -0.3949938075777409408, -0.1058382717557502933, -1.148293963254593431 ) ) ;
#9904 = CARTESIAN_POINT ( 'NONE',  ( 0.1070741851644054915, -0.3996062992125986035, -2.604986876640420057 ) ) ;
#9905 = DIRECTION ( 'NONE',  ( 0.000000000000000000, -0.000000000000000000, 1.000000000000000000 ) ) ;
#9906 = CARTESIAN_POINT ( 'NONE',  ( -0.1958661417322834220, -0.3392501089628018884, -0.3727034120734908362 ) ) ;
#9907 = CARTESIAN_POINT ( 'NONE',  ( -0.09842519685039295696, 0.07958543189024071263, -0.2665933059059888421 ) ) ;
#9908 = CARTESIAN_POINT ( 'NONE',  ( -0.3543307086614165824, -0.6692913385826771977, 8.415575281601705876E-17 ) ) ;
#9909 = CARTESIAN_POINT ( 'NONE',  ( 1.082677165354331228, -0.5400638737290844871, 0.3530559997133364547 ) ) ;
#9910 = CARTESIAN_POINT ( 'NONE',  ( -0.3949938075777409963, -7.255918531996591613E-17, -2.005905511811023612 ) ) ;
#9911 = CARTESIAN_POINT ( 'NONE',  ( -0.1771653543307080136, 0.07958543189024071263, -0.2665933059059888421 ) ) ;
#9912 = CARTESIAN_POINT ( 'NONE',  ( -0.9448818897637790704, -0.1870078740157480879, -0.4822834645669291653 ) ) ;
#9913 = CARTESIAN_POINT ( 'NONE',  ( 1.036745406824147508, -0.4281496062992127816, -0.4176697321401328100 ) ) ;
#9914 = CARTESIAN_POINT ( 'NONE',  ( 0.2362204724409451007, -0.4091458600556402980, -2.611548556430446144 ) ) ;
#9915 = CARTESIAN_POINT ( 'NONE',  ( -0.2925321140481932924, 0.2925321140481931814, -1.751968503937007648 ) ) ;
#9916 = CARTESIAN_POINT ( 'NONE',  ( -1.157146581871515012E-16, 0.4724409448818898682, -2.753937007874015741 ) ) ;
#9917 = VERTEX_POINT ( 'NONE', #30753 ) ;
#9918 = CARTESIAN_POINT ( 'NONE',  ( 0.8333333333333340365, 0.2952755905511810774, -0.1292274648535930714 ) ) ;
#9919 = VECTOR ( 'NONE', #21831, 39.37007874015748143 ) ;
#9920 = CARTESIAN_POINT ( 'NONE',  ( -1.502624671916009680, -0.05778040916215560624, -0.4822834645669293319 ) ) ;
#9922 = CARTESIAN_POINT ( 'NONE',  ( -1.640419947506561060, 0.05413385826771666132, 0.4176697321401328100 ) ) ;
#9921 = CARTESIAN_POINT ( 'NONE',  ( 1.548556430446194954, 0.2306618581243847221, -0.2411417322834647770 ) ) ;
#9923 = CARTESIAN_POINT ( 'NONE',  ( -0.1958661417322836440, 0.3392501089628016664, -2.770321891567242734 ) ) ;
#9924 = CARTESIAN_POINT ( 'NONE',  ( -1.003937007874014853, 0.1012011053420777407, 0.2882089793578256898 ) ) ;
#9925 = CARTESIAN_POINT ( 'NONE',  ( 1.266404199475066328, -0.3162353388693409650, -0.4822834645669289433 ) ) ;
#9926 = CARTESIAN_POINT ( 'NONE',  ( 1.016821367227983552, 1.537401574803149984, 0.4744094488188975722 ) ) ;
#9927 = CARTESIAN_POINT ( 'NONE',  ( -0.1837270341207343505, -0.6046776061558807314, 0.2411417322834647770 ) ) ;
#9928 = CARTESIAN_POINT ( 'NONE',  ( -0.6692913385826764205, -0.6692913385826771977, 8.415575281601705876E-17 ) ) ;
#9929 = CARTESIAN_POINT ( 'NONE',  ( 1.614173228346457378, 0.2952755905511811885, 0.000000000000000000 ) ) ;
#9930 = CARTESIAN_POINT ( 'NONE',  ( -0.1958661417322836718, 0.3392501089628017219, -0.2552493438320210806 ) ) ;
#9931 = CARTESIAN_POINT ( 'NONE',  ( 0.2230971128608929543, 0.05413385826771626580, -0.4176697321401330321 ) ) ;
#9932 = CARTESIAN_POINT ( 'NONE',  ( 4.797336870675656522E-17, -0.3917322834645670104, -2.275590551181102317 ) ) ;
#9933 = CARTESIAN_POINT ( 'NONE',  ( -1.482939632545930975, -0.004921259842519576551, 0.3153832671262227771 ) ) ;
#9934 = ORIENTED_EDGE ( 'NONE', *, *, #1832, .F. ) ;
#9935 = CARTESIAN_POINT ( 'NONE',  ( 0.3420746716998659953, 0.1974969037888705536, -2.178477690288714186 ) ) ;
#9936 = VERTEX_POINT ( 'NONE', #82519 ) ;
#9937 = DIRECTION ( 'NONE',  ( 0.000000000000000000, -0.5150380749100564870, -0.8571673007021107793 ) ) ;
#9938 = CARTESIAN_POINT ( 'NONE',  ( -1.666666666666665853, 0.05413385826771626580, -0.4176697321401330321 ) ) ;
#9939 = CARTESIAN_POINT ( 'NONE',  ( 0.3996062992125986590, -0.1070741851644053111, -1.213910761154855189 ) ) ;
#9940 = CARTESIAN_POINT ( 'NONE',  ( 0.5626772485143710645, 7.570362723507360306E-16, 0.3791483426435171555 ) ) ;
#9941 = CARTESIAN_POINT ( 'NONE',  ( 0.4724409448818898682, 2.892866454678787531E-17, -0.8248031496062991907 ) ) ;
#9942 = DIRECTION ( 'NONE',  ( 0.000000000000000000, 0.000000000000000000, 1.000000000000000000 ) ) ;
#9943 = CARTESIAN_POINT ( 'NONE',  ( 0.009627693921961720178, -0.3964540044758448900, -2.755905511808609987 ) ) ;
#9944 = CARTESIAN_POINT ( 'NONE',  ( 0.3917322834645670104, -0.1049643490035303411, -0.03871391076115493490 ) ) ;
#9945 = CARTESIAN_POINT ( 'NONE',  ( -0.2362204724409440182, -0.1870078740157479769, 0.3641732283464567677 ) ) ;
#9946 = CARTESIAN_POINT ( 'NONE',  ( -0.8923884514435688198, 0.1283753931104746893, -0.1820866141732285504 ) ) ;
#9947 = CARTESIAN_POINT ( 'NONE',  ( -1.036745406824146176, -0.4281496062992124485, 0.4176697321401328655 ) ) ;
#9948 = CARTESIAN_POINT ( 'NONE',  ( 0.7020997375328090762, -0.05778040916215560624, -0.4822834645669293319 ) ) ;
#9949 = CARTESIAN_POINT ( 'NONE',  ( -1.476377952755905110, 0.1660481256975885056, 0.3530559997133364547 ) ) ;
#9950 = CARTESIAN_POINT ( 'NONE',  ( -0.1049643490035307020, 0.3917322834645669549, 0.1587926509186352031 ) ) ;
#9951 = VERTEX_POINT ( 'NONE', #71031 ) ;
#9952 = EDGE_CURVE ( 'NONE', #60445, #26484, #56416, .T. ) ;
#9953 = B_SPLINE_CURVE_WITH_KNOTS ( 'NONE', 3,
 ( #3757, #37797, #48772, #62656 ),
 .UNSPECIFIED., .F., .F.,
 ( 4, 4 ),
 ( 0.2160131946215620991, 0.2174264745397616883 ),
 .UNSPECIFIED. ) ;
#9954 = CARTESIAN_POINT ( 'NONE',  ( -1.227034120734907141, -0.6692913385826773087, -0.1292274648535924053 ) ) ;
#9955 = LINE ( 'NONE', #35626, #23194 ) ;
#9956 =( LENGTH_UNIT ( ) NAMED_UNIT ( * ) SI_UNIT ( $, .METRE. ) );
#9957 = CARTESIAN_POINT ( 'NONE',  ( 0.4724409448818897572, -0.1265901696524988906, -1.528871391076114916 ) ) ;
#9958 = CARTESIAN_POINT ( 'NONE',  ( 1.915796337058191412, 1.134406187872327054, -0.2508088161067802413 ) ) ;
#9959 = EDGE_CURVE ( 'NONE', #19993, #312, #74981, .T. ) ;
#9960 = CARTESIAN_POINT ( 'NONE',  ( 4.797336870675656522E-17, -0.3917322834645670104, -0.5433070866141732624 ) ) ;
#9961 = FACE_OUTER_BOUND ( 'NONE', #63745, .T. ) ;
#9962 = CARTESIAN_POINT ( 'NONE',  ( -0.8595800524934373854, -0.05778040916215522460, 0.4822834645669289988 ) ) ;
#9963 = CARTESIAN_POINT ( 'NONE',  ( 1.587926509186352586, -0.4281496062992127816, -0.4176697321401328100 ) ) ;
#9965 = CARTESIAN_POINT ( 'NONE',  ( -0.4359958488159811907, 1.724409448818897905, 2.630268417803910186 ) ) ;
#9964 = DIRECTION ( 'NONE',  ( -0.000000000000000000, -1.000000000000000000, 0.000000000000000000 ) ) ;
#9966 = CARTESIAN_POINT ( 'NONE',  ( 1.673228346456693494, 0.1660481256975885056, 0.3530559997133364547 ) ) ;
#9967 = CARTESIAN_POINT ( 'NONE',  ( -0.8530183727034112984, -0.4281496062992127816, -0.4176697321401328100 ) ) ;
#9969 = B_SPLINE_CURVE_WITH_KNOTS ( 'NONE', 3,
 ( #65544, #33121, #46151, #33539 ),
 .UNSPECIFIED., .F., .F.,
 ( 4, 4 ),
 ( 3.593986969187450165E-07, 0.001287825409103264106 ),
 .UNSPECIFIED. ) ;
#9968 = CARTESIAN_POINT ( 'NONE',  ( -0.3917322834645670659, 0.1049643490035301607, 0.04463873835401757639 ) ) ;
#9970 = CARTESIAN_POINT ( 'NONE',  ( 0.1181102362204730916, -0.5511811023622047445, 6.969142054262312111E-17 ) ) ;
#9971 = CARTESIAN_POINT ( 'NONE',  ( -0.3392501089628019995, 0.1958661417322832277, -0.5833333333333334814 ) ) ;
#9972 = AXIS2_PLACEMENT_3D ( 'NONE', #7443, #51609, #33114 ) ;
#9973 = CARTESIAN_POINT ( 'NONE',  ( -0.1377952755905504645, -0.4536011799217368745, -0.2665933059059886201 ) ) ;
#9974 = CARTESIAN_POINT ( 'NONE',  ( 0.9711286089238851948, 0.1283753931104748280, 0.1820866141732283561 ) ) ;
#9975 = CARTESIAN_POINT ( 'NONE',  ( 0.6955380577427828781, 0.05413385826771626580, -0.4176697321401330321 ) ) ;
#9976 = PRODUCT_DEFINITION_CONTEXT ( 'detailed design', #45472, 'design' ) ;
#9977 = CARTESIAN_POINT ( 'NONE',  ( -0.3740157480314953431, 0.07958543189024085140, 0.2665933059059887866 ) ) ;
#9978 = CARTESIAN_POINT ( 'NONE',  ( 4.797336870675656522E-17, -0.3917322834645670104, -2.275590551181102317 ) ) ;
#9979 = CARTESIAN_POINT ( 'NONE',  ( -1.568241469816272105, -0.3162353388693409650, -0.4822834645669289433 ) ) ;
#9980 = EDGE_CURVE ( 'NONE', #7209, #75163, #77940, .T. ) ;
#9981 = CARTESIAN_POINT ( 'NONE',  ( -1.377952755905511140, -0.5511811023622047445, 6.969142054262312111E-17 ) ) ;
#9982 = CARTESIAN_POINT ( 'NONE',  ( 0.4091458600556403535, 0.2362204724409449896, -0.3654855643044619407 ) ) ;
#9983 = CARTESIAN_POINT ( 'NONE',  ( 0.1049868766404206816, -0.6046776061558809534, -0.2411417322834644161 ) ) ;
#9984 = EDGE_CURVE ( 'NONE', #55534, #1065, #26410, .T. ) ;
#9985 = CARTESIAN_POINT ( 'NONE',  ( -0.5511811023622038563, -0.1870078740157479769, 0.4822834645669291653 ) ) ;
#9986 = CARTESIAN_POINT ( 'NONE',  ( 1.686351706036745890, 0.1771653543307087630, 0.09757992244046791164 ) ) ;
#9987 = CONICAL_SURFACE ( 'NONE', #77147, 0.1771653543307086798, 0.7853981633974482790 ) ;
#9988 = CARTESIAN_POINT ( 'NONE',  ( 0.4986876640419954376, 0.1283753931104748280, 0.1820866141732283561 ) ) ;
#9989 = CARTESIAN_POINT ( 'NONE',  ( -0.1771653543307080136, -0.5400638737290844871, 0.3530559997133364547 ) ) ;
#9990 = CARTESIAN_POINT ( 'NONE',  ( -0.5905511811023613777, -0.6692913385826771977, 8.415575281601705876E-17 ) ) ;
#9991 = PLANE ( 'NONE',  #42565 ) ;
#9992 = DIRECTION ( 'NONE',  ( 0.000000000000000000, 1.000000000000000000, 0.000000000000000000 ) ) ;
#9993 = CARTESIAN_POINT ( 'NONE',  ( -0.03937007874015669567, 0.2952755905511811885, 0.000000000000000000 ) ) ;
#9994 = EDGE_LOOP ( 'NONE', ( #81531, #69446, #25715, #3520 ) ) ;
#9995 = CARTESIAN_POINT ( 'NONE',  ( 0.3996062992125986035, -0.1070741851644052972, -1.605643044619422977 ) ) ;
#9996 = CARTESIAN_POINT ( 'NONE',  ( 1.509186351706037543, -0.4281496062992127816, -0.4176697321401328100 ) ) ;
#9997 = CARTESIAN_POINT ( 'NONE',  ( -0.2034120734908131112, -0.5511811023622048555, -0.09757992244046775898 ) ) ;
#9998 = CARTESIAN_POINT ( 'NONE',  ( -0.6102362204724400829, 0.1660481256975885056, 0.3530559997133364547 ) ) ;
#9999 = CARTESIAN_POINT ( 'NONE',  ( -1.522309711286088607, -0.5023911411419708095, 0.1820866141732285504 ) ) ;
#10000 = CARTESIAN_POINT ( 'NONE',  ( 1.522309711286089939, 0.2306618581243848609, 0.2411417322834645549 ) ) ;
#10001 = CARTESIAN_POINT ( 'NONE',  ( -1.646981627296586703, -0.05778040916215522460, 0.4822834645669289988 ) ) ;
#10002 = CARTESIAN_POINT ( 'NONE',  ( -0.8070866141732276899, -0.4536011799217367080, 0.2665933059059888421 ) ) ;
#10003 = CARTESIAN_POINT ( 'NONE',  ( 0.3996062992125984925, 0.1070741851644054499, -0.3589238845144357426 ) ) ;
#10004 = CARTESIAN_POINT ( 'NONE',  ( 4.893765752498283924E-17, -0.3996062992125986035, -0.7086614173228346081 ) ) ;
#10005 = CARTESIAN_POINT ( 'NONE',  ( -0.1058382717557497937, -0.3949938075777411628, 0.08530183727034117147 ) ) ;
#10006 = CARTESIAN_POINT ( 'NONE',  ( 1.456692913385827515, -0.5511811023622047445, 6.969142054262312111E-17 ) ) ;
#10007 = CARTESIAN_POINT ( 'NONE',  ( 0.9842519685039375910, 0.1771653543307087630, 0.000000000000000000 ) ) ;
#10008 = CARTESIAN_POINT ( 'NONE',  ( 0.9055118110236227702, -0.6692913385826771977, 8.415575281601705876E-17 ) ) ;
#10009 = CARTESIAN_POINT ( 'NONE',  ( 0.4133858267716541968, 0.1012011053420777407, 0.2882089793578256898 ) ) ;
#10010 = CARTESIAN_POINT ( 'NONE',  ( 0.8530183727034126306, 0.05413385826771626580, -0.4176697321401330321 ) ) ;
#10011 = CARTESIAN_POINT ( 'NONE',  ( 0.1058382717557500852, -0.3949938075777408852, -1.106955380577427706 ) ) ;
#10012 = CARTESIAN_POINT ( 'NONE',  ( 1.397637795275591177, 0.07958543189024071263, -0.2665933059059888421 ) ) ;
#10013 = CARTESIAN_POINT ( 'NONE',  ( -0.07874015748031421014, -0.1870078740157479769, 0.4822834645669291653 ) ) ;
#10014 = CARTESIAN_POINT ( 'NONE',  ( -0.6627296587926501115, 0.2952755905511810774, -0.1292274648535930714 ) ) ;
#10015 = CARTESIAN_POINT ( 'NONE',  ( 1.587926509186352586, -0.4281496062992127816, -0.4176697321401328100 ) ) ;
#10016 = CARTESIAN_POINT ( 'NONE',  ( 0.4724409448818897572, -0.1265901696524988906, -1.056430446194225992 ) ) ;
#10017 = CARTESIAN_POINT ( 'NONE',  ( -0.1070741851644051862, -0.3996062992125986590, -2.276902887139107268 ) ) ;
#10018 = CARTESIAN_POINT ( 'NONE',  ( 0.5118110236220478892, 0.1771653543307087630, 0.000000000000000000 ) ) ;
#10019 = ORIENTED_EDGE ( 'NONE', *, *, #19613, .F. ) ;
#10020 = CARTESIAN_POINT ( 'NONE',  ( -0.2867679344610365444, -0.2867679344610367664, -0.8431951688002119472 ) ) ;
#10021 = ORIENTED_EDGE ( 'NONE', *, *, #15160, .F. ) ;
#10022 = CARTESIAN_POINT ( 'NONE',  ( -0.3608923884514428360, -0.6692913385826773087, -0.1292274648535924053 ) ) ;
#10023 = CARTESIAN_POINT ( 'NONE',  ( -0.2362204724409440182, -0.1870078740157479769, 0.4822834645669291653 ) ) ;
#10024 = CARTESIAN_POINT ( 'NONE',  ( -0.1312335958005241554, -0.6046776061558809534, -0.2411417322834644161 ) ) ;
#10025 = AXIS2_PLACEMENT_3D ( 'NONE', #641, #7362, #20827 ) ;
#10026 = CARTESIAN_POINT ( 'NONE',  ( 0.7414698162729663755, 0.2952755905511811885, 0.1292274648535926551 ) ) ;
#10027 = CARTESIAN_POINT ( 'NONE',  ( -1.082677165354329896, -0.5400638737290845981, -0.3530559997133363437 ) ) ;
#10028 = CARTESIAN_POINT ( 'NONE',  ( -0.3805774278215216522, -0.4281496062992127816, -0.4176697321401328100 ) ) ;
#10029 = CARTESIAN_POINT ( 'NONE',  ( 1.213910761154856299, -0.6692913385826773087, -0.1292274648535924053 ) ) ;
#10030 = CARTESIAN_POINT ( 'NONE',  ( 1.108923884514436242, -0.05778040916215522460, 0.4822834645669289988 ) ) ;
#10031 = EDGE_CURVE ( 'NONE', #76587, #75749, #43153, .T. ) ;
#10032 = CARTESIAN_POINT ( 'NONE',  ( 0.6692913385826778638, -0.6692913385826771977, 8.415575281601705876E-17 ) ) ;
#10033 = CARTESIAN_POINT ( 'NONE',  ( 4.797336870675656522E-17, -0.3917322834645670104, -1.173228346456692828 ) ) ;
#10034 = CARTESIAN_POINT ( 'NONE',  ( 0.04593175853018440641, -0.5511811023622046335, 0.09757992244046803654 ) ) ;
#10035 = VERTEX_POINT ( 'NONE', #37480 ) ;
#10036 = CARTESIAN_POINT ( 'NONE',  ( 4.837279021331060870E-17, -0.3949938075777409963, -0.8661417322834645827 ) ) ;
#10037 = VERTEX_POINT ( 'NONE', #77770 ) ;
#10038 = CARTESIAN_POINT ( 'NONE',  ( -0.9186351706036736120, 0.1283753931104748280, 0.1820866141732283561 ) ) ;
#10039 = CARTESIAN_POINT ( 'NONE',  ( -0.4790026246719152336, -0.05778040916215560624, -0.4822834645669293319 ) ) ;
#10040 = CARTESIAN_POINT ( 'NONE',  ( -0.2755905511811031494, 0.000000000000000000, 6.062992125984251857 ) ) ;
#10041 = CARTESIAN_POINT ( 'NONE',  ( -0.7545931758530177724, 0.2952755905511811885, 0.1292274648535926551 ) ) ;
#10042 = CARTESIAN_POINT ( 'NONE',  ( -0.4986876640419942164, -0.6046776061558807314, 0.2411417322834647770 ) ) ;
#10043 = CARTESIAN_POINT ( 'NONE',  ( -1.135170603674539924, 0.2952755905511810774, -0.1292274648535930714 ) ) ;
#10044 = CARTESIAN_POINT ( 'NONE',  ( -1.502624671916009680, -0.05778040916215560624, -0.4822834645669293319 ) ) ;
#10045 = CIRCLE ( 'NONE', #57050, 1.122047244094488194 ) ;
#10046 = CARTESIAN_POINT ( 'NONE',  ( 0.8464566929133866546, -0.4536011799217367080, 0.2665933059059888421 ) ) ;
#10047 = LINE ( 'NONE', #61380, #41761 ) ;
#10048 = CARTESIAN_POINT ( 'NONE',  ( 0.2896968578984297493, 0.05818598865049057212, 5.869712490931006776 ) ) ;
#10049 = CARTESIAN_POINT ( 'NONE',  ( 0.6430446194225728496, -0.004921259842519576551, 0.3153832671262227771 ) ) ;
#10050 = CARTESIAN_POINT ( 'NONE',  ( -0.1377952755905504645, -0.5400638737290845981, -0.3530559997133363437 ) ) ;
#10051 = CARTESIAN_POINT ( 'NONE',  ( -0.1902887139107604098, 0.2952755905511810774, -0.1292274648535930714 ) ) ;
#10052 = ORIENTED_EDGE ( 'NONE', *, *, #13591, .F. ) ;
#10053 = CARTESIAN_POINT ( 'NONE',  ( 0.1998031496062992740, 0.3460692066303959757, -1.561679790026246684 ) ) ;
#10054 = CARTESIAN_POINT ( 'NONE',  ( -1.595398199321656829, 1.013096522517430875, 0.1559797534342477754 ) ) ;
#10055 = EDGE_LOOP ( 'NONE', ( #66268, #12524, #70904, #21274 ) ) ;
#10056 = CARTESIAN_POINT ( 'NONE',  ( -0.3996062992125986590, 0.1070741851644051723, -1.054461942257217899 ) ) ;
#10057 = CARTESIAN_POINT ( 'NONE',  ( 1.515748031496063186, -0.5400638737290845981, -0.3530559997133363437 ) ) ;
#10058 = CARTESIAN_POINT ( 'NONE',  ( -0.7874015748031489847, -0.1870078740157479769, 0.3641732283464567677 ) ) ;
#10059 = CARTESIAN_POINT ( 'NONE',  ( -0.8858267716535425107, 0.1660481256975883668, -0.3530559997133364547 ) ) ;
#10060 = CARTESIAN_POINT ( 'NONE',  ( 0.1265901696524990294, -0.4724409448818896462, -0.2427821522309711322 ) ) ;
#10061 = CARTESIAN_POINT ( 'NONE',  ( 0.3917322834645670104, 2.398668435337828261E-17, -2.722440944881889369 ) ) ;
#10062 = CARTESIAN_POINT ( 'NONE',  ( -1.489501312335957062, -0.08942795157527998196, 0.3641732283464567121 ) ) ;
#10063 = CARTESIAN_POINT ( 'NONE',  ( 0.5511811023622054106, -0.1870078740157480879, -0.4822834645669291653 ) ) ;
#10064 = CARTESIAN_POINT ( 'NONE',  ( 0.5905511811023629321, 0.2952755905511811885, 0.000000000000000000 ) ) ;
#10065 = CARTESIAN_POINT ( 'NONE',  ( -0.6824146981627288167, 0.1283753931104748280, 0.1820866141732283561 ) ) ;
#10066 = CARTESIAN_POINT ( 'NONE',  ( 0.1771653543307093182, 0.1660481256975885056, 0.3530559997133364547 ) ) ;
#10067 = CARTESIAN_POINT ( 'NONE',  ( 0.4091458600556403535, 0.2362204724409449896, -2.412729658792650778 ) ) ;
#10068 = CARTESIAN_POINT ( 'NONE',  ( -0.5446194225721777693, -0.08942795157527998196, 0.3641732283464567121 ) ) ;
#10069 = CARTESIAN_POINT ( 'NONE',  ( -0.4330708661417315697, 0.2952755905511811885, 0.000000000000000000 ) ) ;
#10070 = CARTESIAN_POINT ( 'NONE',  ( -0.1058382717557503072, 0.3949938075777408852, -1.658136482939632339 ) ) ;
#10071 = CARTESIAN_POINT ( 'NONE',  ( 1.279527559055118724, 0.07958543189024085140, 0.2665933059059887866 ) ) ;
#10072 = CARTESIAN_POINT ( 'NONE',  ( 0.04593175853018440641, 0.1771653543307087075, -0.09757992244046823083 ) ) ;
#10073 = CARTESIAN_POINT ( 'NONE',  ( 0.9711286089238851948, -0.5023911411419708095, -0.1820866141732282451 ) ) ;
#10074 = CARTESIAN_POINT ( 'NONE',  ( -1.325459317585300889, -0.4281496062992127816, -0.4176697321401328100 ) ) ;
#10075 = CARTESIAN_POINT ( 'NONE',  ( -0.8727034120734901146, -0.2845877964562159024, 0.3641732283464567677 ) ) ;
#10076 = CARTESIAN_POINT ( 'NONE',  ( 0.2362204724409449064, 0.4091458600556404646, -2.268372703412073310 ) ) ;
#10077 = CARTESIAN_POINT ( 'NONE',  ( -1.017060367454067249, -0.3162353388693409650, -0.4822834645669289433 ) ) ;
#10078 = CARTESIAN_POINT ( 'NONE',  ( -0.5839895013123351797, -0.6692913385826771977, 0.1292274648535927661 ) ) ;
#10079 = ADVANCED_FACE ( 'NONE', ( #5493 ), #31155, .T. ) ;
#10080 = CARTESIAN_POINT ( 'NONE',  ( 0.2165354330708668673, -0.5400638737290844871, 0.3530559997133364547 ) ) ;
#10081 = CARTESIAN_POINT ( 'NONE',  ( 0.2867679344610365999, 0.2867679344610365999, -2.422552862695851683 ) ) ;
#10082 = DIRECTION ( 'NONE',  ( 1.000000000000000000, 0.000000000000000000, 3.491481338843135327E-15 ) ) ;
#10083 = CARTESIAN_POINT ( 'NONE',  ( 0.4986876640419954376, -0.5023911411419708095, -0.1820866141732282451 ) ) ;
#10084 = CARTESIAN_POINT ( 'NONE',  ( 0.9776902887139113929, 0.2952755905511811885, 0.1292274648535926551 ) ) ;
#10085 = CARTESIAN_POINT ( 'NONE',  ( -1.102362204724408601, -0.1870078740157479769, 0.3641732283464567677 ) ) ;
#10086 = CARTESIAN_POINT ( 'NONE',  ( 1.089238845144357759, 0.05413385826771626580, -0.4176697321401330321 ) ) ;
#10087 = CARTESIAN_POINT ( 'NONE',  ( -1.627296587926508442, -0.5023911411419708095, -0.1820866141732282451 ) ) ;
#10088 = CARTESIAN_POINT ( 'NONE',  ( 1.587926509186352142, -0.004921259842519576551, 0.3153832671262227771 ) ) ;
#10089 = CARTESIAN_POINT ( 'NONE',  ( -0.7677165354330699465, 0.1660481256975885056, 0.3530559997133364547 ) ) ;
#10090 = CARTESIAN_POINT ( 'NONE',  ( 0.3018372703412079971, -0.004921259842519870586, -0.3153832671262229437 ) ) ;
#10091 = CARTESIAN_POINT ( 'NONE',  ( 1.607037972344098176, 0.2931805072228713116, 0.04654416842230573587 ) ) ;
#10092 = CARTESIAN_POINT ( 'NONE',  ( 0.5052493438320215802, 0.1771653543307087630, 0.09757992244046791164 ) ) ;
#10093 = AXIS2_PLACEMENT_3D ( 'NONE', #1058, #27542, #7355 ) ;
#10094 = CARTESIAN_POINT ( 'NONE',  ( -0.1640419947506553400, -0.05778040916215560624, -0.4822834645669293319 ) ) ;
#10095 = CARTESIAN_POINT ( 'NONE',  ( 0.1070741851644054776, -0.3996062992125984925, -0.3195538057742782212 ) ) ;
#10096 =( BOUNDED_CURVE ( )  B_SPLINE_CURVE ( 1, ( #70301, #43374 ),
 .UNSPECIFIED., .F., .F. ) 
 B_SPLINE_CURVE_WITH_KNOTS ( ( 2, 2 ),
 ( 3.469446951953614189E-18, 0.002000000000000008715 ),
 .UNSPECIFIED. ) 
 CURVE ( )  GEOMETRIC_REPRESENTATION_ITEM ( )  RATIONAL_B_SPLINE_CURVE ( ( 0.9875488213027523443, 0.9875488213027523443 ) ) 
 REPRESENTATION_ITEM ( '' )  );
#10097 = CARTESIAN_POINT ( 'NONE',  ( -1.010498687664041384, -0.4281496062992127816, -0.4176697321401328100 ) ) ;
#10098 = CARTESIAN_POINT ( 'NONE',  ( -0.3917322834645669549, -0.1049643490035306603, -1.705380577427821898 ) ) ;
#10099 = CARTESIAN_POINT ( 'NONE',  ( 0.9776902887139113929, 0.1771653543307087630, 0.09757992244046791164 ) ) ;
#10100 = CARTESIAN_POINT ( 'NONE',  ( 0.2362204724409456558, -0.1870078740157479769, 0.4822834645669291653 ) ) ;
#10101 = CARTESIAN_POINT ( 'NONE',  ( -0.08530183727034056085, -0.3162353388693405765, 0.4822834645669290543 ) ) ;
#10102 = CARTESIAN_POINT ( 'NONE',  ( -0.2755905511811015396, -0.5511811023622047445, 6.969142054262312111E-17 ) ) ;
#10103 = PLANE ( 'NONE',  #29293 ) ;
#10104 = CARTESIAN_POINT ( 'NONE',  ( -0.3215223097112853146, -0.08942795157528024563, -0.3641732283464568787 ) ) ;
#10105 = CARTESIAN_POINT ( 'NONE',  ( 0.4658792650918641698, -0.05778040916215560624, -0.4822834645669293319 ) ) ;
#10106 = EDGE_CURVE ( 'NONE', #43155, #5951, #54578, .T. ) ;
#10107 = CARTESIAN_POINT ( 'NONE',  ( -1.233595800524933894, 0.1283753931104748280, 0.1820866141732283561 ) ) ;
#10109 = CARTESIAN_POINT ( 'NONE',  ( -0.1070741851644051862, -0.3996062992125986590, -0.9363517060367454459 ) ) ;
#10108 = AXIS2_PLACEMENT_3D ( 'NONE', #15336, #41001, #28361 ) ;
#10110 = CARTESIAN_POINT ( 'NONE',  ( -1.509186351706035767, -0.4281496062992124485, 0.4176697321401328655 ) ) ;
#10111 = CARTESIAN_POINT ( 'NONE',  ( 0.2099737532808405305, 0.1539470093639521697, -0.1968503937007875793 ) ) ;
#10112 = ORIENTED_EDGE ( 'NONE', *, *, #43446, .F. ) ;
#10113 = EDGE_CURVE ( 'NONE', #71072, #1230, #45695, .T. ) ;
#10114 = CARTESIAN_POINT ( 'NONE',  ( -1.653543307086613234, -0.1870078740157480601, -0.3641732283464567677 ) ) ;
#10115 = CARTESIAN_POINT ( 'NONE',  ( -0.3674540682414692561, -0.6046776061558809534, -0.2411417322834644161 ) ) ;
#10116 = CARTESIAN_POINT ( 'NONE',  ( -1.036745406824146176, -0.4281496062992124485, 0.4176697321401328655 ) ) ;
#10117 = CARTESIAN_POINT ( 'NONE',  ( -0.3392501089628017219, -0.1958661417322836718, -1.554461942257217899 ) ) ;
#10118 = CARTESIAN_POINT ( 'NONE',  ( 5.785732909357575061E-17, -0.4724409448818898682, -2.125984251968504157 ) ) ;
#10119 = CARTESIAN_POINT ( 'NONE',  ( 1.286089238845145033, -0.6046776061558809534, -0.2411417322834644161 ) ) ;
#10120 = CARTESIAN_POINT ( 'NONE',  ( 0.6496062992125991586, -0.5400638737290845981, -0.3530559997133363437 ) ) ;
#10121 = CARTESIAN_POINT ( 'NONE',  ( 0.4724409448818897017, 0.1265901696524990294, -0.4396325459317584894 ) ) ;
#10122 = CARTESIAN_POINT ( 'NONE',  ( 0.2925321140481931814, -0.2925321140481931259, -2.379921259842519898 ) ) ;
#10123 = CARTESIAN_POINT ( 'NONE',  ( -1.614173228346456268, -0.6692913385826771977, 8.415575281601705876E-17 ) ) ;
#10124 = CARTESIAN_POINT ( 'NONE',  ( -0.3460692066303958092, -0.1998031496062994683, -0.5249343832020997302 ) ) ;
#10125 = ORIENTED_EDGE ( 'NONE', *, *, #38297, .F. ) ;
#10126 = CARTESIAN_POINT ( 'NONE',  ( -0.9908136482939626788, 0.1771653543307087630, 0.09757992244046791164 ) ) ;
#10127 = CARTESIAN_POINT ( 'NONE',  ( 0.2867679344610365999, -0.2867679344610365444, -2.137795275590551380 ) ) ;
#10128 = ORIENTED_EDGE ( 'NONE', *, *, #55786, .F. ) ;
#10129 = B_SPLINE_CURVE_WITH_KNOTS ( 'NONE', 3,
 ( #29259, #22534, #16232, #74720 ),
 .UNSPECIFIED., .F., .F.,
 ( 4, 4 ),
 ( 0.08225757503446740060, 0.08243036250299845547 ),
 .UNSPECIFIED. ) ;
#10130 = CARTESIAN_POINT ( 'NONE',  ( 0.9448818897637802916, -0.1870078740157479769, 0.4822834645669291653 ) ) ;
#10131 = CARTESIAN_POINT ( 'NONE',  ( -0.4855643044619415427, -0.4281496062992124485, 0.4176697321401328655 ) ) ;
#10132 = CARTESIAN_POINT ( 'NONE',  ( -1.253280839895012377, -0.3162353388693409650, -0.4822834645669289433 ) ) ;
#10133 = CARTESIAN_POINT ( 'NONE',  ( 1.174540682414699111, -0.3162353388693405765, 0.4822834645669290543 ) ) ;
#10134 = CARTESIAN_POINT ( 'NONE',  ( -1.135170603674539924, 0.1771653543307087075, -0.09757992244046823083 ) ) ;
#10135 = FACE_OUTER_BOUND ( 'NONE', #66863, .T. ) ;
#10136 = CARTESIAN_POINT ( 'NONE',  ( 0.3805774278215230400, -0.4281496062992124485, 0.4176697321401328655 ) ) ;
#10137 = CARTESIAN_POINT ( 'NONE',  ( -0.6955380577427815458, 0.05413385826771666132, 0.4176697321401328100 ) ) ;
#10138 = CARTESIAN_POINT ( 'NONE',  ( 0.3917322834645668994, -0.1049643490035303134, -1.451424253771966599 ) ) ;
#10139 = CARTESIAN_POINT ( 'NONE',  ( -1.043307086614172041, -0.5400638737290844871, 0.3530559997133364547 ) ) ;
#10140 = DIRECTION ( 'NONE',  ( -3.491481338843132961E-15, -0.000000000000000000, 1.000000000000000000 ) ) ;
#10141 = CARTESIAN_POINT ( 'NONE',  ( 1.023622047244095334, -0.1870078740157479769, 0.4822834645669291653 ) ) ;
#10142 = CARTESIAN_POINT ( 'NONE',  ( 0.1049643490035304938, -0.3917322834645669549, 0.08005249343832024356 ) ) ;
#10143 = CARTESIAN_POINT ( 'NONE',  ( 1.338582677165355062, -0.1870078740157479769, 0.3641732283464567677 ) ) ;
#10144 = ORIENTED_EDGE ( 'NONE', *, *, #22709, .F. ) ;
#10145 = CARTESIAN_POINT ( 'NONE',  ( -0.1049643490035307158, 0.3917322834645670104, -2.680465510007561836 ) ) ;
#10146 = CARTESIAN_POINT ( 'NONE',  ( -0.4855643044619415427, 0.05413385826771626580, -0.4176697321401330321 ) ) ;
#10147 = EDGE_LOOP ( 'NONE', ( #41508, #10843, #43820, #62935 ) ) ;
#10148 = CARTESIAN_POINT ( 'NONE',  ( 0.6036745406824153282, -0.5023911411419708095, 0.1820866141732285504 ) ) ;
#10149 = CARTESIAN_POINT ( 'NONE',  ( -1.601049868766403650, -0.6046776061558807314, 0.2411417322834647770 ) ) ;
#10150 = CARTESIAN_POINT ( 'NONE',  ( 1.043307086614173818, -0.5400638737290845981, -0.3530559997133363437 ) ) ;
#10151 = CARTESIAN_POINT ( 'NONE',  ( 0.9448818897637802916, -0.1870078740157479769, 0.4822834645669291653 ) ) ;
#10152 = CARTESIAN_POINT ( 'NONE',  ( -0.1246719160104980823, 0.2952755905511811885, 0.1292274648535926551 ) ) ;
#10153 = CARTESIAN_POINT ( 'NONE',  ( -9.594673741351313045E-17, 0.3917322834645670659, -1.414061310532495286 ) ) ;
#10154 = CARTESIAN_POINT ( 'NONE',  ( -0.6561679790026240244, 0.2306618581243847221, -0.2411417322834647770 ) ) ;
#10155 = CARTESIAN_POINT ( 'NONE',  ( -0.3392501089628017219, -0.1958661417322836718, -2.184383202099737797 ) ) ;
#10156 = CARTESIAN_POINT ( 'NONE',  ( -1.660104986876639543, -0.05778040916215560624, -0.4822834645669293319 ) ) ;
#10157 = CARTESIAN_POINT ( 'NONE',  ( -0.8333333333333323711, 0.2952755905511811885, 0.1292274648535926551 ) ) ;
#10158 = CARTESIAN_POINT ( 'NONE',  ( 1.345144356955381593, -0.05778040916215522460, 0.4822834645669289988 ) ) ;
#10159 = CARTESIAN_POINT ( 'NONE',  ( 1.614173228346457378, -0.6692913385826771977, 8.415575281601705876E-17 ) ) ;
#10160 = CARTESIAN_POINT ( 'NONE',  ( 0.2925321140481932369, 0.2925321140481932369, -0.2952755905511811885 ) ) ;
#10161 = CARTESIAN_POINT ( 'NONE',  ( -0.7874015748031489847, -0.1870078740157479769, 0.4822834645669291653 ) ) ;
#10162 = CARTESIAN_POINT ( 'NONE',  ( 0.2925321140481932369, -0.2925321140481931814, 0.1397637795275590289 ) ) ;
#10163 = CARTESIAN_POINT ( 'NONE',  ( 0.4199475065616803948, -0.6046776061558809534, -0.2411417322834644161 ) ) ;
#10164 = CARTESIAN_POINT ( 'NONE',  ( -0.3996062992125987146, 0.1070741851644051862, -2.080052493438320216 ) ) ;
#10165 = CARTESIAN_POINT ( 'NONE',  ( -0.4068241469816264999, -0.4281496062992124485, 0.4176697321401328655 ) ) ;
#10166 = AXIS2_PLACEMENT_3D ( 'NONE', #59869, #2223, #27888 ) ;
#10167 = CARTESIAN_POINT ( 'NONE',  ( -1.587926509186350810, -0.004921259842519870586, -0.3153832671262229437 ) ) ;
#10168 = CARTESIAN_POINT ( 'NONE',  ( 0.5314960629921267055, -0.4536011799217367080, 0.2665933059059888421 ) ) ;
#10169 = CARTESIAN_POINT ( 'NONE',  ( 1.522309711286089939, -0.6046776061558809534, -0.2411417322834644161 ) ) ;
#10170 = CARTESIAN_POINT ( 'NONE',  ( -0.3458507752293906723, -0.3458507752293910609, -0.9232283464566929387 ) ) ;
#10171 = CARTESIAN_POINT ( 'NONE',  ( 0.5971128608923891301, 0.1771653543307087075, -0.09757992244046823083 ) ) ;
#10172 = CARTESIAN_POINT ( 'NONE',  ( 0.7874015748031503170, -0.1870078740157479769, 0.4822834645669291653 ) ) ;
#10173 = CARTESIAN_POINT ( 'NONE',  ( -0.2891555358219909388, -0.2891555358219912164, -0.7657480314960630752 ) ) ;
#10174 = CARTESIAN_POINT ( 'NONE',  ( -0.3477690288713905509, -0.6692913385826771977, 0.1292274648535927661 ) ) ;
#10175 = CARTESIAN_POINT ( 'NONE',  ( 0.5314960629921372526, 2.716535433070866645, -3.224202737261813834 ) ) ;
#10176 = CARTESIAN_POINT ( 'NONE',  ( 1.332020997375328974, -0.08942795157528024563, -0.3641732283464568787 ) ) ;
#10177 = CARTESIAN_POINT ( 'NONE',  ( -0.5314960629921254842, -0.5400638737290845981, -0.3530559997133363437 ) ) ;
#10178 = CARTESIAN_POINT ( 'NONE',  ( 0.1058382717557500852, -0.3949938075777408852, -0.4770341207349081403 ) ) ;
#10179 = CARTESIAN_POINT ( 'NONE',  ( 1.345144356955381593, -0.05778040916215522460, 0.4822834645669289988 ) ) ;
#10180 = CARTESIAN_POINT ( 'NONE',  ( 0.04593175853018440641, 0.2952755905511810774, -0.1292274648535930714 ) ) ;
#10181 = CARTESIAN_POINT ( 'NONE',  ( 0.4921259842519691285, -0.4536011799217368745, -0.2665933059059886201 ) ) ;
#10182 = CARTESIAN_POINT ( 'NONE',  ( -0.3251038240001069002, 1.191559816073523237, -1.073976752645962041 ) ) ;
#10183 = CARTESIAN_POINT ( 'NONE',  ( -0.01312335958005186876, -0.004921259842519870586, -0.3153832671262229437 ) ) ;
#10184 = CARTESIAN_POINT ( 'NONE',  ( 0.6955380577427828781, -0.004921259842519870586, -0.3153832671262229437 ) ) ;
#10185 = CARTESIAN_POINT ( 'NONE',  ( 0.000000000000000000, 0.000000000000000000, 0.1574803149606299191 ) ) ;
#10186 = CARTESIAN_POINT ( 'NONE',  ( 0.2925321140481932369, 0.2925321140481932369, -1.159448818897637734 ) ) ;
#10187 = CARTESIAN_POINT ( 'NONE',  ( 0.7414698162729663755, 0.2952755905511811885, 0.1292274648535926551 ) ) ;
#10188 = CARTESIAN_POINT ( 'NONE',  ( 0.2867679344610365999, -0.2867679344610365444, -1.192913385826771755 ) ) ;
#10189 = CARTESIAN_POINT ( 'NONE',  ( 1.660104986876641320, -0.08942795157527998196, 0.3641732283464567121 ) ) ;
#10190 = CARTESIAN_POINT ( 'NONE',  ( -0.3436793299028276794, 0.1882840440723393405, 1.128668216881735357E-17 ) ) ;
#10191 = CARTESIAN_POINT ( 'NONE',  ( 0.1181102362204730916, -0.5511811023622047445, 6.969142054262312111E-17 ) ) ;
#10192 = CARTESIAN_POINT ( 'NONE',  ( 0.2821522309711292364, 0.2952755905511810774, -0.1292274648535930714 ) ) ;
#10193 = CARTESIAN_POINT ( 'NONE',  ( 1.496062992125985147, -0.1870078740157479769, 0.3641732283464567677 ) ) ;
#10194 = CARTESIAN_POINT ( 'NONE',  ( -1.148293963254592542, -0.5511811023622048555, -0.09757992244046775898 ) ) ;
#10195 = CARTESIAN_POINT ( 'NONE',  ( -1.246719160104986512, 0.05413385826771666132, 0.4176697321401328100 ) ) ;
#10196 = CARTESIAN_POINT ( 'NONE',  ( 0.3215223097112867578, -0.3162353388693409650, -0.4822834645669289433 ) ) ;
#10197 = CARTESIAN_POINT ( 'NONE',  ( 1.010498687664042716, -0.4281496062992124485, 0.4176697321401328655 ) ) ;
#10198 = CARTESIAN_POINT ( 'NONE',  ( -0.4724409448818898682, -8.678599364036362592E-17, -0.2736220472440945017 ) ) ;
#10199 = CARTESIAN_POINT ( 'NONE',  ( 0.2952755905511816326, -0.5400638737290844871, 0.3530559997133364547 ) ) ;
#10200 = CARTESIAN_POINT ( 'NONE',  ( 1.102362204724410155, -0.1870078740157480879, -0.4822834645669291653 ) ) ;
#10201 = CARTESIAN_POINT ( 'NONE',  ( 1.167979002624672580, -0.4281496062992124485, 0.4176697321401328655 ) ) ;
#10202 = CARTESIAN_POINT ( 'NONE',  ( -1.614173228346457378, 2.157411728916712068, -0.1372047244094477536 ) ) ;
#10203 = CARTESIAN_POINT ( 'NONE',  ( 0.6036745406824154392, 0.1283753931104746893, -0.1820866141732285504 ) ) ;
#10204 = CARTESIAN_POINT ( 'NONE',  ( -1.620734908136482577, 0.1771653543307087630, 0.09757992244046791164 ) ) ;
#10205 = EDGE_CURVE ( 'NONE', #77294, #74332, #4895, .T. ) ;
#10206 = CARTESIAN_POINT ( 'NONE',  ( 0.1312335958005255154, -0.5023911411419708095, 0.1820866141732285504 ) ) ;
#10207 = CARTESIAN_POINT ( 'NONE',  ( 0.1443569553805781891, 0.05413385826771626580, -0.4176697321401330321 ) ) ;
#10208 = CARTESIAN_POINT ( 'NONE',  ( 0.6889763779527563470, 0.1660481256975883668, -0.3530559997133364547 ) ) ;
#10209 = CARTESIAN_POINT ( 'NONE',  ( -0.2099737532808391705, 0.2306618581243848609, 0.2411417322834645549 ) ) ;
#10210 = CARTESIAN_POINT ( 'NONE',  ( -0.2296587926509179312, -0.2845877964562161244, -0.3641732283464567121 ) ) ;
#10211 = CARTESIAN_POINT ( 'NONE',  ( 0.9251968503937015864, -0.5400638737290844871, 0.3530559997133364547 ) ) ;
#10212 = CARTESIAN_POINT ( 'NONE',  ( 1.069553805774278832, 0.1771653543307087075, -0.09757992244046823083 ) ) ;
#10213 = CARTESIAN_POINT ( 'NONE',  ( -1.627024087650608131, 1.136692823381468598, 0.2539777673203736374 ) ) ;
#10215 = LINE ( 'NONE', #29555, #27162 ) ;
#10214 = CARTESIAN_POINT ( 'NONE',  ( 1.220472440944882164, 0.2066929133858268208, 4.479895975645240118E-15 ) ) ;
#10216 = CARTESIAN_POINT ( 'NONE',  ( -1.948818897637795367, 0.000000000000000000, 5.701968306260621233 ) ) ;
#10218 = VECTOR ( 'NONE', #68138, 39.37007874015748143 ) ;
#10217 = CARTESIAN_POINT ( 'NONE',  ( -1.384514435695537005, -0.6692913385826773087, -0.1292274648535924053 ) ) ;
#10219 = CARTESIAN_POINT ( 'NONE',  ( -0.3149606299212590610, -0.1870078740157479769, 0.4822834645669291653 ) ) ;
#10220 = CARTESIAN_POINT ( 'NONE',  ( 0.4724409448818896462, 0.1265901696524990294, -0.1246719160104986929 ) ) ;
#10221 = CARTESIAN_POINT ( 'NONE',  ( -0.1974969037888706647, 0.3420746716998658843, -2.217847769028871596 ) ) ;
#10222 = ORIENTED_EDGE ( 'NONE', *, *, #16744, .T. ) ;
#10223 = CARTESIAN_POINT ( 'NONE',  ( 0.4002624671916016896, -0.08942795157527998196, 0.3641732283464567121 ) ) ;
#10224 = CARTESIAN_POINT ( 'NONE',  ( 0.2867679344610365999, 0.2867679344610365999, -0.9173228346456693272 ) ) ;
#10225 = CARTESIAN_POINT ( 'NONE',  ( 0.9186351706036751663, -0.6046776061558807314, 0.2411417322834647770 ) ) ;
#10226 = CARTESIAN_POINT ( 'NONE',  ( 0.4091458600556404646, -0.2362204724409448231, -2.467191601049868677 ) ) ;
#10227 = CARTESIAN_POINT ( 'NONE',  ( 0.2362204724409449064, 0.4091458600556404646, -0.8510498687664042050 ) ) ;
#10228 = CARTESIAN_POINT ( 'NONE',  ( -1.305774278215222184, -0.5511811023622048555, -0.09757992244046775898 ) ) ;
#10229 = CARTESIAN_POINT ( 'NONE',  ( 1.489501312335958172, -0.3162353388693405765, 0.4822834645669290543 ) ) ;
#10230 = CARTESIAN_POINT ( 'NONE',  ( 1.535433070866142335, -0.5511811023622047445, 6.969142054262312111E-17 ) ) ;
#10231 = CARTESIAN_POINT ( 'NONE',  ( 0.4921259842519691285, -0.5400638737290845981, -0.3530559997133363437 ) ) ;
#10232 = B_SPLINE_CURVE_WITH_KNOTS ( 'NONE', 3,
 ( #955, #28268, #65344, #20719 ),
 .UNSPECIFIED., .F., .F.,
 ( 4, 4 ),
 ( 1.999999999927407068E-07, 0.006970199999999936863 ),
 .UNSPECIFIED. ) ;
#10233 = CARTESIAN_POINT ( 'NONE',  ( 0.3392501089628018329, 0.1958661417322835052, -0.3687470884176359265 ) ) ;
#10234 = CARTESIAN_POINT ( 'NONE',  ( 0.2165354330708668673, -0.5400638737290844871, 0.3530559997133364547 ) ) ;
#10235 = CARTESIAN_POINT ( 'NONE',  ( -0.9908136482939626788, -0.5511811023622048555, -0.09757992244046775898 ) ) ;
#10236 = CARTESIAN_POINT ( 'NONE',  ( 0.3083989501312343062, -0.3162353388693405765, 0.4822834645669290543 ) ) ;
#10237 = CARTESIAN_POINT ( 'NONE',  ( 0.01968503937007930540, 0.1660481256975885056, 0.3530559997133364547 ) ) ;
#10238 = DIRECTION ( 'NONE',  ( -0.000000000000000000, -1.000000000000000000, -0.000000000000000000 ) ) ;
#10239 = CARTESIAN_POINT ( 'NONE',  ( -0.1049643490035307158, 0.3917322834645670104, -1.420622990322521373 ) ) ;
#10240 = CARTESIAN_POINT ( 'NONE',  ( 0.8923884514435703741, 0.2306618581243848609, 0.2411417322834645549 ) ) ;
#10241 = CARTESIAN_POINT ( 'NONE',  ( -0.5577427821522301654, -0.05778040916215560624, -0.4822834645669293319 ) ) ;
#10242 = CARTESIAN_POINT ( 'NONE',  ( -1.089238845144356427, -0.4281496062992127816, -0.4176697321401328100 ) ) ;
#10243 = CARTESIAN_POINT ( 'NONE',  ( 1.148293963254593653, 0.2952755905511810774, -0.1292274648535930714 ) ) ;
#10244 = CARTESIAN_POINT ( 'NONE',  ( 0.5446194225721792126, -0.3162353388693405765, 0.4822834645669290543 ) ) ;
#10245 = CARTESIAN_POINT ( 'NONE',  ( -0.1049643490035307020, 0.3917322834645669549, -1.036089238845144589 ) ) ;
#10246 = CARTESIAN_POINT ( 'NONE',  ( -0.3412073490813641308, -0.6046776061558807314, 0.2411417322834647770 ) ) ;
#10247 = CARTESIAN_POINT ( 'NONE',  ( 0.3805774278215230400, -0.4281496062992124485, 0.4176697321401328655 ) ) ;
#10248 = CARTESIAN_POINT ( 'NONE',  ( -0.5380577427821514602, 0.05413385826771666132, 0.4176697321401328100 ) ) ;
#10249 = CARTESIAN_POINT ( 'NONE',  ( 0.8923884514435703741, 0.1283753931104748280, 0.1820866141732283561 ) ) ;
#10250 = CARTESIAN_POINT ( 'NONE',  ( 1.646981627296588035, -0.2845877964562159024, 0.3641732283464567677 ) ) ;
#10251 = CARTESIAN_POINT ( 'NONE',  ( -1.660104986876639543, -0.05778040916215560624, -0.4822834645669293319 ) ) ;
#10252 = CARTESIAN_POINT ( 'NONE',  ( 0.4133858267716541968, -0.5400638737290845981, -0.3530559997133363437 ) ) ;
#10253 = SURFACE_SIDE_STYLE ('',( #42221 ) ) ;
#10254 = CARTESIAN_POINT ( 'NONE',  ( 0.3392501089628018884, -0.1958661417322834220, -2.301837270341207553 ) ) ;
#10255 = ORIENTED_EDGE ( 'NONE', *, *, #3392, .T. ) ;
#10256 = ORIENTED_EDGE ( 'NONE', *, *, #82229, .T. ) ;
#10257 = CIRCLE ( 'NONE', #68057, 0.5118110236220472231 ) ;
#10258 = CARTESIAN_POINT ( 'NONE',  ( 0.7480314960629927956, 0.2952755905511811885, 0.000000000000000000 ) ) ;
#10259 = CARTESIAN_POINT ( 'NONE',  ( 0.5052493438320215802, 0.1771653543307087630, 0.09757992244046791164 ) ) ;
#10260 = AXIS2_PLACEMENT_3D ( 'NONE', #1601, #65991, #2013 ) ;
#10261 = VECTOR ( 'NONE', #1225, 39.37007874015748143 ) ;
#10263 = CARTESIAN_POINT ( 'NONE',  ( 2.554262525012302110, 1.537401574803149984, 0.4744094488188975722 ) ) ;
#10262 = CARTESIAN_POINT ( 'NONE',  ( -1.017211938244154013, 1.569780109764696396, 0.4735748448513866782 ) ) ;
#10264 = CARTESIAN_POINT ( 'NONE',  ( 0.1958661417322836440, -0.3392501089628017219, -0.9639107611548557442 ) ) ;
#10265 = CARTESIAN_POINT ( 'NONE',  ( -0.03443470937339728616, 0.000000000000000000, -1.537015892239756099 ) ) ;
#10266 =( NAMED_UNIT ( * ) SI_UNIT ( $, .STERADIAN. ) SOLID_ANGLE_UNIT ( ) );
#10267 = CARTESIAN_POINT ( 'NONE',  ( 0.3996062992125986035, -0.1070741851644052972, -2.393044619422572072 ) ) ;
#10268 = CARTESIAN_POINT ( 'NONE',  ( 0.9120734908136489683, -0.6692913385826771977, 0.1292274648535927661 ) ) ;
#10269 = CARTESIAN_POINT ( 'NONE',  ( -0.8005249343832011588, 0.05413385826771626580, -0.4176697321401330321 ) ) ;
#10270 = CARTESIAN_POINT ( 'NONE',  ( -0.5643044619422565855, 0.05413385826771626580, -0.4176697321401330321 ) ) ;
#10271 = CARTESIAN_POINT ( 'NONE',  ( 0.4986876640419954376, 0.2306618581243848609, 0.2411417322834645549 ) ) ;
#10272 = CARTESIAN_POINT ( 'NONE',  ( 1.456692913385827515, 0.2952755905511811885, 0.000000000000000000 ) ) ;
#10273 = CARTESIAN_POINT ( 'NONE',  ( -1.084117400955593835, 1.161042249202826504, 0.2904890618464239238 ) ) ;
#10274 = SHAPE_DEFINITION_REPRESENTATION ( #58731, #7298 ) ;
#10275 = CARTESIAN_POINT ( 'NONE',  ( 1.240157480314961314, 0.07958543189024071263, -0.2665933059059888421 ) ) ;
#10276 = CARTESIAN_POINT ( 'NONE',  ( 0.3996062992125985480, -0.1070741851644052972, -2.078083989501312345 ) ) ;
#10277 = CARTESIAN_POINT ( 'NONE',  ( -1.233595800524933894, -0.5023911411419708095, -0.1820866141732282451 ) ) ;
#10278 = CARTESIAN_POINT ( 'NONE',  ( 1.854472803289052507, 2.716535433070866645, 0.5314960629921260393 ) ) ;
#10279 = CARTESIAN_POINT ( 'NONE',  ( 0.1902887139107617975, -0.6692913385826773087, -0.1292274648535924053 ) ) ;
#10280 = AXIS2_PLACEMENT_3D ( 'NONE', #13681, #65021, #65453 ) ;
#10282 = CARTESIAN_POINT ( 'NONE',  ( -0.1938976377952756625, 0.1938976377952755792, -0.3740157480314971750 ) ) ;
#10281 = CARTESIAN_POINT ( 'NONE',  ( 1.213910761154856299, 0.2952755905511811885, 0.1292274648535926551 ) ) ;
#10283 = CARTESIAN_POINT ( 'NONE',  ( -1.108923884514435132, -0.2845877964562159024, 0.3641732283464567677 ) ) ;
#10284 = CARTESIAN_POINT ( 'NONE',  ( 0.3346456692913393205, -0.5400638737290845981, -0.3530559997133363437 ) ) ;
#10285 = CARTESIAN_POINT ( 'NONE',  ( 1.102362204724410155, -0.1870078740157479769, 0.3641732283464567677 ) ) ;
#10286 = CARTESIAN_POINT ( 'NONE',  ( -0.3917322834645668994, -0.1049643490035306742, -1.543287770832334038 ) ) ;
#10287 = CARTESIAN_POINT ( 'NONE',  ( -1.102362204724408601, -0.1870078740157479769, 0.3641732283464567677 ) ) ;
#10288 = CARTESIAN_POINT ( 'NONE',  ( 1.528871391076116026, 0.2952755905511811885, 0.1292274648535926551 ) ) ;
#10289 = CARTESIAN_POINT ( 'NONE',  ( 2.554262525012262586, 1.537401574803149984, -0.4744094488188970171 ) ) ;
#10290 = CARTESIAN_POINT ( 'NONE',  ( -0.1968503937007867743, -0.5511811023622047445, 6.969142054262312111E-17 ) ) ;
#10291 = CARTESIAN_POINT ( 'NONE',  ( 0.01312335958005323398, 0.05413385826771666132, 0.4176697321401328100 ) ) ;
#10292 = CARTESIAN_POINT ( 'NONE',  ( -1.325459317585300889, -0.004921259842519576551, 0.3153832671262227771 ) ) ;
#10293 = CARTESIAN_POINT ( 'NONE',  ( -0.8464566929133852113, -0.5400638737290845981, -0.3530559997133363437 ) ) ;
#10294 = CARTESIAN_POINT ( 'NONE',  ( -1.397637795275589623, -0.4536011799217368745, -0.2665933059059886201 ) ) ;
#10295 = CARTESIAN_POINT ( 'NONE',  ( 0.1049643490035303967, 0.3917322834645670659, -0.4626177409786895178 ) ) ;
#10296 = EDGE_CURVE ( 'NONE', #69029, #37547, #42495, .T. ) ;
#10297 = CARTESIAN_POINT ( 'NONE',  ( 1.092353285368624860, -4.408777212815537393E-16, -0.4445507791589063395 ) ) ;
#10298 = CARTESIAN_POINT ( 'NONE',  ( 1.220472440944882386, -0.6692913385826771977, 8.415575281601705876E-17 ) ) ;
#10299 = CARTESIAN_POINT ( 'NONE',  ( 5.785732909357575061E-17, -0.4724409448818898682, -1.887795275590550936 ) ) ;
#10300 = CARTESIAN_POINT ( 'NONE',  ( -1.338582677165353729, -0.1870078740157480879, -0.4822834645669291653 ) ) ;
#10301 = CARTESIAN_POINT ( 'NONE',  ( -1.246719160104985846, -0.3690944881889765550, -0.3153832671262227771 ) ) ;
#10302 = CARTESIAN_POINT ( 'NONE',  ( -0.6167979002624665030, -0.004921259842519576551, 0.3153832671262227771 ) ) ;
#10303 = CARTESIAN_POINT ( 'NONE',  ( -3.937007874015748143, 2.755905511811024056, -0.5314960629921260393 ) ) ;
#10304 = CARTESIAN_POINT ( 'NONE',  ( 0.1312335958005257930, 0.2306618581243847221, -0.2411417322834647770 ) ) ;
#10305 = CARTESIAN_POINT ( 'NONE',  ( 0.2099737532808405305, -0.5023911411419708095, 0.1820866141732285504 ) ) ;
#10306 = CARTESIAN_POINT ( 'NONE',  ( -1.010498687664041384, -0.3690944881889765550, -0.3153832671262227771 ) ) ;
#10307 = CARTESIAN_POINT ( 'NONE',  ( -1.482939632545930975, -0.4281496062992127816, -0.4176697321401328100 ) ) ;
#10308 = CARTESIAN_POINT ( 'NONE',  ( 1.194225721784777594, -0.3690944881889765550, -0.3153832671262227771 ) ) ;
#10309 = ADVANCED_FACE ( 'NONE', ( #27240 ), #73542, .F. ) ;
#10310 = CARTESIAN_POINT ( 'NONE',  ( 1.509186351706037543, 0.05413385826771666132, 0.4176697321401328100 ) ) ;
#10311 = CARTESIAN_POINT ( 'NONE',  ( 0.3234312996134217078, 1.189126250296160592, 1.964625460076719898 ) ) ;
#10312 = CARTESIAN_POINT ( 'NONE',  ( 0.6430446194225729606, -0.3690944881889765550, -0.3153832671262227771 ) ) ;
#10313 = CARTESIAN_POINT ( 'NONE',  ( 1.095800524934383846, -0.05778040916215560624, -0.4822834645669293319 ) ) ;
#10314 = CARTESIAN_POINT ( 'NONE',  ( 1.524059884292196751E-16, 0.04488074079120461107, 1.244489337948955221 ) ) ;
#10315 = CARTESIAN_POINT ( 'NONE',  ( 0.9908136482939640111, 0.1771653543307087075, -0.09757992244046823083 ) ) ;
#10316 = VERTEX_POINT ( 'NONE', #2415 ) ;
#10317 = CARTESIAN_POINT ( 'NONE',  ( -1.292650918635170010, 0.2952755905511810774, -0.1292274648535930714 ) ) ;
#10318 = CARTESIAN_POINT ( 'NONE',  ( -0.6955380577427815458, 0.05413385826771666132, 0.4176697321401328100 ) ) ;
#10319 = CARTESIAN_POINT ( 'NONE',  ( -0.1115485564304456306, 0.2952755905511810774, -0.1292274648535930714 ) ) ;
#10320 = CIRCLE ( 'NONE', #57319, 2.637795275590551380 ) ;
#10321 = DIRECTION ( 'NONE',  ( 0.000000000000000000, 1.000000000000000000, -0.000000000000000000 ) ) ;
#10322 = CARTESIAN_POINT ( 'NONE',  ( -0.3460692066303960313, 0.1998031496062989965, -2.307742782152231165 ) ) ;
#10323 = CARTESIAN_POINT ( 'NONE',  ( 0.9973753280839902091, 0.2306618581243847221, -0.2411417322834647770 ) ) ;
#10324 = CARTESIAN_POINT ( 'NONE',  ( 1.423884514435696191, -0.08942795157527998196, 0.3641732283464567121 ) ) ;
#10325 = CONICAL_SURFACE ( 'NONE', #21064, 0.4923228346456693938, 0.7853981633974415066 ) ;
#10326 = AXIS2_PLACEMENT_3D ( 'NONE', #30091, #74314, #42716 ) ;
#10327 = CARTESIAN_POINT ( 'NONE',  ( -0.02624671916010428221, 0.2306618581243847221, -0.2411417322834647770 ) ) ;
#10328 = CARTESIAN_POINT ( 'NONE',  ( 0.8070866141732288002, 0.1660481256975885056, 0.3530559997133364547 ) ) ;
#10329 = CARTESIAN_POINT ( 'NONE',  ( -0.3996062992125987146, 0.1070741851644051862, -1.607611548556430403 ) ) ;
#10330 = CARTESIAN_POINT ( 'NONE',  ( -0.3949938075777411628, 0.1058382717557497937, -1.292650918635170676 ) ) ;
#10331 = CARTESIAN_POINT ( 'NONE',  ( -0.1070741851644051862, -0.3996062992125987146, -2.434383202099737353 ) ) ;
#10332 = CARTESIAN_POINT ( 'NONE',  ( -0.4091458600556405756, 0.2362204724409446288, -0.6561679790026246906 ) ) ;
#10333 = CARTESIAN_POINT ( 'NONE',  ( -0.3917322834645670104, -7.196005306013484475E-17, -0.03149606299212594218 ) ) ;
#10334 = CARTESIAN_POINT ( 'NONE',  ( -0.2624671916010490880, 0.1283753931104746893, -0.1820866141732285504 ) ) ;
#10335 = CARTESIAN_POINT ( 'NONE',  ( -0.6036745406824141069, 0.2306618581243848609, 0.2411417322834645549 ) ) ;
#10336 = CARTESIAN_POINT ( 'NONE',  ( 0.6692913385826777528, 0.2952755905511811885, 0.000000000000000000 ) ) ;
#10337 = CARTESIAN_POINT ( 'NONE',  ( -0.3949938075777408852, -0.1058382717557502933, -2.327427821522309870 ) ) ;
#10338 = CARTESIAN_POINT ( 'NONE',  ( -0.4527559055118102749, -0.4536011799217368745, -0.2665933059059886201 ) ) ;
#10339 =( BOUNDED_CURVE ( )  B_SPLINE_CURVE ( 2, ( #42205, #3090, #74215, #67900, #61150, #3502, #29987, #49344, #67070, #67480, #35906, #73382, #54837 ),
 .UNSPECIFIED., .F., .F. ) 
 B_SPLINE_CURVE_WITH_KNOTS ( ( 3, 2, 2, 2, 2, 2, 3 ),
 ( 0.3096947309984372509, 0.3106060606060606077, 0.3143939393939393923, 0.3181818181818181768, 0.3219696969696969613, 0.3257575757575757458, 0.3266689053651991581 ),
 .UNSPECIFIED. ) 
 CURVE ( )  GEOMETRIC_REPRESENTATION_ITEM ( )  RATIONAL_B_SPLINE_CURVE ( ( 0.9875488213027530104, 0.9918020599134685922, 1.000000000000000000, 0.9659258262890683122, 1.000000000000000000, 0.9659258262890683122, 1.000000000000000000, 0.9659258262890683122, 1.000000000000000000, 0.9659258262890683122, 1.000000000000000000, 0.9918020599134680371, 0.9875488213027523443 ) ) 
 REPRESENTATION_ITEM ( '' )  );
#10340 = CARTESIAN_POINT ( 'NONE',  ( 1.607611548556431069, 0.2952755905511811885, 0.1292274648535926551 ) ) ;
#10341 = CARTESIAN_POINT ( 'NONE',  ( 1.069553805774278610, -0.6692913385826771977, 0.1292274648535927661 ) ) ;
#10342 = CARTESIAN_POINT ( 'NONE',  ( -0.2362204724409447953, -0.4091458600556404646, -2.427821522309711266 ) ) ;
#10343 = CARTESIAN_POINT ( 'NONE',  ( 0.2925321140481932369, -0.2925321140481932369, -1.673228346456692828 ) ) ;
#10344 = DIRECTION ( 'NONE',  ( -1.000000000000000000, -0.000000000000000000, -0.000000000000000000 ) ) ;
#10345 = ORIENTED_EDGE ( 'NONE', *, *, #23671, .T. ) ;
#10346 = CARTESIAN_POINT ( 'NONE',  ( 1.089238845144357537, -0.4281496062992124485, 0.4176697321401328655 ) ) ;
#10347 = CARTESIAN_POINT ( 'NONE',  ( 1.128608923884514947, 0.1283753931104748280, 0.1820866141732283561 ) ) ;
#10349 = CARTESIAN_POINT ( 'NONE',  ( -1.515748031496062076, -0.5400638737290844871, 0.3530559997133364547 ) ) ;
#10348 = CARTESIAN_POINT ( 'NONE',  ( -1.561679790026246017, -0.3690944881889765550, -0.3153832671262227771 ) ) ;
#10350 = CARTESIAN_POINT ( 'NONE',  ( 0.3917322834645668994, -0.1049643490035303134, -2.868747088417636704 ) ) ;
#10351 = SURFACE_STYLE_USAGE ( .BOTH. , #5256 ) ;
#10352 = CARTESIAN_POINT ( 'NONE',  ( 0.6364829396325465405, -0.3162353388693409650, -0.4822834645669289433 ) ) ;
#10353 = CARTESIAN_POINT ( 'NONE',  ( -1.476377952755905110, -0.5400638737290845981, -0.3530559997133363437 ) ) ;
#10354 = CARTESIAN_POINT ( 'NONE',  ( -0.5118110236220466680, -0.6692913385826771977, 8.415575281601705876E-17 ) ) ;
#10355 = CARTESIAN_POINT ( 'NONE',  ( -0.7808398950131225646, -0.05778040916215522460, 0.4822834645669289988 ) ) ;
#10356 = CARTESIAN_POINT ( 'NONE',  ( -1.502624671916009680, -0.3162353388693405765, 0.4822834645669290543 ) ) ;
#10357 = CARTESIAN_POINT ( 'NONE',  ( -0.3917322834645669549, -0.1049643490035306603, -0.1305774278215224293 ) ) ;
#10358 = CARTESIAN_POINT ( 'NONE',  ( 0.2624671916010504757, -0.6046776061558809534, -0.2411417322834644161 ) ) ;
#10359 = CARTESIAN_POINT ( 'NONE',  ( -0.3917322834645670104, -7.196005306013484475E-17, -2.393700787401574992 ) ) ;
#10360 = CARTESIAN_POINT ( 'NONE',  ( -1.601049868766403650, 0.1283753931104746893, -0.1820866141732285504 ) ) ;
#10361 = EDGE_LOOP ( 'NONE', ( #73166, #30222 ) ) ;
#10362 = CARTESIAN_POINT ( 'NONE',  ( 0.1058382717557499880, 0.3949938075777411073, -2.828083989501312345 ) ) ;
#10363 = ORIENTED_EDGE ( 'NONE', *, *, #50107, .F. ) ;
#10364 = DIRECTION ( 'NONE',  ( 0.000000000000000000, 0.000000000000000000, -1.000000000000000000 ) ) ;
#10365 = CARTESIAN_POINT ( 'NONE',  ( -1.476377952755905110, -0.5400638737290845981, -0.3530559997133363437 ) ) ;
#10366 = CARTESIAN_POINT ( 'NONE',  ( -0.3996062992125986035, -7.340648628747425578E-17, -0.9842519685039369248 ) ) ;
#10367 = CARTESIAN_POINT ( 'NONE',  ( 0.5611900217179910388, 1.223219560026271499E-15, 0.4445507791589056734 ) ) ;
#10368 = CARTESIAN_POINT ( 'NONE',  ( -0.1377952755905504645, 0.1012011053420777407, 0.2882089793578257453 ) ) ;
#10369 = CARTESIAN_POINT ( 'NONE',  ( 2.795275590551181466, 2.244094488188977277, 0.000000000000000000 ) ) ;
#10370 = CARTESIAN_POINT ( 'NONE',  ( 0.002049465651556450167, -0.3981765293560898256, -2.755905511811024056 ) ) ;
#10371 = CARTESIAN_POINT ( 'NONE',  ( -9.594673741351313045E-17, 0.3917322834645670104, -0.2421259842519686289 ) ) ;
#10372 = CARTESIAN_POINT ( 'NONE',  ( -0.4199475065616791736, -0.5023911411419708095, 0.1820866141732285504 ) ) ;
#10373 = ADVANCED_FACE ( 'NONE', ( #66812 ), #14290, .F. ) ;
#10374 = CARTESIAN_POINT ( 'NONE',  ( -1.161417322834644716, -0.4536011799217368745, -0.2665933059059886201 ) ) ;
#10375 = CARTESIAN_POINT ( 'NONE',  ( -1.555118110236219930, -0.5400638737290845981, -0.3530559997133363437 ) ) ;
#10376 = CARTESIAN_POINT ( 'NONE',  ( 0.3280839895013130669, 0.05413385826771666132, 0.4176697321401328100 ) ) ;
#10377 = CARTESIAN_POINT ( 'NONE',  ( -1.496062992125983815, -0.1870078740157479769, 0.4822834645669291653 ) ) ;
#10378 = CARTESIAN_POINT ( 'NONE',  ( 0.1958661417322836440, -0.3392501089628017219, -0.2414698162729658204 ) ) ;
#10379 = ORIENTED_EDGE ( 'NONE', *, *, #3797, .T. ) ;
#10380 = CARTESIAN_POINT ( 'NONE',  ( -1.253280839895012377, -0.3162353388693409650, -0.4822834645669289433 ) ) ;
#10381 = CARTESIAN_POINT ( 'NONE',  ( 0.000000000000000000, 0.4374015748031496176, 0.000000000000000000 ) ) ;
#10382 = LENGTH_MEASURE_WITH_UNIT ( LENGTH_MEASURE( 0.02539999999999999897 ), #9956 );
#10383 = AXIS2_PLACEMENT_3D ( 'NONE', #16024, #14780, #66116 ) ;
#10384 = CARTESIAN_POINT ( 'NONE',  ( -0.1265901696524993347, 0.4724409448818895907, -1.738845144356955696 ) ) ;
#10385 = CARTESIAN_POINT ( 'NONE',  ( 2.112655059233934818, 1.697151583350148263, 0.4469586986359062042 ) ) ;
#10386 = CIRCLE ( 'NONE', #29169, 1.220472440944881942 ) ;
#10387 = LINE ( 'NONE', #36044, #22396 ) ;
#10388 = CARTESIAN_POINT ( 'NONE',  ( -0.7349081364829387342, -0.6046776061558807314, 0.2411417322834647770 ) ) ;
#10389 = CARTESIAN_POINT ( 'NONE',  ( 1.345144356955381593, -0.05778040916215522460, 0.4822834645669289988 ) ) ;
#10390 = AXIS2_PLACEMENT_3D ( 'NONE', #26498, #71956, #71534 ) ;
#10392 = CARTESIAN_POINT ( 'NONE',  ( -0.4417575354491581896, 1.710976477253047801, 2.620897244026389572 ) ) ;
#10391 = CARTESIAN_POINT ( 'NONE',  ( -2.787279214012418738, 0.000000000000000000, 0.000000000000000000 ) ) ;
#10393 = CARTESIAN_POINT ( 'NONE',  ( -1.646981627296586703, -0.3162353388693409650, -0.4822834645669289433 ) ) ;
#10394 = CARTESIAN_POINT ( 'NONE',  ( -0.9580052493438311334, -0.4281496062992124485, 0.4176697321401328655 ) ) ;
#10395 = CARTESIAN_POINT ( 'NONE',  ( -0.1958661417322836440, 0.3392501089628016664, -0.09315653723653360974 ) ) ;
#10396 = CARTESIAN_POINT ( 'NONE',  ( 5.463695987328526437E-16, -0.1870078740157479769, 0.3641732283464567677 ) ) ;
#10397 = CARTESIAN_POINT ( 'NONE',  ( -0.2867679344610366554, 0.2867679344610365444, -0.5767716535433071723 ) ) ;
#10398 = CARTESIAN_POINT ( 'NONE',  ( 0.05249343832021075018, -0.5023911411419708095, 0.1820866141732285504 ) ) ;
#10399 = CARTESIAN_POINT ( 'NONE',  ( 0.7414698162729663755, -0.5511811023622048555, -0.09757992244046775898 ) ) ;
#10400 = CARTESIAN_POINT ( 'NONE',  ( 0.4068241469816279987, -0.4281496062992127816, -0.4176697321401328100 ) ) ;
#10401 = CARTESIAN_POINT ( 'NONE',  ( -0.3083989501312330295, -0.2845877964562161244, -0.3641732283464567121 ) ) ;
#10402 = CARTESIAN_POINT ( 'NONE',  ( 0.3392501089628018884, -0.1958661417322834220, -2.301837270341207553 ) ) ;
#10403 = CARTESIAN_POINT ( 'NONE',  ( 1.541994750656168645, -0.6692913385826771977, 0.1292274648535927661 ) ) ;
#10404 = CARTESIAN_POINT ( 'NONE',  ( -0.9973753280839886548, 0.2306618581243848609, 0.2411417322834645549 ) ) ;
#10405 = CARTESIAN_POINT ( 'NONE',  ( -0.4724409448818899238, 0.1265901696524986686, -0.8969816272965877024 ) ) ;
#10406 = CARTESIAN_POINT ( 'NONE',  ( 0.07217847769028949700, -0.05778040916215560624, -0.4822834645669293319 ) ) ;
#10407 = CARTESIAN_POINT ( 'NONE',  ( -0.5249343832020990641, 0.2306618581243848609, 0.2411417322834645549 ) ) ;
#10408 = CARTESIAN_POINT ( 'NONE',  ( 1.627296587926509996, -0.5023911411419708095, 0.1820866141732285504 ) ) ;
#10409 = CARTESIAN_POINT ( 'NONE',  ( -0.02624671916010428221, -0.5023911411419708095, 0.1820866141732285504 ) ) ;
#10410 = CARTESIAN_POINT ( 'NONE',  ( -0.09186351706036689768, 0.05413385826771626580, -0.4176697321401330321 ) ) ;
#10411 = CARTESIAN_POINT ( 'NONE',  ( -0.8070866141732276899, 0.1660481256975883668, -0.3530559997133364547 ) ) ;
#10412 = CARTESIAN_POINT ( 'NONE',  ( 1.586052503253845281, 0.7480314960629931287, -0.1653254495020588799 ) ) ;
#10413 = CARTESIAN_POINT ( 'NONE',  ( 0.4724409448818898682, 2.892866454678787531E-17, -0.2755905511811023723 ) ) ;
#10414 = CARTESIAN_POINT ( 'NONE',  ( 0.2493438320209980519, 0.05413385826771666132, 0.4176697321401328100 ) ) ;
#10415 = ORIENTED_EDGE ( 'NONE', *, *, #16161, .T. ) ;
#10416 = CARTESIAN_POINT ( 'NONE',  ( -0.1998031496062991630, -0.3460692066303959202, -2.189632545931758489 ) ) ;
#10417 = CARTESIAN_POINT ( 'NONE',  ( 1.423884514435696191, -0.05778040916215522460, 0.4822834645669289988 ) ) ;
#10418 = CARTESIAN_POINT ( 'NONE',  ( -0.4724409448818890911, -0.1870078740157479769, 0.3641732283464567677 ) ) ;
#10419 = CARTESIAN_POINT ( 'NONE',  ( -0.7217847769028863381, 0.05413385826771626580, -0.4176697321401330321 ) ) ;
#10420 = CARTESIAN_POINT ( 'NONE',  ( 1.463254593175853824, -0.6692913385826771977, 0.1292274648535927661 ) ) ;
#10421 = CARTESIAN_POINT ( 'NONE',  ( 1.528871391076116026, 0.2952755905511811885, 0.1292274648535926551 ) ) ;
#10422 = CARTESIAN_POINT ( 'NONE',  ( -1.581364829396324945, -0.05778040916215560624, -0.4822834645669293319 ) ) ;
#10423 = CARTESIAN_POINT ( 'NONE',  ( -0.8923884514435688198, 0.1283753931104746893, -0.1820866141732285504 ) ) ;
#10424 = CARTESIAN_POINT ( 'NONE',  ( 0.1070741851644053527, 0.3996062992125985480, -0.2276902887139107545 ) ) ;
#10425 = CARTESIAN_POINT ( 'NONE',  ( 0.3460692066303959202, 0.1998031496062993295, -0.6036745406824146620 ) ) ;
#10426 = CARTESIAN_POINT ( 'NONE',  ( 0.1049643490035304799, -0.3917322834645670104, -2.916685982448506298 ) ) ;
#10427 = CARTESIAN_POINT ( 'NONE',  ( 1.686351706036745890, 0.1771653543307087630, 0.09757992244046791164 ) ) ;
#10428 = EDGE_CURVE ( 'NONE', #50308, #75749, #17721, .T. ) ;
#10429 = CARTESIAN_POINT ( 'NONE',  ( 1.207349081364829990, -0.5023911411419708095, -0.1820866141732282451 ) ) ;
#10430 = CARTESIAN_POINT ( 'NONE',  ( 0.8398950131233602345, 0.2306618581243847221, -0.2411417322834647770 ) ) ;
#10431 = CARTESIAN_POINT ( 'NONE',  ( -1.653543307086613234, -0.1870078740157480879, -0.4822834645669291653 ) ) ;
#10432 = CARTESIAN_POINT ( 'NONE',  ( 0.9383202099737536495, -0.3162353388693405765, 0.4822834645669290543 ) ) ;
#10433 = CARTESIAN_POINT ( 'NONE',  ( 0.3949938075777409408, -0.1058382717557499186, -0.8182414698162731037 ) ) ;
#10434 = CARTESIAN_POINT ( 'NONE',  ( 1.364829396325460076, 0.1283753931104748280, 0.1820866141732283561 ) ) ;
#10435 = CARTESIAN_POINT ( 'NONE',  ( 0.1377952755905518800, 0.1660481256975883668, -0.3530559997133364547 ) ) ;
#10436 = CARTESIAN_POINT ( 'NONE',  ( -1.023622047244093558, -0.1870078740157479769, 0.4822834645669291653 ) ) ;
#10437 = CARTESIAN_POINT ( 'NONE',  ( 1.338582677165355062, -0.1870078740157479769, 0.4822834645669291653 ) ) ;
#10438 = CARTESIAN_POINT ( 'NONE',  ( 0.1265901696524990294, -0.4724409448818896462, -1.187664041994750619 ) ) ;
#10439 = AXIS2_PLACEMENT_3D ( 'NONE', #61565, #5958, #45913 ) ;
#10440 = CARTESIAN_POINT ( 'NONE',  ( -0.3460692066303958092, -0.1998031496062994683, -2.257217847769029007 ) ) ;
#10441 = CARTESIAN_POINT ( 'NONE',  ( 0.5249343832021003964, 0.1283753931104746893, -0.1820866141732285504 ) ) ;
#10442 = EDGE_LOOP ( 'NONE', ( #23462, #62611, #68519, #46459 ) ) ;
#10443 = CARTESIAN_POINT ( 'NONE',  ( 0.1049643490035303967, 0.3917322834645670659, -0.9350586858605794971 ) ) ;
#10444 = VERTEX_POINT ( 'NONE', #73112 ) ;
#10445 = CARTESIAN_POINT ( 'NONE',  ( -0.8792650918635160906, 0.05413385826771626580, -0.4176697321401330321 ) ) ;
#10446 = CARTESIAN_POINT ( 'NONE',  ( -0.1377952755905504645, -0.5400638737290845981, -0.3530559997133363437 ) ) ;
#10447 = CARTESIAN_POINT ( 'NONE',  ( -0.1509186351706028884, -0.3162353388693409650, -0.4822834645669289433 ) ) ;
#10448 = CARTESIAN_POINT ( 'NONE',  ( 0.8464566929133866546, -0.5400638737290844871, 0.3530559997133364547 ) ) ;
#10449 = CARTESIAN_POINT ( 'NONE',  ( -1.187664041994749731, -0.3162353388693405765, 0.4822834645669290543 ) ) ;
#10450 = CARTESIAN_POINT ( 'NONE',  ( -0.5577427821522301654, -0.05778040916215560624, -0.4822834645669293319 ) ) ;
#10451 = CARTESIAN_POINT ( 'NONE',  ( 0.5971128608923890191, -0.6692913385826771977, 0.1292274648535927661 ) ) ;
#10452 = ADVANCED_FACE ( 'NONE', ( #79032 ), #78612, .F. ) ;
#10453 = CARTESIAN_POINT ( 'NONE',  ( 0.6889763779527563470, 0.1660481256975883668, -0.3530559997133364547 ) ) ;
#10454 = CARTESIAN_POINT ( 'NONE',  ( 0.9120734908136490793, 0.2952755905511810774, -0.1292274648535930714 ) ) ;
#10455 = EDGE_CURVE ( 'NONE', #4549, #3211, #20935, .T. ) ;
#10456 = CARTESIAN_POINT ( 'NONE',  ( -0.1049643490035302024, -0.3917322834645671215, -1.166666666666666519 ) ) ;
#10457 = CARTESIAN_POINT ( 'NONE',  ( -0.6102362204724400829, -0.4536011799217368745, -0.2665933059059886201 ) ) ;
#10458 = EDGE_LOOP ( 'NONE', ( #13975, #70018, #81969, #35058 ) ) ;
#10459 = CARTESIAN_POINT ( 'NONE',  ( -0.3949938075777409408, -0.1058382717557502933, -1.463254593175853158 ) ) ;
#10460 = ORIENTED_EDGE ( 'NONE', *, *, #32216, .F. ) ;
#10461 = CARTESIAN_POINT ( 'NONE',  ( -0.9580052493438311334, -0.3690944881889763329, 0.3153832671262228327 ) ) ;
#10462 = CARTESIAN_POINT ( 'NONE',  ( -0.3543307086614165824, 0.2952755905511811885, 0.000000000000000000 ) ) ;
#10463 = CARTESIAN_POINT ( 'NONE',  ( -0.2925321140481930704, -0.2925321140481933480, 0.09842519685039367860 ) ) ;
#10464 = CARTESIAN_POINT ( 'NONE',  ( -0.7808398950131225646, -0.05778040916215522460, 0.4822834645669289988 ) ) ;
#10465 = CARTESIAN_POINT ( 'NONE',  ( -0.8136482939632537770, -0.6046776061558807314, 0.2411417322834647770 ) ) ;
#10466 = CARTESIAN_POINT ( 'NONE',  ( -1.384514435695537005, -0.6692913385826773087, -0.1292274648535924053 ) ) ;
#10467 = CARTESIAN_POINT ( 'NONE',  ( -1.496062992125983815, -0.1870078740157480879, -0.4822834645669291653 ) ) ;
#10468 = CARTESIAN_POINT ( 'NONE',  ( 0.9514435695538062676, -0.2845877964562161244, -0.3641732283464567121 ) ) ;
#10469 = CARTESIAN_POINT ( 'NONE',  ( 1.193521905106662784, 3.421639014772782816E-16, 0.3464511005275203726 ) ) ;
#10470 = CARTESIAN_POINT ( 'NONE',  ( 0.3273801728231982566, 0.000000000000000000, 0.3464511005275205946 ) ) ;
#10471 = CARTESIAN_POINT ( 'NONE',  ( 0.1837270341207354329, 0.1283753931104748280, 0.1820866141732283561 ) ) ;
#10472 = CARTESIAN_POINT ( 'NONE',  ( 0.1509186351706045259, -0.05778040916215560624, -0.4822834645669293319 ) ) ;
#10473 = CARTESIAN_POINT ( 'NONE',  ( -0.2559055118110227234, -0.5400638737290844871, 0.3530559997133364547 ) ) ;
#10474 = ORIENTED_EDGE ( 'NONE', *, *, #61021, .F. ) ;
#10475 = CARTESIAN_POINT ( 'NONE',  ( -0.2925321140481930704, -0.2925321140481933480, -1.791338582677165059 ) ) ;
#10476 = FACE_OUTER_BOUND ( 'NONE', #13157, .T. ) ;
#10477 = ORIENTED_EDGE ( 'NONE', *, *, #54568, .T. ) ;
#10478 = CARTESIAN_POINT ( 'NONE',  ( -0.1998031496062994405, 0.3460692066303957537, -1.664698162729658426 ) ) ;
#10479 = CARTESIAN_POINT ( 'NONE',  ( 1.541994750656168645, -0.6692913385826771977, 0.1292274648535927661 ) ) ;
#10480 = CARTESIAN_POINT ( 'NONE',  ( -0.7086614173228339419, -0.1870078740157480601, -0.3641732283464567677 ) ) ;
#10481 = CARTESIAN_POINT ( 'NONE',  ( -1.108923884514435132, -0.3162353388693405765, 0.4822834645669290543 ) ) ;
#10482 = CARTESIAN_POINT ( 'NONE',  ( -0.4724409448818895907, -0.1265901696524993070, -0.5183727034120735322 ) ) ;
#10483 = CARTESIAN_POINT ( 'NONE',  ( -0.01548373826924297550, 1.062992125984252079, 3.937007874015748143 ) ) ;
#10484 = CARTESIAN_POINT ( 'NONE',  ( -0.3392501089628019995, 0.1958661417322832277, -2.630577427821522374 ) ) ;
#10485 = CARTESIAN_POINT ( 'NONE',  ( 1.240157480314961314, 0.1660481256975883668, -0.3530559997133364547 ) ) ;
#10486 = CARTESIAN_POINT ( 'NONE',  ( 0.5774278215223103139, -0.6046776061558809534, -0.2411417322834644161 ) ) ;
#10487 = CARTESIAN_POINT ( 'NONE',  ( 0.5577427821522316087, -0.05778040916215522460, 0.4822834645669289988 ) ) ;
#10488 = CARTESIAN_POINT ( 'NONE',  ( -0.7086614173228339419, -0.1870078740157479769, 0.3641732283464567677 ) ) ;
#10489 = CARTESIAN_POINT ( 'NONE',  ( -0.09842519685039295696, 0.1660481256975883668, -0.3530559997133364547 ) ) ;
#10490 = CARTESIAN_POINT ( 'NONE',  ( -0.4091458600556402980, -0.2362204724409451284, -2.333989501312335957 ) ) ;
#10491 = CARTESIAN_POINT ( 'NONE',  ( -0.4199475065616791736, 0.2306618581243847221, -0.2411417322834647770 ) ) ;
#10492 = CARTESIAN_POINT ( 'NONE',  ( -9.674558042662122972E-17, 0.3949938075777409963, -1.966535433070866423 ) ) ;
#10493 = CARTESIAN_POINT ( 'NONE',  ( 1.384514435695538337, -0.5511811023622046335, 0.09757992244046803654 ) ) ;
#10494 = CARTESIAN_POINT ( 'NONE',  ( -0.4002624671916004129, -0.08942795157528024563, -0.3641732283464568787 ) ) ;
#10495 = CARTESIAN_POINT ( 'NONE',  ( 0.9645669291338591078, -0.4536011799217368745, -0.2665933059059886201 ) ) ;
#10496 = CARTESIAN_POINT ( 'NONE',  ( -1.286089238845143479, -0.6046776061558807314, 0.2411417322834647770 ) ) ;
#10497 = CARTESIAN_POINT ( 'NONE',  ( -1.148293963254592542, 0.1771653543307087630, 0.09757992244046791164 ) ) ;
#10498 = CARTESIAN_POINT ( 'NONE',  ( 0.4724409448818915891, -0.1265901696524958653, -2.235564304461942875 ) ) ;
#10499 = CARTESIAN_POINT ( 'NONE',  ( -1.141732283464566011, -0.6692913385826771977, 8.415575281601705876E-17 ) ) ;
#10500 = CARTESIAN_POINT ( 'NONE',  ( -0.6364829396325453192, -0.05778040916215560624, -0.4822834645669293319 ) ) ;
#10501 = CARTESIAN_POINT ( 'NONE',  ( 0.4330708661417329575, 0.2952755905511811885, 0.000000000000000000 ) ) ;
#10502 = CARTESIAN_POINT ( 'NONE',  ( -0.3392501089628018329, -0.1958661417322836440, -2.337251025425510331 ) ) ;
#10503 = CARTESIAN_POINT ( 'NONE',  ( 1.092023077763014882, -8.904001037647063530E-16, -0.4281989832122458095 ) ) ;
#10504 = CARTESIAN_POINT ( 'NONE',  ( 0.5380577427821529035, -0.3690944881889763329, 0.3153832671262228327 ) ) ;
#10505 = CARTESIAN_POINT ( 'NONE',  ( -1.463254593175852492, -0.5511811023622048555, -0.09757992244046775898 ) ) ;
#10506 = CARTESIAN_POINT ( 'NONE',  ( 0.7611548556430454138, 0.2306618581243847221, -0.2411417322834647770 ) ) ;
#10507 = CARTESIAN_POINT ( 'NONE',  ( -1.509186351706035767, -0.004921259842519870586, -0.3153832671262229437 ) ) ;
#10508 = CARTESIAN_POINT ( 'NONE',  ( 1.253280839895013710, -0.2845877964562159024, 0.3641732283464567677 ) ) ;
#10509 = CARTESIAN_POINT ( 'NONE',  ( -0.8136482939632537770, -0.6046776061558807314, 0.2411417322834647770 ) ) ;
#10510 = CARTESIAN_POINT ( 'NONE',  ( -0.4593175853018364174, -0.3690944881889765550, -0.3153832671262227771 ) ) ;
#10511 = DIRECTION ( 'NONE',  ( 1.000000000000000000, 1.387778780781445676E-15, 0.000000000000000000 ) ) ;
#10512 = CARTESIAN_POINT ( 'NONE',  ( 0.6889763779527563470, 0.07958543189024071263, -0.2665933059059888421 ) ) ;
#10513 = EDGE_CURVE ( 'NONE', #47374, #79188, #54319, .T. ) ;
#10514 = CARTESIAN_POINT ( 'NONE',  ( -0.2493438320209966919, -0.4281496062992124485, 0.4176697321401328655 ) ) ;
#10515 = CARTESIAN_POINT ( 'NONE',  ( 0.2925321140481932369, 0.2925321140481932369, -0.8444881889763780070 ) ) ;
#10516 = CARTESIAN_POINT ( 'NONE',  ( -0.1958661417322836718, 0.3392501089628017219, -1.830052493438320216 ) ) ;
#10517 = CARTESIAN_POINT ( 'NONE',  ( 0.5249343832021003964, 0.1283753931104746893, -0.1820866141732285504 ) ) ;
#10518 = CARTESIAN_POINT ( 'NONE',  ( 0.2296587926509192634, -0.3162353388693405765, 0.4822834645669290543 ) ) ;
#10519 = CARTESIAN_POINT ( 'NONE',  ( -0.1443569553805765515, -0.4281496062992127816, -0.4176697321401328100 ) ) ;
#10520 = CARTESIAN_POINT ( 'NONE',  ( -0.5577427821522301654, -0.2845877964562159024, 0.3641732283464567677 ) ) ;
#10521 = FACE_BOUND ( 'NONE', #76585, .T. ) ;
#10522 = CARTESIAN_POINT ( 'NONE',  ( -0.4724409448818890911, -0.1870078740157480601, -0.3641732283464567677 ) ) ;
#10523 = CARTESIAN_POINT ( 'NONE',  ( 0.5380577427821529035, -0.4281496062992124485, 0.4176697321401328655 ) ) ;
#10524 = CARTESIAN_POINT ( 'NONE',  ( -0.9580052493438311334, -0.3690944881889763329, 0.3153832671262228327 ) ) ;
#10525 = CARTESIAN_POINT ( 'NONE',  ( -0.1998031496062991630, -0.3460692066303959202, -1.402230971128609172 ) ) ;
#10526 = CARTESIAN_POINT ( 'NONE',  ( -1.364829396325458521, -0.6046776061558807314, 0.2411417322834647770 ) ) ;
#10527 = DIRECTION ( 'NONE',  ( 0.000000000000000000, 0.000000000000000000, -1.000000000000000000 ) ) ;
#10528 = ORIENTED_EDGE ( 'NONE', *, *, #10513, .T. ) ;
#10529 = CARTESIAN_POINT ( 'NONE',  ( -1.496062992125983815, -0.1870078740157480601, -0.3641732283464567677 ) ) ;
#10530 = CARTESIAN_POINT ( 'NONE',  ( -0.5971128608923877978, 0.2952755905511811885, 0.1292274648535926551 ) ) ;
#10531 = CARTESIAN_POINT ( 'NONE',  ( -1.135170603674539924, 0.2952755905511810774, -0.1292274648535930714 ) ) ;
#10532 = CARTESIAN_POINT ( 'NONE',  ( -0.1049643490035307020, 0.3917322834645669549, -1.666010498687664043 ) ) ;
#10533 = CARTESIAN_POINT ( 'NONE',  ( -0.4724409448818898682, -8.678599364036362592E-17, -2.086614173228346303 ) ) ;
#10534 = CARTESIAN_POINT ( 'NONE',  ( 1.568241469816273659, -0.05778040916215560624, -0.4822834645669293319 ) ) ;
#10535 = CARTESIAN_POINT ( 'NONE',  ( 0.2493438320209980519, 0.05413385826771666132, 0.4176697321401328100 ) ) ;
#10536 = CARTESIAN_POINT ( 'NONE',  ( 0.000000000000000000, 0.000000000000000000, 0.000000000000000000 ) ) ;
#10537 = CARTESIAN_POINT ( 'NONE',  ( 0.3460692066303959202, -0.1998031496062991630, -2.386482939632545985 ) ) ;
#10538 = CARTESIAN_POINT ( 'NONE',  ( 1.496062992125984703, -0.1870078740157480601, -0.3641732283464567677 ) ) ;
#10539 = CARTESIAN_POINT ( 'NONE',  ( 0.1998031496062994405, -0.3460692066303958092, -0.8792650918635170898 ) ) ;
#10540 = ORIENTED_EDGE ( 'NONE', *, *, #61360, .F. ) ;
#10541 = CARTESIAN_POINT ( 'NONE',  ( -0.9973753280839886548, 0.1283753931104748280, 0.1820866141732283561 ) ) ;
#10542 = CARTESIAN_POINT ( 'NONE',  ( 0.1958661417322834775, 0.3392501089628018884, -2.498687664041994605 ) ) ;
#10543 = EDGE_LOOP ( 'NONE', ( #46039, #64264, #80035, #68202 ) ) ;
#10544 = CARTESIAN_POINT ( 'NONE',  ( 0.3477690288713918276, 0.2952755905511811885, 0.1292274648535926551 ) ) ;
#10545 = CARTESIAN_POINT ( 'NONE',  ( -0.4593175853018366950, 0.05413385826771666132, 0.4176697321401328100 ) ) ;
#10546 = CARTESIAN_POINT ( 'NONE',  ( -1.194225721784776262, -0.4281496062992124485, 0.4176697321401328655 ) ) ;
#10547 = CARTESIAN_POINT ( 'NONE',  ( 0.9448818897637802916, -0.1870078740157480879, -0.4822834645669291653 ) ) ;
#10548 = CARTESIAN_POINT ( 'NONE',  ( -1.167979002624671470, -0.004921259842519576551, 0.3153832671262227771 ) ) ;
#10549 = CARTESIAN_POINT ( 'NONE',  ( 0.08943933388982898414, 7.699586553780600482E-16, 0.4118484887281971263 ) ) ;
#10550 = CARTESIAN_POINT ( 'NONE',  ( 0.1443569553805781891, 0.05413385826771626580, -0.4176697321401330321 ) ) ;
#10551 = CARTESIAN_POINT ( 'NONE',  ( -0.9580052493438311334, 0.05413385826771626580, -0.4176697321401330321 ) ) ;
#10552 = CARTESIAN_POINT ( 'NONE',  ( 0.3917322834645668994, -0.1049643490035303134, -1.608904568732596685 ) ) ;
#10553 = CARTESIAN_POINT ( 'NONE',  ( 0.000000000000000000, 0.000000000000000000, 6.062992125984251857 ) ) ;
#10554 = FACE_OUTER_BOUND ( 'NONE', #25320, .T. ) ;
#10555 = CARTESIAN_POINT ( 'NONE',  ( 0.3917322834645670104, -0.1049643490035303411, -2.715879265091863726 ) ) ;
#10556 = CARTESIAN_POINT ( 'NONE',  ( 0.8070866141732289112, -0.4536011799217368745, -0.2665933059059886201 ) ) ;
#10557 = VERTEX_POINT ( 'NONE', #54147 ) ;
#10558 = CARTESIAN_POINT ( 'NONE',  ( -0.3917322834645670104, -0.1049643490035307020, -2.877315903708348444 ) ) ;
#10559 = CARTESIAN_POINT ( 'NONE',  ( -0.2952755905511803003, -0.5400638737290845981, -0.3530559997133363437 ) ) ;
#10560 = VERTEX_POINT ( 'NONE', #46594 ) ;
#10561 = CARTESIAN_POINT ( 'NONE',  ( 0.5774278215223103139, -0.5023911411419708095, -0.1820866141732282451 ) ) ;
#10562 = CARTESIAN_POINT ( 'NONE',  ( -1.712598425196849572, 0.1660481256975885056, 0.3530559997133364547 ) ) ;
#10563 = CARTESIAN_POINT ( 'NONE',  ( 0.6167979002624678353, -0.4281496062992124485, 0.4176697321401328655 ) ) ;
#10564 = CARTESIAN_POINT ( 'NONE',  ( 0.2887139107611556010, -0.6046776061558807314, 0.2411417322834647770 ) ) ;
#10565 = CARTESIAN_POINT ( 'NONE',  ( -0.1509186351706028884, -0.05778040916215522460, 0.4822834645669289988 ) ) ;
#10566 = CARTESIAN_POINT ( 'NONE',  ( 0.1958661417322836718, -0.3392501089628017219, -1.190964197671602998 ) ) ;
#10567 = CARTESIAN_POINT ( 'NONE',  ( -0.9645669291338575535, 0.1660481256975883668, -0.3530559997133364547 ) ) ;
#10568 = EDGE_CURVE ( 'NONE', #49988, #76797, #52483, .T. ) ;
#10569 = CARTESIAN_POINT ( 'NONE',  ( 0.3917322834645670104, 2.398668435337828261E-17, -2.250000000000000000 ) ) ;
#10570 = CARTESIAN_POINT ( 'NONE',  ( 1.568241469816273437, -0.2845877964562159024, 0.3641732283464567677 ) ) ;
#10571 = CARTESIAN_POINT ( 'NONE',  ( -0.8858267716535425107, -0.5400638737290844871, 0.3530559997133364547 ) ) ;
#10572 = CARTESIAN_POINT ( 'NONE',  ( 1.509186351706037543, 0.05413385826771666132, 0.4176697321401328100 ) ) ;
#10573 = CARTESIAN_POINT ( 'NONE',  ( 1.135170603674541256, -0.6692913385826773087, -0.1292274648535924053 ) ) ;
#10574 = CARTESIAN_POINT ( 'NONE',  ( -0.3460692066303958092, -0.1998031496062994683, -0.3674540682414698112 ) ) ;
#10575 = CARTESIAN_POINT ( 'NONE',  ( -0.9251968503937002541, 0.1660481256975885056, 0.3530559997133364547 ) ) ;
#10576 = CARTESIAN_POINT ( 'NONE',  ( -0.1070741851644051862, -0.3996062992125986590, 0.1660104986876640432 ) ) ;
#10577 = CARTESIAN_POINT ( 'NONE',  ( 0.08530183727034192087, -0.3162353388693409650, -0.4822834645669289433 ) ) ;
#10578 = CARTESIAN_POINT ( 'NONE',  ( -0.1070741851644051862, -0.3996062992125987146, -2.276902887139107268 ) ) ;
#10579 = CARTESIAN_POINT ( 'NONE',  ( -0.6692913385826764205, 0.2952755905511811885, 0.000000000000000000 ) ) ;
#10580 = CARTESIAN_POINT ( 'NONE',  ( 1.679790026246720025, 0.2306618581243848609, 0.2411417322834645549 ) ) ;
#10581 = CARTESIAN_POINT ( 'NONE',  ( 0.5577427821522316087, -0.08942795157527998196, 0.3641732283464567121 ) ) ;
#10582 = CARTESIAN_POINT ( 'NONE',  ( 1.286089238845145033, 0.2306618581243848609, 0.2411417322834645549 ) ) ;
#10583 = CARTESIAN_POINT ( 'NONE',  ( 0.4091458600556404646, -0.2362204724409448231, -0.9691601049868766582 ) ) ;
#10584 = CARTESIAN_POINT ( 'NONE',  ( 0.5577427821522316087, -0.08942795157527998196, 0.3641732283464567121 ) ) ;
#10585 = EDGE_CURVE ( 'NONE', #55865, #40881, #20698, .T. ) ;
#10586 = CARTESIAN_POINT ( 'NONE',  ( 0.6692913385826777528, 0.2952755905511811885, 0.000000000000000000 ) ) ;
#10587 = CARTESIAN_POINT ( 'NONE',  ( 0.1974969037888704704, 0.3420746716998660508, -0.3786089238845145033 ) ) ;
#10588 = CARTESIAN_POINT ( 'NONE',  ( -0.6758530183727028406, -0.6692913385826773087, -0.1292274648535924053 ) ) ;
#10589 = DIRECTION ( 'NONE',  ( 0.000000000000000000, -1.000000000000000000, 0.000000000000000000 ) ) ;
#10590 = CARTESIAN_POINT ( 'NONE',  ( 1.391076115485564868, -0.5023911411419708095, 0.1820866141732285504 ) ) ;
#10591 = CARTESIAN_POINT ( 'NONE',  ( -0.7349081364829390672, 0.2306618581243847221, -0.2411417322834647770 ) ) ;
#10592 = EDGE_CURVE ( 'NONE', #83014, #54436, #23653, .T. ) ;
#10593 = CARTESIAN_POINT ( 'NONE',  ( 0.2165354330708668673, 0.1660481256975883668, -0.3530559997133364547 ) ) ;
#10594 = CARTESIAN_POINT ( 'NONE',  ( 0.1115485564304470045, 0.2066929133858267931, 0.1054918080437490802 ) ) ;
#10595 = CARTESIAN_POINT ( 'NONE',  ( 0.07874015748031558404, -0.1870078740157480879, -0.4822834645669291653 ) ) ;
#10596 = CARTESIAN_POINT ( 'NONE',  ( -0.03280839895013062252, 0.1771653543307087075, -0.09757992244046823083 ) ) ;
#10597 = CARTESIAN_POINT ( 'NONE',  ( -2.784923006909794996, 1.160811571118585572, 0.2889173282905625473 ) ) ;
#10598 = CARTESIAN_POINT ( 'NONE',  ( 0.006561679790026889343, -0.2845877964562161244, -0.3641732283464567121 ) ) ;
#10599 = CARTESIAN_POINT ( 'NONE',  ( 0.5905511811023629321, -0.5511811023622047445, 6.969142054262312111E-17 ) ) ;
#10600 = LINE ( 'NONE', #37073, #16191 ) ;
#10601 = CARTESIAN_POINT ( 'NONE',  ( 0.1998031496062994128, -0.3460692066303957537, -1.585958005249344049 ) ) ;
#10602 = CARTESIAN_POINT ( 'NONE',  ( 0.5249343832021005074, -0.6046776061558807314, 0.2411417322834647770 ) ) ;
#10603 = CARTESIAN_POINT ( 'NONE',  ( -9.594673741351313045E-17, 0.3917322834645670104, -1.251968503937008093 ) ) ;
#10604 = CARTESIAN_POINT ( 'NONE',  ( 0.2251228153049674996, -4.135162568743707313E-16, -0.3954985857520057491 ) ) ;
#10605 = CARTESIAN_POINT ( 'NONE',  ( 0.1474713956048451791, 8.471767977567108961E-16, -0.4445507791589058955 ) ) ;
#10606 = CARTESIAN_POINT ( 'NONE',  ( -0.6036745406824141069, 0.1283753931104748280, 0.1820866141732283561 ) ) ;
#10607 = CARTESIAN_POINT ( 'NONE',  ( 0.3018372703412079971, 0.05413385826771626580, -0.4176697321401330321 ) ) ;
#10608 = CARTESIAN_POINT ( 'NONE',  ( 0.8333333333333340365, -0.5511811023622046335, 0.09757992244046803654 ) ) ;
#10609 = CARTESIAN_POINT ( 'NONE',  ( -1.456692913385826182, -0.5511811023622047445, 6.969142054262312111E-17 ) ) ;
#10610 = CARTESIAN_POINT ( 'NONE',  ( -1.614173228346456268, -0.6692913385826771977, 8.415575281601705876E-17 ) ) ;
#10611 = CARTESIAN_POINT ( 'NONE',  ( 0.1312335958005257930, 0.2306618581243847221, -0.2411417322834647770 ) ) ;
#10612 = EDGE_CURVE ( 'NONE', #35624, #2570, #16294, .T. ) ;
#10613 = CARTESIAN_POINT ( 'NONE',  ( 1.213910761154856299, 0.2952755905511811885, 0.1292274648535926551 ) ) ;
#10614 = CARTESIAN_POINT ( 'NONE',  ( 0.1049868766404206816, -0.6046776061558809534, -0.2411417322834644161 ) ) ;
#10615 = CARTESIAN_POINT ( 'NONE',  ( 1.135170603674541256, -0.6692913385826773087, -0.1292274648535924053 ) ) ;
#10616 = CARTESIAN_POINT ( 'NONE',  ( 0.7874015748031503170, -0.1870078740157480879, -0.4822834645669291653 ) ) ;
#10617 = CARTESIAN_POINT ( 'NONE',  ( 1.968503937007874072, 0.000000000000000000, 5.879133660591329580 ) ) ;
#10618 = CARTESIAN_POINT ( 'NONE',  ( 0.7086614173228353852, -0.1870078740157479769, 0.3641732283464567677 ) ) ;
#10619 = CARTESIAN_POINT ( 'NONE',  ( -1.601049868766403650, 0.1283753931104746893, -0.1820866141732285504 ) ) ;
#10620 = EDGE_CURVE ( 'NONE', #44077, #43739, #27688, .T. ) ;
#10621 = CARTESIAN_POINT ( 'NONE',  ( 0.2887139107611556010, -0.5023911411419708095, 0.1820866141732285504 ) ) ;
#10622 = CARTESIAN_POINT ( 'NONE',  ( -0.2821522309711278487, -0.6692913385826773087, -0.1292274648535924053 ) ) ;
#10623 = CARTESIAN_POINT ( 'NONE',  ( 0.8530183727034126306, 0.05413385826771626580, -0.4176697321401330321 ) ) ;
#10624 = CARTESIAN_POINT ( 'NONE',  ( -0.5511811023622038563, -0.1870078740157479769, 0.4822834645669291653 ) ) ;
#10625 = CARTESIAN_POINT ( 'NONE',  ( -0.3917322834645670104, -0.1049643490035307020, -1.932434013944568818 ) ) ;
#10626 = CARTESIAN_POINT ( 'NONE',  ( -0.06561679790026180015, -0.3690944881889765550, -0.3153832671262227771 ) ) ;
#10627 = CARTESIAN_POINT ( 'NONE',  ( 0.9514435695538062676, -0.05778040916215522460, 0.4822834645669289988 ) ) ;
#10628 = CARTESIAN_POINT ( 'NONE',  ( 0.9055118110236227702, 0.1771653543307087630, 0.000000000000000000 ) ) ;
#10629 = ADVANCED_FACE ( 'NONE', ( #54979 ), #43576, .F. ) ;
#10630 = DIRECTION ( 'NONE',  ( 0.000000000000000000, 0.000000000000000000, -1.000000000000000000 ) ) ;
#10632 = CARTESIAN_POINT ( 'NONE',  ( 1.607611548556431069, 0.2952755905511811885, 0.1292274648535926551 ) ) ;
#10631 = DIRECTION ( 'NONE',  ( 0.000000000000000000, 1.000000000000000000, 8.673617379884024625E-16 ) ) ;
#10633 = CARTESIAN_POINT ( 'NONE',  ( -1.194225721784776262, 0.009842519685039144428, -0.3409548833797004797 ) ) ;
#10634 = CARTESIAN_POINT ( 'NONE',  ( -1.391076115485563314, -0.6046776061558809534, -0.2411417322834644161 ) ) ;
#10635 = CARTESIAN_POINT ( 'NONE',  ( -0.4068241469816267775, 0.05413385826771626580, -0.4176697321401330321 ) ) ;
#10636 = CARTESIAN_POINT ( 'NONE',  ( -0.1265901696524993347, 0.4724409448818895907, 0.1509186351706036378 ) ) ;
#10637 = CARTESIAN_POINT ( 'NONE',  ( 0.3420746716998659953, 0.1974969037888705536, -2.808398950131233640 ) ) ;
#10638 = ORIENTED_EDGE ( 'NONE', *, *, #68819, .F. ) ;
#10639 = CARTESIAN_POINT ( 'NONE',  ( 0.4330708661417329575, 0.1771653543307087630, 0.000000000000000000 ) ) ;
#10640 = CARTESIAN_POINT ( 'NONE',  ( 0.1958661417322834775, 0.3392501089628018884, -1.238845144356955252 ) ) ;
#10641 = CARTESIAN_POINT ( 'NONE',  ( 1.049868766404200127, -0.6046776061558809534, -0.2411417322834644161 ) ) ;
#10642 = CARTESIAN_POINT ( 'NONE',  ( -0.3458507752293906723, -0.3458507752293910609, -2.263779527559055094 ) ) ;
#10643 = CARTESIAN_POINT ( 'NONE',  ( 1.614173228346456712, 0.7166040191147866611, 0.1372047244094478646 ) ) ;
#10644 = CARTESIAN_POINT ( 'NONE',  ( -0.2755905511811018171, 0.2952755905511811885, 0.000000000000000000 ) ) ;
#10645 = CARTESIAN_POINT ( 'NONE',  ( -0.07858598928476964729, 1.069287512630840764, 1.119396547425128841 ) ) ;
#10646 = CARTESIAN_POINT ( 'NONE',  ( 1.332020997375328974, -0.08942795157528024563, -0.3641732283464568787 ) ) ;
#10647 = CARTESIAN_POINT ( 'NONE',  ( 0.4133858267716541968, 0.1660481256975885056, 0.3530559997133364547 ) ) ;
#10648 = CARTESIAN_POINT ( 'NONE',  ( -0.3917322834645669549, -7.196005306013483243E-17, -0.2768835713572685431 ) ) ;
#10649 = CARTESIAN_POINT ( 'NONE',  ( -0.4724409448818890911, -0.1870078740157480879, -0.4822834645669291653 ) ) ;
#10650 = CARTESIAN_POINT ( 'NONE',  ( -1.049868766404198794, 0.1283753931104746893, -0.1820866141732285504 ) ) ;
#10651 = CARTESIAN_POINT ( 'NONE',  ( 0.4658792650918640033, -0.3162353388693405765, 0.4822834645669290543 ) ) ;
#10652 = CARTESIAN_POINT ( 'NONE',  ( -0.2624671916010490880, 0.2306618581243847221, -0.2411417322834647770 ) ) ;
#10653 = CARTESIAN_POINT ( 'NONE',  ( -0.4091458600556405756, 0.2362204724409446288, -0.02624671916010498651 ) ) ;
#10654 = CARTESIAN_POINT ( 'NONE',  ( 0.1070741851644054915, -0.3996062992125986035, -2.919947506561679784 ) ) ;
#10655 = CARTESIAN_POINT ( 'NONE',  ( 4.797336870675656522E-17, -0.3917322834645670659, -1.807762097934070278 ) ) ;
#10656 = CARTESIAN_POINT ( 'NONE',  ( 0.7742782152230979209, 0.05413385826771626580, -0.4176697321401330321 ) ) ;
#10657 = CARTESIAN_POINT ( 'NONE',  ( -0.1640419947506555343, -0.3162353388693405765, 0.4822834645669290543 ) ) ;
#10658 = CARTESIAN_POINT ( 'NONE',  ( -1.568241469816272105, -0.3162353388693409650, -0.4822834645669289433 ) ) ;
#10659 = VECTOR ( 'NONE', #42839, 39.37007874015748143 ) ;
#10660 = CARTESIAN_POINT ( 'NONE',  ( 0.9776902887139113929, 0.2952755905511811885, 0.1292274648535926551 ) ) ;
#10661 = CARTESIAN_POINT ( 'NONE',  ( 0.6692913385826778638, -0.6692913385826771977, 8.415575281601705876E-17 ) ) ;
#10662 = CARTESIAN_POINT ( 'NONE',  ( 0.1958661417322834775, 0.3392501089628018884, -1.173884514435695525 ) ) ;
#10663 = CARTESIAN_POINT ( 'NONE',  ( -0.2887139107611542133, 0.2306618581243848609, 0.2411417322834645549 ) ) ;
#10664 = CARTESIAN_POINT ( 'NONE',  ( 0.1115485564304470323, 0.2952755905511811885, 0.1292274648535926551 ) ) ;
#10665 = CARTESIAN_POINT ( 'NONE',  ( -0.5643044619422565855, -0.4281496062992124485, 0.4176697321401328655 ) ) ;
#10666 = CARTESIAN_POINT ( 'NONE',  ( 0.1312335958005257930, 0.1283753931104746893, -0.1820866141732285504 ) ) ;
#10667 = CARTESIAN_POINT ( 'NONE',  ( -1.660104986876639543, -0.05778040916215560624, -0.4822834645669293319 ) ) ;
#10668 = CARTESIAN_POINT ( 'NONE',  ( -0.4426497960380713637, 1.366130357955172014, -2.619358585163587438 ) ) ;
#10669 = CARTESIAN_POINT ( 'NONE',  ( 0.5249343832021003964, 0.2306618581243847221, -0.2411417322834647770 ) ) ;
#10670 = DIRECTION ( 'NONE',  ( -1.000000000000000000, -0.000000000000000000, -0.000000000000000000 ) ) ;
#10671 = CARTESIAN_POINT ( 'NONE',  ( 1.528871391076116026, -0.6692913385826773087, -0.1292274648535924053 ) ) ;
#10672 = CARTESIAN_POINT ( 'NONE',  ( 0.1049643490035303689, 0.3917322834645670104, -2.190288713910760521 ) ) ;
#10673 = VERTEX_POINT ( 'NONE', #41938 ) ;
#10674 = VERTEX_POINT ( 'NONE', #68860 ) ;
#10675 = CARTESIAN_POINT ( 'NONE',  ( 0.6561679790026253567, -0.6046776061558809534, -0.2411417322834644161 ) ) ;
#10676 = CARTESIAN_POINT ( 'NONE',  ( 0.2755905511811031494, -0.5511811023622047445, 6.969142054262312111E-17 ) ) ;
#10678 = CARTESIAN_POINT ( 'NONE',  ( 1.534064387305127072E-17, -0.1742125984251973736, -0.3937007874015748254 ) ) ;
#10677 = CARTESIAN_POINT ( 'NONE',  ( 3.937007874015748143, 1.724409448818897905, -0.6299212598425196763 ) ) ;
#10679 = CARTESIAN_POINT ( 'NONE',  ( -0.3392501089628019995, 0.1958661417322832277, -0.8982939632545933195 ) ) ;
#10680 = PLANE ( 'NONE',  #49079 ) ;
#10681 = CARTESIAN_POINT ( 'NONE',  ( 0.6889763779527560139, 0.000000000000000000, 0.1181102362204724116 ) ) ;
#10682 = EDGE_CURVE ( 'NONE', #69303, #2585, #11577, .T. ) ;
#10683 = CARTESIAN_POINT ( 'NONE',  ( 0.3460692066303959202, -0.1998031496062991630, -2.386482939632545985 ) ) ;
#10684 = CARTESIAN_POINT ( 'NONE',  ( 0.4330708661417329575, -0.6692913385826771977, 8.415575281601705876E-17 ) ) ;
#10685 = CARTESIAN_POINT ( 'NONE',  ( -0.8792650918635160906, -0.4281496062992124485, 0.4176697321401328655 ) ) ;
#10686 = CARTESIAN_POINT ( 'NONE',  ( -0.5380577427821514602, -0.4281496062992127816, -0.4176697321401328100 ) ) ;
#10687 = CARTESIAN_POINT ( 'NONE',  ( 0.6299212598425204535, -0.1870078740157479769, 0.4822834645669291653 ) ) ;
#10688 = CARTESIAN_POINT ( 'NONE',  ( 1.358267716535433323, -0.5400638737290845981, -0.3530559997133363437 ) ) ;
#10689 = CARTESIAN_POINT ( 'NONE',  ( -1.115269913029420135, 1.079232407413005523, 0.1240654315417908660 ) ) ;
#10690 = SHAPE_DEFINITION_REPRESENTATION ( #28543, #48103 ) ;
#10691 = CARTESIAN_POINT ( 'NONE',  ( 1.358267716535433323, 0.07958543189024085140, 0.2665933059059887866 ) ) ;
#10692 = CARTESIAN_POINT ( 'NONE',  ( -0.8267716535433065062, 0.2952755905511811885, 0.000000000000000000 ) ) ;
#10693 = CARTESIAN_POINT ( 'NONE',  ( 1.443569553805774897, -0.6046776061558809534, -0.2411417322834644161 ) ) ;
#10694 = LINE ( 'NONE', #73424, #14075 ) ;
#10695 = CARTESIAN_POINT ( 'NONE',  ( -0.2624671916010490880, -0.6046776061558807314, 0.2411417322834647770 ) ) ;
#10697 = CARTESIAN_POINT ( 'NONE',  ( -3.908320185825792326, 1.537401574803149984, -0.4744094488188975722 ) ) ;
#10696 = CARTESIAN_POINT ( 'NONE',  ( 1.272965879265092637, -0.4281496062992127816, -0.4176697321401328100 ) ) ;
#10698 = CARTESIAN_POINT ( 'NONE',  ( -1.148293963254592542, -0.5511811023622048555, -0.09757992244046775898 ) ) ;
#10699 = CARTESIAN_POINT ( 'NONE',  ( 0.1771653543307093182, -0.5400638737290845981, -0.3530559997133363437 ) ) ;
#10700 = CARTESIAN_POINT ( 'NONE',  ( 1.108923884514436242, -0.08942795157527998196, 0.3641732283464567121 ) ) ;
#10701 = CARTESIAN_POINT ( 'NONE',  ( 0.2867679344610365999, -0.2867679344610365999, -1.595781209152543845 ) ) ;
#10702 = CARTESIAN_POINT ( 'NONE',  ( -1.089238845144356427, -0.004921259842519576551, 0.3153832671262227771 ) ) ;
#10703 = CARTESIAN_POINT ( 'NONE',  ( 1.325459317585302665, -0.4281496062992124485, 0.4176697321401328655 ) ) ;
#10704 = DIRECTION ( 'NONE',  ( -0.8660254037844432595, 0.000000000000000000, 0.4999999999999918954 ) ) ;
#10705 = CARTESIAN_POINT ( 'NONE',  ( -0.3018372703412066094, -0.004921259842519576551, 0.3153832671262227771 ) ) ;
#10706 = CARTESIAN_POINT ( 'NONE',  ( 5.463695987328526437E-16, -0.1870078740157479769, 0.4822834645669291653 ) ) ;
#10707 = CARTESIAN_POINT ( 'NONE',  ( -1.345144356955379816, -0.2845877964562159024, 0.3641732283464567677 ) ) ;
#10708 = CARTESIAN_POINT ( 'NONE',  ( -0.7217847769028863381, 0.05413385826771626580, -0.4176697321401330321 ) ) ;
#10709 = CARTESIAN_POINT ( 'NONE',  ( 1.541994750656168645, 0.2952755905511810774, -0.1292274648535930714 ) ) ;
#10710 = CARTESIAN_POINT ( 'NONE',  ( 0.3917322834645670659, 2.398668435337828261E-17, -0.4298093420285583055 ) ) ;
#10711 = CARTESIAN_POINT ( 'NONE',  ( -0.9973753280839886548, 0.1283753931104748280, 0.1820866141732283561 ) ) ;
#10712 = DIRECTION ( 'NONE',  ( 0.000000000000000000, 0.000000000000000000, -1.000000000000000000 ) ) ;
#10713 = CARTESIAN_POINT ( 'NONE',  ( 1.574803149606299746, -0.1870078740157479769, 0.4822834645669291653 ) ) ;
#10714 = CARTESIAN_POINT ( 'NONE',  ( 0.3458507752293908943, -0.3458507752293908943, -2.064960629921259283 ) ) ;
#10715 = CARTESIAN_POINT ( 'NONE',  ( -1.115485564304461219, -0.4281496062992124485, 0.4176697321401328655 ) ) ;
#10716 = CARTESIAN_POINT ( 'NONE',  ( -1.003937007874014853, 0.07958543189024085140, 0.2665933059059887866 ) ) ;
#10717 = CARTESIAN_POINT ( 'NONE',  ( -0.5839895013123351797, 0.1771653543307087075, -0.09757992244046823083 ) ) ;
#10718 = CARTESIAN_POINT ( 'NONE',  ( -1.574803149606298192, -0.1870078740157480879, -0.4822834645669291653 ) ) ;
#10719 = CARTESIAN_POINT ( 'NONE',  ( -0.1509186351706028884, -0.3162353388693409650, -0.4822834645669289433 ) ) ;
#10720 = CARTESIAN_POINT ( 'NONE',  ( -0.1509186351706028884, -0.2845877964562161244, -0.3641732283464567121 ) ) ;
#10721 = CARTESIAN_POINT ( 'NONE',  ( -0.9645669291338575535, -0.4536011799217367080, 0.2665933059059888421 ) ) ;
#10722 = CARTESIAN_POINT ( 'NONE',  ( -1.430446194225721390, -0.4281496062992124485, 0.4176697321401328655 ) ) ;
#10723 = CARTESIAN_POINT ( 'NONE',  ( 1.476377952755906220, 0.07958543189024071263, -0.2665933059059888421 ) ) ;
#10724 = CARTESIAN_POINT ( 'NONE',  ( 0.8267716535433078384, -0.6692913385826771977, 8.415575281601705876E-17 ) ) ;
#10725 = DIRECTION ( 'NONE',  ( -1.000000000000000000, -3.412570772413390973E-16, 0.000000000000000000 ) ) ;
#10726 = CARTESIAN_POINT ( 'NONE',  ( 0.2624671916010504757, 0.1283753931104748280, 0.1820866141732283561 ) ) ;
#10727 = CARTESIAN_POINT ( 'NONE',  ( 0.8464566929133866546, -0.5400638737290844871, 0.3530559997133364547 ) ) ;
#10728 = CARTESIAN_POINT ( 'NONE',  ( 1.167979002624672580, -0.004921259842519870586, -0.3153832671262229437 ) ) ;
#10729 = ORIENTED_EDGE ( 'NONE', *, *, #55755, .T. ) ;
#10730 = CARTESIAN_POINT ( 'NONE',  ( -1.397637795275589623, -0.5400638737290845981, -0.3530559997133363437 ) ) ;
#10731 = CARTESIAN_POINT ( 'NONE',  ( -1.069553805774277722, -0.6692913385826773087, -0.1292274648535924053 ) ) ;
#10732 = CARTESIAN_POINT ( 'NONE',  ( -0.01968503937007793844, -0.5400638737290844871, 0.3530559997133364547 ) ) ;
#10733 = CARTESIAN_POINT ( 'NONE',  ( -2.169549097624052791, 1.554815631980116297, -0.4741686481756397509 ) ) ;
#10734 = CARTESIAN_POINT ( 'NONE',  ( 0.3996062992125985480, 2.446882876249141654E-17, -2.084645669291338876 ) ) ;
#10735 = CARTESIAN_POINT ( 'NONE',  ( 0.7217847769028878924, -0.4281496062992127816, -0.4176697321401328100 ) ) ;
#10736 = CARTESIAN_POINT ( 'NONE',  ( 1.404199475065617264, -0.3690944881889763329, 0.3153832671262228327 ) ) ;
#10737 = CARTESIAN_POINT ( 'NONE',  ( 0.05249343832021075018, -0.6046776061558807314, 0.2411417322834647770 ) ) ;
#10738 = CARTESIAN_POINT ( 'NONE',  ( 0.8923884514435701520, -0.6046776061558809534, -0.2411417322834644161 ) ) ;
#10739 = CARTESIAN_POINT ( 'NONE',  ( -0.1998031496062991907, -0.3460692066303959757, -1.797900262467191590 ) ) ;
#10740 = CARTESIAN_POINT ( 'NONE',  ( 0.1058382717557499880, 0.3949938075777411073, -0.9383202099737534274 ) ) ;
#10741 = CARTESIAN_POINT ( 'NONE',  ( -0.3460692066303958092, -0.1998031496062994683, -2.414698162729658648 ) ) ;
#10742 = CARTESIAN_POINT ( 'NONE',  ( -0.2035438835850315042, -0.2140388612101737920, 0.1320934087364891429 ) ) ;
#10743 = CARTESIAN_POINT ( 'NONE',  ( -9.594673741351313045E-17, 0.3917322834645670104, -0.7795275590551180578 ) ) ;
#10744 = CARTESIAN_POINT ( 'NONE',  ( -0.4199475065616791736, 0.1283753931104746893, -0.1820866141732285504 ) ) ;
#10745 = CARTESIAN_POINT ( 'NONE',  ( -0.8398950131233589023, -0.6046776061558809534, -0.2411417322834644161 ) ) ;
#10746 = CARTESIAN_POINT ( 'NONE',  ( 0.2821522309711292364, -0.6692913385826771977, 0.1292274648535927661 ) ) ;
#10747 = CARTESIAN_POINT ( 'NONE',  ( 0.3949938075777408852, 0.1058382717557500435, -2.248687664041995049 ) ) ;
#10748 = CARTESIAN_POINT ( 'NONE',  ( -1.469816272965878357, 0.2306618581243848609, 0.2411417322834645549 ) ) ;
#10749 = CARTESIAN_POINT ( 'NONE',  ( 1.305774278215223960, 0.2952755905511810774, -0.1292274648535930714 ) ) ;
#10750 = CARTESIAN_POINT ( 'NONE',  ( 0.2362204724409449064, 0.4091458600556404646, -2.506561679790026087 ) ) ;
#10751 = CARTESIAN_POINT ( 'NONE',  ( 0.2925321140481932369, 0.2925321140481932369, -1.712598425196850460 ) ) ;
#10752 = CARTESIAN_POINT ( 'NONE',  ( 1.154855643044620184, 0.2306618581243847221, -0.2411417322834647770 ) ) ;
#10753 = CARTESIAN_POINT ( 'NONE',  ( 1.062992125984252745, -0.6692913385826771977, 8.415575281601705876E-17 ) ) ;
#10754 = CARTESIAN_POINT ( 'NONE',  ( 1.266404199475066328, -0.08942795157527998196, 0.3641732283464567121 ) ) ;
#10756 = CARTESIAN_POINT ( 'NONE',  ( -1.391076115485563314, -0.6046776061558809534, -0.2411417322834644161 ) ) ;
#10755 = CARTESIAN_POINT ( 'NONE',  ( -1.502624671916009680, -0.2845877964562159024, 0.3641732283464567677 ) ) ;
#10757 = CARTESIAN_POINT ( 'NONE',  ( 0.1958661417322836162, -0.3392501089628018329, -2.849062049047557998 ) ) ;
#10758 = CARTESIAN_POINT ( 'NONE',  ( -0.2017716535433071445, 0.2017716535433070613, -0.3937007874015748254 ) ) ;
#10759 = CARTESIAN_POINT ( 'NONE',  ( 0.9842519685039378130, -0.6692913385826771977, 8.415575281601705876E-17 ) ) ;
#10760 = CARTESIAN_POINT ( 'NONE',  ( 1.679790026246720025, 0.1283753931104748280, 0.1820866141732283561 ) ) ;
#10761 = CARTESIAN_POINT ( 'NONE',  ( -0.6955380577427815458, -0.4281496062992127816, -0.4176697321401328100 ) ) ;
#10762 = CARTESIAN_POINT ( 'NONE',  ( -0.4199475065616791736, 0.2306618581243847221, -0.2411417322834647770 ) ) ;
#10763 = CARTESIAN_POINT ( 'NONE',  ( 1.450131233595801428, 0.2952755905511811885, 0.1292274648535926551 ) ) ;
#10764 = CARTESIAN_POINT ( 'NONE',  ( 0.3392501089628018884, -0.1958661417322834220, -0.03215223097112869521 ) ) ;
#10765 = CARTESIAN_POINT ( 'NONE',  ( 0.01312335958005323398, 0.05413385826771666132, 0.4176697321401328100 ) ) ;
#10766 = CARTESIAN_POINT ( 'NONE',  ( 0.3917322834645669549, 0.1049643490035304660, -2.321522309711285814 ) ) ;
#10767 = CARTESIAN_POINT ( 'NONE',  ( -1.581364829396324945, -0.08942795157528024563, -0.3641732283464568787 ) ) ;
#10768 = ORIENTED_EDGE ( 'NONE', *, *, #43922, .T. ) ;
#10769 = CARTESIAN_POINT ( 'NONE',  ( -9.674558042662121740E-17, 0.3949938075777409963, -2.834645669291338432 ) ) ;
#10770 = ORIENTED_EDGE ( 'NONE', *, *, #45969, .F. ) ;
#10771 = CARTESIAN_POINT ( 'NONE',  ( -1.313877454013331780, 0.2755905511811023723, 0.8967544760595740350 ) ) ;
#10772 = CARTESIAN_POINT ( 'NONE',  ( -1.450131233595799651, -0.6692913385826771977, 0.1292274648535927661 ) ) ;
#10773 = CARTESIAN_POINT ( 'NONE',  ( 4.893765752498283924E-17, -0.3996062992125986035, -1.023622047244094446 ) ) ;
#10774 = CARTESIAN_POINT ( 'NONE',  ( 1.561679790026247350, -0.004921259842519870586, -0.3153832671262229437 ) ) ;
#10775 = CARTESIAN_POINT ( 'NONE',  ( -0.5314960629921323676, 2.755905511811024056, 1.813482582612291560 ) ) ;
#10776 = CARTESIAN_POINT ( 'NONE',  ( -0.5314960629921146040, 2.755905511811024056, -3.264097702071374840 ) ) ;
#10777 = CARTESIAN_POINT ( 'NONE',  ( -0.3072632741606444173, 1.737537999042348513, 0.06216925787398272507 ) ) ;
#10778 = CARTESIAN_POINT ( 'NONE',  ( -0.1049643490035307020, 0.3917322834645669549, -0.4061679790026246351 ) ) ;
#10779 = CARTESIAN_POINT ( 'NONE',  ( -0.3215223097112853146, -0.08942795157528024563, -0.3641732283464568787 ) ) ;
#10780 = CARTESIAN_POINT ( 'NONE',  ( -1.259842519685038686, -0.1870078740157479769, 0.3641732283464567677 ) ) ;
#10781 = CARTESIAN_POINT ( 'NONE',  ( 1.561679790026247350, -0.4281496062992124485, 0.4176697321401328655 ) ) ;
#10782 = CARTESIAN_POINT ( 'NONE',  ( 0.3149606299212603933, -0.1870078740157479769, 0.4822834645669291653 ) ) ;
#10783 = CARTESIAN_POINT ( 'NONE',  ( -1.364829396325458521, -0.6046776061558807314, 0.2411417322834647770 ) ) ;
#10784 = CARTESIAN_POINT ( 'NONE',  ( 0.1958661417322834775, 0.3392501089628018884, -0.2939632545931757934 ) ) ;
#10785 = VERTEX_POINT ( 'NONE', #61720 ) ;
#10786 = CARTESIAN_POINT ( 'NONE',  ( -1.627296587926508442, 0.2306618581243848609, 0.2411417322834645549 ) ) ;
#10787 = DIRECTION ( 'NONE',  ( 0.000000000000000000, -1.000000000000000000, 0.000000000000000000 ) ) ;
#10788 = CARTESIAN_POINT ( 'NONE',  ( -0.4724409448818895907, -0.1265901696524993070, -1.620734908136482799 ) ) ;
#10789 = DIRECTION ( 'NONE',  ( -1.000000000000000000, 0.000000000000000000, -0.000000000000000000 ) ) ;
#10790 = CARTESIAN_POINT ( 'NONE',  ( -0.3917322834645670104, -7.196005306013484475E-17, -2.643700787401574548 ) ) ;
#10791 = CARTESIAN_POINT ( 'NONE',  ( -0.8202099737532799750, 0.2952755905511810774, -0.1292274648535930714 ) ) ;
#10792 = CARTESIAN_POINT ( 'NONE',  ( 1.397637795275591177, 0.1660481256975883668, -0.3530559997133364547 ) ) ;
#10794 = DIRECTION ( 'NONE',  ( 0.000000000000000000, -1.000000000000000000, -0.000000000000000000 ) ) ;
#10793 = CARTESIAN_POINT ( 'NONE',  ( 0.7414698162729664865, 0.2952755905511811885, 0.1292274648535926551 ) ) ;
#10795 = CARTESIAN_POINT ( 'NONE',  ( 1.469816272965879911, -0.6046776061558807314, 0.2411417322834647770 ) ) ;
#10796 = CARTESIAN_POINT ( 'NONE',  ( -0.7874015748031489847, -0.1870078740157479769, 0.4822834645669291653 ) ) ;
#10797 = CARTESIAN_POINT ( 'NONE',  ( 0.2867679344610365999, 0.2867679344610365999, -0.2178284532470323442 ) ) ;
#10798 = CARTESIAN_POINT ( 'NONE',  ( 0.03280839895013198948, 0.1771653543307087630, 0.09757992244046791164 ) ) ;
#10799 = CARTESIAN_POINT ( 'NONE',  ( 0.3917322834645669549, 0.1049643490035304660, -0.5242782152230972548 ) ) ;
#10800 = CARTESIAN_POINT ( 'NONE',  ( -0.01968503937007793844, 0.07958543189024071263, -0.2665933059059888421 ) ) ;
#10801 = CARTESIAN_POINT ( 'NONE',  ( 0.5314960629921264834, 0.07958543189024071263, -0.2665933059059888421 ) ) ;
#10802 = CARTESIAN_POINT ( 'NONE',  ( 0.3346456692913390985, 0.1660481256975885056, 0.3530559997133364547 ) ) ;
#10803 = CARTESIAN_POINT ( 'NONE',  ( -0.5511811023622038563, -0.1870078740157479769, 0.3641732283464567677 ) ) ;
#10804 = CARTESIAN_POINT ( 'NONE',  ( 0.1049643490035304938, -0.3917322834645669549, -2.439632545931758045 ) ) ;
#10805 = CARTESIAN_POINT ( 'NONE',  ( 1.450131233595801428, 0.2952755905511811885, 0.1292274648535926551 ) ) ;
#10806 = CARTESIAN_POINT ( 'NONE',  ( -1.049868766404198794, -0.6046776061558807314, 0.2411417322834647770 ) ) ;
#10807 = CARTESIAN_POINT ( 'NONE',  ( -1.157146581871515012E-16, 0.4724409448818898682, -0.7066929133858268486 ) ) ;
#10808 = CARTESIAN_POINT ( 'NONE',  ( -0.05249343832020938322, -0.6046776061558809534, -0.2411417322834644161 ) ) ;
#10809 = CARTESIAN_POINT ( 'NONE',  ( -0.3608923884514428360, 0.2952755905511811885, 0.1292274648535926551 ) ) ;
#10810 = CARTESIAN_POINT ( 'NONE',  ( 1.062992125984252745, 0.1771653543307087630, 0.000000000000000000 ) ) ;
#10811 = CARTESIAN_POINT ( 'NONE',  ( 0.2952755905511816326, -0.4536011799217367080, 0.2665933059059888421 ) ) ;
#10812 = CARTESIAN_POINT ( 'NONE',  ( -0.2362204724409442680, -0.1870078740157480879, -0.4822834645669291653 ) ) ;
#10813 = CARTESIAN_POINT ( 'NONE',  ( -0.8398950131233585692, 0.2306618581243848609, 0.2411417322834645549 ) ) ;
#10814 = CARTESIAN_POINT ( 'NONE',  ( -3.884611959489589594, 2.725289161120230563, 0.5314960629921258173 ) ) ;
#10815 = CARTESIAN_POINT ( 'NONE',  ( 1.679790026246720025, 0.1283753931104748280, 0.1820866141732283561 ) ) ;
#10816 = CARTESIAN_POINT ( 'NONE',  ( 0.2362204724409456558, -0.1870078740157479769, 0.4822834645669291653 ) ) ;
#10817 = ORIENTED_EDGE ( 'NONE', *, *, #57389, .F. ) ;
#10818 = CARTESIAN_POINT ( 'NONE',  ( 0.3996062992125985480, 2.446882876249141654E-17, -1.927165354330708569 ) ) ;
#10819 =( BOUNDED_CURVE ( )  B_SPLINE_CURVE ( 1, ( #59907, #2259 ),
 .UNSPECIFIED., .F., .F. ) 
 B_SPLINE_CURVE_WITH_KNOTS ( ( 2, 2 ),
 ( 0.000000000000000000, 0.002000000000000001776 ),
 .UNSPECIFIED. ) 
 CURVE ( )  GEOMETRIC_REPRESENTATION_ITEM ( )  RATIONAL_B_SPLINE_CURVE ( ( 0.9875488213027523443, 0.9875488213027523443 ) ) 
 REPRESENTATION_ITEM ( '' )  );
#10820 = CARTESIAN_POINT ( 'NONE',  ( 1.351706036745407458, -0.4281496062992127816, -0.4176697321401328100 ) ) ;
#10821 = CARTESIAN_POINT ( 'NONE',  ( -0.6233595800524928121, -0.08942795157527998196, 0.3641732283464567121 ) ) ;
#10822 = CARTESIAN_POINT ( 'NONE',  ( -0.5249343832020990641, -0.6046776061558809534, -0.2411417322834644161 ) ) ;
#10823 = CARTESIAN_POINT ( 'NONE',  ( 1.128608923884515169, -0.6046776061558809534, -0.2411417322834644161 ) ) ;
#10824 = CARTESIAN_POINT ( 'NONE',  ( 0.8267716535433078384, -0.6692913385826771977, 8.415575281601705876E-17 ) ) ;
#10825 = CYLINDRICAL_SURFACE ( 'NONE', #11580, 0.4744094488188972947 ) ;
#10826 = CARTESIAN_POINT ( 'NONE',  ( -1.056430446194224881, 0.1771653543307087075, -0.09757992244046823083 ) ) ;
#10827 = CARTESIAN_POINT ( 'NONE',  ( -0.3996062992125984925, -0.1070741851644056719, -0.4376640419947506744 ) ) ;
#10828 = CARTESIAN_POINT ( 'NONE',  ( 0.3996062992125986590, -0.1070741851644053111, -0.5839895013123358458 ) ) ;
#10829 = CARTESIAN_POINT ( 'NONE',  ( -0.1974969037888706647, 0.3420746716998658843, 0.1443569553805773842 ) ) ;
#10830 = CARTESIAN_POINT ( 'NONE',  ( 1.469816272965879911, -0.5023911411419708095, 0.1820866141732285504 ) ) ;
#10831 = CARTESIAN_POINT ( 'NONE',  ( 0.7939632545931766261, -0.08942795157527998196, 0.3641732283464567121 ) ) ;
#10832 = CONICAL_SURFACE ( 'NONE', #5477, 3.228346456692913424, 0.7853981633974500554 ) ;
#10833 = CARTESIAN_POINT ( 'NONE',  ( 0.6102362204724416372, -0.5400638737290844871, 0.3530559997133364547 ) ) ;
#10834 = CARTESIAN_POINT ( 'NONE',  ( 0.4265091863517068149, 0.2066929133858267931, 0.1054918080437490802 ) ) ;
#10835 = CARTESIAN_POINT ( 'NONE',  ( -0.2891555358219911054, 0.2891555358219909388, -1.041338582677165503 ) ) ;
#10836 = CARTESIAN_POINT ( 'NONE',  ( 0.8070866141732289112, -0.4536011799217368745, -0.2665933059059886201 ) ) ;
#10837 = CARTESIAN_POINT ( 'NONE',  ( -0.1968503937007867743, 0.2952755905511811885, 0.000000000000000000 ) ) ;
#10838 = CARTESIAN_POINT ( 'NONE',  ( -0.6496062992125976043, 0.1660481256975883668, -0.3530559997133364547 ) ) ;
#10839 = CARTESIAN_POINT ( 'NONE',  ( 1.430446194225722500, -0.4281496062992127816, -0.4176697321401328100 ) ) ;
#10840 = CARTESIAN_POINT ( 'NONE',  ( -0.4091458600556402980, -0.2362204724409451284, -1.312335958005249381 ) ) ;
#10841 = CARTESIAN_POINT ( 'NONE',  ( -9.787531504996567848E-17, 0.3996062992125986035, -2.362204724409448620 ) ) ;
#10842 = CARTESIAN_POINT ( 'NONE',  ( 0.03280839895013198948, 0.1771653543307087630, 0.09757992244046791164 ) ) ;
#10843 = ORIENTED_EDGE ( 'NONE', *, *, #9952, .F. ) ;
#10844 = CARTESIAN_POINT ( 'NONE',  ( -0.2867679344610367109, 0.2867679344610365444, -0.9613054050206844003 ) ) ;
#10845 = VERTEX_POINT ( 'NONE', #62128 ) ;
#10846 = CARTESIAN_POINT ( 'NONE',  ( -1.030183727034119867, -0.05778040916215560624, -0.4822834645669293319 ) ) ;
#10847 = CARTESIAN_POINT ( 'NONE',  ( -0.07874015748031421014, -0.1870078740157479769, 0.4822834645669291653 ) ) ;
#10848 = CARTESIAN_POINT ( 'NONE',  ( -0.2230971128608915943, 0.05413385826771666132, 0.4176697321401328100 ) ) ;
#10849 = CARTESIAN_POINT ( 'NONE',  ( 0.4593175853018380828, 0.05413385826771626580, -0.4176697321401330321 ) ) ;
#10850 = CARTESIAN_POINT ( 'NONE',  ( -0.6102362204724400829, -0.5400638737290845981, -0.3530559997133363437 ) ) ;
#10851 = CARTESIAN_POINT ( 'NONE',  ( -1.141732283464566011, 0.2952755905511811885, 0.000000000000000000 ) ) ;
#10852 = CARTESIAN_POINT ( 'NONE',  ( -0.9251968503937002541, 0.1660481256975885056, 0.3530559997133364547 ) ) ;
#10853 = CARTESIAN_POINT ( 'NONE',  ( 0.9055118110236227702, -0.6692913385826771977, 8.415575281601705876E-17 ) ) ;
#10854 = CARTESIAN_POINT ( 'NONE',  ( 0.6627296587926515548, 0.2952755905511811885, 0.1292274648535926551 ) ) ;
#10855 = EDGE_CURVE ( 'NONE', #32199, #5751, #15011, .T. ) ;
#10856 = CARTESIAN_POINT ( 'NONE',  ( -0.1049643490035307020, 0.3917322834645669549, -0.9435695538057740084 ) ) ;
#10857 = CARTESIAN_POINT ( 'NONE',  ( -0.5249343832020990641, 0.1283753931104748280, 0.1820866141732283561 ) ) ;
#10858 = EDGE_LOOP ( 'NONE', ( #46512, #46650, #26275, #46230 ) ) ;
#10859 = CARTESIAN_POINT ( 'NONE',  ( 0.3420746716998660508, -0.1974969037888703871, -1.364829396325459410 ) ) ;
#10860 = ORIENTED_EDGE ( 'NONE', *, *, #1370, .F. ) ;
#10861 = CARTESIAN_POINT ( 'NONE',  ( -1.095800524934382292, -0.08942795157527998196, 0.3641732283464567121 ) ) ;
#10862 = CARTESIAN_POINT ( 'NONE',  ( -0.3608923884514428360, 0.2952755905511811885, 0.1292274648535926551 ) ) ;
#10863 = CARTESIAN_POINT ( 'NONE',  ( 0.7749820319012125092, 2.784432375088962958E-17, -0.3464511005275205946 ) ) ;
#10864 = CARTESIAN_POINT ( 'NONE',  ( -0.6627296587926503335, -0.6692913385826771977, 0.1292274648535927661 ) ) ;
#10865 = CARTESIAN_POINT ( 'NONE',  ( -0.7349081364829390672, 0.2306618581243847221, -0.2411417322834647770 ) ) ;
#10866 = CARTESIAN_POINT ( 'NONE',  ( -1.240157480314959759, -0.5400638737290845981, -0.3530559997133363437 ) ) ;
#10867 = DIRECTION ( 'NONE',  ( 1.000000000000000000, 0.000000000000000000, 0.000000000000000000 ) ) ;
#10868 = CARTESIAN_POINT ( 'NONE',  ( 0.8530183727034128527, -0.3690944881889763329, 0.3153832671262228327 ) ) ;
#10869 = FACE_OUTER_BOUND ( 'NONE', #932, .T. ) ;
#10870 = CARTESIAN_POINT ( 'NONE',  ( -0.3392501089628019995, 0.1958661417322832277, 0.04658792650918625738 ) ) ;
#10871 = CARTESIAN_POINT ( 'NONE',  ( 0.006561679790026889343, -0.08942795157527998196, 0.3641732283464567121 ) ) ;
#10872 = CARTESIAN_POINT ( 'NONE',  ( -0.4790026246719152336, -0.05778040916215560624, -0.4822834645669293319 ) ) ;
#10873 = CARTESIAN_POINT ( 'NONE',  ( -0.2690288713910754526, -0.6692913385826771977, 0.1292274648535927661 ) ) ;
#10874 = ORIENTED_EDGE ( 'NONE', *, *, #57015, .F. ) ;
#10875 = CARTESIAN_POINT ( 'NONE',  ( -0.3460692066303958092, -0.1998031496062994683, -2.257217847769029007 ) ) ;
#10876 = CARTESIAN_POINT ( 'NONE',  ( -3.184294706754630777, 2.755905511811024056, 0.5314960629921260393 ) ) ;
#10877 = ORIENTED_EDGE ( 'NONE', *, *, #68192, .T. ) ;
#10878 = CARTESIAN_POINT ( 'NONE',  ( -0.3996062992125985480, -7.340648628747423112E-17, -1.690944881889763884 ) ) ;
#10879 = CARTESIAN_POINT ( 'NONE',  ( -0.2087913723976025926, 0.2087913723976025371, 0.1248231986745539646 ) ) ;
#10880 = CARTESIAN_POINT ( 'NONE',  ( -0.7939632545931754048, -0.2845877964562159024, 0.3641732283464567677 ) ) ;
#10881 = CARTESIAN_POINT ( 'NONE',  ( -1.095800524934382292, -0.05778040916215522460, 0.4822834645669289988 ) ) ;
#10882 = B_SPLINE_CURVE_WITH_KNOTS ( 'NONE', 3,
 ( #71193, #78354, #63621, #45072, #70775, #6789, #26146, #32885, #31628, #52230 ),
 .UNSPECIFIED., .F., .F.,
 ( 4, 2, 2, 2, 4 ),
 ( 0.000000000000000000, 0.001551611299846700686, 0.002327416949770050921, 0.002715319774731726581, 0.003103222599693402674 ),
 .UNSPECIFIED. ) ;
#10883 = CARTESIAN_POINT ( 'NONE',  ( -0.1265901696524986964, -0.4724409448818899238, -0.5446194225721783244 ) ) ;
#10884 = CARTESIAN_POINT ( 'NONE',  ( -0.3772065495488707287, 1.248034150500769046, 3.918934030054451512 ) ) ;
#10885 = CARTESIAN_POINT ( 'NONE',  ( -0.2867679344610364334, -0.2867679344610367109, -0.05118110236220468900 ) ) ;
#10886 = CARTESIAN_POINT ( 'NONE',  ( 1.167979002624672580, -0.4281496062992124485, 0.4176697321401328655 ) ) ;
#10887 = CARTESIAN_POINT ( 'NONE',  ( 0.3018372703412079971, -0.4281496062992124485, 0.4176697321401328655 ) ) ;
#10888 = CARTESIAN_POINT ( 'NONE',  ( 0.6364829396325465405, -0.3162353388693409650, -0.4822834645669289433 ) ) ;
#10889 = CARTESIAN_POINT ( 'NONE',  ( -0.5905511811023613777, -0.5511811023622047445, 6.969142054262312111E-17 ) ) ;
#10890 = CARTESIAN_POINT ( 'NONE',  ( -0.3477690288713905509, -0.6692913385826771977, 0.1292274648535927661 ) ) ;
#10891 = CARTESIAN_POINT ( 'NONE',  ( -0.4724409448818899238, 0.1265901696524986686, -2.314304461942256808 ) ) ;
#10892 = CARTESIAN_POINT ( 'NONE',  ( -0.8858267716535425107, 0.1660481256975883668, -0.3530559997133364547 ) ) ;
#10893 = CARTESIAN_POINT ( 'NONE',  ( -0.3420746716998662729, 0.1974969037888702206, -2.150262467191601523 ) ) ;
#10894 = CARTESIAN_POINT ( 'NONE',  ( 1.430446194225722500, -0.004921259842519576551, 0.3153832671262227771 ) ) ;
#10895 = CARTESIAN_POINT ( 'NONE',  ( -0.2362204724409442680, -0.1870078740157480601, -0.3641732283464567677 ) ) ;
#10896 = CARTESIAN_POINT ( 'NONE',  ( 1.207349081364829990, 0.1283753931104748280, 0.1820866141732283561 ) ) ;
#10898 = ADVANCED_FACE ( 'NONE', ( #22592 ), #75601, .F. ) ;
#10897 = CARTESIAN_POINT ( 'NONE',  ( -1.719160104986876103, 0.05413385826771666132, 0.4176697321401328100 ) ) ;
#10899 = CONICAL_SURFACE ( 'NONE', #37796, 0.1771653543307085410, 1.029744258676653645 ) ;
#10900 = CARTESIAN_POINT ( 'NONE',  ( -1.043307086614172041, -0.4536011799217367080, 0.2665933059059888421 ) ) ;
#10901 = CARTESIAN_POINT ( 'NONE',  ( 1.601049868766404982, 0.2306618581243848609, 0.2411417322834645549 ) ) ;
#10902 = CARTESIAN_POINT ( 'NONE',  ( -1.272965879265091305, -0.4281496062992124485, 0.4176697321401328655 ) ) ;
#10903 = CARTESIAN_POINT ( 'NONE',  ( -0.4527559055118102749, -0.5400638737290845981, -0.3530559997133363437 ) ) ;
#10904 = CARTESIAN_POINT ( 'NONE',  ( 0.2821522309711292364, 0.2952755905511810219, -0.1292274648535930437 ) ) ;
#10905 = CARTESIAN_POINT ( 'NONE',  ( -0.1377952755905504645, -0.4536011799217368745, -0.2665933059059886201 ) ) ;
#10906 = CARTESIAN_POINT ( 'NONE',  ( -1.692913385826770645, 0.1771653543307087630, 0.000000000000000000 ) ) ;
#10907 = CARTESIAN_POINT ( 'NONE',  ( 0.6627296587926517768, -0.6692913385826773087, -0.1292274648535924053 ) ) ;
#10908 = LINE ( 'NONE', #42873, #7553 ) ;
#10909 = CARTESIAN_POINT ( 'NONE',  ( 1.345144356955381593, -0.2845877964562161244, -0.3641732283464567121 ) ) ;
#10910 = CARTESIAN_POINT ( 'NONE',  ( -0.8530183727034112984, -0.4281496062992127816, -0.4176697321401328100 ) ) ;
#10911 = CARTESIAN_POINT ( 'NONE',  ( -0.07217847769028787330, -0.08942795157527998196, 0.3641732283464567121 ) ) ;
#10912 = CARTESIAN_POINT ( 'NONE',  ( 0.000000000000000000, 0.03937007874015747977, 0.000000000000000000 ) ) ;
#10913 = CARTESIAN_POINT ( 'NONE',  ( 0.1049868766404206816, -0.5023911411419708095, -0.1820866141732282451 ) ) ;
#10914 = CARTESIAN_POINT ( 'NONE',  ( -0.02624671916010428221, 0.2306618581243847221, -0.2411417322834647770 ) ) ;
#10915 = ADVANCED_FACE ( 'NONE', ( #16706 ), #42347, .F. ) ;
#10916 = CARTESIAN_POINT ( 'NONE',  ( -0.1070741851644056997, 0.3996062992125984925, -0.8707349081364830212 ) ) ;
#10917 = CARTESIAN_POINT ( 'NONE',  ( -0.3392501089628017219, -0.1958661417322836718, -2.341863517060367439 ) ) ;
#10918 = CARTESIAN_POINT ( 'NONE',  ( 0.6102362204724416372, -0.4536011799217367080, 0.2665933059059888421 ) ) ;
#10919 = CARTESIAN_POINT ( 'NONE',  ( -0.5774278215223089816, -0.6046776061558807314, 0.2411417322834647770 ) ) ;
#10920 = CARTESIAN_POINT ( 'NONE',  ( -0.7939632545931750718, -0.05778040916215560624, -0.4822834645669293319 ) ) ;
#10921 = CARTESIAN_POINT ( 'NONE',  ( -0.7414698162729651543, -0.5511811023622046335, 0.09757992244046803654 ) ) ;
#10922 = CARTESIAN_POINT ( 'NONE',  ( 2.795275590551181466, 2.793565526369266916, 0.000000000000000000 ) ) ;
#10923 = CARTESIAN_POINT ( 'NONE',  ( -0.5708661417322825615, -0.4536011799217367080, 0.2665933059059888421 ) ) ;
#10924 = CARTESIAN_POINT ( 'NONE',  ( -0.03280839895013062252, 0.2952755905511810774, -0.1292274648535930714 ) ) ;
#10925 = CARTESIAN_POINT ( 'NONE',  ( -1.371391076115484831, 0.1771653543307087075, -0.09757992244046823083 ) ) ;
#10926 = CARTESIAN_POINT ( 'NONE',  ( 0.2925321140481932369, 0.2925321140481932369, -1.316929133858267820 ) ) ;
#10927 = CARTESIAN_POINT ( 'NONE',  ( 1.568241469816273437, -0.3162353388693405765, 0.4822834645669290543 ) ) ;
#10928 = CARTESIAN_POINT ( 'NONE',  ( -0.4724409448818917001, 0.1265901696524956710, -2.237532808398950301 ) ) ;
#10929 = ORIENTED_EDGE ( 'NONE', *, *, #10612, .F. ) ;
#10930 = CARTESIAN_POINT ( 'NONE',  ( -1.338582677165353729, -0.1870078740157480601, -0.3641732283464567677 ) ) ;
#10931 = CARTESIAN_POINT ( 'NONE',  ( -0.3149606299212590610, -0.1870078740157479769, 0.4822834645669291653 ) ) ;
#10932 = CARTESIAN_POINT ( 'NONE',  ( -1.332020997375327642, -0.05778040916215522460, 0.4822834645669289988 ) ) ;
#10933 = CARTESIAN_POINT ( 'NONE',  ( 0.3917322834645670104, 2.398668435337828261E-17, -1.462598425196850460 ) ) ;
#10934 = CARTESIAN_POINT ( 'NONE',  ( 1.614173228346456712, 2.401574803149606474, 0.1372047244094478646 ) ) ;
#10935 = CARTESIAN_POINT ( 'NONE',  ( 0.8661417322834653598, -0.1870078740157479769, 0.4822834645669291653 ) ) ;
#10936 = CARTESIAN_POINT ( 'NONE',  ( 0.4658792650918641698, -0.05778040916215560624, -0.4822834645669293319 ) ) ;
#10937 = DIRECTION ( 'NONE',  ( 0.000000000000000000, -0.000000000000000000, 1.000000000000000000 ) ) ;
#10938 = CARTESIAN_POINT ( 'NONE',  ( 0.2925321140481931814, 0.2925321140481931814, -2.419291338582677309 ) ) ;
#10939 = CARTESIAN_POINT ( 'NONE',  ( 1.030183727034121421, -0.2845877964562161244, -0.3641732283464567121 ) ) ;
#10940 = CARTESIAN_POINT ( 'NONE',  ( -0.3996062992125986035, -0.1070741851644056997, -0.9908136482939633449 ) ) ;
#10941 = EDGE_LOOP ( 'NONE', ( #25934, #13972, #37451, #72748 ) ) ;
#10942 = CARTESIAN_POINT ( 'NONE',  ( -0.7742782152230962556, -0.3690944881889765550, -0.3153832671262227771 ) ) ;
#10943 = CARTESIAN_POINT ( 'NONE',  ( -0.3917322834645669549, -0.1049643490035306603, -2.557742782152230721 ) ) ;
#10944 = ORIENTED_EDGE ( 'NONE', *, *, #51527, .F. ) ;
#10945 = CARTESIAN_POINT ( 'NONE',  ( 0.2493438320209980519, -0.4281496062992127816, -0.4176697321401328100 ) ) ;
#10946 = CARTESIAN_POINT ( 'NONE',  ( -0.3083989501312330295, -0.05778040916215522460, 0.4822834645669289988 ) ) ;
#10947 = CARTESIAN_POINT ( 'NONE',  ( -1.082677165354329896, -0.5400638737290845981, -0.3530559997133363437 ) ) ;
#10948 = CARTESIAN_POINT ( 'NONE',  ( 0.8989501312335964611, 0.2952755905511811885, 0.1292274648535926551 ) ) ;
#10949 = CARTESIAN_POINT ( 'NONE',  ( -1.443569553805773564, 0.1283753931104746893, -0.1820866141732285504 ) ) ;
#10950 = DIRECTION ( 'NONE',  ( 0.000000000000000000, 0.000000000000000000, -1.000000000000000000 ) ) ;
#10951 = CARTESIAN_POINT ( 'NONE',  ( 0.1312335958005257930, 0.2306618581243847221, -0.2411417322834647770 ) ) ;
#10952 = CARTESIAN_POINT ( 'NONE',  ( -1.227034120734907141, -0.6692913385826773087, -0.1292274648535924053 ) ) ;
#10953 = CARTESIAN_POINT ( 'NONE',  ( -0.1958661417322834497, -0.3392501089628018884, -1.877933440123672471 ) ) ;
#10954 = DIRECTION ( 'NONE',  ( 0.000000000000000000, 0.000000000000000000, -1.000000000000000000 ) ) ;
#10955 = CARTESIAN_POINT ( 'NONE',  ( 2.554262525012262586, 1.537401574803149984, -0.4744094488188970171 ) ) ;
#10956 = CARTESIAN_POINT ( 'NONE',  ( 0.3917322834645670104, 2.398668435337828261E-17, 0.04724409448818902429 ) ) ;
#10957 = CARTESIAN_POINT ( 'NONE',  ( 0.8792650918635177559, -0.004921259842519576551, 0.3153832671262227771 ) ) ;
#10958 = EDGE_LOOP ( 'NONE', ( #65709, #73696, #15934, #12428 ) ) ;
#10959 = CARTESIAN_POINT ( 'NONE',  ( 0.2891555358219910499, 0.2891555358219910499, -0.2952755905511811885 ) ) ;
#10960 = CARTESIAN_POINT ( 'NONE',  ( -0.7086614173228339419, -0.1870078740157479769, 0.4822834645669291653 ) ) ;
#10961 = ORIENTED_EDGE ( 'NONE', *, *, #27771, .F. ) ;
#10962 = CARTESIAN_POINT ( 'NONE',  ( 0.006561679790026889343, -0.08942795157527998196, 0.3641732283464567121 ) ) ;
#10963 = CARTESIAN_POINT ( 'NONE',  ( -1.620734908136482577, -0.6692913385826773087, -0.1292274648535924053 ) ) ;
#10964 = CARTESIAN_POINT ( 'NONE',  ( 0.5118110236220478892, 0.2952755905511811885, 0.000000000000000000 ) ) ;
#10965 = CARTESIAN_POINT ( 'NONE',  ( 0.5446194225721792126, -0.05778040916215560624, -0.4822834645669293319 ) ) ;
#10966 = CARTESIAN_POINT ( 'NONE',  ( -0.5511811023622041894, -0.1870078740157480879, -0.4822834645669291653 ) ) ;
#10967 = CARTESIAN_POINT ( 'NONE',  ( -0.1958661417322836995, 0.3392501089628017219, -1.112224040191287955 ) ) ;
#10968 = CARTESIAN_POINT ( 'NONE',  ( -0.7677165354330699465, -0.5400638737290845981, -0.3530559997133363437 ) ) ;
#10969 = CARTESIAN_POINT ( 'NONE',  ( -0.1049643490035302024, -0.3917322834645671215, -2.833989501312335957 ) ) ;
#10970 = CARTESIAN_POINT ( 'NONE',  ( 1.227034120734908917, -0.5511811023622046335, 0.09757992244046803654 ) ) ;
#10971 = CARTESIAN_POINT ( 'NONE',  ( -1.194225721784776262, -0.4281496062992124485, 0.4176697321401328655 ) ) ;
#10972 = CARTESIAN_POINT ( 'NONE',  ( 0.8398950131233602345, -0.6046776061558807314, 0.2411417322834647770 ) ) ;
#10973 = CARTESIAN_POINT ( 'NONE',  ( 1.017060367454068803, -0.3162353388693405765, 0.4822834645669290543 ) ) ;
#10974 = CARTESIAN_POINT ( 'NONE',  ( 0.3996062992125986035, 2.446882876249141962E-17, -1.062992125984252079 ) ) ;
#10975 = CARTESIAN_POINT ( 'NONE',  ( -1.332020997375327642, -0.3162353388693409650, -0.4822834645669289433 ) ) ;
#10976 = CARTESIAN_POINT ( 'NONE',  ( -0.1070741851644051862, -0.3996062992125986590, -0.4639107611548556331 ) ) ;
#10977 = CARTESIAN_POINT ( 'NONE',  ( 0.2034120734908142214, 0.2952755905511810774, -0.1292274648535930714 ) ) ;
#10978 = CARTESIAN_POINT ( 'NONE',  ( -0.2925321140481932924, 0.2925321140481931814, -2.381889763779527325 ) ) ;
#10979 = CARTESIAN_POINT ( 'NONE',  ( -1.377952755905511140, -0.5511811023622047445, 6.969142054262312111E-17 ) ) ;
#10980 = CARTESIAN_POINT ( 'NONE',  ( 0.4527559055118117182, 0.07958543189024071263, -0.2665933059059888421 ) ) ;
#10981 = CARTESIAN_POINT ( 'NONE',  ( 1.043307086614173818, -0.5400638737290845981, -0.3530559997133363437 ) ) ;
#10982 = CARTESIAN_POINT ( 'NONE',  ( -0.4724409448818899238, 0.1265901696524986686, -0.8969816272965877024 ) ) ;
#10983 = CARTESIAN_POINT ( 'NONE',  ( 0.7677165354330716118, 0.07958543189024071263, -0.2665933059059888421 ) ) ;
#10984 = CARTESIAN_POINT ( 'NONE',  ( 0.6430446194225728496, 0.05413385826771666132, 0.4176697321401328100 ) ) ;
#10985 = CARTESIAN_POINT ( 'NONE',  ( -0.3949938075777408852, -0.1058382717557502933, -0.4376640419947507299 ) ) ;
#10986 = CARTESIAN_POINT ( 'NONE',  ( -0.8464566929133852113, -0.5400638737290845981, -0.3530559997133363437 ) ) ;
#10987 = CARTESIAN_POINT ( 'NONE',  ( -0.2165354330708654795, 0.1660481256975885056, 0.3530559997133364547 ) ) ;
#10988 = CARTESIAN_POINT ( 'NONE',  ( 1.056430446194226436, -0.5511811023622048555, -0.09757992244046775898 ) ) ;
#10989 = CARTESIAN_POINT ( 'NONE',  ( -0.6496062992125976043, -0.5400638737290844871, 0.3530559997133364547 ) ) ;
#10990 = CARTESIAN_POINT ( 'NONE',  ( 0.1640419947506569498, -0.05778040916215522460, 0.4822834645669289988 ) ) ;
#10991 = FACE_OUTER_BOUND ( 'NONE', #6110, .T. ) ;
#10993 = EDGE_CURVE ( 'NONE', #13510, #52467, #57990, .T. ) ;
#10992 = CARTESIAN_POINT ( 'NONE',  ( 0.03280839895013198948, 0.2952755905511811885, 0.1292274648535926551 ) ) ;
#10994 = CARTESIAN_POINT ( 'NONE',  ( -0.01968503937007793844, 0.07958543189024071263, -0.2665933059059888421 ) ) ;
#10995 = CARTESIAN_POINT ( 'NONE',  ( -2.846947862837596599, 1.092324130688937744, -0.1650676745531605427 ) ) ;
#10996 = CARTESIAN_POINT ( 'NONE',  ( 0.1246719160104994284, 0.1771653543307087075, -0.09757992244046823083 ) ) ;
#10997 = CARTESIAN_POINT ( 'NONE',  ( 0.9514435695538062676, -0.08942795157527998196, 0.3641732283464567121 ) ) ;
#10998 = LINE ( 'NONE', #36658, #47851 ) ;
#10999 = B_SPLINE_CURVE_WITH_KNOTS ( 'NONE', 3,
 ( #42780, #36474, #30158, #36891 ),
 .UNSPECIFIED., .F., .F.,
 ( 4, 4 ),
 ( 2.453269466693398698E-18, 0.002136818956423001525 ),
 .UNSPECIFIED. ) ;
#11000 = CARTESIAN_POINT ( 'NONE',  ( -0.2925321140481930149, -0.2925321140481933480, -1.710629921259842812 ) ) ;
#11001 = CARTESIAN_POINT ( 'NONE',  ( 0.1706036745406830368, -0.4281496062992127816, -0.4176697321401328100 ) ) ;
#11002 = EDGE_CURVE ( 'NONE', #4749, #26176, #76873, .T. ) ;
#11003 = CARTESIAN_POINT ( 'NONE',  ( -0.3917322834645670104, -7.196005306013484475E-17, -1.291338582677165503 ) ) ;
#11004 = CARTESIAN_POINT ( 'NONE',  ( 1.535433070866142558, 0.1771653543307087630, 0.000000000000000000 ) ) ;
#11005 = DIRECTION ( 'NONE',  ( 0.000000000000000000, 1.000000000000000000, 0.000000000000000000 ) ) ;
#11006 = CARTESIAN_POINT ( 'NONE',  ( -0.3674540682414692561, -0.5023911411419708095, -0.1820866141732282451 ) ) ;
#11007 = CARTESIAN_POINT ( 'NONE',  ( -0.5183727034120726440, 0.2952755905511811885, 0.1292274648535926551 ) ) ;
#11008 = CARTESIAN_POINT ( 'NONE',  ( 1.115485564304462551, -0.3690944881889765550, -0.3153832671262227771 ) ) ;
#11009 = CYLINDRICAL_SURFACE ( 'NONE', #5806, 0.4744094488188972947 ) ;
#11010 = CARTESIAN_POINT ( 'NONE',  ( 1.312335958005249825, 0.1283753931104746893, -0.1820866141732285504 ) ) ;
#11011 = CARTESIAN_POINT ( 'NONE',  ( -0.05905511811023545637, 0.1660481256975885056, 0.3530559997133364547 ) ) ;
#11012 = VECTOR ( 'NONE', #15265, 39.37007874015748143 ) ;
#11013 = CARTESIAN_POINT ( 'NONE',  ( 0.9711286089238851948, -0.6046776061558809534, -0.2411417322834644161 ) ) ;
#11014 = ADVANCED_FACE ( 'NONE', ( #38097 ), #76103, .T. ) ;
#11015 = CYLINDRICAL_SURFACE ( 'NONE', #35683, 0.4744094488188972947 ) ;
#11016 = CARTESIAN_POINT ( 'NONE',  ( 0.05905511811023681640, 0.1660481256975883668, -0.3530559997133364547 ) ) ;
#11017 = CARTESIAN_POINT ( 'NONE',  ( 1.502624671916010790, -0.05778040916215522460, 0.4822834645669289988 ) ) ;
#11018 = CARTESIAN_POINT ( 'NONE',  ( 0.4986876640419954376, -0.6046776061558809534, -0.2411417322834644161 ) ) ;
#11019 = EDGE_CURVE ( 'NONE', #55450, #32253, #69687, .T. ) ;
#11020 = CARTESIAN_POINT ( 'NONE',  ( -1.732283464566928277, -0.1870078740157479769, 0.3641732283464567677 ) ) ;
#11021 = CARTESIAN_POINT ( 'NONE',  ( 0.8464566929133866546, -0.4536011799217367080, 0.2665933059059888421 ) ) ;
#11022 = CARTESIAN_POINT ( 'NONE',  ( 1.187664041994751285, -0.05778040916215522460, 0.4822834645669289988 ) ) ;
#11023 = CARTESIAN_POINT ( 'NONE',  ( 0.1574803149606306130, -0.1870078740157479769, 0.3641732283464567677 ) ) ;
#11024 = CARTESIAN_POINT ( 'NONE',  ( -0.1181102362204717315, -0.6692913385826771977, 8.415575281601705876E-17 ) ) ;
#11025 = CARTESIAN_POINT ( 'NONE',  ( 0.5839895013123367340, -0.6692913385826773087, -0.1292274648535924053 ) ) ;
#11026 = PRODUCT_RELATED_PRODUCT_CATEGORY ( 'part', '', ( #25763 ) ) ;
#11027 = CARTESIAN_POINT ( 'NONE',  ( -0.6430446194225712953, 0.05413385826771626580, -0.4176697321401330321 ) ) ;
#11028 = CARTESIAN_POINT ( 'NONE',  ( -0.3280839895013117347, -0.3690944881889763329, 0.3153832671262228327 ) ) ;
#11029 = CARTESIAN_POINT ( 'NONE',  ( 0.6036745406824153282, -0.6046776061558807314, 0.2411417322834647770 ) ) ;
#11030 = CARTESIAN_POINT ( 'NONE',  ( 1.108923884514436686, -0.2845877964562161244, -0.3641732283464567121 ) ) ;
#11031 = CARTESIAN_POINT ( 'NONE',  ( 0.1443569553805781891, 0.05413385826771626580, -0.4176697321401330321 ) ) ;
#11032 = CARTESIAN_POINT ( 'NONE',  ( -1.519422763189357539, 0.000000000000000000, 0.7302211324797359682 ) ) ;
#11034 = DIRECTION ( 'NONE',  ( -1.000000000000000000, -0.000000000000000000, -0.000000000000000000 ) ) ;
#11033 = CARTESIAN_POINT ( 'NONE',  ( 0.000000000000000000, 2.677165354330708791, 0.000000000000000000 ) ) ;
#11035 = CARTESIAN_POINT ( 'NONE',  ( -0.3917322834645669549, -0.1049643490035306603, -2.242782152230970993 ) ) ;
#11036 = CARTESIAN_POINT ( 'NONE',  ( -1.043307086614172041, -0.5400638737290844871, 0.3530559997133364547 ) ) ;
#11037 = CARTESIAN_POINT ( 'NONE',  ( -0.4265091863517051496, 0.2952755905511810774, -0.1292274648535930714 ) ) ;
#11038 = CARTESIAN_POINT ( 'NONE',  ( -0.4724409448818895907, -0.1265901696524993070, -0.5183727034120735322 ) ) ;
#11039 = CARTESIAN_POINT ( 'NONE',  ( -0.3949938075777411628, 0.1058382717557497937, -2.867454068241469756 ) ) ;
#11040 = VERTEX_POINT ( 'NONE', #18748 ) ;
#11041 = CARTESIAN_POINT ( 'NONE',  ( 0.2034120734908144990, -0.5511811023622046335, 0.09757992244046803654 ) ) ;
#11042 = CARTESIAN_POINT ( 'NONE',  ( -0.1049643490035307020, 0.3917322834645669549, -1.258530183727033958 ) ) ;
#11043 = CARTESIAN_POINT ( 'NONE',  ( 0.7742782152230978099, -0.4281496062992124485, 0.4176697321401328655 ) ) ;
#11044 = CARTESIAN_POINT ( 'NONE',  ( -0.4091458600556402980, -0.2362204724409451284, -2.257217847769029007 ) ) ;
#11045 = DIRECTION ( 'NONE',  ( 9.381338752702735711E-17, -0.6427876096865389188, 0.7660444431189783465 ) ) ;
#11046 = ADVANCED_FACE ( 'NONE', ( #642 ), #77664, .F. ) ;
#11047 = CARTESIAN_POINT ( 'NONE',  ( -0.2821522309711278487, 0.2952755905511811885, 0.1292274648535926551 ) ) ;
#11048 = CARTESIAN_POINT ( 'NONE',  ( 1.089238845144357759, 0.05413385826771626580, -0.4176697321401330321 ) ) ;
#11049 = CARTESIAN_POINT ( 'NONE',  ( 1.463254593175853824, 0.1771653543307087075, -0.09757992244046823083 ) ) ;
#11050 = CARTESIAN_POINT ( 'NONE',  ( 0.01312335958005323398, -0.4281496062992127816, -0.4176697321401328100 ) ) ;
#11051 = CARTESIAN_POINT ( 'NONE',  ( -0.3917322834645670659, 0.1049643490035301607, -0.7427628364491322133 ) ) ;
#11052 = CARTESIAN_POINT ( 'NONE',  ( -0.4265091863517051496, -0.6692913385826771977, 0.1292274648535927661 ) ) ;
#11053 = CARTESIAN_POINT ( 'NONE',  ( -1.095800524934382292, -0.08942795157527998196, 0.3641732283464567121 ) ) ;
#11054 = CARTESIAN_POINT ( 'NONE',  ( 0.5183727034120741983, 0.2952755905511810774, -0.1292274648535930714 ) ) ;
#11055 = CARTESIAN_POINT ( 'NONE',  ( -0.5643044619422565855, 0.05413385826771626580, -0.4176697321401330321 ) ) ;
#11056 = CARTESIAN_POINT ( 'NONE',  ( 0.000000000000000000, 2.755905511811024056, 0.000000000000000000 ) ) ;
#11057 = CARTESIAN_POINT ( 'NONE',  ( -0.5314960629921325896, 2.755905511811024056, 1.895394334970790018 ) ) ;
#11058 = ORIENTED_EDGE ( 'NONE', *, *, #82624, .F. ) ;
#11059 = CARTESIAN_POINT ( 'NONE',  ( -0.3392501089628017219, -0.1958661417322836995, -1.938995693734595127 ) ) ;
#11060 = CARTESIAN_POINT ( 'NONE',  ( 0.2821522309711292364, 0.2952755905511810774, -0.1292274648535930714 ) ) ;
#11061 = CARTESIAN_POINT ( 'NONE',  ( -0.4855643044619415427, -0.4281496062992124485, 0.4176697321401328655 ) ) ;
#11062 = CARTESIAN_POINT ( 'NONE',  ( -1.437007874015747477, 0.1660481256975883668, -0.3530559997133364547 ) ) ;
#11063 = CARTESIAN_POINT ( 'NONE',  ( 1.128608923884514947, 0.2306618581243848609, 0.2411417322834645549 ) ) ;
#11064 = CARTESIAN_POINT ( 'NONE',  ( 0.4658792650918641698, -0.05778040916215560624, -0.4822834645669293319 ) ) ;
#11065 = CARTESIAN_POINT ( 'NONE',  ( 0.2867679344610365999, -0.2867679344610365444, -0.8129921259842518566 ) ) ;
#11066 = CARTESIAN_POINT ( 'NONE',  ( -0.9317585301837263412, 0.05413385826771666132, 0.4176697321401328100 ) ) ;
#11067 = CARTESIAN_POINT ( 'NONE',  ( 0.4133858267716541968, 0.1660481256975885056, 0.3530559997133364547 ) ) ;
#11068 = CARTESIAN_POINT ( 'NONE',  ( -0.4461942257217840213, -0.6046776061558809534, -0.2411417322834644161 ) ) ;
#11069 = CARTESIAN_POINT ( 'NONE',  ( 0.1574803149606306130, -0.1870078740157480601, -0.3641732283464567677 ) ) ;
#11070 = DIRECTION ( 'NONE',  ( 0.000000000000000000, 0.000000000000000000, 1.000000000000000000 ) ) ;
#11071 = CARTESIAN_POINT ( 'NONE',  ( -1.586052503253847501, 1.299212598425198095, -0.1653254495020571035 ) ) ;
#11072 = CARTESIAN_POINT ( 'NONE',  ( 0.1771653543307093182, 0.1660481256975885056, 0.3530559997133364547 ) ) ;
#11073 = AXIS2_PLACEMENT_3D ( 'NONE', #8142, #33807, #39276 ) ;
#11074 = DIRECTION ( 'NONE',  ( 0.000000000000000000, 1.000000000000000000, -0.000000000000000000 ) ) ;
#11075 = ADVANCED_FACE ( 'NONE', ( #25046 ), #24643, .F. ) ;
#11076 = CARTESIAN_POINT ( 'NONE',  ( -1.640419947506561060, 0.05413385826771666132, 0.4176697321401328100 ) ) ;
#11077 = CARTESIAN_POINT ( 'NONE',  ( 0.2867679344610365999, -0.2867679344610365444, -2.767716535433069946 ) ) ;
#11078 = ORIENTED_EDGE ( 'NONE', *, *, #15825, .T. ) ;
#11079 = VERTEX_POINT ( 'NONE', #19995 ) ;
#11080 = CARTESIAN_POINT ( 'NONE',  ( 0.5971128608923891301, 0.2952755905511810774, -0.1292274648535930714 ) ) ;
#11081 = CARTESIAN_POINT ( 'NONE',  ( 0.2296587926509192634, -0.08942795157528024563, -0.3641732283464568787 ) ) ;
#11083 = DIRECTION ( 'NONE',  ( 1.000000000000000000, 0.000000000000000000, 0.000000000000000000 ) ) ;
#11082 = DIRECTION ( 'NONE',  ( -1.734723475976806848E-16, -1.000000000000000000, 0.000000000000000000 ) ) ;
#11084 = CARTESIAN_POINT ( 'NONE',  ( -0.3917322834645669549, -0.1049643490035306603, -0.7604986876640419391 ) ) ;
#11085 = CARTESIAN_POINT ( 'NONE',  ( -0.4091458600556402980, -0.2362204724409451284, 0.1856955380577427484 ) ) ;
#11086 = CARTESIAN_POINT ( 'NONE',  ( 0.7186703366786207914, -1.374501131054255944E-15, 0.4445507791589066726 ) ) ;
#11087 = CARTESIAN_POINT ( 'NONE',  ( 0.2925321140481932369, -0.2925321140481931814, -2.537401574803149984 ) ) ;
#11088 =( REPRESENTATION_RELATIONSHIP ('NONE','NONE', #79348, #48103 ) REPRESENTATION_RELATIONSHIP_WITH_TRANSFORMATION ( #81810 )SHAPE_REPRESENTATION_RELATIONSHIP( ) );
#11089 = CARTESIAN_POINT ( 'NONE',  ( 0.4265091863517067039, -0.6692913385826773087, -0.1292274648535924053 ) ) ;
#11090 = CARTESIAN_POINT ( 'NONE',  ( -0.7217847769028863381, -0.4281496062992124485, 0.4176697321401328655 ) ) ;
#11091 = CARTESIAN_POINT ( 'NONE',  ( -1.351706036745406347, 0.05413385826771626580, -0.4176697321401330321 ) ) ;
#11092 = CARTESIAN_POINT ( 'NONE',  ( 0.5708661417322841158, -0.5400638737290845981, -0.3530559997133363437 ) ) ;
#11093 = CARTESIAN_POINT ( 'NONE',  ( 1.489501312335958172, -0.05778040916215560624, -0.4822834645669293319 ) ) ;
#11094 = CARTESIAN_POINT ( 'NONE',  ( 1.509186351706037543, -0.004921259842519576551, 0.3153832671262227771 ) ) ;
#11095 = CARTESIAN_POINT ( 'NONE',  ( 1.220472440944882608, 0.1771653543307087630, 0.000000000000000000 ) ) ;
#11096 = CARTESIAN_POINT ( 'NONE',  ( -0.9120734908136475250, -0.6692913385826773087, -0.1292274648535924053 ) ) ;
#11097 = CARTESIAN_POINT ( 'NONE',  ( -0.3460692066303960313, 0.1998031496062989965, -0.5754593175853018883 ) ) ;
#11098 = CARTESIAN_POINT ( 'NONE',  ( 1.423884514435696413, -0.3162353388693409650, -0.4822834645669289433 ) ) ;
#11099 = EDGE_CURVE ( 'NONE', #77311, #65182, #3522, .T. ) ;
#11100 = CARTESIAN_POINT ( 'NONE',  ( 0.3392501089628018884, -0.1958661417322834220, -0.2545931758530183275 ) ) ;
#11101 = CARTESIAN_POINT ( 'NONE',  ( -0.2821522309711278487, -0.6692913385826773087, -0.1292274648535924053 ) ) ;
#11102 = CLOSED_SHELL ( 'NONE', ( #12860, #62457, #37076, #46190, #70542, #41965, #35003, #70263, #56538, #66639, #63049, #23839, #69767, #81565, #42118, #17218, #44095, #74767, #49011, #23364, #46434, #43418, #39387, #3231, #53780, #27008, #73345, #62001, #43832, #63578, #52459, #12985, #49613, #55236, #37297, #48865, #6567, #23820, #42951, #74212, #51683, #19892, #54843, #48134, #20809, #1547, #60902, #223, #57898, #50514 ) ) ;
#11104 = CARTESIAN_POINT ( 'NONE',  ( -3.910251735077579838, 1.664246877830559024, -0.4582626050727204858 ) ) ;
#11103 = CARTESIAN_POINT ( 'NONE',  ( 1.187664041994751285, -0.05778040916215522460, 0.4822834645669289988 ) ) ;
#11105 = CARTESIAN_POINT ( 'NONE',  ( -1.030183727034119867, -0.08942795157528024563, -0.3641732283464568787 ) ) ;
#11106 = CARTESIAN_POINT ( 'NONE',  ( 0.5905511811023629321, 0.2952755905511811885, 0.000000000000000000 ) ) ;
#11107 = CARTESIAN_POINT ( 'NONE',  ( 0.9711286089238851948, 0.1283753931104748280, 0.1820866141732283561 ) ) ;
#11108 = CARTESIAN_POINT ( 'NONE',  ( 0.3917322834645668994, 0.1049643490035304522, -1.779508243273278945 ) ) ;
#11109 = CARTESIAN_POINT ( 'NONE',  ( -1.332020997375327642, -0.2845877964562161244, -0.3641732283464567121 ) ) ;
#11110 = CARTESIAN_POINT ( 'NONE',  ( 0.7611548556430454138, 0.2306618581243847221, -0.2411417322834647770 ) ) ;
#11111 = DIRECTION ( 'NONE',  ( 0.000000000000000000, 1.000000000000000000, 0.000000000000000000 ) ) ;
#11112 = CARTESIAN_POINT ( 'NONE',  ( -0.4658792650918627265, -0.08942795157527998196, 0.3641732283464567121 ) ) ;
#11113 = CARTESIAN_POINT ( 'NONE',  ( -0.01968503937007793844, -0.5400638737290844871, 0.3530559997133364547 ) ) ;
#11114 = CARTESIAN_POINT ( 'NONE',  ( -1.391076115485563314, -0.5023911411419708095, -0.1820866141732282451 ) ) ;
#11115 = CARTESIAN_POINT ( 'NONE',  ( -0.8267716535433065062, -0.6692913385826771977, 8.415575281601705876E-17 ) ) ;
#11116 = CARTESIAN_POINT ( 'NONE',  ( 1.397637795275591177, 0.1660481256975883668, -0.3530559997133364547 ) ) ;
#11117 = CARTESIAN_POINT ( 'NONE',  ( 0.1958661417322834775, 0.3392501089628018884, -0.6135363761492932388 ) ) ;
#11118 = CARTESIAN_POINT ( 'NONE',  ( -0.8267716535433065062, 0.1771653543307087630, 0.000000000000000000 ) ) ;
#11119 = CARTESIAN_POINT ( 'NONE',  ( 1.102321318565061548, 1.111600770690012840, 0.2114527220942730157 ) ) ;
#11120 = CARTESIAN_POINT ( 'NONE',  ( 1.502624671916010790, -0.3162353388693409650, -0.4822834645669289433 ) ) ;
#11121 = CARTESIAN_POINT ( 'NONE',  ( 0.4091458600556404646, -0.2362204724409448231, -2.229002624671915900 ) ) ;
#11122 = CARTESIAN_POINT ( 'NONE',  ( -1.312335958005248715, -0.6046776061558809534, -0.2411417322834644161 ) ) ;
#11123 = CARTESIAN_POINT ( 'NONE',  ( -1.627296587926508442, 0.1283753931104748280, 0.1820866141732283561 ) ) ;
#11124 = CARTESIAN_POINT ( 'NONE',  ( -0.7611548556430438595, 0.1283753931104748280, 0.1820866141732283561 ) ) ;
#11125 = CARTESIAN_POINT ( 'NONE',  ( -0.4848604877838266214, -2.609869883881465018E-15, -0.3464511005275220379 ) ) ;
#11126 = CARTESIAN_POINT ( 'NONE',  ( -0.05905511811023545637, 0.1660481256975885056, 0.3530559997133364547 ) ) ;
#11127 = CARTESIAN_POINT ( 'NONE',  ( -0.09186351706036663400, -0.3690944881889763329, 0.3153832671262228327 ) ) ;
#11128 = CARTESIAN_POINT ( 'NONE',  ( -1.351706036745406347, -0.004921259842519870586, -0.3153832671262229437 ) ) ;
#11129 = CARTESIAN_POINT ( 'NONE',  ( -1.673228346456691717, 0.1660481256975883668, -0.3530559997133364547 ) ) ;
#11130 = CARTESIAN_POINT ( 'NONE',  ( 1.240157480314961314, -0.4536011799217367080, 0.2665933059059888421 ) ) ;
#11131 = AXIS2_PLACEMENT_3D ( 'NONE', #46278, #63567, #31574 ) ;
#11132 = CARTESIAN_POINT ( 'NONE',  ( 1.141732283464567788, -0.6692913385826771977, 8.415575281601705876E-17 ) ) ;
#11133 = CARTESIAN_POINT ( 'NONE',  ( 0.1807843743677491344, 1.098495470880705538, 1.883124800463723991 ) ) ;
#11134 = CARTESIAN_POINT ( 'NONE',  ( 0.4724409448818904789, -0.1870078740157480601, -0.3641732283464567677 ) ) ;
#11135 = CARTESIAN_POINT ( 'NONE',  ( 1.049868766404200349, 0.2306618581243848609, 0.2411417322834645549 ) ) ;
#11136 = CARTESIAN_POINT ( 'NONE',  ( 0.9776902887139113929, 0.1771653543307087630, 0.09757992244046791164 ) ) ;
#11137 = ORIENTED_EDGE ( 'NONE', *, *, #76918, .T. ) ;
#11138 = CARTESIAN_POINT ( 'NONE',  ( -1.364829396325458521, -0.6046776061558807314, 0.2411417322834647770 ) ) ;
#11139 = CARTESIAN_POINT ( 'NONE',  ( -1.102362204724408601, -0.1870078740157480879, -0.4822834645669291653 ) ) ;
#11140 = CARTESIAN_POINT ( 'NONE',  ( -0.2690288713910754526, 0.2952755905511810774, -0.1292274648535930714 ) ) ;
#11141 = CARTESIAN_POINT ( 'NONE',  ( -0.3996062992125985480, -0.1070741851644057135, -0.04593175853018374027 ) ) ;
#11142 = CARTESIAN_POINT ( 'NONE',  ( 0.3996062992125985480, 2.446882876249141654E-17, -2.714566929133858331 ) ) ;
#11143 = CARTESIAN_POINT ( 'NONE',  ( 0.2559055118110243332, -0.5400638737290845981, -0.3530559997133363437 ) ) ;
#11144 = CARTESIAN_POINT ( 'NONE',  ( 1.469816272965879911, 0.1283753931104746893, -0.1820866141732285504 ) ) ;
#11145 = CARTESIAN_POINT ( 'NONE',  ( -0.05249343832020911260, 0.2306618581243848609, 0.2411417322834645549 ) ) ;
#11146 = CARTESIAN_POINT ( 'NONE',  ( 0.7217847769028878924, -0.4281496062992127816, -0.4176697321401328100 ) ) ;
#11147 = EDGE_CURVE ( 'NONE', #58782, #51415, #50310, .T. ) ;
#11148 = CARTESIAN_POINT ( 'NONE',  ( -0.1070741851644051862, -0.3996062992125987146, -1.961942257217847763 ) ) ;
#11149 = CARTESIAN_POINT ( 'NONE',  ( 0.3949938075777411073, -0.1058382717557499464, -1.371391076115485719 ) ) ;
#11150 = CARTESIAN_POINT ( 'NONE',  ( -0.4744094488189006809, 1.506132068098321675, 1.016821367227982220 ) ) ;
#11151 = CARTESIAN_POINT ( 'NONE',  ( 3.912088859918621431, 1.709704544164725615, 0.4423030945488138355 ) ) ;
#11152 = CARTESIAN_POINT ( 'NONE',  ( -0.1958661417322836718, 0.3392501089628017219, -0.7926509186351704539 ) ) ;
#11153 = EDGE_CURVE ( 'NONE', #73823, #76967, #38465, .T. ) ;
#11154 = CARTESIAN_POINT ( 'NONE',  ( -0.6430446194225716283, -0.3690944881889763329, 0.3153832671262228327 ) ) ;
#11155 = CARTESIAN_POINT ( 'NONE',  ( -0.6758530183727028406, -0.6692913385826773087, -0.1292274648535924053 ) ) ;
#11156 = CARTESIAN_POINT ( 'NONE',  ( 0.4133858267716541968, -0.5400638737290845981, -0.3530559997133363437 ) ) ;
#11157 = CARTESIAN_POINT ( 'NONE',  ( -0.3949938075777411073, 0.1058382717557497660, -2.786745406824147064 ) ) ;
#11158 = CARTESIAN_POINT ( 'NONE',  ( 0.8005249343832028242, -0.4281496062992127816, -0.4176697321401328100 ) ) ;
#11159 = CARTESIAN_POINT ( 'NONE',  ( 1.509186351706037543, -0.4281496062992127816, -0.4176697321401328100 ) ) ;
#11160 = CARTESIAN_POINT ( 'NONE',  ( 1.266404199475066328, -0.05778040916215522460, 0.4822834645669289988 ) ) ;
#11161 = CARTESIAN_POINT ( 'NONE',  ( 0.4091458600556403535, 0.2362204724409449896, -2.335958005249343827 ) ) ;
#11162 = CARTESIAN_POINT ( 'NONE',  ( -0.3996062992125986035, -0.1070741851644056997, -2.250656167979002920 ) ) ;
#11163 = DIRECTION ( 'NONE',  ( 0.000000000000000000, 0.000000000000000000, 1.000000000000000000 ) ) ;
#11164 = CARTESIAN_POINT ( 'NONE',  ( 0.9055118110236227702, -0.6692913385826771977, 8.415575281601705876E-17 ) ) ;
#11165 = CARTESIAN_POINT ( 'NONE',  ( 0.4855643044619428750, 0.05413385826771666132, 0.4176697321401328100 ) ) ;
#11166 = CARTESIAN_POINT ( 'NONE',  ( 1.305774278215223960, 0.1771653543307087075, -0.09757992244046823083 ) ) ;
#11168 = CARTESIAN_POINT ( 'NONE',  ( 1.528871391076116026, -0.6692913385826773087, -0.1292274648535924053 ) ) ;
#11167 = CARTESIAN_POINT ( 'NONE',  ( 1.581364829396326277, -0.3162353388693409650, -0.4822834645669289433 ) ) ;
#11169 = CARTESIAN_POINT ( 'NONE',  ( -0.3917322834645668994, -0.1049643490035306742, -2.803130290517373613 ) ) ;
#11170 = PLANE ( 'NONE',  #81642 ) ;
#11171 = CARTESIAN_POINT ( 'NONE',  ( 0.7283464566929143125, 0.1660481256975885056, 0.3530559997133364547 ) ) ;
#11172 = AXIS2_PLACEMENT_3D ( 'NONE', #35556, #28823, #62056 ) ;
#11173 = CARTESIAN_POINT ( 'NONE',  ( 1.535433070866142558, 0.1771653543307087630, 0.000000000000000000 ) ) ;
#11174 = CARTESIAN_POINT ( 'NONE',  ( -0.6233595800524928121, -0.05778040916215522460, 0.4822834645669289988 ) ) ;
#11175 = CARTESIAN_POINT ( 'NONE',  ( -0.6233595800524928121, -0.05778040916215522460, 0.4822834645669289988 ) ) ;
#11176 = CARTESIAN_POINT ( 'NONE',  ( 1.568241469816273437, -0.3162353388693405765, 0.4822834645669290543 ) ) ;
#11177 = CARTESIAN_POINT ( 'NONE',  ( -0.2867679344610364334, -0.2867679344610367109, -0.3011811023622048000 ) ) ;
#11178 = CARTESIAN_POINT ( 'NONE',  ( 0.1958661417322834775, 0.3392501089628018884, -1.711286089238845287 ) ) ;
#11179 = CARTESIAN_POINT ( 'NONE',  ( -0.3917322834645671215, 0.1049643490035301469, -2.229658792650918819 ) ) ;
#11180 = CARTESIAN_POINT ( 'NONE',  ( -1.653543307086613234, -0.1870078740157479769, 0.3641732283464567677 ) ) ;
#11181 = VERTEX_POINT ( 'NONE', #26299 ) ;
#11182 = CARTESIAN_POINT ( 'NONE',  ( 0.2891555358219910499, 0.2891555358219910499, -2.814960629921259727 ) ) ;
#11183 = ORIENTED_EDGE ( 'NONE', *, *, #80420, .F. ) ;
#11184 = CARTESIAN_POINT ( 'NONE',  ( -1.586052503253847057, 1.574803149606300412, -0.1653254495020572423 ) ) ;
#11185 = CARTESIAN_POINT ( 'NONE',  ( 1.476377952755906220, 0.07958543189024071263, -0.2665933059059888421 ) ) ;
#11186 = CARTESIAN_POINT ( 'NONE',  ( -9.787531504996567848E-17, 0.3996062992125986035, -0.9448818897637796255 ) ) ;
#11187 = FACE_OUTER_BOUND ( 'NONE', #67586, .T. ) ;
#11188 = CARTESIAN_POINT ( 'NONE',  ( 0.000000000000000000, 0.5905511811023621549, -0.1937007874015747588 ) ) ;
#11189 = CARTESIAN_POINT ( 'NONE',  ( 0.4531182788721078158, 1.535433070866141447, 0.5309055118110234117 ) ) ;
#11190 = CARTESIAN_POINT ( 'NONE',  ( -0.2493074132419488831, 1.884549279140503408, 0.1897364805620621597 ) ) ;
#11191 = CARTESIAN_POINT ( 'NONE',  ( 0.1049643490035303689, 0.3917322834645670104, -0.5505249343832020470 ) ) ;
#11192 =( BOUNDED_SURFACE ( )  B_SPLINE_SURFACE ( 3, 2, ( 
 ( #54341, #80051, #23184, #42539, #53923, #21953, #29502, #22370, #3427, #42129, #48854, #10576, #2603, #67824, #16900, #10162, #36233, #35828, #61903, #29907, #15655, #9741, #48029, #47196, #61077, #40896, #66577, #8912, #55162, #47611, #74138, #3842, #73730, #41714, #28261, #29090, #80872, #55571, #34587, #73307, #35412, #34999, #74555, #21536, #54760, #28680, #4244, #16068, #66997, #15236, #9329, #60665, #80466, #22776, #74968, #75369, #56404, #6299, #69046, #63962, #24010, #30320, #50491, #31975, #4649, #5884, #17314, #37467, #70273, #76194, #31141, #44580, #56808, #38286, #81279, #5072, #82103, #75782, #11812, #18531, #23595, #37876, #50901, #63140, #49266, #49678, #69462, #36636, #55988, #24416, #12627, #62312, #81699, #17716, #43344, #82507, #24823, #44174, #57214, #11395, #30741, #69867, #18124, #42942, #37052, #62734, #68637, #10976, #50086, #82916, #43756, #5480, #63550, #12219, #31557, #25236, #76601, #18932, #7568, #39542, #46683, #46262, #20186, #27326, #1669, #65657, #58050, #39970, #33240, #13883, #65230, #32387, #39117, #38702, #416, #26072, #8397, #7986, #71535, #64798, #77433, #52986, #58902, #7137, #26499, #1262, #52151, #72376, #77015, #21022, #14725, #78699, #40378, #20610, #51731, #32810, #19347, #44997, #19768, #26910, #45837, #841, #58477, #14310, #25650, #66061, #71957, #77857, #71117, #57635, #51312, #70696, #13049, #52570, #45421, #33650, #16834, #64381, #78278, #6717, #13460, #59313, #60972, #66899, #23084, #54654, #40789, #72783, #53818, #2082, #35310, #27747, #79120, #48751, #3323, #21437, #42026, #10056, #67720, #74450, #79532, #28987, #35719, #60151, #34902, #3738, #61389, #80364, #54235, #34064, #22677, #73628, #53411, #47093, #66474, #16796, #9641, #42433, #15133, #8809, #2503, #48336, #68133, #74033, #9229, #2915, #67306, #28578, #59727, #34485, #80769, #28162, #29402, #21846, #16380, #47510, #41211, #73202, #15552, #60564, #55061, #22265, #79952, #47923, #15970, #41617, #57119, #24730, #30643, #23914, #25137, #4144, #61804, #29809, #82005, #62215, #18439, #76507, #17212, #17618, #18836, #30223, #75275, #37374, #43249, #82813, #31044, #42845, #49163, #55886, #55470, #11718, #81180, #23497, #50806, #63044, #74869, #44081, #69774, #12118, #44481, #81597, #5383, #37776, #36539, #11297, #63451, #5787, #56712, #56308, #10478, #82411, #49989, #68538, #10878, #4553, #36131, #69364, #49579, #68947, #36956, #62633, #50398, #4977, #76095, #43662, #31457, #24319, #75687, #18028, #45739, #7037, #70172, #44892, #25548, #6198, #22054, #19241, #47298, #83227, #32287, #52469, #6616, #76911, #65127, #66686, #26811, #20089, #52051, #60357, #58802, #32707, #41003, #15341, #78177, #70591, #21638, #71435, #26393, #77756, #12945, #51627, #51215, #38603, #64281, #12525, #72987, #736, #77331, #57947, #9021, #314, #19660, #13782, #45322, #2704, #7462, #25968, #71017, #13361, #38186, #39439, #63861, #31876, #28364, #33132, #57536, #34694, #54026, #79737, #39014, #64698, #1160, #58373, #73832, #48546, #17418, #75071, #48962, #67926, #47716, #74662, #3947, #41415, #15763, #54445, #62421, #23291, #30434, #67099, #60766, #16172, #17006, #81803, #42646, #80979, #68343, #23704, #28783, #80572, #10683, #10267, #73414, #22474, #3116, #9430, #35099, #80157, #49375, #48135, #9844, #30016, #67508, #41817, #36338, #43049, #4349, #62012, #29608, #36744, #55680, #35935, #68745, #11087, #81388, #35516, #4758, #56099, #55268, #61179, #3533, #29200, #54866, #22882, #74244, #16586, #42232, #61603, #31252, #43871, #19460, #83024, #56919, #76307, #57330, #18638, #13165, #43458, #70816, #64493, #45110, #38815, #70384, #82210, #82614, #69156, #11507, #69570, #25347, #12326, #50600, #5585, #64078, #75485, #6831, #38399, #44282, #37573, #32500, #17825, #37163, #62843, #37984, #75892, #32085 ),
 ( #76708, #58164, #30843, #57746, #5179, #63659, #24115, #19041, #51009, #49784, #44688, #56508, #24529, #24930, #69972, #6000, #31669, #12740, #50194, #6416, #77126, #108, #18232, #11918, #25762, #63246, #51424, #59016, #72897, #64916, #58591, #26614, #52267, #32926, #7253, #959, #14834, #65766, #1780, #72485, #77972, #20302, #66173, #46375, #46794, #27439, #45951, #71649, #14000, #40494, #40079, #72068, #39658, #59843, #65348, #52684, #1372, #53101, #7685, #78810, #39231, #33353, #53523, #21139, #2195, #77554, #27023, #78392, #27863, #21546, #20723, #14427, #8512, #8098, #33763, #34178, #79231, #47207, #59424, #15248, #40907, #66589, #8924, #34601, #532, #26186, #51847, #19887, #45535, #71233, #13577, #79646, #21963, #47623, #10587, #3023, #29512, #3852, #35422, #80476, #41326, #16495, #36244, #10985, #73319, #15665, #48448, #73742, #55173, #68647, #42139, #41723, #16911, #67417, #35011, #17324, #60266, #80882, #22788, #68252, #42953, #67007, #9750, #2616, #80063, #61087, #23195, #3438, #49276, #48866, #9340, #60675, #22381, #28272, #61506, #53934, #28690, #74979, #74565, #54351, #61913, #4255, #29918, #48040, #16078, #42549, #55581, #29101, #54772, #81292, #23607, #74148, #67834, #10173, #35838, #76205, #30332, #4658, #43356, #51325, #12231, #19361, #55998, #49687, #62747, #63564, #70710, #37888, #69878, #57227, #12639, #17728, #69472, #5898, #56819, #36646, #11405, #75380, #81709, #62321, #69056, #38299, #37062, #82113, #18944, #56414, #5082, #31570, #31988, #76614, #82928, #18543, #25664, #25249, #82517, #6311, #63975, #44592, #30751, #70287, #50914, #44187, #57648, #24427, #18134, #50096, #75792, #43767, #24019, #11, #50502, #11825, #37478, #77029, #45010, #63150, #5491, #31152, #24833, #2095, #32400, #59741, #53425, #8410, #27760, #59326, #71130, #20199, #58063, #430, #58490, #71971, #1275, #39556, #77870, #52999, #64394, #79133, #27341, #33254, #26512, #21450, #6730, #26085, #51745, #26923, #64811, #47107, #77448, #19782, #52583, #52166, #65673, #13062, #78292, #45850, #78712, #71549, #13473, #38716, #45435, #39983, #58916, #39130, #7152, #32823, #13898, #855, #65244, #7582, #20624, #46275, #8000, #14325, #33663, #21037, #1682, #46696, #72389, #14739, #40391, #66074, #34078, #29823, #81196, #79966, #47939, #67321, #3337, #10070, #23511, #29415, #42448, #29001, #72796, #15565, #60988, #28175, #47524, #73642, #61818, #53832, #73215, #41225, #66912, #21859, #79546, #9243, #3751, #54667, #74047, #61402, #34916, #60578, #55074, #35325, #35734, #16395, #2929, #28593, #54250, #80782, #80378, #22691, #22279, #48766, #15984, #41631, #9655, #42041, #48350, #67737, #23098, #74465, #68148, #16812, #10492, #66487, #36146, #4158, #55485, #15146, #40803, #8822, #34499, #60164, #2517, #69789, #50822, #70189, #30239, #44096, #44499, #37791, #63876, #12135, #6215, #57552, #43264, #11733, #24334, #74883, #5397, #68552, #10893, #36553, #82832, #75289, #18453, #76112, #50004, #69379, #55902, #31060, #25154, #81614, #17632, #11311, #63469, #56728, #37388, #68961, #76524, #30659, #18043, #75701, #5803, #56322, #31474, #4568, #36970, #18852, #50412, #12543, #42859, #82021, #43676, #38202, #31891, #23928, #49595, #57135, #63060, #82425, #83243, #49180, #17228, #62650, #62229, #4991, #24745, #40295, #71874, #65976, #33980, #19679, #71451, #752, #51231, #65145, #44910, #70607, #12962, #59227, #51644, #78194, #52486, #26413, #45755, #6631, #7481, #1588, #59641, #38619, #64297, #13799, #39031, #20525, #25565, #33151, #7056, #65570, #32724, #331, #8313, #76930, #46177, #39457, #32303, #19257, #45338, #52066, #57964, #13378, #25985, #77348, #71034, #14223, #64715, #58392, #33565, #77773, #58820, #14639, #39883, #1177, #72293, #26828, #20105, #7904, #27243, #52902, #78616, #20939, #46597 ),
 ( #22182, #1998, #60065, #40704, #21354, #36051, #34397, #61300, #15048, #47424, #67637, #21761, #8727, #80282, #66815, #28905, #34820, #74366, #22595, #2419, #66388, #73115, #53326, #3240, #79035, #47007, #16709, #54567, #72701, #9968, #3658, #35640, #42350, #15467, #48256, #29321, #28076, #2829, #54982, #80690, #73952, #47839, #27660, #16298, #41537, #53734, #79442, #41124, #68048, #60890, #10395, #9148, #60478, #28490, #41941, #54150, #23003, #35226, #48669, #79864, #73545, #15888, #67224, #9556, #61724, #36457, #17131, #81096, #12440, #10797, #37690, #74780, #23830, #43996, #81508, #68459, #56627, #57035, #18353, #11627, #43579, #50724, #50313, #24234, #31370, #5699, #69690, #62131, #12033, #37288, #17943, #69281, #4471, #43167, #42763, #30139, #55802, #4061, #63365, #75604, #68863, #49498, #82730, #62963, #11212, #30559, #5301, #56225, #76422, #23413, #25049, #18751, #44395, #70087, #24646, #75191, #36871, #49080, #17535, #62549, #30960, #49906, #4885, #81923, #29728, #55390, #82327, #76011, #58280, #51540, #52799, #31787, #6115, #57450, #26302, #6534, #46069, #20832, #44806, #45232, #46485, #57861, #13278, #27135, #19155, #12859, #64200, #32204, #70501, #38517, #228, #52377, #19998, #39345, #26723, #25878, #77243, #20417, #645, #1070, #65031, #19573, #70933, #38930, #78085, #77667, #51961, #64610, #14115, #6947, #32618, #45649, #7366, #71344, #33036, #76823, #13691, #7796, #58704, #39768, #83142, #71762, #65463, #33462, #59124, #1481, #78509, #72180, #38100, #63774, #25462, #51129, #35534, #78924, #9447, #9864, #3136, #29218, #60784, #54885, #22897, #8623, #60374, #73007, #40189, #54043, #33873, #59537, #1894, #48155, #40601, #67116, #41433, #15359, #34713, #21246, #79756, #73850, #48565, #27554, #53213, #2722, #27971, #35118, #14538, #22074, #79337, #54464, #21657, #72595, #80590, #65873, #28800, #28383, #46901, #8208, #34294, #41020, #14942, #2310, #66283, #59955, #53629, #80177, #47317, #66706, #22492, #9039, #47733, #3553, #16190, #73431, #61196, #15781, #41837, #67527, #81407, #49395, #68764, #4777, #12651, #442, #32001, #45022, #30453, #74263, #17025, #62440, #29627, #48980, #42249, #10286, #56117, #42664, #23, #58076, #80997, #23724, #26097, #10701, #55699, #17843, #75089, #64407, #38312, #23310, #55287, #36356, #67944, #75504, #35953, #61622, #6742, #44603, #3964, #25676, #51336, #77040, #32414, #62032, #70299, #19372, #68363, #17437, #70723, #13076, #63987, #11108, #16605, #6326, #81823, #74679, #4368, #30036, #43067, #49803, #36764, #24133, #57660, #38730, #78724, #2528, #53011, #1694, #72401, #27772, #32835, #1286, #27352, #71982, #51757, #26525, #7164, #71144, #77460, #867, #53436, #64826, #13911, #34089, #71561, #58503, #46709, #47119, #8421, #21049, #33675, #40815, #40404, #14336, #21461, #79144, #59752, #52179, #2106, #14750, #8011, #59337, #77882, #33268, #20214, #45863, #39568, #19798, #72808, #65684, #58927, #65257, #15157, #66085, #26935, #20635, #66499, #46287, #8833, #13486, #34510, #60175, #45447, #39142, #7594, #52597, #78303, #39996, #47535, #79976, #16405, #54678, #9666, #73653, #29426, #53844, #10502, #55084, #3347, #22289, #61829, #79557, #28603, #67333, #29833, #47950, #4169, #2939, #9255, #10081, #55496, #66923, #80793, #21870, #80390, #36156, #35744, #74059, #28186, #61412, #73226, #15577, #29012, #22701, #42051, #3762, #48776, #41235, #34927, #60589, #23110, #54260, #67747, #42458, #48360, #74475, #16822, #15995, #68158, #41642, #35335, #60999, #52441, #26785, #78152, #34359, #1958, #21314, #8689, #20483, #46137, #2380, #65937, #66350, #46967, #71832, #14181, #65528, #60025, #59603, #8273, #39839, #79404, #1546, #72251, #20900, #72661, #27200, #15009, #58773, #7860, #73077, #40666, #21723, #13758, #52864, #78574, #47386, #41087 ),
 ( #28037, #60441, #28452, #33525, #33938, #46553, #45714, #27620, #39415, #65099, #7436, #53695, #59188, #15426, #66776, #14600, #40254, #1135, #53283, #9109, #54112, #33106, #78994, #34782, #2793, #20061, #71411, #36017, #61264, #36424, #3618, #54529, #36837, #79827, #23378, #42314, #41502, #73505, #3204, #80244, #10764, #61688, #81062, #68424, #28867, #22560, #62097, #68013, #42728, #49046, #48222, #73918, #41905, #4439, #4029, #10357, #16259, #55767, #29284, #48633, #80654, #74743, #54948, #17093, #35190, #67599, #49463, #30105, #81474, #15853, #22967, #74328, #23791, #17502, #9930, #35602, #75157, #16675, #29694, #43134, #68830, #11177, #60851, #62510, #4848, #30523, #22144, #47801, #67187, #9518, #55356, #18720, #31335, #81888, #12408, #75569, #17910, #43546, #6500, #82293, #25429, #83110, #57000, #76387, #37253, #38066, #32170, #6915, #69246, #11593, #44362, #69655, #51094, #64577, #63742, #37653, #12826, #63331, #30926, #13249, #56185, #76792, #70054, #62928, #49870, #50279, #82697, #24199, #43959, #38898, #24612, #5262, #19123, #56593, #75977, #64167, #18317, #6081, #45196, #44772, #31755, #19539, #57417, #11999, #5668, #25016, #50689, #70469, #38483, #57826, #194, #25846, #51506, #77210, #70899, #63589, #38327, #5924, #50940, #6342, #11435, #63177, #31596, #50528, #30359, #5110, #64420, #62776, #32014, #43386, #75821, #12667, #50122, #37090, #25273, #25689, #70312, #57253, #12255, #19386, #18968, #76234, #36, #57674, #64000, #30777, #51350, #82955, #69901, #37912, #56438, #11849, #82141, #24456, #18163, #56028, #77053, #44211, #37502, #43795, #45038, #76637, #5515, #82543, #44617, #24861, #70738, #49716, #13091, #38744, #81736, #24045, #75412, #69500, #31180, #17756, #69087, #56845, #18568, #78319, #33282, #71575, #46722, #58090, #53450, #21062, #26950, #20229, #21475, #455, #26111, #51772, #20650, #58518, #14763, #72824, #13499, #13926, #15174, #26541, #39583, #33690, #65272, #79158, #27365, #39155, #45461, #52194, #77476, #8027, #19812, #71159, #47133, #59351, #64840, #40419, #66100, #8436, #40831, #77898, #1710, #34106, #32849, #7609, #59767, #2122, #53026, #52613, #6755, #78739, #46303, #7178, #882, #45877, #32427, #65697, #58943, #1301, #71997, #14351, #40010, #72414, #27788, #16421, #3779, #42472, #47551, #16010, #42067, #3364, #66516, #41251, #21887, #2542, #29442, #10098, #73243, #9270, #28618, #55101, #22717, #29028, #34941, #68175, #47967, #35351, #67347, #35762, #73668, #61430, #15592, #60604, #36170, #67762, #10516, #60191, #41656, #9680, #61843, #4184, #66938, #2953, #74491, #61013, #48376, #80810, #29847, #55510, #54276, #23125, #81218, #48793, #23534, #16838, #49203, #74905, #79992, #54697, #80405, #8848, #74075, #28200, #53859, #79571, #17253, #22306, #34526, #69810, #18065, #63083, #23948, #82450, #76546, #76955, #4589, #62253, #31083, #56344, #12159, #51253, #24765, #24358, #82857, #50028, #17657, #83267, #42881, #37815, #5421, #30260, #36574, #36993, #55924, #81639, #49616, #50846, #18874, #44523, #31914, #5014, #63491, #70211, #68985, #43699, #12567, #38225, #44118, #56750, #68576, #5825, #50433, #75310, #10917, #43288, #57576, #18476, #25590, #11334, #62673, #30683, #82045, #76135, #63902, #31498, #57157, #6238, #75725, #69403, #25178, #11756, #37411, #77373, #57991, #38643, #53352, #51670, #78641, #32329, #64741, #1611, #39058, #19283, #46204, #58844, #12988, #70631, #26012, #34006, #78219, #2023, #64321, #355, #7079, #32750, #52511, #27267, #20552, #39908, #20964, #19705, #52090, #71898, #39484, #44934, #45363, #71059, #6656, #13403, #58417, #46623, #776, #26438, #52928, #77799, #20131, #14249, #14665, #59254, #65595, #1202, #8340, #7928, #65171, #72319, #40323, #66001, #45779, #59668, #33589, #26852, #27687, #71478, #13825, #7507, #33176 ) ),
 .UNSPECIFIED., .F., .F., .F. ) 
 B_SPLINE_SURFACE_WITH_KNOTS ( ( 4, 4 ),
 ( 3, 2, 2, 2, 2, 2, 2, 2, 2, 2, 2, 2, 2, 2, 2, 2, 2, 2, 2, 2, 2, 2, 2, 2, 2, 2, 2, 2, 2, 2, 2, 2, 2, 2, 2, 2, 2, 2, 2, 2, 2, 2, 2, 2, 2, 2, 2, 2, 2, 2, 2, 2, 2, 2, 2, 2, 2, 2, 2, 2, 2, 2, 2, 2, 2, 2, 2, 2, 2, 2, 2, 2, 2, 2, 2, 2, 2, 2, 2, 2, 2, 2, 2, 2, 2, 2, 2, 2, 2, 2, 2, 2, 2, 2, 2, 2, 2, 2, 2, 2, 2, 2, 2, 2, 2, 2, 2, 2, 2, 2, 2, 2, 2, 2, 2, 2, 2, 2, 2, 2, 2, 2, 2, 2, 2, 2, 2, 2, 2, 2, 2, 2, 2, 2, 2, 2, 2, 2, 2, 2, 2, 2, 2, 2, 2, 2, 2, 2, 2, 2, 2, 2, 2, 2, 2, 2, 2, 2, 2, 2, 2, 2, 2, 2, 2, 2, 2, 2, 2, 2, 2, 2, 2, 2, 2, 2, 2, 2, 2, 2, 2, 2, 2, 2, 2, 2, 2, 2, 2, 2, 2, 2, 2, 2, 2, 2, 2, 2, 2, 2, 2, 2, 2, 2, 2, 2, 2, 2, 2, 2, 2, 2, 2, 2, 2, 2, 2, 2, 2, 2, 2, 2, 2, 2, 2, 2, 2, 2, 2, 2, 2, 2, 2, 2, 2, 2, 2, 3 ),
 ( 0.000000000000000000, 1.000000000000000000 ),
 ( 0.000000000000000000, 0.004166666666666666609, 0.008333333333333333218, 0.01250000000000000069, 0.01666666666666666644, 0.02083333333333333218, 0.02500000000000000139, 0.02916666666666666713, 0.03333333333333333287, 0.03749999999999999861, 0.04166666666666666435, 0.04583333333333333010, 0.05000000000000000278, 0.05416666666666666852, 0.05833333333333333426, 0.06250000000000000000, 0.06666666666666666574, 0.07083333333333333148, 0.07499999999999999722, 0.07916666666666666297, 0.08333333333333332871, 0.08749999999999999445, 0.09166666666666666019, 0.09583333333333333981, 0.1000000000000000056, 0.1041666666666666713, 0.1083333333333333370, 0.1125000000000000028, 0.1166666666666666685, 0.1208333333333333343, 0.1250000000000000000, 0.1291666666666666796, 0.1333333333333333315, 0.1375000000000000111, 0.1416666666666666630, 0.1458333333333333426, 0.1499999999999999944, 0.1541666666666666741, 0.1583333333333333259, 0.1625000000000000056, 0.1666666666666666574, 0.1708333333333333370, 0.1749999999999999889, 0.1791666666666666685, 0.1833333333333333204, 0.1875000000000000000, 0.1916666666666666796, 0.1958333333333333315, 0.2000000000000000111, 0.2041666666666666630, 0.2083333333333333426, 0.2124999999999999944, 0.2166666666666666741, 0.2208333333333333259, 0.2250000000000000056, 0.2291666666666666574, 0.2333333333333333370, 0.2374999999999999889, 0.2416666666666666685, 0.2458333333333333204, 0.2500000000000000000, 0.2541666666666666519, 0.2583333333333333592, 0.2625000000000000111, 0.2666666666666666630, 0.2708333333333333148, 0.2750000000000000222, 0.2791666666666666741, 0.2833333333333333259, 0.2874999999999999778, 0.2916666666666666852, 0.2958333333333333370, 0.2999999999999999889, 0.3041666666666666408, 0.3083333333333333481, 0.3125000000000000000, 0.3166666666666666519, 0.3208333333333333592, 0.3250000000000000111, 0.3291666666666666630, 0.3333333333333333148, 0.3375000000000000222, 0.3416666666666666741, 0.3458333333333333259, 0.3499999999999999778, 0.3541666666666666852, 0.3583333333333333370, 0.3624999999999999889, 0.3666666666666666408, 0.3708333333333333481, 0.3750000000000000000, 0.3791666666666666519, 0.3833333333333333592, 0.3875000000000000111, 0.3916666666666666630, 0.3958333333333333148, 0.4000000000000000222, 0.4041666666666666741, 0.4083333333333333259, 0.4124999999999999778, 0.4166666666666666852, 0.4208333333333333370, 0.4249999999999999889, 0.4291666666666666408, 0.4333333333333333481, 0.4375000000000000000, 0.4416666666666666519, 0.4458333333333333592, 0.4500000000000000111, 0.4541666666666666630, 0.4583333333333333148, 0.4625000000000000222, 0.4666666666666666741, 0.4708333333333333259, 0.4749999999999999778, 0.4791666666666666852, 0.4833333333333333370, 0.4874999999999999889, 0.4916666666666666408, 0.4958333333333333481, 0.5000000000000000000, 0.5041666666666666519, 0.5083333333333333037, 0.5124999999999999556, 0.5166666666666667185, 0.5208333333333333703, 0.5250000000000000222, 0.5291666666666666741, 0.5333333333333333259, 0.5374999999999999778, 0.5416666666666666297, 0.5458333333333332815, 0.5500000000000000444, 0.5541666666666666963, 0.5583333333333333481, 0.5625000000000000000, 0.5666666666666666519, 0.5708333333333333037, 0.5749999999999999556, 0.5791666666666667185, 0.5833333333333333703, 0.5875000000000000222, 0.5916666666666666741, 0.5958333333333333259, 0.5999999999999999778, 0.6041666666666666297, 0.6083333333333332815, 0.6125000000000000444, 0.6166666666666666963, 0.6208333333333333481, 0.6250000000000000000, 0.6291666666666666519, 0.6333333333333333037, 0.6374999999999999556, 0.6416666666666667185, 0.6458333333333333703, 0.6500000000000000222, 0.6541666666666666741, 0.6583333333333333259, 0.6624999999999999778, 0.6666666666666666297, 0.6708333333333332815, 0.6750000000000000444, 0.6791666666666666963, 0.6833333333333333481, 0.6875000000000000000, 0.6916666666666666519, 0.6958333333333333037, 0.6999999999999999556, 0.7041666666666667185, 0.7083333333333333703, 0.7125000000000000222, 0.7166666666666666741, 0.7208333333333333259, 0.7249999999999999778, 0.7291666666666666297, 0.7333333333333332815, 0.7375000000000000444, 0.7416666666666666963, 0.7458333333333333481, 0.7500000000000000000, 0.7541666666666666519, 0.7583333333333333037, 0.7624999999999999556, 0.7666666666666667185, 0.7708333333333333703, 0.7750000000000000222, 0.7791666666666666741, 0.7833333333333333259, 0.7874999999999999778, 0.7916666666666666297, 0.7958333333333332815, 0.8000000000000000444, 0.8041666666666666963, 0.8083333333333333481, 0.8125000000000000000, 0.8166666666666666519, 0.8208333333333333037, 0.8249999999999999556, 0.8291666666666667185, 0.8333333333333333703, 0.8375000000000000222, 0.8416666666666666741, 0.8458333333333333259, 0.8499999999999999778, 0.8541666666666666297, 0.8583333333333332815, 0.8625000000000000444, 0.8666666666666666963, 0.8708333333333333481, 0.8750000000000000000, 0.8791666666666666519, 0.8833333333333333037, 0.8874999999999999556, 0.8916666666666667185, 0.8958333333333333703, 0.9000000000000000222, 0.9041666666666666741, 0.9083333333333333259, 0.9124999999999999778, 0.9166666666666666297, 0.9208333333333332815, 0.9250000000000000444, 0.9291666666666666963, 0.9333333333333333481, 0.9375000000000000000, 0.9416666666666666519, 0.9458333333333333037, 0.9499999999999999556, 0.9541666666666667185, 0.9583333333333333703, 0.9625000000000000222, 0.9666666666666666741, 0.9708333333333333259, 0.9749999999999999778, 0.9791666666666666297, 0.9833333333333332815, 0.9875000000000000444 ),
 .UNSPECIFIED. ) 
 GEOMETRIC_REPRESENTATION_ITEM ( )  RATIONAL_B_SPLINE_SURFACE ( (
 ( 1.000000000000000000, 0.9659258262890683122, 1.000000000000000000, 0.9659258262890683122, 1.000000000000000000, 0.9659258262890683122, 1.000000000000000000, 0.9659258262890683122, 1.000000000000000000, 0.9659258262890683122, 1.000000000000000000, 0.9659258262890683122, 1.000000000000000000, 0.9659258262890683122, 1.000000000000000000, 0.9659258262890683122, 1.000000000000000000, 0.9659258262890683122, 1.000000000000000000, 0.9659258262890683122, 1.000000000000000000, 0.9659258262890683122, 1.000000000000000000, 0.9659258262890683122, 1.000000000000000000, 0.9659258262890683122, 1.000000000000000000, 0.9659258262890683122, 1.000000000000000000, 0.9659258262890683122, 1.000000000000000000, 0.9659258262890683122, 1.000000000000000000, 0.9659258262890683122, 1.000000000000000000, 0.9659258262890683122, 1.000000000000000000, 0.9659258262890683122, 1.000000000000000000, 0.9659258262890683122, 1.000000000000000000, 0.9659258262890683122, 1.000000000000000000, 0.9659258262890683122, 1.000000000000000000, 0.9659258262890683122, 1.000000000000000000, 0.9659258262890683122, 1.000000000000000000, 0.9659258262890683122, 1.000000000000000000, 0.9659258262890683122, 1.000000000000000000, 0.9659258262890683122, 1.000000000000000000, 0.9659258262890683122, 1.000000000000000000, 0.9659258262890683122, 1.000000000000000000, 0.9659258262890683122, 1.000000000000000000, 0.9659258262890683122, 1.000000000000000000, 0.9659258262890683122, 1.000000000000000000, 0.9659258262890683122, 1.000000000000000000, 0.9659258262890683122, 1.000000000000000000, 0.9659258262890683122, 1.000000000000000000, 0.9659258262890683122, 1.000000000000000000, 0.9659258262890683122, 1.000000000000000000, 0.9659258262890683122, 1.000000000000000000, 0.9659258262890683122, 1.000000000000000000, 0.9659258262890683122, 1.000000000000000000, 0.9659258262890683122, 1.000000000000000000, 0.9659258262890683122, 1.000000000000000000, 0.9659258262890683122, 1.000000000000000000, 0.9659258262890683122, 1.000000000000000000, 0.9659258262890683122, 1.000000000000000000, 0.9659258262890683122, 1.000000000000000000, 0.9659258262890683122, 1.000000000000000000, 0.9659258262890683122, 1.000000000000000000, 0.9659258262890683122, 1.000000000000000000, 0.9659258262890683122, 1.000000000000000000, 0.9659258262890683122, 1.000000000000000000, 0.9659258262890683122, 1.000000000000000000, 0.9659258262890683122, 1.000000000000000000, 0.9659258262890683122, 1.000000000000000000, 0.9659258262890683122, 1.000000000000000000, 0.9659258262890683122, 1.000000000000000000, 0.9659258262890683122, 1.000000000000000000, 0.9659258262890683122, 1.000000000000000000, 0.9659258262890683122, 1.000000000000000000, 0.9659258262890683122, 1.000000000000000000, 0.9659258262890683122, 1.000000000000000000, 0.9659258262890683122, 1.000000000000000000, 0.9659258262890683122, 1.000000000000000000, 0.9659258262890683122, 1.000000000000000000, 0.9659258262890683122, 1.000000000000000000, 0.9659258262890683122, 1.000000000000000000, 0.9659258262890683122, 1.000000000000000000, 0.9659258262890683122, 1.000000000000000000, 0.9659258262890683122, 1.000000000000000000, 0.9659258262890683122, 1.000000000000000000, 0.9659258262890683122, 1.000000000000000000, 0.9659258262890683122, 1.000000000000000000, 0.9659258262890683122, 1.000000000000000000, 0.9659258262890683122, 1.000000000000000000, 0.9659258262890683122, 1.000000000000000000, 0.9659258262890683122, 1.000000000000000000, 0.9659258262890683122, 1.000000000000000000, 0.9659258262890683122, 1.000000000000000000, 0.9659258262890683122, 1.000000000000000000, 0.9659258262890683122, 1.000000000000000000, 0.9659258262890683122, 1.000000000000000000, 0.9659258262890683122, 1.000000000000000000, 0.9659258262890683122, 1.000000000000000000, 0.9659258262890683122, 1.000000000000000000, 0.9659258262890683122, 1.000000000000000000, 0.9659258262890683122, 1.000000000000000000, 0.9659258262890683122, 1.000000000000000000, 0.9659258262890683122, 1.000000000000000000, 0.9659258262890683122, 1.000000000000000000, 0.9659258262890683122, 1.000000000000000000, 0.9659258262890683122, 1.000000000000000000, 0.9659258262890683122, 1.000000000000000000, 0.9659258262890683122, 1.000000000000000000, 0.9659258262890683122, 1.000000000000000000, 0.9659258262890683122, 1.000000000000000000, 0.9659258262890683122, 1.000000000000000000, 0.9659258262890683122, 1.000000000000000000, 0.9659258262890683122, 1.000000000000000000, 0.9659258262890683122, 1.000000000000000000, 0.9659258262890683122, 1.000000000000000000, 0.9659258262890683122, 1.000000000000000000, 0.9659258262890683122, 1.000000000000000000, 0.9659258262890683122, 1.000000000000000000, 0.9659258262890683122, 1.000000000000000000, 0.9659258262890683122, 1.000000000000000000, 0.9659258262890683122, 1.000000000000000000, 0.9659258262890683122, 1.000000000000000000, 0.9659258262890683122, 1.000000000000000000, 0.9659258262890683122, 1.000000000000000000, 0.9659258262890683122, 1.000000000000000000, 0.9659258262890683122, 1.000000000000000000, 0.9659258262890683122, 1.000000000000000000, 0.9659258262890683122, 1.000000000000000000, 0.9659258262890683122, 1.000000000000000000, 0.9659258262890683122, 1.000000000000000000, 0.9659258262890683122, 1.000000000000000000, 0.9659258262890683122, 1.000000000000000000, 0.9659258262890683122, 1.000000000000000000, 0.9659258262890683122, 1.000000000000000000, 0.9659258262890683122, 1.000000000000000000, 0.9659258262890683122, 1.000000000000000000, 0.9659258262890683122, 1.000000000000000000, 0.9659258262890683122, 1.000000000000000000, 0.9659258262890683122, 1.000000000000000000, 0.9659258262890683122, 1.000000000000000000, 0.9659258262890683122, 1.000000000000000000, 0.9659258262890683122, 1.000000000000000000, 0.9659258262890683122, 1.000000000000000000, 0.9659258262890683122, 1.000000000000000000, 0.9659258262890683122, 1.000000000000000000, 0.9659258262890683122, 1.000000000000000000, 0.9659258262890683122, 1.000000000000000000, 0.9659258262890683122, 1.000000000000000000, 0.9659258262890683122, 1.000000000000000000, 0.9659258262890683122, 1.000000000000000000, 0.9659258262890683122, 1.000000000000000000, 0.9659258262890683122, 1.000000000000000000, 0.9659258262890683122, 1.000000000000000000, 0.9659258262890683122, 1.000000000000000000, 0.9659258262890683122, 1.000000000000000000, 0.9659258262890683122, 1.000000000000000000, 0.9659258262890683122, 1.000000000000000000, 0.9659258262890683122, 1.000000000000000000, 0.9659258262890683122, 1.000000000000000000, 0.9659258262890683122, 1.000000000000000000, 0.9659258262890683122, 1.000000000000000000, 0.9659258262890683122, 1.000000000000000000, 0.9659258262890683122, 1.000000000000000000, 0.9659258262890683122, 1.000000000000000000, 0.9659258262890683122, 1.000000000000000000, 0.9659258262890683122, 1.000000000000000000, 0.9659258262890683122, 1.000000000000000000, 0.9659258262890683122, 1.000000000000000000, 0.9659258262890683122, 1.000000000000000000, 0.9659258262890683122, 1.000000000000000000, 0.9659258262890683122, 1.000000000000000000, 0.9659258262890683122, 1.000000000000000000, 0.9659258262890683122, 1.000000000000000000, 0.9659258262890683122, 1.000000000000000000, 0.9659258262890683122, 1.000000000000000000, 0.9659258262890683122, 1.000000000000000000, 0.9659258262890683122, 1.000000000000000000, 0.9659258262890683122, 1.000000000000000000, 0.9659258262890683122, 1.000000000000000000, 0.9659258262890683122, 1.000000000000000000, 0.9659258262890683122, 1.000000000000000000, 0.9659258262890683122, 1.000000000000000000, 0.9659258262890683122, 1.000000000000000000, 0.9659258262890683122, 1.000000000000000000, 0.9659258262890683122, 1.000000000000000000, 0.9659258262890683122, 1.000000000000000000, 0.9659258262890683122, 1.000000000000000000, 0.9659258262890683122, 1.000000000000000000, 0.9659258262890683122, 1.000000000000000000, 0.9659258262890683122, 1.000000000000000000, 0.9659258262890683122, 1.000000000000000000, 0.9659258262890683122, 1.000000000000000000, 0.9659258262890683122, 1.000000000000000000, 0.9659258262890683122, 1.000000000000000000, 0.9659258262890683122, 1.000000000000000000, 0.9659258262890683122, 1.000000000000000000, 0.9659258262890683122, 1.000000000000000000, 0.9659258262890683122, 1.000000000000000000, 0.9659258262890683122, 1.000000000000000000, 0.9659258262890683122, 1.000000000000000000, 0.9659258262890683122, 1.000000000000000000, 0.9659258262890683122, 1.000000000000000000, 0.9659258262890683122, 1.000000000000000000, 0.9659258262890683122, 1.000000000000000000, 0.9659258262890683122, 1.000000000000000000, 0.9659258262890683122, 1.000000000000000000, 0.9659258262890683122, 1.000000000000000000, 0.9659258262890683122, 1.000000000000000000, 0.9659258262890683122, 1.000000000000000000, 0.9659258262890683122, 1.000000000000000000, 0.9659258262890683122, 1.000000000000000000, 0.9659258262890683122, 1.000000000000000000, 0.9659258262890683122, 1.000000000000000000, 0.9659258262890683122, 1.000000000000000000, 0.9659258262890683122, 1.000000000000000000, 0.9659258262890683122, 1.000000000000000000, 0.9659258262890683122, 1.000000000000000000, 0.9659258262890683122, 1.000000000000000000, 0.9659258262890683122, 1.000000000000000000, 0.9659258262890683122, 1.000000000000000000, 0.9659258262890683122, 1.000000000000000000, 0.9659258262890683122, 1.000000000000000000, 0.9659258262890683122, 1.000000000000000000, 0.9659258262890683122, 1.000000000000000000, 0.9659258262890683122, 1.000000000000000000, 0.9659258262890683122, 1.000000000000000000, 0.9659258262890683122, 1.000000000000000000, 0.9659258262890683122, 1.000000000000000000, 0.9659258262890683122, 1.000000000000000000, 0.9659258262890683122, 1.000000000000000000, 0.9659258262890683122, 1.000000000000000000, 0.9659258262890683122, 1.000000000000000000, 0.9659258262890683122, 1.000000000000000000, 0.9659258262890683122, 1.000000000000000000, 0.9659258262890683122, 1.000000000000000000, 0.9659258262890683122, 1.000000000000000000, 0.9659258262890683122, 1.000000000000000000, 0.9659258262890683122, 1.000000000000000000, 0.9659258262890683122, 1.000000000000000000, 0.9659258262890683122, 1.000000000000000000, 0.9659258262890683122, 1.000000000000000000, 0.9659258262890683122, 1.000000000000000000, 0.9659258262890683122, 1.000000000000000000, 0.9659258262890683122, 1.000000000000000000, 0.9659258262890683122, 1.000000000000000000, 0.9659258262890683122, 1.000000000000000000, 0.9659258262890683122, 1.000000000000000000, 0.9659258262890683122, 1.000000000000000000, 0.9659258262890683122, 1.000000000000000000, 0.9659258262890683122, 1.000000000000000000, 0.9659258262890683122, 1.000000000000000000, 0.9659258262890683122, 1.000000000000000000),
 ( 0.8047378541243631611, 0.7773170766911672303, 0.8047378541243631611, 0.7773170766911672303, 0.8047378541243631611, 0.7773170766911672303, 0.8047378541243631611, 0.7773170766911672303, 0.8047378541243631611, 0.7773170766911672303, 0.8047378541243631611, 0.7773170766911672303, 0.8047378541243631611, 0.7773170766911672303, 0.8047378541243631611, 0.7773170766911672303, 0.8047378541243631611, 0.7773170766911672303, 0.8047378541243631611, 0.7773170766911672303, 0.8047378541243631611, 0.7773170766911672303, 0.8047378541243631611, 0.7773170766911672303, 0.8047378541243631611, 0.7773170766911672303, 0.8047378541243631611, 0.7773170766911672303, 0.8047378541243631611, 0.7773170766911672303, 0.8047378541243631611, 0.7773170766911672303, 0.8047378541243631611, 0.7773170766911672303, 0.8047378541243631611, 0.7773170766911672303, 0.8047378541243631611, 0.7773170766911672303, 0.8047378541243631611, 0.7773170766911672303, 0.8047378541243631611, 0.7773170766911672303, 0.8047378541243631611, 0.7773170766911672303, 0.8047378541243631611, 0.7773170766911672303, 0.8047378541243631611, 0.7773170766911672303, 0.8047378541243631611, 0.7773170766911672303, 0.8047378541243631611, 0.7773170766911672303, 0.8047378541243631611, 0.7773170766911672303, 0.8047378541243631611, 0.7773170766911672303, 0.8047378541243631611, 0.7773170766911672303, 0.8047378541243631611, 0.7773170766911672303, 0.8047378541243631611, 0.7773170766911672303, 0.8047378541243631611, 0.7773170766911672303, 0.8047378541243631611, 0.7773170766911672303, 0.8047378541243631611, 0.7773170766911672303, 0.8047378541243631611, 0.7773170766911672303, 0.8047378541243631611, 0.7773170766911672303, 0.8047378541243631611, 0.7773170766911672303, 0.8047378541243631611, 0.7773170766911672303, 0.8047378541243631611, 0.7773170766911672303, 0.8047378541243631611, 0.7773170766911672303, 0.8047378541243631611, 0.7773170766911672303, 0.8047378541243631611, 0.7773170766911672303, 0.8047378541243631611, 0.7773170766911672303, 0.8047378541243631611, 0.7773170766911672303, 0.8047378541243631611, 0.7773170766911672303, 0.8047378541243631611, 0.7773170766911672303, 0.8047378541243631611, 0.7773170766911672303, 0.8047378541243631611, 0.7773170766911672303, 0.8047378541243631611, 0.7773170766911672303, 0.8047378541243631611, 0.7773170766911672303, 0.8047378541243631611, 0.7773170766911672303, 0.8047378541243631611, 0.7773170766911672303, 0.8047378541243631611, 0.7773170766911672303, 0.8047378541243631611, 0.7773170766911672303, 0.8047378541243631611, 0.7773170766911672303, 0.8047378541243631611, 0.7773170766911672303, 0.8047378541243631611, 0.7773170766911672303, 0.8047378541243631611, 0.7773170766911672303, 0.8047378541243631611, 0.7773170766911672303, 0.8047378541243631611, 0.7773170766911672303, 0.8047378541243631611, 0.7773170766911672303, 0.8047378541243631611, 0.7773170766911672303, 0.8047378541243631611, 0.7773170766911672303, 0.8047378541243631611, 0.7773170766911672303, 0.8047378541243631611, 0.7773170766911672303, 0.8047378541243631611, 0.7773170766911672303, 0.8047378541243631611, 0.7773170766911672303, 0.8047378541243631611, 0.7773170766911672303, 0.8047378541243631611, 0.7773170766911672303, 0.8047378541243631611, 0.7773170766911672303, 0.8047378541243631611, 0.7773170766911672303, 0.8047378541243631611, 0.7773170766911672303, 0.8047378541243631611, 0.7773170766911672303, 0.8047378541243631611, 0.7773170766911672303, 0.8047378541243631611, 0.7773170766911672303, 0.8047378541243631611, 0.7773170766911672303, 0.8047378541243631611, 0.7773170766911672303, 0.8047378541243631611, 0.7773170766911672303, 0.8047378541243631611, 0.7773170766911672303, 0.8047378541243631611, 0.7773170766911672303, 0.8047378541243631611, 0.7773170766911672303, 0.8047378541243631611, 0.7773170766911672303, 0.8047378541243631611, 0.7773170766911672303, 0.8047378541243631611, 0.7773170766911672303, 0.8047378541243631611, 0.7773170766911672303, 0.8047378541243631611, 0.7773170766911672303, 0.8047378541243631611, 0.7773170766911672303, 0.8047378541243631611, 0.7773170766911672303, 0.8047378541243631611, 0.7773170766911672303, 0.8047378541243631611, 0.7773170766911672303, 0.8047378541243631611, 0.7773170766911672303, 0.8047378541243631611, 0.7773170766911672303, 0.8047378541243631611, 0.7773170766911672303, 0.8047378541243631611, 0.7773170766911672303, 0.8047378541243631611, 0.7773170766911672303, 0.8047378541243631611, 0.7773170766911672303, 0.8047378541243631611, 0.7773170766911672303, 0.8047378541243631611, 0.7773170766911672303, 0.8047378541243631611, 0.7773170766911672303, 0.8047378541243631611, 0.7773170766911672303, 0.8047378541243631611, 0.7773170766911672303, 0.8047378541243631611, 0.7773170766911672303, 0.8047378541243631611, 0.7773170766911672303, 0.8047378541243631611, 0.7773170766911672303, 0.8047378541243631611, 0.7773170766911672303, 0.8047378541243631611, 0.7773170766911672303, 0.8047378541243631611, 0.7773170766911672303, 0.8047378541243631611, 0.7773170766911672303, 0.8047378541243631611, 0.7773170766911672303, 0.8047378541243631611, 0.7773170766911672303, 0.8047378541243631611, 0.7773170766911672303, 0.8047378541243631611, 0.7773170766911672303, 0.8047378541243631611, 0.7773170766911672303, 0.8047378541243631611, 0.7773170766911672303, 0.8047378541243631611, 0.7773170766911672303, 0.8047378541243631611, 0.7773170766911672303, 0.8047378541243631611, 0.7773170766911672303, 0.8047378541243631611, 0.7773170766911672303, 0.8047378541243631611, 0.7773170766911672303, 0.8047378541243631611, 0.7773170766911672303, 0.8047378541243631611, 0.7773170766911672303, 0.8047378541243631611, 0.7773170766911672303, 0.8047378541243631611, 0.7773170766911672303, 0.8047378541243631611, 0.7773170766911672303, 0.8047378541243631611, 0.7773170766911672303, 0.8047378541243631611, 0.7773170766911672303, 0.8047378541243631611, 0.7773170766911672303, 0.8047378541243631611, 0.7773170766911672303, 0.8047378541243631611, 0.7773170766911672303, 0.8047378541243631611, 0.7773170766911672303, 0.8047378541243631611, 0.7773170766911672303, 0.8047378541243631611, 0.7773170766911672303, 0.8047378541243631611, 0.7773170766911672303, 0.8047378541243631611, 0.7773170766911672303, 0.8047378541243631611, 0.7773170766911672303, 0.8047378541243631611, 0.7773170766911672303, 0.8047378541243631611, 0.7773170766911672303, 0.8047378541243631611, 0.7773170766911672303, 0.8047378541243631611, 0.7773170766911672303, 0.8047378541243631611, 0.7773170766911672303, 0.8047378541243631611, 0.7773170766911672303, 0.8047378541243631611, 0.7773170766911672303, 0.8047378541243631611, 0.7773170766911672303, 0.8047378541243631611, 0.7773170766911672303, 0.8047378541243631611, 0.7773170766911672303, 0.8047378541243631611, 0.7773170766911672303, 0.8047378541243631611, 0.7773170766911672303, 0.8047378541243631611, 0.7773170766911672303, 0.8047378541243631611, 0.7773170766911672303, 0.8047378541243631611, 0.7773170766911672303, 0.8047378541243631611, 0.7773170766911672303, 0.8047378541243631611, 0.7773170766911672303, 0.8047378541243631611, 0.7773170766911672303, 0.8047378541243631611, 0.7773170766911672303, 0.8047378541243631611, 0.7773170766911672303, 0.8047378541243631611, 0.7773170766911672303, 0.8047378541243631611, 0.7773170766911672303, 0.8047378541243631611, 0.7773170766911672303, 0.8047378541243631611, 0.7773170766911672303, 0.8047378541243631611, 0.7773170766911672303, 0.8047378541243631611, 0.7773170766911672303, 0.8047378541243631611, 0.7773170766911672303, 0.8047378541243631611, 0.7773170766911672303, 0.8047378541243631611, 0.7773170766911672303, 0.8047378541243631611, 0.7773170766911672303, 0.8047378541243631611, 0.7773170766911672303, 0.8047378541243631611, 0.7773170766911672303, 0.8047378541243631611, 0.7773170766911672303, 0.8047378541243631611, 0.7773170766911672303, 0.8047378541243631611, 0.7773170766911672303, 0.8047378541243631611, 0.7773170766911672303, 0.8047378541243631611, 0.7773170766911672303, 0.8047378541243631611, 0.7773170766911672303, 0.8047378541243631611, 0.7773170766911672303, 0.8047378541243631611, 0.7773170766911672303, 0.8047378541243631611, 0.7773170766911672303, 0.8047378541243631611, 0.7773170766911672303, 0.8047378541243631611, 0.7773170766911672303, 0.8047378541243631611, 0.7773170766911672303, 0.8047378541243631611, 0.7773170766911672303, 0.8047378541243631611, 0.7773170766911672303, 0.8047378541243631611, 0.7773170766911672303, 0.8047378541243631611, 0.7773170766911672303, 0.8047378541243631611, 0.7773170766911672303, 0.8047378541243631611, 0.7773170766911672303, 0.8047378541243631611, 0.7773170766911672303, 0.8047378541243631611, 0.7773170766911672303, 0.8047378541243631611, 0.7773170766911672303, 0.8047378541243631611, 0.7773170766911672303, 0.8047378541243631611, 0.7773170766911672303, 0.8047378541243631611, 0.7773170766911672303, 0.8047378541243631611, 0.7773170766911672303, 0.8047378541243631611, 0.7773170766911672303, 0.8047378541243631611, 0.7773170766911672303, 0.8047378541243631611, 0.7773170766911672303, 0.8047378541243631611, 0.7773170766911672303, 0.8047378541243631611, 0.7773170766911672303, 0.8047378541243631611, 0.7773170766911672303, 0.8047378541243631611, 0.7773170766911672303, 0.8047378541243631611, 0.7773170766911672303, 0.8047378541243631611, 0.7773170766911672303, 0.8047378541243631611, 0.7773170766911672303, 0.8047378541243631611, 0.7773170766911672303, 0.8047378541243631611, 0.7773170766911672303, 0.8047378541243631611, 0.7773170766911672303, 0.8047378541243631611, 0.7773170766911672303, 0.8047378541243631611, 0.7773170766911672303, 0.8047378541243631611, 0.7773170766911672303, 0.8047378541243631611, 0.7773170766911672303, 0.8047378541243631611, 0.7773170766911672303, 0.8047378541243631611, 0.7773170766911672303, 0.8047378541243631611, 0.7773170766911672303, 0.8047378541243631611, 0.7773170766911672303, 0.8047378541243631611, 0.7773170766911672303, 0.8047378541243631611, 0.7773170766911672303, 0.8047378541243631611, 0.7773170766911672303, 0.8047378541243631611, 0.7773170766911672303, 0.8047378541243631611, 0.7773170766911672303, 0.8047378541243631611, 0.7773170766911672303, 0.8047378541243631611, 0.7773170766911672303, 0.8047378541243631611, 0.7773170766911672303, 0.8047378541243631611, 0.7773170766911672303, 0.8047378541243631611, 0.7773170766911672303, 0.8047378541243631611, 0.7773170766911672303, 0.8047378541243631611, 0.7773170766911672303, 0.8047378541243631611, 0.7773170766911672303, 0.8047378541243631611, 0.7773170766911672303, 0.8047378541243631611, 0.7773170766911672303, 0.8047378541243631611, 0.7773170766911672303, 0.8047378541243631611, 0.7773170766911672303, 0.8047378541243631611, 0.7773170766911672303, 0.8047378541243631611, 0.7773170766911672303, 0.8047378541243631611, 0.7773170766911672303, 0.8047378541243631611, 0.7773170766911672303, 0.8047378541243631611, 0.7773170766911672303, 0.8047378541243631611, 0.7773170766911672303, 0.8047378541243631611, 0.7773170766911672303, 0.8047378541243631611),
 ( 0.8047378541243631611, 0.7773170766911672303, 0.8047378541243631611, 0.7773170766911672303, 0.8047378541243631611, 0.7773170766911672303, 0.8047378541243631611, 0.7773170766911672303, 0.8047378541243631611, 0.7773170766911672303, 0.8047378541243631611, 0.7773170766911672303, 0.8047378541243631611, 0.7773170766911672303, 0.8047378541243631611, 0.7773170766911672303, 0.8047378541243631611, 0.7773170766911672303, 0.8047378541243631611, 0.7773170766911672303, 0.8047378541243631611, 0.7773170766911672303, 0.8047378541243631611, 0.7773170766911672303, 0.8047378541243631611, 0.7773170766911672303, 0.8047378541243631611, 0.7773170766911672303, 0.8047378541243631611, 0.7773170766911672303, 0.8047378541243631611, 0.7773170766911672303, 0.8047378541243631611, 0.7773170766911672303, 0.8047378541243631611, 0.7773170766911672303, 0.8047378541243631611, 0.7773170766911672303, 0.8047378541243631611, 0.7773170766911672303, 0.8047378541243631611, 0.7773170766911672303, 0.8047378541243631611, 0.7773170766911672303, 0.8047378541243631611, 0.7773170766911672303, 0.8047378541243631611, 0.7773170766911672303, 0.8047378541243631611, 0.7773170766911672303, 0.8047378541243631611, 0.7773170766911672303, 0.8047378541243631611, 0.7773170766911672303, 0.8047378541243631611, 0.7773170766911672303, 0.8047378541243631611, 0.7773170766911672303, 0.8047378541243631611, 0.7773170766911672303, 0.8047378541243631611, 0.7773170766911672303, 0.8047378541243631611, 0.7773170766911672303, 0.8047378541243631611, 0.7773170766911672303, 0.8047378541243631611, 0.7773170766911672303, 0.8047378541243631611, 0.7773170766911672303, 0.8047378541243631611, 0.7773170766911672303, 0.8047378541243631611, 0.7773170766911672303, 0.8047378541243631611, 0.7773170766911672303, 0.8047378541243631611, 0.7773170766911672303, 0.8047378541243631611, 0.7773170766911672303, 0.8047378541243631611, 0.7773170766911672303, 0.8047378541243631611, 0.7773170766911672303, 0.8047378541243631611, 0.7773170766911672303, 0.8047378541243631611, 0.7773170766911672303, 0.8047378541243631611, 0.7773170766911672303, 0.8047378541243631611, 0.7773170766911672303, 0.8047378541243631611, 0.7773170766911672303, 0.8047378541243631611, 0.7773170766911672303, 0.8047378541243631611, 0.7773170766911672303, 0.8047378541243631611, 0.7773170766911672303, 0.8047378541243631611, 0.7773170766911672303, 0.8047378541243631611, 0.7773170766911672303, 0.8047378541243631611, 0.7773170766911672303, 0.8047378541243631611, 0.7773170766911672303, 0.8047378541243631611, 0.7773170766911672303, 0.8047378541243631611, 0.7773170766911672303, 0.8047378541243631611, 0.7773170766911672303, 0.8047378541243631611, 0.7773170766911672303, 0.8047378541243631611, 0.7773170766911672303, 0.8047378541243631611, 0.7773170766911672303, 0.8047378541243631611, 0.7773170766911672303, 0.8047378541243631611, 0.7773170766911672303, 0.8047378541243631611, 0.7773170766911672303, 0.8047378541243631611, 0.7773170766911672303, 0.8047378541243631611, 0.7773170766911672303, 0.8047378541243631611, 0.7773170766911672303, 0.8047378541243631611, 0.7773170766911672303, 0.8047378541243631611, 0.7773170766911672303, 0.8047378541243631611, 0.7773170766911672303, 0.8047378541243631611, 0.7773170766911672303, 0.8047378541243631611, 0.7773170766911672303, 0.8047378541243631611, 0.7773170766911672303, 0.8047378541243631611, 0.7773170766911672303, 0.8047378541243631611, 0.7773170766911672303, 0.8047378541243631611, 0.7773170766911672303, 0.8047378541243631611, 0.7773170766911672303, 0.8047378541243631611, 0.7773170766911672303, 0.8047378541243631611, 0.7773170766911672303, 0.8047378541243631611, 0.7773170766911672303, 0.8047378541243631611, 0.7773170766911672303, 0.8047378541243631611, 0.7773170766911672303, 0.8047378541243631611, 0.7773170766911672303, 0.8047378541243631611, 0.7773170766911672303, 0.8047378541243631611, 0.7773170766911672303, 0.8047378541243631611, 0.7773170766911672303, 0.8047378541243631611, 0.7773170766911672303, 0.8047378541243631611, 0.7773170766911672303, 0.8047378541243631611, 0.7773170766911672303, 0.8047378541243631611, 0.7773170766911672303, 0.8047378541243631611, 0.7773170766911672303, 0.8047378541243631611, 0.7773170766911672303, 0.8047378541243631611, 0.7773170766911672303, 0.8047378541243631611, 0.7773170766911672303, 0.8047378541243631611, 0.7773170766911672303, 0.8047378541243631611, 0.7773170766911672303, 0.8047378541243631611, 0.7773170766911672303, 0.8047378541243631611, 0.7773170766911672303, 0.8047378541243631611, 0.7773170766911672303, 0.8047378541243631611, 0.7773170766911672303, 0.8047378541243631611, 0.7773170766911672303, 0.8047378541243631611, 0.7773170766911672303, 0.8047378541243631611, 0.7773170766911672303, 0.8047378541243631611, 0.7773170766911672303, 0.8047378541243631611, 0.7773170766911672303, 0.8047378541243631611, 0.7773170766911672303, 0.8047378541243631611, 0.7773170766911672303, 0.8047378541243631611, 0.7773170766911672303, 0.8047378541243631611, 0.7773170766911672303, 0.8047378541243631611, 0.7773170766911672303, 0.8047378541243631611, 0.7773170766911672303, 0.8047378541243631611, 0.7773170766911672303, 0.8047378541243631611, 0.7773170766911672303, 0.8047378541243631611, 0.7773170766911672303, 0.8047378541243631611, 0.7773170766911672303, 0.8047378541243631611, 0.7773170766911672303, 0.8047378541243631611, 0.7773170766911672303, 0.8047378541243631611, 0.7773170766911672303, 0.8047378541243631611, 0.7773170766911672303, 0.8047378541243631611, 0.7773170766911672303, 0.8047378541243631611, 0.7773170766911672303, 0.8047378541243631611, 0.7773170766911672303, 0.8047378541243631611, 0.7773170766911672303, 0.8047378541243631611, 0.7773170766911672303, 0.8047378541243631611, 0.7773170766911672303, 0.8047378541243631611, 0.7773170766911672303, 0.8047378541243631611, 0.7773170766911672303, 0.8047378541243631611, 0.7773170766911672303, 0.8047378541243631611, 0.7773170766911672303, 0.8047378541243631611, 0.7773170766911672303, 0.8047378541243631611, 0.7773170766911672303, 0.8047378541243631611, 0.7773170766911672303, 0.8047378541243631611, 0.7773170766911672303, 0.8047378541243631611, 0.7773170766911672303, 0.8047378541243631611, 0.7773170766911672303, 0.8047378541243631611, 0.7773170766911672303, 0.8047378541243631611, 0.7773170766911672303, 0.8047378541243631611, 0.7773170766911672303, 0.8047378541243631611, 0.7773170766911672303, 0.8047378541243631611, 0.7773170766911672303, 0.8047378541243631611, 0.7773170766911672303, 0.8047378541243631611, 0.7773170766911672303, 0.8047378541243631611, 0.7773170766911672303, 0.8047378541243631611, 0.7773170766911672303, 0.8047378541243631611, 0.7773170766911672303, 0.8047378541243631611, 0.7773170766911672303, 0.8047378541243631611, 0.7773170766911672303, 0.8047378541243631611, 0.7773170766911672303, 0.8047378541243631611, 0.7773170766911672303, 0.8047378541243631611, 0.7773170766911672303, 0.8047378541243631611, 0.7773170766911672303, 0.8047378541243631611, 0.7773170766911672303, 0.8047378541243631611, 0.7773170766911672303, 0.8047378541243631611, 0.7773170766911672303, 0.8047378541243631611, 0.7773170766911672303, 0.8047378541243631611, 0.7773170766911672303, 0.8047378541243631611, 0.7773170766911672303, 0.8047378541243631611, 0.7773170766911672303, 0.8047378541243631611, 0.7773170766911672303, 0.8047378541243631611, 0.7773170766911672303, 0.8047378541243631611, 0.7773170766911672303, 0.8047378541243631611, 0.7773170766911672303, 0.8047378541243631611, 0.7773170766911672303, 0.8047378541243631611, 0.7773170766911672303, 0.8047378541243631611, 0.7773170766911672303, 0.8047378541243631611, 0.7773170766911672303, 0.8047378541243631611, 0.7773170766911672303, 0.8047378541243631611, 0.7773170766911672303, 0.8047378541243631611, 0.7773170766911672303, 0.8047378541243631611, 0.7773170766911672303, 0.8047378541243631611, 0.7773170766911672303, 0.8047378541243631611, 0.7773170766911672303, 0.8047378541243631611, 0.7773170766911672303, 0.8047378541243631611, 0.7773170766911672303, 0.8047378541243631611, 0.7773170766911672303, 0.8047378541243631611, 0.7773170766911672303, 0.8047378541243631611, 0.7773170766911672303, 0.8047378541243631611, 0.7773170766911672303, 0.8047378541243631611, 0.7773170766911672303, 0.8047378541243631611, 0.7773170766911672303, 0.8047378541243631611, 0.7773170766911672303, 0.8047378541243631611, 0.7773170766911672303, 0.8047378541243631611, 0.7773170766911672303, 0.8047378541243631611, 0.7773170766911672303, 0.8047378541243631611, 0.7773170766911672303, 0.8047378541243631611, 0.7773170766911672303, 0.8047378541243631611, 0.7773170766911672303, 0.8047378541243631611, 0.7773170766911672303, 0.8047378541243631611, 0.7773170766911672303, 0.8047378541243631611, 0.7773170766911672303, 0.8047378541243631611, 0.7773170766911672303, 0.8047378541243631611, 0.7773170766911672303, 0.8047378541243631611, 0.7773170766911672303, 0.8047378541243631611, 0.7773170766911672303, 0.8047378541243631611, 0.7773170766911672303, 0.8047378541243631611, 0.7773170766911672303, 0.8047378541243631611, 0.7773170766911672303, 0.8047378541243631611, 0.7773170766911672303, 0.8047378541243631611, 0.7773170766911672303, 0.8047378541243631611, 0.7773170766911672303, 0.8047378541243631611, 0.7773170766911672303, 0.8047378541243631611, 0.7773170766911672303, 0.8047378541243631611, 0.7773170766911672303, 0.8047378541243631611, 0.7773170766911672303, 0.8047378541243631611, 0.7773170766911672303, 0.8047378541243631611, 0.7773170766911672303, 0.8047378541243631611, 0.7773170766911672303, 0.8047378541243631611, 0.7773170766911672303, 0.8047378541243631611, 0.7773170766911672303, 0.8047378541243631611, 0.7773170766911672303, 0.8047378541243631611, 0.7773170766911672303, 0.8047378541243631611, 0.7773170766911672303, 0.8047378541243631611, 0.7773170766911672303, 0.8047378541243631611, 0.7773170766911672303, 0.8047378541243631611, 0.7773170766911672303, 0.8047378541243631611, 0.7773170766911672303, 0.8047378541243631611, 0.7773170766911672303, 0.8047378541243631611, 0.7773170766911672303, 0.8047378541243631611, 0.7773170766911672303, 0.8047378541243631611, 0.7773170766911672303, 0.8047378541243631611, 0.7773170766911672303, 0.8047378541243631611, 0.7773170766911672303, 0.8047378541243631611, 0.7773170766911672303, 0.8047378541243631611, 0.7773170766911672303, 0.8047378541243631611, 0.7773170766911672303, 0.8047378541243631611, 0.7773170766911672303, 0.8047378541243631611, 0.7773170766911672303, 0.8047378541243631611, 0.7773170766911672303, 0.8047378541243631611, 0.7773170766911672303, 0.8047378541243631611, 0.7773170766911672303, 0.8047378541243631611, 0.7773170766911672303, 0.8047378541243631611, 0.7773170766911672303, 0.8047378541243631611, 0.7773170766911672303, 0.8047378541243631611, 0.7773170766911672303, 0.8047378541243631611, 0.7773170766911672303, 0.8047378541243631611, 0.7773170766911672303, 0.8047378541243631611, 0.7773170766911672303, 0.8047378541243631611, 0.7773170766911672303, 0.8047378541243631611),
 ( 1.000000000000000000, 0.9659258262890683122, 1.000000000000000000, 0.9659258262890683122, 1.000000000000000000, 0.9659258262890683122, 1.000000000000000000, 0.9659258262890683122, 1.000000000000000000, 0.9659258262890683122, 1.000000000000000000, 0.9659258262890683122, 1.000000000000000000, 0.9659258262890683122, 1.000000000000000000, 0.9659258262890683122, 1.000000000000000000, 0.9659258262890683122, 1.000000000000000000, 0.9659258262890683122, 1.000000000000000000, 0.9659258262890683122, 1.000000000000000000, 0.9659258262890683122, 1.000000000000000000, 0.9659258262890683122, 1.000000000000000000, 0.9659258262890683122, 1.000000000000000000, 0.9659258262890683122, 1.000000000000000000, 0.9659258262890683122, 1.000000000000000000, 0.9659258262890683122, 1.000000000000000000, 0.9659258262890683122, 1.000000000000000000, 0.9659258262890683122, 1.000000000000000000, 0.9659258262890683122, 1.000000000000000000, 0.9659258262890683122, 1.000000000000000000, 0.9659258262890683122, 1.000000000000000000, 0.9659258262890683122, 1.000000000000000000, 0.9659258262890683122, 1.000000000000000000, 0.9659258262890683122, 1.000000000000000000, 0.9659258262890683122, 1.000000000000000000, 0.9659258262890683122, 1.000000000000000000, 0.9659258262890683122, 1.000000000000000000, 0.9659258262890683122, 1.000000000000000000, 0.9659258262890683122, 1.000000000000000000, 0.9659258262890683122, 1.000000000000000000, 0.9659258262890683122, 1.000000000000000000, 0.9659258262890683122, 1.000000000000000000, 0.9659258262890683122, 1.000000000000000000, 0.9659258262890683122, 1.000000000000000000, 0.9659258262890683122, 1.000000000000000000, 0.9659258262890683122, 1.000000000000000000, 0.9659258262890683122, 1.000000000000000000, 0.9659258262890683122, 1.000000000000000000, 0.9659258262890683122, 1.000000000000000000, 0.9659258262890683122, 1.000000000000000000, 0.9659258262890683122, 1.000000000000000000, 0.9659258262890683122, 1.000000000000000000, 0.9659258262890683122, 1.000000000000000000, 0.9659258262890683122, 1.000000000000000000, 0.9659258262890683122, 1.000000000000000000, 0.9659258262890683122, 1.000000000000000000, 0.9659258262890683122, 1.000000000000000000, 0.9659258262890683122, 1.000000000000000000, 0.9659258262890683122, 1.000000000000000000, 0.9659258262890683122, 1.000000000000000000, 0.9659258262890683122, 1.000000000000000000, 0.9659258262890683122, 1.000000000000000000, 0.9659258262890683122, 1.000000000000000000, 0.9659258262890683122, 1.000000000000000000, 0.9659258262890683122, 1.000000000000000000, 0.9659258262890683122, 1.000000000000000000, 0.9659258262890683122, 1.000000000000000000, 0.9659258262890683122, 1.000000000000000000, 0.9659258262890683122, 1.000000000000000000, 0.9659258262890683122, 1.000000000000000000, 0.9659258262890683122, 1.000000000000000000, 0.9659258262890683122, 1.000000000000000000, 0.9659258262890683122, 1.000000000000000000, 0.9659258262890683122, 1.000000000000000000, 0.9659258262890683122, 1.000000000000000000, 0.9659258262890683122, 1.000000000000000000, 0.9659258262890683122, 1.000000000000000000, 0.9659258262890683122, 1.000000000000000000, 0.9659258262890683122, 1.000000000000000000, 0.9659258262890683122, 1.000000000000000000, 0.9659258262890683122, 1.000000000000000000, 0.9659258262890683122, 1.000000000000000000, 0.9659258262890683122, 1.000000000000000000, 0.9659258262890683122, 1.000000000000000000, 0.9659258262890683122, 1.000000000000000000, 0.9659258262890683122, 1.000000000000000000, 0.9659258262890683122, 1.000000000000000000, 0.9659258262890683122, 1.000000000000000000, 0.9659258262890683122, 1.000000000000000000, 0.9659258262890683122, 1.000000000000000000, 0.9659258262890683122, 1.000000000000000000, 0.9659258262890683122, 1.000000000000000000, 0.9659258262890683122, 1.000000000000000000, 0.9659258262890683122, 1.000000000000000000, 0.9659258262890683122, 1.000000000000000000, 0.9659258262890683122, 1.000000000000000000, 0.9659258262890683122, 1.000000000000000000, 0.9659258262890683122, 1.000000000000000000, 0.9659258262890683122, 1.000000000000000000, 0.9659258262890683122, 1.000000000000000000, 0.9659258262890683122, 1.000000000000000000, 0.9659258262890683122, 1.000000000000000000, 0.9659258262890683122, 1.000000000000000000, 0.9659258262890683122, 1.000000000000000000, 0.9659258262890683122, 1.000000000000000000, 0.9659258262890683122, 1.000000000000000000, 0.9659258262890683122, 1.000000000000000000, 0.9659258262890683122, 1.000000000000000000, 0.9659258262890683122, 1.000000000000000000, 0.9659258262890683122, 1.000000000000000000, 0.9659258262890683122, 1.000000000000000000, 0.9659258262890683122, 1.000000000000000000, 0.9659258262890683122, 1.000000000000000000, 0.9659258262890683122, 1.000000000000000000, 0.9659258262890683122, 1.000000000000000000, 0.9659258262890683122, 1.000000000000000000, 0.9659258262890683122, 1.000000000000000000, 0.9659258262890683122, 1.000000000000000000, 0.9659258262890683122, 1.000000000000000000, 0.9659258262890683122, 1.000000000000000000, 0.9659258262890683122, 1.000000000000000000, 0.9659258262890683122, 1.000000000000000000, 0.9659258262890683122, 1.000000000000000000, 0.9659258262890683122, 1.000000000000000000, 0.9659258262890683122, 1.000000000000000000, 0.9659258262890683122, 1.000000000000000000, 0.9659258262890683122, 1.000000000000000000, 0.9659258262890683122, 1.000000000000000000, 0.9659258262890683122, 1.000000000000000000, 0.9659258262890683122, 1.000000000000000000, 0.9659258262890683122, 1.000000000000000000, 0.9659258262890683122, 1.000000000000000000, 0.9659258262890683122, 1.000000000000000000, 0.9659258262890683122, 1.000000000000000000, 0.9659258262890683122, 1.000000000000000000, 0.9659258262890683122, 1.000000000000000000, 0.9659258262890683122, 1.000000000000000000, 0.9659258262890683122, 1.000000000000000000, 0.9659258262890683122, 1.000000000000000000, 0.9659258262890683122, 1.000000000000000000, 0.9659258262890683122, 1.000000000000000000, 0.9659258262890683122, 1.000000000000000000, 0.9659258262890683122, 1.000000000000000000, 0.9659258262890683122, 1.000000000000000000, 0.9659258262890683122, 1.000000000000000000, 0.9659258262890683122, 1.000000000000000000, 0.9659258262890683122, 1.000000000000000000, 0.9659258262890683122, 1.000000000000000000, 0.9659258262890683122, 1.000000000000000000, 0.9659258262890683122, 1.000000000000000000, 0.9659258262890683122, 1.000000000000000000, 0.9659258262890683122, 1.000000000000000000, 0.9659258262890683122, 1.000000000000000000, 0.9659258262890683122, 1.000000000000000000, 0.9659258262890683122, 1.000000000000000000, 0.9659258262890683122, 1.000000000000000000, 0.9659258262890683122, 1.000000000000000000, 0.9659258262890683122, 1.000000000000000000, 0.9659258262890683122, 1.000000000000000000, 0.9659258262890683122, 1.000000000000000000, 0.9659258262890683122, 1.000000000000000000, 0.9659258262890683122, 1.000000000000000000, 0.9659258262890683122, 1.000000000000000000, 0.9659258262890683122, 1.000000000000000000, 0.9659258262890683122, 1.000000000000000000, 0.9659258262890683122, 1.000000000000000000, 0.9659258262890683122, 1.000000000000000000, 0.9659258262890683122, 1.000000000000000000, 0.9659258262890683122, 1.000000000000000000, 0.9659258262890683122, 1.000000000000000000, 0.9659258262890683122, 1.000000000000000000, 0.9659258262890683122, 1.000000000000000000, 0.9659258262890683122, 1.000000000000000000, 0.9659258262890683122, 1.000000000000000000, 0.9659258262890683122, 1.000000000000000000, 0.9659258262890683122, 1.000000000000000000, 0.9659258262890683122, 1.000000000000000000, 0.9659258262890683122, 1.000000000000000000, 0.9659258262890683122, 1.000000000000000000, 0.9659258262890683122, 1.000000000000000000, 0.9659258262890683122, 1.000000000000000000, 0.9659258262890683122, 1.000000000000000000, 0.9659258262890683122, 1.000000000000000000, 0.9659258262890683122, 1.000000000000000000, 0.9659258262890683122, 1.000000000000000000, 0.9659258262890683122, 1.000000000000000000, 0.9659258262890683122, 1.000000000000000000, 0.9659258262890683122, 1.000000000000000000, 0.9659258262890683122, 1.000000000000000000, 0.9659258262890683122, 1.000000000000000000, 0.9659258262890683122, 1.000000000000000000, 0.9659258262890683122, 1.000000000000000000, 0.9659258262890683122, 1.000000000000000000, 0.9659258262890683122, 1.000000000000000000, 0.9659258262890683122, 1.000000000000000000, 0.9659258262890683122, 1.000000000000000000, 0.9659258262890683122, 1.000000000000000000, 0.9659258262890683122, 1.000000000000000000, 0.9659258262890683122, 1.000000000000000000, 0.9659258262890683122, 1.000000000000000000, 0.9659258262890683122, 1.000000000000000000, 0.9659258262890683122, 1.000000000000000000, 0.9659258262890683122, 1.000000000000000000, 0.9659258262890683122, 1.000000000000000000, 0.9659258262890683122, 1.000000000000000000, 0.9659258262890683122, 1.000000000000000000, 0.9659258262890683122, 1.000000000000000000, 0.9659258262890683122, 1.000000000000000000, 0.9659258262890683122, 1.000000000000000000, 0.9659258262890683122, 1.000000000000000000, 0.9659258262890683122, 1.000000000000000000, 0.9659258262890683122, 1.000000000000000000, 0.9659258262890683122, 1.000000000000000000, 0.9659258262890683122, 1.000000000000000000, 0.9659258262890683122, 1.000000000000000000, 0.9659258262890683122, 1.000000000000000000, 0.9659258262890683122, 1.000000000000000000, 0.9659258262890683122, 1.000000000000000000, 0.9659258262890683122, 1.000000000000000000, 0.9659258262890683122, 1.000000000000000000, 0.9659258262890683122, 1.000000000000000000, 0.9659258262890683122, 1.000000000000000000, 0.9659258262890683122, 1.000000000000000000, 0.9659258262890683122, 1.000000000000000000, 0.9659258262890683122, 1.000000000000000000, 0.9659258262890683122, 1.000000000000000000, 0.9659258262890683122, 1.000000000000000000, 0.9659258262890683122, 1.000000000000000000, 0.9659258262890683122, 1.000000000000000000, 0.9659258262890683122, 1.000000000000000000, 0.9659258262890683122, 1.000000000000000000, 0.9659258262890683122, 1.000000000000000000, 0.9659258262890683122, 1.000000000000000000, 0.9659258262890683122, 1.000000000000000000, 0.9659258262890683122, 1.000000000000000000, 0.9659258262890683122, 1.000000000000000000, 0.9659258262890683122, 1.000000000000000000, 0.9659258262890683122, 1.000000000000000000, 0.9659258262890683122, 1.000000000000000000, 0.9659258262890683122, 1.000000000000000000, 0.9659258262890683122, 1.000000000000000000, 0.9659258262890683122, 1.000000000000000000, 0.9659258262890683122, 1.000000000000000000, 0.9659258262890683122, 1.000000000000000000, 0.9659258262890683122, 1.000000000000000000, 0.9659258262890683122, 1.000000000000000000) ) ) 
 REPRESENTATION_ITEM ( '' )  SURFACE ( )  );
#11193 = AXIS2_PLACEMENT_3D ( 'NONE', #3376, #68188, #54710 ) ;
#11194 = CARTESIAN_POINT ( 'NONE',  ( -0.8136482939632537770, 0.1283753931104746893, -0.1820866141732285504 ) ) ;
#11195 = CARTESIAN_POINT ( 'NONE',  ( -1.181102362204723644, -0.1870078740157480601, -0.3641732283464567677 ) ) ;
#11196 = CARTESIAN_POINT ( 'NONE',  ( 0.6496062992125991586, 0.1660481256975885056, 0.3530559997133364547 ) ) ;
#11197 = CARTESIAN_POINT ( 'NONE',  ( -1.279527559055116948, 0.1660481256975883668, -0.3530559997133364547 ) ) ;
#11198 = CARTESIAN_POINT ( 'NONE',  ( 0.2867679344610365999, -0.2867679344610365444, -0.2480314960629920740 ) ) ;
#11199 = ORIENTED_EDGE ( 'NONE', *, *, #24920, .F. ) ;
#11200 = CARTESIAN_POINT ( 'NONE',  ( 1.391076115485564868, -0.6046776061558807314, 0.2411417322834647770 ) ) ;
#11201 = CARTESIAN_POINT ( 'NONE',  ( 0.000000000000000000, 0.000000000000000000, -1.512162153811850596 ) ) ;
#11202 =( NAMED_UNIT ( * ) PLANE_ANGLE_UNIT ( ) SI_UNIT ( $, .RADIAN. ) );
#11203 = CARTESIAN_POINT ( 'NONE',  ( 5.785732909357575061E-17, -0.4724409448818898682, -1.811023622047244208 ) ) ;
#11204 = DIRECTION ( 'NONE',  ( -1.000000000000000000, 0.000000000000000000, 0.000000000000000000 ) ) ;
#11205 = CARTESIAN_POINT ( 'NONE',  ( -0.4091458600556405756, 0.2362204724409446288, -0.9711286089238845287 ) ) ;
#11206 = CARTESIAN_POINT ( 'NONE',  ( -1.049868766404198794, -0.6046776061558807314, 0.2411417322834647770 ) ) ;
#11207 = CARTESIAN_POINT ( 'NONE',  ( 1.161417322834646493, -0.5400638737290844871, 0.3530559997133364547 ) ) ;
#11209 = CARTESIAN_POINT ( 'NONE',  ( 0.3458507752293908943, -0.3458507752293908943, -1.988188976377952777 ) ) ;
#11208 = DIRECTION ( 'NONE',  ( 0.000000000000000000, 0.000000000000000000, 1.000000000000000000 ) ) ;
#11210 = CARTESIAN_POINT ( 'NONE',  ( -1.725721784776902190, -0.05778040916215522460, 0.4822834645669289988 ) ) ;
#11211 = CARTESIAN_POINT ( 'NONE',  ( -1.200787401574802349, 0.1660481256975883668, -0.3530559997133364547 ) ) ;
#11212 = CARTESIAN_POINT ( 'NONE',  ( -0.3392501089628018329, -0.1958661417322836440, -0.4474872458979509138 ) ) ;
#11213 = CARTESIAN_POINT ( 'NONE',  ( 0.1968503937007881344, 0.1771653543307087630, 0.000000000000000000 ) ) ;
#11214 = CARTESIAN_POINT ( 'NONE',  ( 0.1958661417322834775, 0.3392501089628018884, -1.016404199475065662 ) ) ;
#11215 = CARTESIAN_POINT ( 'NONE',  ( -0.1246719160104980823, -0.5511811023622048555, -0.09757992244046775898 ) ) ;
#11216 = CARTESIAN_POINT ( 'NONE',  ( 0.4921259842519691285, 0.07958543189024085140, 0.2665933059059887866 ) ) ;
#11217 = CARTESIAN_POINT ( 'NONE',  ( 0.5183727034120741983, 0.2952755905511810774, -0.1292274648535930714 ) ) ;
#11218 = CARTESIAN_POINT ( 'NONE',  ( -0.6889763779527552368, 0.07958543189024085140, 0.2665933059059887866 ) ) ;
#11219 = CARTESIAN_POINT ( 'NONE',  ( -9.594673741351313045E-17, 0.3917322834645670104, -2.196850393700787496 ) ) ;
#11220 = CARTESIAN_POINT ( 'NONE',  ( 1.476377952755906220, 0.1660481256975883668, -0.3530559997133364547 ) ) ;
#11221 = CARTESIAN_POINT ( 'NONE',  ( -0.8333333333333323711, 0.2952755905511811885, 0.1292274648535926551 ) ) ;
#11222 = CARTESIAN_POINT ( 'NONE',  ( 0.1265901696524989462, 0.4724409448818897572, -0.7001312335958002064 ) ) ;
#11223 = B_SPLINE_CURVE_WITH_KNOTS ( 'NONE', 3,
 ( #58700, #1066, #78081, #72176 ),
 .UNSPECIFIED., .F., .F.,
 ( 4, 4 ),
 ( 0.07239528109754661545, 0.07258229963060301715 ),
 .UNSPECIFIED. ) ;
#11224 = CARTESIAN_POINT ( 'NONE',  ( -0.1509186351706028884, -0.05778040916215522460, 0.4822834645669289988 ) ) ;
#11225 = CARTESIAN_POINT ( 'NONE',  ( -0.7086614173228339419, -0.1870078740157479769, 0.4822834645669291653 ) ) ;
#11226 = CARTESIAN_POINT ( 'NONE',  ( 1.154855643044620184, -0.5023911411419708095, 0.1820866141732285504 ) ) ;
#11227 = CARTESIAN_POINT ( 'NONE',  ( -0.03937007874015669567, -0.5511811023622047445, 6.969142054262312111E-17 ) ) ;
#11228 = CARTESIAN_POINT ( 'NONE',  ( -0.1902887139107604098, -0.6692913385826771977, 0.1292274648535927661 ) ) ;
#11229 = CARTESIAN_POINT ( 'NONE',  ( -1.325459317585300889, 0.05413385826771666132, 0.4176697321401328100 ) ) ;
#11230 = CARTESIAN_POINT ( 'NONE',  ( -3.870235431238101764, 2.740199102106095186, 0.5314960629921260393 ) ) ;
#11231 = CARTESIAN_POINT ( 'NONE',  ( 1.673228346456693494, 0.07958543189024085140, 0.2665933059059887866 ) ) ;
#11232 = CONICAL_SURFACE ( 'NONE', #19260, 3.228346456692913424, 0.7853981633974500554 ) ;
#11233 = CARTESIAN_POINT ( 'NONE',  ( -0.2427821522309703550, -0.3162353388693405765, 0.4822834645669290543 ) ) ;
#11234 = ORIENTED_EDGE ( 'NONE', *, *, #4397, .F. ) ;
#11235 = CARTESIAN_POINT ( 'NONE',  ( -0.2925321140481930149, -0.2925321140481933480, -2.025590551181101873 ) ) ;
#11236 = CARTESIAN_POINT ( 'NONE',  ( 0.9580052493438326877, 0.05413385826771666132, 0.4176697321401328100 ) ) ;
#11237 = CARTESIAN_POINT ( 'NONE',  ( -0.7152230971128602510, -0.08942795157528024563, -0.3641732283464568787 ) ) ;
#11238 = CARTESIAN_POINT ( 'NONE',  ( -0.6430446194225716283, -0.4281496062992124485, 0.4176697321401328655 ) ) ;
#11239 = CARTESIAN_POINT ( 'NONE',  ( 1.076115485564305141, 0.2306618581243847221, -0.2411417322834647770 ) ) ;
#11240 = CARTESIAN_POINT ( 'NONE',  ( 0.7217847769028878924, 0.05413385826771666132, 0.4176697321401328100 ) ) ;
#11241 = DIRECTION ( 'NONE',  ( 0.000000000000000000, 0.000000000000000000, 1.000000000000000000 ) ) ;
#11242 = CARTESIAN_POINT ( 'NONE',  ( -1.128608923884513837, -0.5023911411419708095, 0.1820866141732285504 ) ) ;
#11244 = EDGE_CURVE ( 'NONE', #35624, #32899, #23598, .T. ) ;
#11243 = CARTESIAN_POINT ( 'NONE',  ( -0.1070741851644057135, 0.3996062992125984925, -0.08333333333333335646 ) ) ;
#11245 = CARTESIAN_POINT ( 'NONE',  ( -0.1998031496062994683, 0.3460692066303958092, -0.6430446194225721834 ) ) ;
#11246 = VECTOR ( 'NONE', #43428, 39.37007874015748143 ) ;
#11247 = CARTESIAN_POINT ( 'NONE',  ( 0.3420746716998660508, -0.1974969037888703871, -0.2624671916010499206 ) ) ;
#11248 = CARTESIAN_POINT ( 'NONE',  ( 0.4698424923132817899, 1.469648236684818476, 2.565231856145545830 ) ) ;
#11249 = CARTESIAN_POINT ( 'NONE',  ( 0.03143970413924662005, -0.3977953519386796533, -5.548669992249399297E-14 ) ) ;
#11250 = CARTESIAN_POINT ( 'NONE',  ( 0.6889763779527563470, 0.07958543189024071263, -0.2665933059059888421 ) ) ;
#11251 = CARTESIAN_POINT ( 'NONE',  ( 0.3477690288713918276, 0.2952755905511811885, 0.1292274648535926551 ) ) ;
#11252 = CARTESIAN_POINT ( 'NONE',  ( 0.2198823481317033202, -0.1972978822260922083, 0.1376690760605703834 ) ) ;
#11253 = CARTESIAN_POINT ( 'NONE',  ( -9.674558042662122972E-17, 0.3949938075777409963, -0.7066929133858269596 ) ) ;
#11254 = CARTESIAN_POINT ( 'NONE',  ( 0.7217847769028878924, -0.004921259842519576551, 0.3153832671262227771 ) ) ;
#11255 = CARTESIAN_POINT ( 'NONE',  ( -0.1574803149606292529, -0.1870078740157480879, -0.4822834645669291653 ) ) ;
#11256 = CARTESIAN_POINT ( 'NONE',  ( -0.9580052493438311334, 0.05413385826771626580, -0.4176697321401330321 ) ) ;
#11257 = CARTESIAN_POINT ( 'NONE',  ( 1.423884514435696413, -0.3162353388693409650, -0.4822834645669289433 ) ) ;
#11258 = CARTESIAN_POINT ( 'NONE',  ( 0.4091458600556403535, 0.2362204724409449896, -1.076115485564304475 ) ) ;
#11259 = CARTESIAN_POINT ( 'NONE',  ( 0.1070741851644053666, 0.3996062992125986035, -2.513123359580052174 ) ) ;
#11260 = CARTESIAN_POINT ( 'NONE',  ( -0.2755905511811018171, 0.1771653543307087630, 0.000000000000000000 ) ) ;
#11261 = ORIENTED_EDGE ( 'NONE', *, *, #75321, .F. ) ;
#11262 = CARTESIAN_POINT ( 'NONE',  ( -0.3392501089628019995, 0.1958661417322831999, -0.8103867698500807348 ) ) ;
#11263 = ORIENTED_EDGE ( 'NONE', *, *, #64557, .T. ) ;
#11264 = CARTESIAN_POINT ( 'NONE',  ( -1.056430446194224881, 0.2952755905511810774, -0.1292274648535930714 ) ) ;
#11265 = CARTESIAN_POINT ( 'NONE',  ( -0.2165354330708654795, 0.1660481256975885056, 0.3530559997133364547 ) ) ;
#11266 = CARTESIAN_POINT ( 'NONE',  ( -0.4002624671916004129, -0.3162353388693405765, 0.4822834645669290543 ) ) ;
#11267 = CARTESIAN_POINT ( 'NONE',  ( 0.3083989501312343062, -0.05778040916215560624, -0.4822834645669293319 ) ) ;
#11268 = CARTESIAN_POINT ( 'NONE',  ( -0.2624671916010490880, -0.6046776061558807314, 0.2411417322834647770 ) ) ;
#11269 = CARTESIAN_POINT ( 'NONE',  ( -1.240157480314959759, -0.5400638737290845981, -0.3530559997133363437 ) ) ;
#11270 = CARTESIAN_POINT ( 'NONE',  ( -0.9120734908136475250, 0.2952755905511811885, 0.1292274648535926551 ) ) ;
#11271 = CARTESIAN_POINT ( 'NONE',  ( 0.9514435695538062676, -0.05778040916215522460, 0.4822834645669289988 ) ) ;
#11272 = CARTESIAN_POINT ( 'NONE',  ( 0.1049643490035304938, -0.3917322834645669549, -0.8648293963254591876 ) ) ;
#11273 = CARTESIAN_POINT ( 'NONE',  ( -0.5511811023622038563, -0.1870078740157479769, 0.3641732283464567677 ) ) ;
#11274 = ORIENTED_EDGE ( 'NONE', *, *, #61486, .T. ) ;
#11275 = CARTESIAN_POINT ( 'NONE',  ( 0.1974969037888706369, -0.3420746716998659953, -1.509186351706036655 ) ) ;
#11276 = ORIENTED_EDGE ( 'NONE', *, *, #37551, .F. ) ;
#11277 = CARTESIAN_POINT ( 'NONE',  ( -1.377952755905511140, 0.1771653543307087630, 0.000000000000000000 ) ) ;
#11278 = CARTESIAN_POINT ( 'NONE',  ( -0.9317585301837263412, -0.4281496062992127816, -0.4176697321401328100 ) ) ;
#11279 = CARTESIAN_POINT ( 'NONE',  ( -0.8464566929133852113, 0.1660481256975885056, 0.3530559997133364547 ) ) ;
#11280 = CARTESIAN_POINT ( 'NONE',  ( -0.3460692066303960868, 0.1998031496062990242, 0.1312335958005249048 ) ) ;
#11281 = CARTESIAN_POINT ( 'NONE',  ( -0.8923884514435688198, 0.2306618581243847221, -0.2411417322834647770 ) ) ;
#11282 = CARTESIAN_POINT ( 'NONE',  ( -0.8333333333333323711, -0.6692913385826773087, -0.1292274648535924053 ) ) ;
#11283 = CARTESIAN_POINT ( 'NONE',  ( -1.522309711286088607, -0.6046776061558807314, 0.2411417322834647770 ) ) ;
#11284 = DIRECTION ( 'NONE',  ( 1.445602896647338917E-16, 1.000000000000000000, 0.000000000000000000 ) ) ;
#11285 = CARTESIAN_POINT ( 'NONE',  ( 0.5577427821522316087, -0.08942795157527998196, 0.3641732283464567121 ) ) ;
#11286 = DIRECTION ( 'NONE',  ( -0.000000000000000000, -0.000000000000000000, -1.000000000000000000 ) ) ;
#11287 = CARTESIAN_POINT ( 'NONE',  ( -0.3917322834645671215, 0.1049643490035301469, 0.1975065616797899160 ) ) ;
#11288 = CARTESIAN_POINT ( 'NONE',  ( 0.1049868766404206816, -0.5023911411419708095, -0.1820866141732282451 ) ) ;
#11289 = AXIS2_PLACEMENT_3D ( 'NONE', #46326, #65295, #21910 ) ;
#11290 = CARTESIAN_POINT ( 'NONE',  ( -0.4593175853018364174, -0.4281496062992127816, -0.4176697321401328100 ) ) ;
#11291 = CARTESIAN_POINT ( 'NONE',  ( 1.587926509186352142, 0.05413385826771666132, 0.4176697321401328100 ) ) ;
#11292 = CARTESIAN_POINT ( 'NONE',  ( -0.06561679790026180015, 0.05413385826771666132, 0.4176697321401328100 ) ) ;
#11293 = ORIENTED_EDGE ( 'NONE', *, *, #75428, .T. ) ;
#11294 = CARTESIAN_POINT ( 'NONE',  ( 0.3460692066303959757, -0.1998031496062991907, -2.152230971128608950 ) ) ;
#11295 = CARTESIAN_POINT ( 'NONE',  ( -0.5636006452641416642, -2.613618158232546091E-15, -0.3464511005275220379 ) ) ;
#11296 = VERTEX_POINT ( 'NONE', #57857 ) ;
#11297 = CARTESIAN_POINT ( 'NONE',  ( 0.2925321140481932369, 0.2925321140481932369, -1.631889763779527325 ) ) ;
#11298 = CARTESIAN_POINT ( 'NONE',  ( 0.6299212598425341092, 1.724409448818898127, -3.937007874015759690 ) ) ;
#11299 = CARTESIAN_POINT ( 'NONE',  ( -0.9120734908136475250, 0.1771653543307087630, 0.09757992244046791164 ) ) ;
#11300 = CARTESIAN_POINT ( 'NONE',  ( -0.9645669291338575535, -0.5400638737290844871, 0.3530559997133364547 ) ) ;
#11301 = CARTESIAN_POINT ( 'NONE',  ( -0.2362204724409451284, 0.4091458600556402425, -0.3280839895013123453 ) ) ;
#11302 = CARTESIAN_POINT ( 'NONE',  ( -0.4029579088642626372, 1.286547554808001648, 3.916341449869456426 ) ) ;
#11303 = CARTESIAN_POINT ( 'NONE',  ( -0.3917322834645670104, -7.196005306013484475E-17, -0.03149606299212594218 ) ) ;
#11304 = CARTESIAN_POINT ( 'NONE',  ( 1.154855643044620184, -0.6046776061558807314, 0.2411417322834647770 ) ) ;
#11305 = CARTESIAN_POINT ( 'NONE',  ( 0.3740157480314966754, 0.1660481256975883668, -0.3530559997133364547 ) ) ;
#11306 = CARTESIAN_POINT ( 'NONE',  ( 0.7086614173228353852, -0.1870078740157479769, 0.4822834645669291653 ) ) ;
#11307 = CARTESIAN_POINT ( 'NONE',  ( -1.003937007874014853, 0.07958543189024085140, 0.2665933059059887866 ) ) ;
#11308 = CARTESIAN_POINT ( 'NONE',  ( -0.3937007874015740483, -0.1870078740157480879, -0.4822834645669291653 ) ) ;
#11309 = CARTESIAN_POINT ( 'NONE',  ( -0.2362204724409451284, 0.4091458600556402425, -2.452099737532808188 ) ) ;
#11310 = CARTESIAN_POINT ( 'NONE',  ( -0.8333333333333323711, -0.6692913385826773087, -0.1292274648535924053 ) ) ;
#11311 = CARTESIAN_POINT ( 'NONE',  ( 0.3949938075777409408, -0.1058382717557499186, -2.235564304461942431 ) ) ;
#11312 = CARTESIAN_POINT ( 'NONE',  ( 1.128608923884514947, 0.1283753931104748280, 0.1820866141732283561 ) ) ;
#11313 = CARTESIAN_POINT ( 'NONE',  ( -0.4986876640419942164, -0.5023911411419708095, 0.1820866141732285504 ) ) ;
#11314 = CARTESIAN_POINT ( 'NONE',  ( 1.108923884514436686, -0.2845877964562161244, -0.3641732283464567121 ) ) ;
#11315 = CARTESIAN_POINT ( 'NONE',  ( 1.574803149606299746, -0.1870078740157479769, 0.3641732283464567677 ) ) ;
#11316 = CARTESIAN_POINT ( 'NONE',  ( -1.108923884514435132, -0.08942795157528024563, -0.3641732283464568787 ) ) ;
#11317 = CARTESIAN_POINT ( 'NONE',  ( 0.1455472725388437250, -8.032016466602779066E-18, -0.3627985898453512936 ) ) ;
#11318 = CARTESIAN_POINT ( 'NONE',  ( 0.4855643044619430415, -0.3690944881889765550, -0.3153832671262227771 ) ) ;
#11319 = CARTESIAN_POINT ( 'NONE',  ( -0.5380577427821514602, 0.05413385826771666132, 0.4176697321401328100 ) ) ;
#11320 =( BOUNDED_SURFACE ( )  B_SPLINE_SURFACE ( 1, 2, ( 
 ( #11502, #23286, #24110, #48956, #74657, #17001, #24927, #6409, #31247, #38811, #50595, #5992, #51418, #7248, #32495, #57740, #19881, #19035, #38392, #18632, #44682, #32920, #76303, #51003, #51842, #26180, #70810, #64488, #37567, #12320, #64911, #63653, #77120, #58159, #44276, #77549, #32079, #6826, #13160, #69966, #37978, #31663, #527, #57324, #76702, #71228, #52261, #45530, #102, #83018, #58586, #13572, #39226, #69565, #954, #25756, #25341, #19453, #45104, #70378, #12733, #26609, #77967, #43866, #11913, #63241, #5581, #56913, #82609, #64072, #53518, #34596, #1366, #2610, #66167, #66583, #47202, #27018, #46369, #65760, #8919, #8093, #27433, #47618, #28686, #40902, #8507, #52679, #9335, #28267, #15661, #45946, #53929, #34173, #78387, #59837, #2190, #53095, #78805, #21959, #41322, #79641, #72892, #15242, #65343, #67003, #7680, #73314, #27859, #60261, #40489, #60671, #20297, #35006, #3019, #54347, #33757, #33349, #79225, #20718, #71644, #13995, #39652, #59011, #14422, #72063, #40073, #21541, #59419, #21134, #1775, #46789, #72480, #14829, #30746, #41719, #16073, #35417, #3847, #81704, #54767, #74560, #37057, #42134, #16906, #35833, #55168, #81286, #42544, #68247, #55576, #73738, #49271, #36640, #17723, #61500, #49682, #62316, #74143, #29507, #23189, #61908, #16488, #67412, #9746, #11400, #24014, #67829, #80877, #80058, #29912, #48860, #61082, #10581, #3433, #74974, #29095, #10168, #4250, #43349, #68641, #36238, #55992, #23602, #17319, #80471, #42947, #69051, #22783, #10980, #4653, #30326, #75374, #62741, #48443, #5077, #22376, #48036, #38711, #51740, #82108, #64389, #70281, #31147, #18939, #12634, #5892, #31564, #58058, #77443, #32395, #25658, #6, #18129, #19776, #43762, #26080, #38293, #51320, #76609, #13468, #56409, #45430, #71125, #39125, #69873, #69467, #63970, #37472, #6725, #64806, #7145, #24421, #50497, #77023, #50091, #6306, #57643, #57222, #12226, #31983, #75787, #424, #11820, #63145, #5486, #56813, #63558, #82512, #24828, #50908, #76200, #18538, #44587, #37883, #82923, #19356, #45005, #70705, #13057, #44181, #25244, #72791, #53827, #71965, #2511, #15141, #26918, #65668, #59321, #14734, #52578, #77865, #20194, #47518, #60159, #20618, #33658, #66907, #66069, #1677, #13891, #78707, #45845, #27755, #39550, #78287, #40386, #79541, #21445, #46691, #8817, #7994, #27334, #7577, #52994, #21854, #65239, #39978, #40797, #66482, #59736, #53419, #26507, #1270, #73210, #46270, #8405, #47102, #33249, #34494, #21031, #79128, #2090, #58911, #14320, #72384, #28170, #34072, #15560, #41220, #32818, #58485, #850, #52161, #71544, #54662, #74879, #17223, #55896, #54244, #80373, #67730, #73637, #42855, #29819, #15979, #28996, #41626, #67315, #23094, #68548, #62225, #2924, #80778, #28588, #48761, #60982, #10889, #74042, #9650, #47934, #74460, #68143, #35319, #22686, #3332, #81608, #4563, #79961, #48345, #49590, #10065, #36549, #23924, #16389, #10488, #42036, #22274, #35728, #61398, #30234, #3747, #16807, #29411, #55070, #9238, #60573, #34910, #75285, #42443, #43260, #17628, #36142, #55480, #61814, #4154, #81190, #23507, #49174, #82825, #38613, #11728, #19251, #37384, #38196, #5798, #18847, #6209, #44903, #50000, #31468, #32297, #69375, #18449, #64291, #68957, #44091, #44493, #69785, #43672, #11307, #50408, #51225, #5393, #75697, #63871, #6625, #25558, #70184, #50817, #70601, #12955, #57957, #37787, #31886, #31055, #76106, #57130, #12130, #56318, #325, #82421, #76923, #25979, #12537, #24330, #19671, #51637, #25149, #63464, #76518, #77342, #57546, #83237, #36966, #62643, #63055, #4987, #30654, #82016, #56724, #18038, #24740, #33558, #20518, #32717, #60057, #58813, #1991, #72695, #46589, #745, #79436, #79029, #59221, #52479, #27237, #15042, #1582, #72287, #40698, #65563, #26404, #45332, #14633, #7897, #2412, #71027, #8720, #34391, #28070, #1170, #58384, #52896, #52060, #27654, #53728, #66383, #13371, #39449, #40289, #39024, #78609, #65970, #46170, #26821, #20932, #64708, #21348, #7048, #77766, #20098, #45749, #78187, #47001, #71444, #39874, #13792, #7473, #8307 ),
 ( #65137, #33974, #33142, #71866, #14216, #59635, #53317, #81091, #79858, #55796, #17124, #16292, #42345, #21755, #54561, #41118, #9963, #61295, #35634, #74775, #47833, #55385, #73538, #74361, #41936, #54977, #68043, #23408, #2823, #67632, #68453, #22175, #80276, #42758, #47418, #22590, #80684, #48251, #15883, #73109, #3235, #4056, #41531, #28484, #16704, #10792, #61718, #22998, #3651, #49075, #36452, #62126, #73947, #10389, #67217, #28899, #29316, #48663, #15460, #36046, #29723, #4468, #60884, #30133, #66808, #9550, #9142, #34813, #60472, #35220, #54144, #68858, #12853, #25455, #69274, #82321, #32198, #31364, #50307, #62541, #43988, #11207, #76415, #4879, #43573, #5693, #44800, #70081, #12027, #57443, #56621, #76005, #56219, #24640, #70495, #30553, #5294, #6108, #63768, #25043, #18745, #75185, #49900, #19149, #17937, #57029, #12434, #81917, #31781, #69684, #44388, #50717, #24228, #75598, #11620, #38094, #37282, #30954, #51122, #6528, #83136, #37684, #62957, #38511, #76817, #64193, #23824, #81503, #63359, #18347, #82723, #49493, #17531, #43162, #36866, #78917, #33866, #27129, #1475, #19566, #52793, #70926, #13272, #57854, #78503, #78079, #14935, #221, #21238, #46894, #40594, #71338, #45226, #65457, #38924, #40182, #72588, #27547, #8616, #51955, #20825, #66276, #7789, #59118, #33029, #13685, #14109, #25872, #8201, #51534, #64604, #77237, #6940, #65025, #59530, #32612, #52371, #58274, #19992, #20411, #39338, #58698, #46478, #46062, #65866, #72174, #639, #77661, #26295, #45643, #71755, #1887, #53204, #7360, #39761, #1063, #33456, #26717, #14531, #15776, #9033, #73000, #22485, #9858, #34706, #54037, #60368, #23304, #3958, #21650, #79750, #74673, #9441, #61616, #80991, #2716, #35528, #28376, #79330, #60778, #47310, #29621, #22067, #48148, #15352, #67110, #34286, #2303, #59947, #10279, #47727, #68356, #55281, #28794, #54878, #27963, #35112, #53622, #73844, #16184, #41831, #48974, #73425, #67938, #41426, #3545, #54457, #67521, #80585, #35946, #41014, #80170, #17018, #3129, #61190, #42658, #66699, #29212, #22891, #48559, #74257, #16598, #42243, #77456, #30446, #17430, #6738, #7160, #51753, #43885, #75905, #45443, #71139, #32831, #62855, #32409, #56111, #17837, #82223, #69168, #81401, #26520, #24127, #19791, #39138, #13070, #49388, #45859, #13481, #24543, #43472, #18244, #64819, #50207, #38725, #43061, #5191, #69583, #10695, #64402, #58072, #11101, #36350, #68758, #81817, #58499, #863, #52175, #55693, #49796, #11519, #75083, #62026, #4362, #77878, #36758, #30030, #20209, #30856, #438, #23717, #37175, #62434, #26093, #4771, #75498, #56521, #20632, #66496, #46283, #27768, #46704, #34086, #79141, #8830, #26932, #72397, #53841, #71979, #1691, #60170, #71557, #53007, #59749, #27349, #14333, #13906, #78720, #34507, #65681, #78300, #21458, #79554, #2525, #2103, #53433, #28183, #21867, #47532, #14747, #47116, #8008, #21045, #66082, #40401, #1283, #73223, #59334, #15574, #39564, #72805, #39991, #65253, #7590, #15154, #8418, #40811, #33262, #58924, #52593, #33672, #36466, #37298, #68873, #17952, #11221, #5710, #48680, #12043, #37701, #31380, #62141, #36061, #56235, #29737, #30969, #63374, #18363, #82739, #42772, #75614, #57045, #81932, #49916, #23840, #4480, #4896, #74376, #82337, #16719, #10404, #68058, #4070, #55812, #50323, #23424, #43176, #42360, #10806, #36881, #30150, #49507, #43589, #62559, #30569, #24243, #61733, #69290, #5311, #69700, #81519, #44006, #56636, #68468, #75200, #17544, #11638, #62972, #55400, #81107, #49089, #24655, #76021, #74790, #17140, #13288, #44404, #38940, #76833, #33048, #6543, #83152, #63785, #64621, #657, #25472, #44815, #51139, #14128, #78097, #12450, #70512, #65475, #239, #52388, #71774, #19167, #26313, #12869, #70098, #51551, #38111, #20428, #38527, #6958, #6124, #57872, #25059, #76432, #50733, #1082, #64209, #59136, #46081, #19584, #45660, #18761, #25891, #31797, #32629, #58292, #51972, #39781, #32213, #58718, #77254, #77679, #45244, #20009, #71356, #26734, #57459, #70943, #7808, #13703, #39358, #33474, #65043, #7380, #34726, #34305 ) ),
 .UNSPECIFIED., .F., .F., .F. ) 
 B_SPLINE_SURFACE_WITH_KNOTS ( ( 2, 2 ),
 ( 3, 2, 2, 2, 2, 2, 2, 2, 2, 2, 2, 2, 2, 2, 2, 2, 2, 2, 2, 2, 2, 2, 2, 2, 2, 2, 2, 2, 2, 2, 2, 2, 2, 2, 2, 2, 2, 2, 2, 2, 2, 2, 2, 2, 2, 2, 2, 2, 2, 2, 2, 2, 2, 2, 2, 2, 2, 2, 2, 2, 2, 2, 2, 2, 2, 2, 2, 2, 2, 2, 2, 2, 2, 2, 2, 2, 2, 2, 2, 2, 2, 2, 2, 2, 2, 2, 2, 2, 2, 2, 2, 2, 2, 2, 2, 2, 2, 2, 2, 2, 2, 2, 2, 2, 2, 2, 2, 2, 2, 2, 2, 2, 2, 2, 2, 2, 2, 2, 2, 2, 2, 2, 2, 2, 2, 2, 2, 2, 2, 2, 2, 2, 2, 2, 2, 2, 2, 2, 2, 2, 2, 2, 2, 2, 2, 2, 2, 2, 2, 2, 2, 2, 2, 2, 2, 2, 2, 2, 2, 2, 2, 2, 2, 2, 2, 2, 2, 2, 2, 2, 2, 2, 2, 2, 2, 2, 2, 2, 2, 2, 2, 2, 2, 2, 2, 2, 2, 2, 2, 2, 2, 2, 2, 2, 2, 2, 2, 2, 2, 2, 2, 2, 2, 2, 2, 2, 2, 2, 2, 2, 2, 2, 2, 2, 2, 2, 2, 2, 2, 2, 2, 2, 2, 2, 2, 2, 2, 2, 2, 2, 2, 2, 2, 2, 2, 2, 2, 2, 2, 2, 2, 2, 2, 2, 2, 2, 2, 2, 2, 2, 2, 2, 2, 2, 2, 3 ),
 ( 0.000000000000000000, 1.000000000000000000 ),
 ( 0.000000000000000000, 0.003787878787878787984, 0.007575757575757575968, 0.01136363636363636395, 0.01515151515151515194, 0.01893939393939393992, 0.02272727272727272790, 0.02651515151515151589, 0.03030303030303030387, 0.03409090909090908839, 0.03787878787878787984, 0.04166666666666666435, 0.04545454545454545581, 0.04924242424242424032, 0.05303030303030303177, 0.05681818181818181629, 0.06060606060606060774, 0.06439393939393939226, 0.06818181818181817677, 0.07196969696969697516, 0.07575757575757575968, 0.07954545454545454419, 0.08333333333333332871, 0.08712121212121212710, 0.09090909090909091161, 0.09469696969696969613, 0.09848484848484848064, 0.1022727272727272790, 0.1060606060606060635, 0.1098484848484848481, 0.1136363636363636326, 0.1174242424242424310, 0.1212121212121212155, 0.1250000000000000000, 0.1287878787878787845, 0.1325757575757575690, 0.1363636363636363535, 0.1401515151515151381, 0.1439393939393939503, 0.1477272727272727348, 0.1515151515151515194, 0.1553030303030303039, 0.1590909090909090884, 0.1628787878787878729, 0.1666666666666666574, 0.1704545454545454419, 0.1742424242424242542, 0.1780303030303030387, 0.1818181818181818232, 0.1856060606060606077, 0.1893939393939393923, 0.1931818181818181768, 0.1969696969696969613, 0.2007575757575757458, 0.2045454545454545581, 0.2083333333333333426, 0.2121212121212121271, 0.2159090909090909116, 0.2196969696969696961, 0.2234848484848484806, 0.2272727272727272652, 0.2310606060606060497, 0.2348484848484848619, 0.2386363636363636465, 0.2424242424242424310, 0.2462121212121212155, 0.2500000000000000000, 0.2537878787878787845, 0.2575757575757575690, 0.2613636363636363535, 0.2651515151515151381, 0.2689393939393939226, 0.2727272727272727071, 0.2765151515151514916, 0.2803030303030302761, 0.2840909090909091161, 0.2878787878787879007, 0.2916666666666666852, 0.2954545454545454697, 0.2992424242424242542, 0.3030303030303030387, 0.3068181818181818232, 0.3106060606060606077, 0.3143939393939393923, 0.3181818181818181768, 0.3219696969696969613, 0.3257575757575757458, 0.3295454545454545303, 0.3333333333333333148, 0.3371212121212120993, 0.3409090909090908839, 0.3446969696969697239, 0.3484848484848485084, 0.3522727272727272929, 0.3560606060606060774, 0.3598484848484848619, 0.3636363636363636465, 0.3674242424242424310, 0.3712121212121212155, 0.3750000000000000000, 0.3787878787878787845, 0.3825757575757575690, 0.3863636363636363535, 0.3901515151515151381, 0.3939393939393939226, 0.3977272727272727071, 0.4015151515151514916, 0.4053030303030302761, 0.4090909090909091161, 0.4128787878787879007, 0.4166666666666666852, 0.4204545454545454697, 0.4242424242424242542, 0.4280303030303030387, 0.4318181818181818232, 0.4356060606060606077, 0.4393939393939393923, 0.4431818181818181768, 0.4469696969696969613, 0.4507575757575757458, 0.4545454545454545303, 0.4583333333333333148, 0.4621212121212120993, 0.4659090909090908839, 0.4696969696969697239, 0.4734848484848485084, 0.4772727272727272929, 0.4810606060606060774, 0.4848484848484848619, 0.4886363636363636465, 0.4924242424242424310, 0.4962121212121212155, 0.5000000000000000000, 0.5037878787878787845, 0.5075757575757575690, 0.5113636363636363535, 0.5151515151515151381, 0.5189393939393939226, 0.5227272727272727071, 0.5265151515151514916, 0.5303030303030302761, 0.5340909090909090606, 0.5378787878787878451, 0.5416666666666666297, 0.5454545454545454142, 0.5492424242424241987, 0.5530303030303029832, 0.5568181818181817677, 0.5606060606060605522, 0.5643939393939394478, 0.5681818181818182323, 0.5719696969696970168, 0.5757575757575758013, 0.5795454545454545858, 0.5833333333333333703, 0.5871212121212121549, 0.5909090909090909394, 0.5946969696969697239, 0.5984848484848485084, 0.6022727272727272929, 0.6060606060606060774, 0.6098484848484848619, 0.6136363636363636465, 0.6174242424242424310, 0.6212121212121212155, 0.6250000000000000000, 0.6287878787878787845, 0.6325757575757575690, 0.6363636363636363535, 0.6401515151515151381, 0.6439393939393939226, 0.6477272727272727071, 0.6515151515151514916, 0.6553030303030302761, 0.6590909090909090606, 0.6628787878787878451, 0.6666666666666666297, 0.6704545454545454142, 0.6742424242424241987, 0.6780303030303029832, 0.6818181818181817677, 0.6856060606060605522, 0.6893939393939394478, 0.6931818181818182323, 0.6969696969696970168, 0.7007575757575758013, 0.7045454545454545858, 0.7083333333333333703, 0.7121212121212121549, 0.7159090909090909394, 0.7196969696969697239, 0.7234848484848485084, 0.7272727272727272929, 0.7310606060606060774, 0.7348484848484848619, 0.7386363636363636465, 0.7424242424242424310, 0.7462121212121212155, 0.7500000000000000000, 0.7537878787878787845, 0.7575757575757575690, 0.7613636363636363535, 0.7651515151515151381, 0.7689393939393939226, 0.7727272727272727071, 0.7765151515151514916, 0.7803030303030302761, 0.7840909090909090606, 0.7878787878787878451, 0.7916666666666666297, 0.7954545454545454142, 0.7992424242424241987, 0.8030303030303029832, 0.8068181818181817677, 0.8106060606060605522, 0.8143939393939394478, 0.8181818181818182323, 0.8219696969696970168, 0.8257575757575758013, 0.8295454545454545858, 0.8333333333333333703, 0.8371212121212121549, 0.8409090909090909394, 0.8446969696969697239, 0.8484848484848485084, 0.8522727272727272929, 0.8560606060606060774, 0.8598484848484848619, 0.8636363636363636465, 0.8674242424242424310, 0.8712121212121212155, 0.8750000000000000000, 0.8787878787878787845, 0.8825757575757575690, 0.8863636363636363535, 0.8901515151515151381, 0.8939393939393939226, 0.8977272727272727071, 0.9015151515151514916, 0.9053030303030302761, 0.9090909090909090606, 0.9128787878787878451, 0.9166666666666666297, 0.9204545454545454142, 0.9242424242424241987, 0.9280303030303029832, 0.9318181818181817677, 0.9356060606060605522, 0.9393939393939394478, 0.9431818181818182323, 0.9469696969696970168, 0.9507575757575758013, 0.9545454545454545858, 0.9583333333333333703, 0.9621212121212121549, 0.9659090909090909394 ),
 .UNSPECIFIED. ) 
 GEOMETRIC_REPRESENTATION_ITEM ( )  RATIONAL_B_SPLINE_SURFACE ( (
 ( 1.000000000000000000, 0.9659258262890683122, 1.000000000000000000, 0.9659258262890683122, 1.000000000000000000, 0.9659258262890683122, 1.000000000000000000, 0.9659258262890683122, 1.000000000000000000, 0.9659258262890683122, 1.000000000000000000, 0.9659258262890683122, 1.000000000000000000, 0.9659258262890683122, 1.000000000000000000, 0.9659258262890683122, 1.000000000000000000, 0.9659258262890683122, 1.000000000000000000, 0.9659258262890683122, 1.000000000000000000, 0.9659258262890683122, 1.000000000000000000, 0.9659258262890683122, 1.000000000000000000, 0.9659258262890683122, 1.000000000000000000, 0.9659258262890683122, 1.000000000000000000, 0.9659258262890683122, 1.000000000000000000, 0.9659258262890683122, 1.000000000000000000, 0.9659258262890683122, 1.000000000000000000, 0.9659258262890683122, 1.000000000000000000, 0.9659258262890683122, 1.000000000000000000, 0.9659258262890683122, 1.000000000000000000, 0.9659258262890683122, 1.000000000000000000, 0.9659258262890683122, 1.000000000000000000, 0.9659258262890683122, 1.000000000000000000, 0.9659258262890683122, 1.000000000000000000, 0.9659258262890683122, 1.000000000000000000, 0.9659258262890683122, 1.000000000000000000, 0.9659258262890683122, 1.000000000000000000, 0.9659258262890683122, 1.000000000000000000, 0.9659258262890683122, 1.000000000000000000, 0.9659258262890683122, 1.000000000000000000, 0.9659258262890683122, 1.000000000000000000, 0.9659258262890683122, 1.000000000000000000, 0.9659258262890683122, 1.000000000000000000, 0.9659258262890683122, 1.000000000000000000, 0.9659258262890683122, 1.000000000000000000, 0.9659258262890683122, 1.000000000000000000, 0.9659258262890683122, 1.000000000000000000, 0.9659258262890683122, 1.000000000000000000, 0.9659258262890683122, 1.000000000000000000, 0.9659258262890683122, 1.000000000000000000, 0.9659258262890683122, 1.000000000000000000, 0.9659258262890683122, 1.000000000000000000, 0.9659258262890683122, 1.000000000000000000, 0.9659258262890683122, 1.000000000000000000, 0.9659258262890683122, 1.000000000000000000, 0.9659258262890683122, 1.000000000000000000, 0.9659258262890683122, 1.000000000000000000, 0.9659258262890683122, 1.000000000000000000, 0.9659258262890683122, 1.000000000000000000, 0.9659258262890683122, 1.000000000000000000, 0.9659258262890683122, 1.000000000000000000, 0.9659258262890683122, 1.000000000000000000, 0.9659258262890683122, 1.000000000000000000, 0.9659258262890683122, 1.000000000000000000, 0.9659258262890683122, 1.000000000000000000, 0.9659258262890683122, 1.000000000000000000, 0.9659258262890683122, 1.000000000000000000, 0.9659258262890683122, 1.000000000000000000, 0.9659258262890683122, 1.000000000000000000, 0.9659258262890683122, 1.000000000000000000, 0.9659258262890683122, 1.000000000000000000, 0.9659258262890683122, 1.000000000000000000, 0.9659258262890683122, 1.000000000000000000, 0.9659258262890683122, 1.000000000000000000, 0.9659258262890683122, 1.000000000000000000, 0.9659258262890683122, 1.000000000000000000, 0.9659258262890683122, 1.000000000000000000, 0.9659258262890683122, 1.000000000000000000, 0.9659258262890683122, 1.000000000000000000, 0.9659258262890683122, 1.000000000000000000, 0.9659258262890683122, 1.000000000000000000, 0.9659258262890683122, 1.000000000000000000, 0.9659258262890683122, 1.000000000000000000, 0.9659258262890683122, 1.000000000000000000, 0.9659258262890683122, 1.000000000000000000, 0.9659258262890683122, 1.000000000000000000, 0.9659258262890683122, 1.000000000000000000, 0.9659258262890683122, 1.000000000000000000, 0.9659258262890683122, 1.000000000000000000, 0.9659258262890683122, 1.000000000000000000, 0.9659258262890683122, 1.000000000000000000, 0.9659258262890683122, 1.000000000000000000, 0.9659258262890683122, 1.000000000000000000, 0.9659258262890683122, 1.000000000000000000, 0.9659258262890683122, 1.000000000000000000, 0.9659258262890683122, 1.000000000000000000, 0.9659258262890683122, 1.000000000000000000, 0.9659258262890683122, 1.000000000000000000, 0.9659258262890683122, 1.000000000000000000, 0.9659258262890683122, 1.000000000000000000, 0.9659258262890683122, 1.000000000000000000, 0.9659258262890683122, 1.000000000000000000, 0.9659258262890683122, 1.000000000000000000, 0.9659258262890683122, 1.000000000000000000, 0.9659258262890683122, 1.000000000000000000, 0.9659258262890683122, 1.000000000000000000, 0.9659258262890683122, 1.000000000000000000, 0.9659258262890683122, 1.000000000000000000, 0.9659258262890683122, 1.000000000000000000, 0.9659258262890683122, 1.000000000000000000, 0.9659258262890683122, 1.000000000000000000, 0.9659258262890683122, 1.000000000000000000, 0.9659258262890683122, 1.000000000000000000, 0.9659258262890683122, 1.000000000000000000, 0.9659258262890683122, 1.000000000000000000, 0.9659258262890683122, 1.000000000000000000, 0.9659258262890683122, 1.000000000000000000, 0.9659258262890683122, 1.000000000000000000, 0.9659258262890683122, 1.000000000000000000, 0.9659258262890683122, 1.000000000000000000, 0.9659258262890683122, 1.000000000000000000, 0.9659258262890683122, 1.000000000000000000, 0.9659258262890683122, 1.000000000000000000, 0.9659258262890683122, 1.000000000000000000, 0.9659258262890683122, 1.000000000000000000, 0.9659258262890683122, 1.000000000000000000, 0.9659258262890683122, 1.000000000000000000, 0.9659258262890683122, 1.000000000000000000, 0.9659258262890683122, 1.000000000000000000, 0.9659258262890683122, 1.000000000000000000, 0.9659258262890683122, 1.000000000000000000, 0.9659258262890683122, 1.000000000000000000, 0.9659258262890683122, 1.000000000000000000, 0.9659258262890683122, 1.000000000000000000, 0.9659258262890683122, 1.000000000000000000, 0.9659258262890683122, 1.000000000000000000, 0.9659258262890683122, 1.000000000000000000, 0.9659258262890683122, 1.000000000000000000, 0.9659258262890683122, 1.000000000000000000, 0.9659258262890683122, 1.000000000000000000, 0.9659258262890683122, 1.000000000000000000, 0.9659258262890683122, 1.000000000000000000, 0.9659258262890683122, 1.000000000000000000, 0.9659258262890683122, 1.000000000000000000, 0.9659258262890683122, 1.000000000000000000, 0.9659258262890683122, 1.000000000000000000, 0.9659258262890683122, 1.000000000000000000, 0.9659258262890683122, 1.000000000000000000, 0.9659258262890683122, 1.000000000000000000, 0.9659258262890683122, 1.000000000000000000, 0.9659258262890683122, 1.000000000000000000, 0.9659258262890683122, 1.000000000000000000, 0.9659258262890683122, 1.000000000000000000, 0.9659258262890683122, 1.000000000000000000, 0.9659258262890683122, 1.000000000000000000, 0.9659258262890683122, 1.000000000000000000, 0.9659258262890683122, 1.000000000000000000, 0.9659258262890683122, 1.000000000000000000, 0.9659258262890683122, 1.000000000000000000, 0.9659258262890683122, 1.000000000000000000, 0.9659258262890683122, 1.000000000000000000, 0.9659258262890683122, 1.000000000000000000, 0.9659258262890683122, 1.000000000000000000, 0.9659258262890683122, 1.000000000000000000, 0.9659258262890683122, 1.000000000000000000, 0.9659258262890683122, 1.000000000000000000, 0.9659258262890683122, 1.000000000000000000, 0.9659258262890683122, 1.000000000000000000, 0.9659258262890683122, 1.000000000000000000, 0.9659258262890683122, 1.000000000000000000, 0.9659258262890683122, 1.000000000000000000, 0.9659258262890683122, 1.000000000000000000, 0.9659258262890683122, 1.000000000000000000, 0.9659258262890683122, 1.000000000000000000, 0.9659258262890683122, 1.000000000000000000, 0.9659258262890683122, 1.000000000000000000, 0.9659258262890683122, 1.000000000000000000, 0.9659258262890683122, 1.000000000000000000, 0.9659258262890683122, 1.000000000000000000, 0.9659258262890683122, 1.000000000000000000, 0.9659258262890683122, 1.000000000000000000, 0.9659258262890683122, 1.000000000000000000, 0.9659258262890683122, 1.000000000000000000, 0.9659258262890683122, 1.000000000000000000, 0.9659258262890683122, 1.000000000000000000, 0.9659258262890683122, 1.000000000000000000, 0.9659258262890683122, 1.000000000000000000, 0.9659258262890683122, 1.000000000000000000, 0.9659258262890683122, 1.000000000000000000, 0.9659258262890683122, 1.000000000000000000, 0.9659258262890683122, 1.000000000000000000, 0.9659258262890683122, 1.000000000000000000, 0.9659258262890683122, 1.000000000000000000, 0.9659258262890683122, 1.000000000000000000, 0.9659258262890683122, 1.000000000000000000, 0.9659258262890683122, 1.000000000000000000, 0.9659258262890683122, 1.000000000000000000, 0.9659258262890683122, 1.000000000000000000, 0.9659258262890683122, 1.000000000000000000, 0.9659258262890683122, 1.000000000000000000, 0.9659258262890683122, 1.000000000000000000, 0.9659258262890683122, 1.000000000000000000, 0.9659258262890683122, 1.000000000000000000, 0.9659258262890683122, 1.000000000000000000, 0.9659258262890683122, 1.000000000000000000, 0.9659258262890683122, 1.000000000000000000, 0.9659258262890683122, 1.000000000000000000, 0.9659258262890683122, 1.000000000000000000, 0.9659258262890683122, 1.000000000000000000, 0.9659258262890683122, 1.000000000000000000, 0.9659258262890683122, 1.000000000000000000, 0.9659258262890683122, 1.000000000000000000, 0.9659258262890683122, 1.000000000000000000, 0.9659258262890683122, 1.000000000000000000, 0.9659258262890683122, 1.000000000000000000, 0.9659258262890683122, 1.000000000000000000, 0.9659258262890683122, 1.000000000000000000, 0.9659258262890683122, 1.000000000000000000, 0.9659258262890683122, 1.000000000000000000, 0.9659258262890683122, 1.000000000000000000, 0.9659258262890683122, 1.000000000000000000, 0.9659258262890683122, 1.000000000000000000, 0.9659258262890683122, 1.000000000000000000, 0.9659258262890683122, 1.000000000000000000, 0.9659258262890683122, 1.000000000000000000, 0.9659258262890683122, 1.000000000000000000, 0.9659258262890683122, 1.000000000000000000, 0.9659258262890683122, 1.000000000000000000, 0.9659258262890683122, 1.000000000000000000, 0.9659258262890683122, 1.000000000000000000, 0.9659258262890683122, 1.000000000000000000, 0.9659258262890683122, 1.000000000000000000, 0.9659258262890683122, 1.000000000000000000, 0.9659258262890683122, 1.000000000000000000, 0.9659258262890683122, 1.000000000000000000, 0.9659258262890683122, 1.000000000000000000, 0.9659258262890683122, 1.000000000000000000, 0.9659258262890683122, 1.000000000000000000, 0.9659258262890683122, 1.000000000000000000, 0.9659258262890683122, 1.000000000000000000, 0.9659258262890683122, 1.000000000000000000, 0.9659258262890683122, 1.000000000000000000, 0.9659258262890683122, 1.000000000000000000, 0.9659258262890683122, 1.000000000000000000, 0.9659258262890683122, 1.000000000000000000, 0.9659258262890683122, 1.000000000000000000, 0.9659258262890683122, 1.000000000000000000, 0.9659258262890683122, 1.000000000000000000, 0.9659258262890683122, 1.000000000000000000, 0.9659258262890683122, 1.000000000000000000, 0.9659258262890683122, 1.000000000000000000, 0.9659258262890683122, 1.000000000000000000, 0.9659258262890683122, 1.000000000000000000, 0.9659258262890683122, 1.000000000000000000, 0.9659258262890683122, 1.000000000000000000, 0.9659258262890683122, 1.000000000000000000, 0.9659258262890683122, 1.000000000000000000, 0.9659258262890683122, 1.000000000000000000, 0.9659258262890683122, 1.000000000000000000, 0.9659258262890683122, 1.000000000000000000, 0.9659258262890683122, 1.000000000000000000, 0.9659258262890683122, 1.000000000000000000, 0.9659258262890683122, 1.000000000000000000, 0.9659258262890683122, 1.000000000000000000, 0.9659258262890683122, 1.000000000000000000),
 ( 1.000000000000000000, 0.9659258262890683122, 1.000000000000000000, 0.9659258262890683122, 1.000000000000000000, 0.9659258262890683122, 1.000000000000000000, 0.9659258262890683122, 1.000000000000000000, 0.9659258262890683122, 1.000000000000000000, 0.9659258262890683122, 1.000000000000000000, 0.9659258262890683122, 1.000000000000000000, 0.9659258262890683122, 1.000000000000000000, 0.9659258262890683122, 1.000000000000000000, 0.9659258262890683122, 1.000000000000000000, 0.9659258262890683122, 1.000000000000000000, 0.9659258262890683122, 1.000000000000000000, 0.9659258262890683122, 1.000000000000000000, 0.9659258262890683122, 1.000000000000000000, 0.9659258262890683122, 1.000000000000000000, 0.9659258262890683122, 1.000000000000000000, 0.9659258262890683122, 1.000000000000000000, 0.9659258262890683122, 1.000000000000000000, 0.9659258262890683122, 1.000000000000000000, 0.9659258262890683122, 1.000000000000000000, 0.9659258262890683122, 1.000000000000000000, 0.9659258262890683122, 1.000000000000000000, 0.9659258262890683122, 1.000000000000000000, 0.9659258262890683122, 1.000000000000000000, 0.9659258262890683122, 1.000000000000000000, 0.9659258262890683122, 1.000000000000000000, 0.9659258262890683122, 1.000000000000000000, 0.9659258262890683122, 1.000000000000000000, 0.9659258262890683122, 1.000000000000000000, 0.9659258262890683122, 1.000000000000000000, 0.9659258262890683122, 1.000000000000000000, 0.9659258262890683122, 1.000000000000000000, 0.9659258262890683122, 1.000000000000000000, 0.9659258262890683122, 1.000000000000000000, 0.9659258262890683122, 1.000000000000000000, 0.9659258262890683122, 1.000000000000000000, 0.9659258262890683122, 1.000000000000000000, 0.9659258262890683122, 1.000000000000000000, 0.9659258262890683122, 1.000000000000000000, 0.9659258262890683122, 1.000000000000000000, 0.9659258262890683122, 1.000000000000000000, 0.9659258262890683122, 1.000000000000000000, 0.9659258262890683122, 1.000000000000000000, 0.9659258262890683122, 1.000000000000000000, 0.9659258262890683122, 1.000000000000000000, 0.9659258262890683122, 1.000000000000000000, 0.9659258262890683122, 1.000000000000000000, 0.9659258262890683122, 1.000000000000000000, 0.9659258262890683122, 1.000000000000000000, 0.9659258262890683122, 1.000000000000000000, 0.9659258262890683122, 1.000000000000000000, 0.9659258262890683122, 1.000000000000000000, 0.9659258262890683122, 1.000000000000000000, 0.9659258262890683122, 1.000000000000000000, 0.9659258262890683122, 1.000000000000000000, 0.9659258262890683122, 1.000000000000000000, 0.9659258262890683122, 1.000000000000000000, 0.9659258262890683122, 1.000000000000000000, 0.9659258262890683122, 1.000000000000000000, 0.9659258262890683122, 1.000000000000000000, 0.9659258262890683122, 1.000000000000000000, 0.9659258262890683122, 1.000000000000000000, 0.9659258262890683122, 1.000000000000000000, 0.9659258262890683122, 1.000000000000000000, 0.9659258262890683122, 1.000000000000000000, 0.9659258262890683122, 1.000000000000000000, 0.9659258262890683122, 1.000000000000000000, 0.9659258262890683122, 1.000000000000000000, 0.9659258262890683122, 1.000000000000000000, 0.9659258262890683122, 1.000000000000000000, 0.9659258262890683122, 1.000000000000000000, 0.9659258262890683122, 1.000000000000000000, 0.9659258262890683122, 1.000000000000000000, 0.9659258262890683122, 1.000000000000000000, 0.9659258262890683122, 1.000000000000000000, 0.9659258262890683122, 1.000000000000000000, 0.9659258262890683122, 1.000000000000000000, 0.9659258262890683122, 1.000000000000000000, 0.9659258262890683122, 1.000000000000000000, 0.9659258262890683122, 1.000000000000000000, 0.9659258262890683122, 1.000000000000000000, 0.9659258262890683122, 1.000000000000000000, 0.9659258262890683122, 1.000000000000000000, 0.9659258262890683122, 1.000000000000000000, 0.9659258262890683122, 1.000000000000000000, 0.9659258262890683122, 1.000000000000000000, 0.9659258262890683122, 1.000000000000000000, 0.9659258262890683122, 1.000000000000000000, 0.9659258262890683122, 1.000000000000000000, 0.9659258262890683122, 1.000000000000000000, 0.9659258262890683122, 1.000000000000000000, 0.9659258262890683122, 1.000000000000000000, 0.9659258262890683122, 1.000000000000000000, 0.9659258262890683122, 1.000000000000000000, 0.9659258262890683122, 1.000000000000000000, 0.9659258262890683122, 1.000000000000000000, 0.9659258262890683122, 1.000000000000000000, 0.9659258262890683122, 1.000000000000000000, 0.9659258262890683122, 1.000000000000000000, 0.9659258262890683122, 1.000000000000000000, 0.9659258262890683122, 1.000000000000000000, 0.9659258262890683122, 1.000000000000000000, 0.9659258262890683122, 1.000000000000000000, 0.9659258262890683122, 1.000000000000000000, 0.9659258262890683122, 1.000000000000000000, 0.9659258262890683122, 1.000000000000000000, 0.9659258262890683122, 1.000000000000000000, 0.9659258262890683122, 1.000000000000000000, 0.9659258262890683122, 1.000000000000000000, 0.9659258262890683122, 1.000000000000000000, 0.9659258262890683122, 1.000000000000000000, 0.9659258262890683122, 1.000000000000000000, 0.9659258262890683122, 1.000000000000000000, 0.9659258262890683122, 1.000000000000000000, 0.9659258262890683122, 1.000000000000000000, 0.9659258262890683122, 1.000000000000000000, 0.9659258262890683122, 1.000000000000000000, 0.9659258262890683122, 1.000000000000000000, 0.9659258262890683122, 1.000000000000000000, 0.9659258262890683122, 1.000000000000000000, 0.9659258262890683122, 1.000000000000000000, 0.9659258262890683122, 1.000000000000000000, 0.9659258262890683122, 1.000000000000000000, 0.9659258262890683122, 1.000000000000000000, 0.9659258262890683122, 1.000000000000000000, 0.9659258262890683122, 1.000000000000000000, 0.9659258262890683122, 1.000000000000000000, 0.9659258262890683122, 1.000000000000000000, 0.9659258262890683122, 1.000000000000000000, 0.9659258262890683122, 1.000000000000000000, 0.9659258262890683122, 1.000000000000000000, 0.9659258262890683122, 1.000000000000000000, 0.9659258262890683122, 1.000000000000000000, 0.9659258262890683122, 1.000000000000000000, 0.9659258262890683122, 1.000000000000000000, 0.9659258262890683122, 1.000000000000000000, 0.9659258262890683122, 1.000000000000000000, 0.9659258262890683122, 1.000000000000000000, 0.9659258262890683122, 1.000000000000000000, 0.9659258262890683122, 1.000000000000000000, 0.9659258262890683122, 1.000000000000000000, 0.9659258262890683122, 1.000000000000000000, 0.9659258262890683122, 1.000000000000000000, 0.9659258262890683122, 1.000000000000000000, 0.9659258262890683122, 1.000000000000000000, 0.9659258262890683122, 1.000000000000000000, 0.9659258262890683122, 1.000000000000000000, 0.9659258262890683122, 1.000000000000000000, 0.9659258262890683122, 1.000000000000000000, 0.9659258262890683122, 1.000000000000000000, 0.9659258262890683122, 1.000000000000000000, 0.9659258262890683122, 1.000000000000000000, 0.9659258262890683122, 1.000000000000000000, 0.9659258262890683122, 1.000000000000000000, 0.9659258262890683122, 1.000000000000000000, 0.9659258262890683122, 1.000000000000000000, 0.9659258262890683122, 1.000000000000000000, 0.9659258262890683122, 1.000000000000000000, 0.9659258262890683122, 1.000000000000000000, 0.9659258262890683122, 1.000000000000000000, 0.9659258262890683122, 1.000000000000000000, 0.9659258262890683122, 1.000000000000000000, 0.9659258262890683122, 1.000000000000000000, 0.9659258262890683122, 1.000000000000000000, 0.9659258262890683122, 1.000000000000000000, 0.9659258262890683122, 1.000000000000000000, 0.9659258262890683122, 1.000000000000000000, 0.9659258262890683122, 1.000000000000000000, 0.9659258262890683122, 1.000000000000000000, 0.9659258262890683122, 1.000000000000000000, 0.9659258262890683122, 1.000000000000000000, 0.9659258262890683122, 1.000000000000000000, 0.9659258262890683122, 1.000000000000000000, 0.9659258262890683122, 1.000000000000000000, 0.9659258262890683122, 1.000000000000000000, 0.9659258262890683122, 1.000000000000000000, 0.9659258262890683122, 1.000000000000000000, 0.9659258262890683122, 1.000000000000000000, 0.9659258262890683122, 1.000000000000000000, 0.9659258262890683122, 1.000000000000000000, 0.9659258262890683122, 1.000000000000000000, 0.9659258262890683122, 1.000000000000000000, 0.9659258262890683122, 1.000000000000000000, 0.9659258262890683122, 1.000000000000000000, 0.9659258262890683122, 1.000000000000000000, 0.9659258262890683122, 1.000000000000000000, 0.9659258262890683122, 1.000000000000000000, 0.9659258262890683122, 1.000000000000000000, 0.9659258262890683122, 1.000000000000000000, 0.9659258262890683122, 1.000000000000000000, 0.9659258262890683122, 1.000000000000000000, 0.9659258262890683122, 1.000000000000000000, 0.9659258262890683122, 1.000000000000000000, 0.9659258262890683122, 1.000000000000000000, 0.9659258262890683122, 1.000000000000000000, 0.9659258262890683122, 1.000000000000000000, 0.9659258262890683122, 1.000000000000000000, 0.9659258262890683122, 1.000000000000000000, 0.9659258262890683122, 1.000000000000000000, 0.9659258262890683122, 1.000000000000000000, 0.9659258262890683122, 1.000000000000000000, 0.9659258262890683122, 1.000000000000000000, 0.9659258262890683122, 1.000000000000000000, 0.9659258262890683122, 1.000000000000000000, 0.9659258262890683122, 1.000000000000000000, 0.9659258262890683122, 1.000000000000000000, 0.9659258262890683122, 1.000000000000000000, 0.9659258262890683122, 1.000000000000000000, 0.9659258262890683122, 1.000000000000000000, 0.9659258262890683122, 1.000000000000000000, 0.9659258262890683122, 1.000000000000000000, 0.9659258262890683122, 1.000000000000000000, 0.9659258262890683122, 1.000000000000000000, 0.9659258262890683122, 1.000000000000000000, 0.9659258262890683122, 1.000000000000000000, 0.9659258262890683122, 1.000000000000000000, 0.9659258262890683122, 1.000000000000000000, 0.9659258262890683122, 1.000000000000000000, 0.9659258262890683122, 1.000000000000000000, 0.9659258262890683122, 1.000000000000000000, 0.9659258262890683122, 1.000000000000000000, 0.9659258262890683122, 1.000000000000000000, 0.9659258262890683122, 1.000000000000000000, 0.9659258262890683122, 1.000000000000000000, 0.9659258262890683122, 1.000000000000000000, 0.9659258262890683122, 1.000000000000000000, 0.9659258262890683122, 1.000000000000000000, 0.9659258262890683122, 1.000000000000000000, 0.9659258262890683122, 1.000000000000000000, 0.9659258262890683122, 1.000000000000000000, 0.9659258262890683122, 1.000000000000000000, 0.9659258262890683122, 1.000000000000000000, 0.9659258262890683122, 1.000000000000000000, 0.9659258262890683122, 1.000000000000000000, 0.9659258262890683122, 1.000000000000000000, 0.9659258262890683122, 1.000000000000000000, 0.9659258262890683122, 1.000000000000000000, 0.9659258262890683122, 1.000000000000000000, 0.9659258262890683122, 1.000000000000000000, 0.9659258262890683122, 1.000000000000000000, 0.9659258262890683122, 1.000000000000000000, 0.9659258262890683122, 1.000000000000000000, 0.9659258262890683122, 1.000000000000000000, 0.9659258262890683122, 1.000000000000000000, 0.9659258262890683122, 1.000000000000000000, 0.9659258262890683122, 1.000000000000000000, 0.9659258262890683122, 1.000000000000000000, 0.9659258262890683122, 1.000000000000000000, 0.9659258262890683122, 1.000000000000000000, 0.9659258262890683122, 1.000000000000000000, 0.9659258262890683122, 1.000000000000000000, 0.9659258262890683122, 1.000000000000000000, 0.9659258262890683122, 1.000000000000000000, 0.9659258262890683122, 1.000000000000000000, 0.9659258262890683122, 1.000000000000000000) ) ) 
 REPRESENTATION_ITEM ( '' )  SURFACE ( )  );
#11321 = CARTESIAN_POINT ( 'NONE',  ( -2.113943251734124118, 1.379671404989104122, 0.4476723508032736110 ) ) ;
#11322 = CARTESIAN_POINT ( 'NONE',  ( -0.2821522309711278487, -0.5511811023622048555, -0.09757992244046775898 ) ) ;
#11323 = CARTESIAN_POINT ( 'NONE',  ( 0.2362204724409449064, 0.4091458600556404646, -1.008530183727034180 ) ) ;
#11324 = CARTESIAN_POINT ( 'NONE',  ( 0.7414698162729663755, 0.2952755905511811885, 0.1292274648535926551 ) ) ;
#11325 = CARTESIAN_POINT ( 'NONE',  ( -0.1133856558944468518, -0.2726377952755905665, 0.1574803149606299191 ) ) ;
#11326 = CARTESIAN_POINT ( 'NONE',  ( 1.213910761154856299, -0.5511811023622048555, -0.09757992244046775898 ) ) ;
#11327 = CARTESIAN_POINT ( 'NONE',  ( -1.069553805774277722, 0.2952755905511811885, 0.1292274648535926551 ) ) ;
#11328 = CARTESIAN_POINT ( 'NONE',  ( -0.3543307086614165824, 0.1771653543307087630, 0.000000000000000000 ) ) ;
#11329 = DIRECTION ( 'NONE',  ( 0.000000000000000000, -1.000000000000000000, 1.734723475976806108E-16 ) ) ;
#11330 = CARTESIAN_POINT ( 'NONE',  ( 0.03280839895013198948, 0.1771653543307087630, 0.09757992244046791164 ) ) ;
#11331 = CARTESIAN_POINT ( 'NONE',  ( -0.4265091863517051496, -0.6692913385826771977, 0.1292274648535927661 ) ) ;
#11332 = CARTESIAN_POINT ( 'NONE',  ( -0.2925321140481930149, -0.2925321140481933480, -0.7657480314960628531 ) ) ;
#11333 = EDGE_CURVE ( 'NONE', #66374, #21108, #81518, .T. ) ;
#11334 = CARTESIAN_POINT ( 'NONE',  ( 0.1049643490035304938, -0.3917322834645669549, -2.374671916010498762 ) ) ;
#11335 = CARTESIAN_POINT ( 'NONE',  ( 0.8005249343832027131, -0.004921259842519576551, 0.3153832671262227771 ) ) ;
#11336 = CARTESIAN_POINT ( 'NONE',  ( -0.3871391076115476282, -0.05778040916215522460, 0.4822834645669289988 ) ) ;
#11337 = CARTESIAN_POINT ( 'NONE',  ( -0.6299212598425188991, -0.1870078740157480879, -0.4822834645669291653 ) ) ;
#11338 = CARTESIAN_POINT ( 'NONE',  ( -0.6233595800524928121, -0.2845877964562161244, -0.3641732283464567121 ) ) ;
#11339 = CARTESIAN_POINT ( 'NONE',  ( -3.934129746973768160, 1.087346627047580006, 0.1532148504152880952 ) ) ;
#11340 = CARTESIAN_POINT ( 'NONE',  ( 0.06561679790026316017, -0.4281496062992124485, 0.4176697321401328655 ) ) ;
#11341 = B_SPLINE_CURVE_WITH_KNOTS ( 'NONE', 3,
 ( #11057, #6385, #5968, #69541 ),
 .UNSPECIFIED., .F., .F.,
 ( 4, 4 ),
 ( 1.009076915740197753E-06, 0.001443158937089476486 ),
 .UNSPECIFIED. ) ;
#11342 = CARTESIAN_POINT ( 'NONE',  ( -1.161417322834644716, -0.4536011799217368745, -0.2665933059059886201 ) ) ;
#11343 = CARTESIAN_POINT ( 'NONE',  ( -1.469816272965878357, 0.2306618581243848609, 0.2411417322834645549 ) ) ;
#11344 = CARTESIAN_POINT ( 'NONE',  ( 2.795275590551181466, 1.968503937007874960, 0.000000000000000000 ) ) ;
#11345 = ADVANCED_FACE ( 'NONE', ( #13275 ), #38927, .F. ) ;
#11346 = VERTEX_POINT ( 'NONE', #64607 ) ;
#11347 = AXIS2_PLACEMENT_3D ( 'NONE', #35222, #48664, #66385 ) ;
#11348 = CARTESIAN_POINT ( 'NONE',  ( -1.397637795275589623, 0.07958543189024085140, 0.2665933059059887866 ) ) ;
#11349 = CARTESIAN_POINT ( 'NONE',  ( -1.561679790026246017, 0.05413385826771666132, 0.4176697321401328100 ) ) ;
#11350 = CARTESIAN_POINT ( 'NONE',  ( -0.9448818897637790704, -0.1870078740157479769, 0.4822834645669291653 ) ) ;
#11351 = CARTESIAN_POINT ( 'NONE',  ( -1.627296587926508442, 0.2306618581243848609, 0.2411417322834645549 ) ) ;
#11352 = CARTESIAN_POINT ( 'NONE',  ( -9.594673741351313045E-17, 0.3917322834645670104, -1.501968503937008093 ) ) ;
#11353 = CARTESIAN_POINT ( 'NONE',  ( -0.1188761721681626526, 0.3738583250858228402, -1.220472440944881942 ) ) ;
#11354 = CARTESIAN_POINT ( 'NONE',  ( 0.9973753280839902091, -0.6046776061558807314, 0.2411417322834647770 ) ) ;
#11355 = CARTESIAN_POINT ( 'NONE',  ( 0.3477690288713918276, -0.6692913385826773087, -0.1292274648535924053 ) ) ;
#11356 = DIRECTION ( 'NONE',  ( -3.491481338843132961E-15, -0.000000000000000000, 1.000000000000000000 ) ) ;
#11357 = CARTESIAN_POINT ( 'NONE',  ( 0.3996062992125985480, -0.1070741851644052972, -2.393044619422572072 ) ) ;
#11358 = CARTESIAN_POINT ( 'NONE',  ( 1.338582677165355062, -0.1870078740157480601, -0.3641732283464567677 ) ) ;
#11359 = CARTESIAN_POINT ( 'NONE',  ( -0.3996062992125986035, -7.340648628747425578E-17, -0.8267716535433070613 ) ) ;
#11360 = ORIENTED_EDGE ( 'NONE', *, *, #34082, .T. ) ;
#11361 = CARTESIAN_POINT ( 'NONE',  ( -1.043307086614172041, -0.4536011799217367080, 0.2665933059059888421 ) ) ;
#11363 = CARTESIAN_POINT ( 'NONE',  ( -0.2867679344610364334, -0.2867679344610367109, -2.728346456692912536 ) ) ;
#11362 = VECTOR ( 'NONE', #75456, 39.37007874015748143 ) ;
#11364 = ORIENTED_EDGE ( 'NONE', *, *, #22547, .F. ) ;
#11365 = CARTESIAN_POINT ( 'NONE',  ( 0.2690288713910767848, -0.6692913385826773087, -0.1292274648535924053 ) ) ;
#11366 = CARTESIAN_POINT ( 'NONE',  ( -0.4199475065616791736, 0.2306618581243847221, -0.2411417322834647770 ) ) ;
#11367 = CARTESIAN_POINT ( 'NONE',  ( -1.272965879265091305, 0.05413385826771626580, -0.4176697321401330321 ) ) ;
#11368 = CARTESIAN_POINT ( 'NONE',  ( 0.9186351706036752773, 0.2306618581243847221, -0.2411417322834647770 ) ) ;
#11369 = CARTESIAN_POINT ( 'NONE',  ( 1.640419947506562393, -0.4281496062992124485, 0.4176697321401328655 ) ) ;
#11370 = DIRECTION ( 'NONE',  ( -1.000000000000000000, 0.000000000000000000, 0.000000000000000000 ) ) ;
#11371 = CARTESIAN_POINT ( 'NONE',  ( 0.02624671916010564918, -0.6046776061558809534, -0.2411417322834644161 ) ) ;
#11372 = CARTESIAN_POINT ( 'NONE',  ( -1.141732283464566011, 0.2952755905511811885, 0.000000000000000000 ) ) ;
#11373 = CARTESIAN_POINT ( 'NONE',  ( -1.614173228346455824, 0.2952755905511811885, 0.000000000000000000 ) ) ;
#11374 = CARTESIAN_POINT ( 'NONE',  ( 0.4426658557721722120, 1.366171107244630534, -2.619331181873139069 ) ) ;
#11375 = CARTESIAN_POINT ( 'NONE',  ( 4.797336870675656522E-17, -0.3917322834645670104, -2.840551181102362044 ) ) ;
#11376 = CARTESIAN_POINT ( 'NONE',  ( 0.6758530183727039509, -0.5511811023622046335, 0.09757992244046803654 ) ) ;
#11377 = VERTEX_POINT ( 'NONE', #56624 ) ;
#11378 = CARTESIAN_POINT ( 'NONE',  ( 0.3420746716998659953, 0.1974969037888705536, -0.1312335958005249881 ) ) ;
#11379 = CARTESIAN_POINT ( 'NONE',  ( -0.7939632545931750718, -0.05778040916215560624, -0.4822834645669293319 ) ) ;
#11380 = VERTEX_POINT ( 'NONE', #18350 ) ;
#11381 = CARTESIAN_POINT ( 'NONE',  ( -0.03937007874015669567, -0.5511811023622047445, 6.969142054262312111E-17 ) ) ;
#11382 = CARTESIAN_POINT ( 'NONE',  ( 0.4091458600556403535, 0.2362204724409449896, -0.1312335958005249326 ) ) ;
#11383 = CARTESIAN_POINT ( 'NONE',  ( 0.6430446194225728496, 0.05413385826771666132, 0.4176697321401328100 ) ) ;
#11384 = CARTESIAN_POINT ( 'NONE',  ( 0.3937007874015754361, -0.1870078740157480879, -0.4822834645669291653 ) ) ;
#11385 = CARTESIAN_POINT ( 'NONE',  ( -0.4199475065616791736, 0.2306618581243847221, -0.2411417322834647770 ) ) ;
#11386 = CARTESIAN_POINT ( 'NONE',  ( 0.3917322834645670659, -0.1049643490035303273, -1.210649237041681703 ) ) ;
#11387 = CARTESIAN_POINT ( 'NONE',  ( -1.371391076115484609, -0.6692913385826771977, 0.1292274648535927661 ) ) ;
#11388 = CARTESIAN_POINT ( 'NONE',  ( -0.1958661417322836718, 0.3392501089628017219, -2.459973753280839670 ) ) ;
#11389 = CARTESIAN_POINT ( 'NONE',  ( 1.489501312335958172, -0.08942795157528024563, -0.3641732283464568787 ) ) ;
#11390 = CARTESIAN_POINT ( 'NONE',  ( -1.213910761154854745, -0.6692913385826771977, 0.1292274648535927661 ) ) ;
#11391 = CARTESIAN_POINT ( 'NONE',  ( 0.7020997375328090762, -0.3162353388693405765, 0.4822834645669290543 ) ) ;
#11392 = CARTESIAN_POINT ( 'NONE',  ( 1.102362204724410155, -0.1870078740157480879, -0.4822834645669291653 ) ) ;
#11393 = CARTESIAN_POINT ( 'NONE',  ( -0.1070741851644056997, 0.3996062992125986035, -0.7939632545931758489 ) ) ;
#11394 = CARTESIAN_POINT ( 'NONE',  ( -1.351706036745406347, 0.05413385826771626580, -0.4176697321401330321 ) ) ;
#11395 = CARTESIAN_POINT ( 'NONE',  ( -0.2925321140481932369, 0.2925321140481931259, -0.4114173228346455491 ) ) ;
#11396 = CARTESIAN_POINT ( 'NONE',  ( 0.1377952755905518800, -0.5400638737290844871, 0.3530559997133364547 ) ) ;
#11397 = CARTESIAN_POINT ( 'NONE',  ( 0.1070741851644054915, -0.3996062992125986035, -2.447506561679789527 ) ) ;
#11398 = CARTESIAN_POINT ( 'NONE',  ( -0.1049643490035302024, -0.3917322834645671215, -1.574146981627296604 ) ) ;
#11399 = CARTESIAN_POINT ( 'NONE',  ( -1.469816272965878357, 0.1283753931104748280, 0.1820866141732283561 ) ) ;
#11400 = CARTESIAN_POINT ( 'NONE',  ( 0.6102362204724416372, 0.07958543189024071263, -0.2665933059059888421 ) ) ;
#11401 = CARTESIAN_POINT ( 'NONE',  ( 1.069553805774278610, -0.6692913385826771977, 0.1292274648535927661 ) ) ;
#11402 = CARTESIAN_POINT ( 'NONE',  ( 5.785732909357575061E-17, -0.4724409448818898682, -1.257874015748031260 ) ) ;
#11403 = CARTESIAN_POINT ( 'NONE',  ( 0.7611548556430454138, 0.1283753931104746893, -0.1820866141732285504 ) ) ;
#11404 = CARTESIAN_POINT ( 'NONE',  ( 0.2887139107611556010, -0.6046776061558807314, 0.2411417322834647770 ) ) ;
#11405 = CARTESIAN_POINT ( 'NONE',  ( -0.3420746716998660508, -0.1974969037888706924, -0.9166666666666668517 ) ) ;
#11406 = ADVANCED_FACE ( 'NONE', ( #57032 ), #82727, .F. ) ;
#11407 = CARTESIAN_POINT ( 'NONE',  ( -0.7808398950131225646, -0.05778040916215522460, 0.4822834645669289988 ) ) ;
#11408 = CARTESIAN_POINT ( 'NONE',  ( -0.2034120734908128059, 0.2952755905511811885, 0.1292274648535926551 ) ) ;
#11409 = AXIS2_PLACEMENT_3D ( 'NONE', #31358, #5288, #70920 ) ;
#11410 = CARTESIAN_POINT ( 'NONE',  ( 1.062992125984252745, -0.5511811023622047445, 6.969142054262312111E-17 ) ) ;
#11411 = CARTESIAN_POINT ( 'NONE',  ( -0.1246719160104980823, 0.2952755905511811885, 0.1292274648535926551 ) ) ;
#11412 = DIRECTION ( 'NONE',  ( 1.000000000000000000, 0.000000000000000000, -0.000000000000000000 ) ) ;
#11413 = CARTESIAN_POINT ( 'NONE',  ( -0.3018372703412066094, 0.05413385826771666132, 0.4176697321401328100 ) ) ;
#11414 = CARTESIAN_POINT ( 'NONE',  ( -0.07217847769028787330, -0.08942795157527998196, 0.3641732283464567121 ) ) ;
#11415 = CARTESIAN_POINT ( 'NONE',  ( -2.593354744918267230, 1.408268389154264222, -0.4567427728026662304 ) ) ;
#11416 = CARTESIAN_POINT ( 'NONE',  ( -0.3740157480314953431, -0.5400638737290845981, -0.3530559997133363437 ) ) ;
#11417 = CARTESIAN_POINT ( 'NONE',  ( 0.8858267716535438430, -0.4536011799217368745, -0.2665933059059886201 ) ) ;
#11418 = CARTESIAN_POINT ( 'NONE',  ( -0.05603898182074958101, 1.066283915671629945, -1.446447749318907183 ) ) ;
#11419 = CARTESIAN_POINT ( 'NONE',  ( 0.1998031496062992463, 0.3460692066303959202, -1.638451443569554078 ) ) ;
#11420 = CARTESIAN_POINT ( 'NONE',  ( 0.4790026246719168435, -0.3162353388693409650, -0.4822834645669289433 ) ) ;
#11421 = CARTESIAN_POINT ( 'NONE',  ( 0.1958661417322836440, -0.3392501089628017219, -1.501312335958005173 ) ) ;
#11422 = CARTESIAN_POINT ( 'NONE',  ( 1.299212598425197429, -0.5511811023622047445, 6.969142054262312111E-17 ) ) ;
#11423 = CARTESIAN_POINT ( 'NONE',  ( 0.3826031302655975019, 1.809133623825372073E-16, -0.3954985857520062487 ) ) ;
#11424 = CARTESIAN_POINT ( 'NONE',  ( -0.4330708661417315697, 0.1771653543307087630, 0.000000000000000000 ) ) ;
#11425 = CIRCLE ( 'NONE', #20850, 3.937007874015748143 ) ;
#11426 = CARTESIAN_POINT ( 'NONE',  ( -0.9186351706036736120, 0.1283753931104748280, 0.1820866141732283561 ) ) ;
#11427 = CARTESIAN_POINT ( 'NONE',  ( -0.2165354330708654795, 0.1660481256975885056, 0.3530559997133364547 ) ) ;
#11428 = CARTESIAN_POINT ( 'NONE',  ( 0.5183727034120741983, 0.2952755905511810774, -0.1292274648535930714 ) ) ;
#11429 = CARTESIAN_POINT ( 'NONE',  ( 1.010498687664042716, -0.3690944881889763329, 0.3153832671262228327 ) ) ;
#11430 = CARTESIAN_POINT ( 'NONE',  ( 0.3760314581298215830, 1.247744516244858604, -1.057212048078999933 ) ) ;
#11431 = CARTESIAN_POINT ( 'NONE',  ( -1.719160104986876103, 0.05413385826771666132, 0.4176697321401328100 ) ) ;
#11432 = CARTESIAN_POINT ( 'NONE',  ( 0.8923884514435703741, 0.2306618581243848609, 0.2411417322834645549 ) ) ;
#11433 = FACE_OUTER_BOUND ( 'NONE', #60132, .T. ) ;
#11434 = CARTESIAN_POINT ( 'NONE',  ( 0.2362204724409456558, -0.1870078740157480879, -0.4822834645669291653 ) ) ;
#11435 = CARTESIAN_POINT ( 'NONE',  ( 0.3392501089628018884, -0.1958661417322834220, -0.8195538057742782767 ) ) ;
#11436 = CARTESIAN_POINT ( 'NONE',  ( 0.8070866141732289112, -0.5400638737290845981, -0.3530559997133363437 ) ) ;
#11437 = CARTESIAN_POINT ( 'NONE',  ( 0.6955380577427828781, -0.4281496062992124485, 0.4176697321401328655 ) ) ;
#11438 = CARTESIAN_POINT ( 'NONE',  ( -0.4682706818399092197, 1.459764456743772199, -3.909061641404189658 ) ) ;
#11439 = CARTESIAN_POINT ( 'NONE',  ( 0.5380577427821529035, -0.3690944881889763329, 0.3153832671262228327 ) ) ;
#11440 = CARTESIAN_POINT ( 'NONE',  ( 1.299212598425197429, -0.6692913385826771977, 8.415575281601705876E-17 ) ) ;
#11441 = CARTESIAN_POINT ( 'NONE',  ( -0.07874015748031421014, -0.1870078740157480601, -0.3641732283464567677 ) ) ;
#11442 = CARTESIAN_POINT ( 'NONE',  ( -0.1706036745406816491, 0.05413385826771626580, -0.4176697321401330321 ) ) ;
#11443 = CARTESIAN_POINT ( 'NONE',  ( 0.2887139107611556010, -0.6046776061558807314, 0.2411417322834647770 ) ) ;
#11444 = CARTESIAN_POINT ( 'NONE',  ( -0.7874015748031489847, -0.1870078740157480879, -0.4822834645669291653 ) ) ;
#11445 = CARTESIAN_POINT ( 'NONE',  ( -0.4724409448818890911, -0.1870078740157479769, 0.3641732283464567677 ) ) ;
#11446 = CARTESIAN_POINT ( 'NONE',  ( 0.3215223097112867578, -0.05778040916215522460, 0.4822834645669289988 ) ) ;
#11447 = CARTESIAN_POINT ( 'NONE',  ( 0.9842519685039378130, -0.5511811023622047445, 6.969142054262312111E-17 ) ) ;
#11448 = CARTESIAN_POINT ( 'NONE',  ( 0.08530183727034192087, -0.05778040916215522460, 0.4822834645669289988 ) ) ;
#11449 = CARTESIAN_POINT ( 'NONE',  ( 1.122047244094488860, 0.1012011053420777407, 0.2882089793578257453 ) ) ;
#11451 = CARTESIAN_POINT ( 'NONE',  ( -0.1070741851644051862, -0.3996062992125986590, -1.017060367454068137 ) ) ;
#11450 = CARTESIAN_POINT ( 'NONE',  ( -0.6155095129759579065, 1.955395699586848224, 0.5046436704918912941 ) ) ;
#11452 = CARTESIAN_POINT ( 'NONE',  ( 1.555118110236221041, 0.1660481256975883668, -0.3530559997133364547 ) ) ;
#11453 = PLANE ( 'NONE',  #67790 ) ;
#11454 = CARTESIAN_POINT ( 'NONE',  ( -1.181102362204723644, -0.1870078740157479769, 0.4822834645669291653 ) ) ;
#11455 = CARTESIAN_POINT ( 'NONE',  ( -0.8661417322834640276, -0.1870078740157480879, -0.4822834645669291653 ) ) ;
#11456 = CARTESIAN_POINT ( 'NONE',  ( 0.1265901696524990294, -0.4724409448818896462, -0.2427821522309711322 ) ) ;
#11457 = CARTESIAN_POINT ( 'NONE',  ( 0.3949938075777409963, 2.418639510665530435E-17, -2.952755905511811108 ) ) ;
#11458 = ORIENTED_EDGE ( 'NONE', *, *, #35860, .F. ) ;
#11459 = CARTESIAN_POINT ( 'NONE',  ( 0.4527559055118117182, 0.07958543189024071263, -0.2665933059059888421 ) ) ;
#11460 = CARTESIAN_POINT ( 'NONE',  ( 0.1049643490035304938, -0.3917322834645669549, -1.337270341207349000 ) ) ;
#11461 = CARTESIAN_POINT ( 'NONE',  ( 0.4790026246719167324, -0.05778040916215522460, 0.4822834645669289988 ) ) ;
#11462 = CARTESIAN_POINT ( 'NONE',  ( -0.4724409448818895907, -0.1265901696524993070, -2.408136482939632561 ) ) ;
#11463 = LINE ( 'NONE', #18192, #9050 ) ;
#11464 = CARTESIAN_POINT ( 'NONE',  ( -0.3033747635708576307, 0.02791078216816064370, 0.4328096321851915285 ) ) ;
#11465 = CARTESIAN_POINT ( 'NONE',  ( 1.246719160104987623, 0.05413385826771626580, -0.4176697321401330321 ) ) ;
#11466 = EDGE_CURVE ( 'NONE', #54098, #80968, #19914, .T. ) ;
#11467 = CARTESIAN_POINT ( 'NONE',  ( 1.148293963254593653, 0.1771653543307087075, -0.09757992244046823083 ) ) ;
#11468 = CARTESIAN_POINT ( 'NONE',  ( 0.2099737532808405305, -0.6046776061558807314, 0.2411417322834647770 ) ) ;
#11469 = CARTESIAN_POINT ( 'NONE',  ( 0.2867679344610365999, -0.2867679344610365999, -0.6508993193887645523 ) ) ;
#11470 = CARTESIAN_POINT ( 'NONE',  ( -0.4199475065616791736, -0.6046776061558807314, 0.2411417322834647770 ) ) ;
#11471 = CARTESIAN_POINT ( 'NONE',  ( -1.489501312335957062, -0.2845877964562161244, -0.3641732283464567121 ) ) ;
#11472 = CARTESIAN_POINT ( 'NONE',  ( 0.2362204724409456558, -0.1870078740157480879, -0.4822834645669291653 ) ) ;
#11474 = EDGE_CURVE ( 'NONE', #16433, #18816, #43794, .T. ) ;
#11473 = CARTESIAN_POINT ( 'NONE',  ( -0.4921259842519677963, -0.5400638737290844871, 0.3530559997133364547 ) ) ;
#11475 = CARTESIAN_POINT ( 'NONE',  ( 1.627296587926509996, -0.6046776061558807314, 0.2411417322834647770 ) ) ;
#11476 = CARTESIAN_POINT ( 'NONE',  ( -0.08519462842575996342, 1.070400731138068995, -1.857255144359619470 ) ) ;
#11477 = VERTEX_POINT ( 'NONE', #65460 ) ;
#11478 = CARTESIAN_POINT ( 'NONE',  ( -0.3917322834645671770, 0.1049643490035302024, -1.919310654364516200 ) ) ;
#11479 = CARTESIAN_POINT ( 'NONE',  ( 0.2427821522309719648, -0.05778040916215522460, 0.4822834645669289988 ) ) ;
#11480 = VECTOR ( 'NONE', #71260, 39.37007874015748143 ) ;
#11481 = CARTESIAN_POINT ( 'NONE',  ( -0.5249343832020990641, -0.6046776061558809534, -0.2411417322834644161 ) ) ;
#11482 = CARTESIAN_POINT ( 'NONE',  ( -1.640419947506561060, 0.05413385826771666132, 0.4176697321401328100 ) ) ;
#11484 = CARTESIAN_POINT ( 'NONE',  ( 0.7283464566929140904, -0.5400638737290845981, -0.3530559997133363437 ) ) ;
#11483 = CONICAL_SURFACE ( 'NONE', #59842, 2.165354330708661568, 0.7853981633974500554 ) ;
#11485 = CARTESIAN_POINT ( 'NONE',  ( 0.2887139107611556010, 0.2306618581243847221, -0.2411417322834647770 ) ) ;
#11486 = CARTESIAN_POINT ( 'NONE',  ( -9.594673741351313045E-17, 0.3917322834645670104, -1.344488188976378007 ) ) ;
#11487 = CARTESIAN_POINT ( 'NONE',  ( -0.9711286089238838626, -0.6046776061558807314, 0.2411417322834647770 ) ) ;
#11488 = CARTESIAN_POINT ( 'NONE',  ( 0.06561679790026316017, -0.4281496062992124485, 0.4176697321401328655 ) ) ;
#11489 = CARTESIAN_POINT ( 'NONE',  ( -0.4724409448818890911, -0.1870078740157480879, -0.4822834645669291653 ) ) ;
#11490 = CARTESIAN_POINT ( 'NONE',  ( 0.3018372703412079971, -0.004921259842519870586, -0.3153832671262229437 ) ) ;
#11491 = CARTESIAN_POINT ( 'NONE',  ( -1.607611548556429737, -0.6692913385826771977, 0.1292274648535927661 ) ) ;
#11492 = CARTESIAN_POINT ( 'NONE',  ( -0.2380158072512372769, -0.1747520019874606034, 5.672240063627636886 ) ) ;
#11493 = CARTESIAN_POINT ( 'NONE',  ( 5.463695987328526437E-16, -0.1870078740157479769, 0.4822834645669291653 ) ) ;
#11494 = CARTESIAN_POINT ( 'NONE',  ( 0.4935044252197983150, 1.488513638086841118, -0.5309055118110237448 ) ) ;
#11495 = CARTESIAN_POINT ( 'NONE',  ( 1.456692913385827515, 0.2952755905511811885, 0.000000000000000000 ) ) ;
#11496 = CARTESIAN_POINT ( 'NONE',  ( -0.3917322834645671215, 0.1049643490035301469, -2.859580052493438274 ) ) ;
#11497 = ORIENTED_EDGE ( 'NONE', *, *, #50269, .F. ) ;
#11498 = ADVANCED_FACE ( 'NONE', ( #33033 ), #65362, .F. ) ;
#11499 = VERTEX_POINT ( 'NONE', #60370 ) ;
#11500 = CARTESIAN_POINT ( 'NONE',  ( 0.7611548556430454138, 0.2306618581243847221, -0.2411417322834647770 ) ) ;
#11501 = CARTESIAN_POINT ( 'NONE',  ( 0.1509186351706042484, -0.2845877964562159024, 0.3641732283464567677 ) ) ;
#11503 = CARTESIAN_POINT ( 'NONE',  ( 1.306827173596999403, 0.000000000000000000, -0.4445507791589060620 ) ) ;
#11502 = CARTESIAN_POINT ( 'NONE',  ( 1.692913385826772421, 0.1771653543307087630, 0.000000000000000000 ) ) ;
#11504 = CARTESIAN_POINT ( 'NONE',  ( -0.3917322834645669549, -0.1049643490035306603, -1.075459317585301777 ) ) ;
#11505 = CARTESIAN_POINT ( 'NONE',  ( 0.1265901696524989462, 0.4724409448818897572, 0.08727034120734905587 ) ) ;
#11506 = FILL_AREA_STYLE_COLOUR ( '', #8318 ) ;
#11507 = CARTESIAN_POINT ( 'NONE',  ( -9.787531504996566615E-17, 0.3996062992125985480, -2.753937007874015741 ) ) ;
#11508 = CARTESIAN_POINT ( 'NONE',  ( 0.3018372703412079971, -0.4281496062992124485, 0.4176697321401328655 ) ) ;
#11509 = CARTESIAN_POINT ( 'NONE',  ( -1.122047244094487306, 0.1660481256975883668, -0.3530559997133364547 ) ) ;
#11510 = CARTESIAN_POINT ( 'NONE',  ( -1.076115485564303809, 0.2306618581243848609, 0.2411417322834645549 ) ) ;
#11511 = CARTESIAN_POINT ( 'NONE',  ( 0.3805774278215230400, 0.05413385826771626580, -0.4176697321401330321 ) ) ;
#11512 = CARTESIAN_POINT ( 'NONE',  ( 1.122047244094488860, 0.1660481256975885056, 0.3530559997133364547 ) ) ;
#11513 = CARTESIAN_POINT ( 'NONE',  ( 1.535433070866142558, 0.1771653543307087630, 0.000000000000000000 ) ) ;
#11514 = CARTESIAN_POINT ( 'NONE',  ( 1.437007874015748810, -0.4536011799217368745, -0.2665933059059886201 ) ) ;
#11515 = CARTESIAN_POINT ( 'NONE',  ( -1.017060367454067249, -0.05778040916215522460, 0.4822834645669289988 ) ) ;
#11516 = CARTESIAN_POINT ( 'NONE',  ( 0.1998031496062994128, -0.3460692066303957537, -0.4835958005249343938 ) ) ;
#11517 = CARTESIAN_POINT ( 'NONE',  ( 1.601049868766404982, -0.6046776061558809534, -0.2411417322834644161 ) ) ;
#11518 = CARTESIAN_POINT ( 'NONE',  ( -0.2867679344610364334, -0.2867679344610367109, -0.3661417322834645827 ) ) ;
#11519 = CARTESIAN_POINT ( 'NONE',  ( -0.3412073490813641308, 0.2306618581243847221, -0.2411417322834647770 ) ) ;
#11521 = CARTESIAN_POINT ( 'NONE',  ( -0.3003296953576023443, 1.169860122871907882, 1.947534171620900922 ) ) ;
#11520 = CARTESIAN_POINT ( 'NONE',  ( 1.076115485564305141, 0.2306618581243847221, -0.2411417322834647770 ) ) ;
#11522 = CARTESIAN_POINT ( 'NONE',  ( -1.607611548556429737, -0.5511811023622046335, 0.09757992244046803654 ) ) ;
#11523 = CARTESIAN_POINT ( 'NONE',  ( 0.5446194225721792126, -0.3162353388693405765, 0.4822834645669290543 ) ) ;
#11524 = CARTESIAN_POINT ( 'NONE',  ( 0.9776902887139113929, 0.1771653543307087630, 0.09757992244046791164 ) ) ;
#11525 = CARTESIAN_POINT ( 'NONE',  ( -1.581364829396324945, -0.2845877964562159024, 0.3641732283464567677 ) ) ;
#11526 = CARTESIAN_POINT ( 'NONE',  ( 0.7480314960629927956, 0.2952755905511811885, 0.000000000000000000 ) ) ;
#11527 = DIRECTION ( 'NONE',  ( -1.000000000000000000, -0.000000000000000000, -0.000000000000000000 ) ) ;
#11528 = CARTESIAN_POINT ( 'NONE',  ( -0.6364829396325453192, -0.2845877964562159024, 0.3641732283464567677 ) ) ;
#11529 = CARTESIAN_POINT ( 'NONE',  ( -0.7020997375328076329, -0.3162353388693409650, -0.4822834645669289433 ) ) ;
#11530 = CARTESIAN_POINT ( 'NONE',  ( 1.456692913385827515, -0.6692913385826771977, 8.415575281601705876E-17 ) ) ;
#11531 = CARTESIAN_POINT ( 'NONE',  ( -0.7086614173228339419, -0.1870078740157480879, -0.4822834645669291653 ) ) ;
#11532 = CARTESIAN_POINT ( 'NONE',  ( 1.528871391076116026, 0.2952755905511811885, 0.1292274648535926551 ) ) ;
#11533 = CARTESIAN_POINT ( 'NONE',  ( -0.1958661417322836995, 0.3392501089628017219, -0.9547437252306580913 ) ) ;
#11534 = CARTESIAN_POINT ( 'NONE',  ( -0.9448818897637790704, -0.1870078740157480601, -0.3641732283464567677 ) ) ;
#11535 = CARTESIAN_POINT ( 'NONE',  ( 1.120401492038572977, 1.066895646367433503, -0.06275413064580409594 ) ) ;
#11536 = CARTESIAN_POINT ( 'NONE',  ( 1.528871391076116026, -0.6692913385826773087, -0.1292274648535924053 ) ) ;
#11537 = CARTESIAN_POINT ( 'NONE',  ( 0.1265901696524989462, 0.4724409448818897572, -1.959973753280839892 ) ) ;
#11538 = VECTOR ( 'NONE', #53187, 39.37007874015748143 ) ;
#11539 = CARTESIAN_POINT ( 'NONE',  ( -0.09067318884954536640, -4.069555009745408348E-17, -0.3627989612356148363 ) ) ;
#11540 = CARTESIAN_POINT ( 'NONE',  ( 1.646981627296588035, -0.3162353388693405765, 0.4822834645669290543 ) ) ;
#11541 = CARTESIAN_POINT ( 'NONE',  ( -1.200787401574802349, 0.07958543189024071263, -0.2665933059059888421 ) ) ;
#11542 = DIRECTION ( 'NONE',  ( 1.000000000000000000, -0.000000000000000000, -0.000000000000000000 ) ) ;
#11543 = CARTESIAN_POINT ( 'NONE',  ( -0.2230971128608915943, 0.05413385826771666132, 0.4176697321401328100 ) ) ;
#11544 = CARTESIAN_POINT ( 'NONE',  ( 0.1181102362204730916, 0.1771653543307087630, 0.000000000000000000 ) ) ;
#11545 = CARTESIAN_POINT ( 'NONE',  ( -1.135170603674539924, -0.5511811023622046335, 0.09757992244046803654 ) ) ;
#11546 = CARTESIAN_POINT ( 'NONE',  ( 1.305774278215223960, 0.1771653543307087075, -0.09757992244046823083 ) ) ;
#11547 = CARTESIAN_POINT ( 'NONE',  ( 0.8398950131233602345, -0.6046776061558807314, 0.2411417322834647770 ) ) ;
#11548 = CARTESIAN_POINT ( 'NONE',  ( 1.607611548556431069, 0.2952755905511811885, 0.1292274648535926551 ) ) ;
#11549 = CARTESIAN_POINT ( 'NONE',  ( 0.4002624671916016896, -0.08942795157527998196, 0.3641732283464567121 ) ) ;
#11550 = DIMENSIONAL_EXPONENTS ( 1.000000000000000000, 0.000000000000000000, 0.000000000000000000, 0.000000000000000000, 0.000000000000000000, 0.000000000000000000, 0.000000000000000000 ) ;
#11551 = CARTESIAN_POINT ( 'NONE',  ( 0.4068241469816281097, 0.05413385826771666132, 0.4176697321401328100 ) ) ;
#11552 = CARTESIAN_POINT ( 'NONE',  ( 0.8070866141732288002, 0.07958543189024085140, 0.2665933059059887866 ) ) ;
#11553 = VERTEX_POINT ( 'NONE', #46482 ) ;
#11554 = CARTESIAN_POINT ( 'NONE',  ( -1.338582677165353729, -0.1870078740157479769, 0.4822834645669291653 ) ) ;
#11555 = EDGE_CURVE ( 'NONE', #45807, #60217, #35784, .T. ) ;
#11556 = CARTESIAN_POINT ( 'NONE',  ( -1.167979002624671470, 0.05413385826771666132, 0.4176697321401328100 ) ) ;
#11557 = CARTESIAN_POINT ( 'NONE',  ( 0.03937007874015806264, 0.2952755905511811885, 0.000000000000000000 ) ) ;
#11558 = CARTESIAN_POINT ( 'NONE',  ( -0.3460692066303960868, 0.1998031496062990242, -0.02624671916010500733 ) ) ;
#11559 = CARTESIAN_POINT ( 'NONE',  ( -0.3460692066303960313, 0.1998031496062989965, -2.780183727034120977 ) ) ;
#11560 = CARTESIAN_POINT ( 'NONE',  ( 0.6036745406824153282, -0.6046776061558807314, 0.2411417322834647770 ) ) ;
#11561 = CARTESIAN_POINT ( 'NONE',  ( 1.358267716535433323, -0.4536011799217368745, -0.2665933059059886201 ) ) ;
#11562 = CARTESIAN_POINT ( 'NONE',  ( 0.03937007874015833325, -0.6692913385826771977, 8.415575281601705876E-17 ) ) ;
#11563 = CARTESIAN_POINT ( 'NONE',  ( 0.3740157480314966754, 0.1660481256975883668, -0.3530559997133364547 ) ) ;
#11564 = CARTESIAN_POINT ( 'NONE',  ( -0.3996062992125986035, -7.340648628747425578E-17, -2.086614173228346303 ) ) ;
#11565 = CARTESIAN_POINT ( 'NONE',  ( 0.3949938075777409963, 2.418639510665530435E-17, -1.535433070866141447 ) ) ;
#11566 = CARTESIAN_POINT ( 'NONE',  ( 0.3996062992125986590, -0.1070741851644053111, -2.788713910761154047 ) ) ;
#11567 = FACE_OUTER_BOUND ( 'NONE', #56370, .T. ) ;
#11568 = CARTESIAN_POINT ( 'NONE',  ( 0.2867679344610366554, -0.2867679344610365444, -0.4055118110236220486 ) ) ;
#11569 = CARTESIAN_POINT ( 'NONE',  ( -0.5052493438320203589, -0.5511811023622046335, 0.09757992244046803654 ) ) ;
#11570 = CARTESIAN_POINT ( 'NONE',  ( -0.6627296587926503335, -0.6692913385826771977, 0.1292274648535927661 ) ) ;
#11571 = CARTESIAN_POINT ( 'NONE',  ( 0.5971128608923890191, -0.6692913385826771977, 0.1292274648535927661 ) ) ;
#11572 = CARTESIAN_POINT ( 'NONE',  ( 0.3949938075777408852, 0.1058382717557500435, -2.563648293963254776 ) ) ;
#11573 = CARTESIAN_POINT ( 'NONE',  ( 0.7217847769028878924, 0.05413385826771666132, 0.4176697321401328100 ) ) ;
#11574 = CARTESIAN_POINT ( 'NONE',  ( -1.568241469816272105, -0.3162353388693409650, -0.4822834645669289433 ) ) ;
#11575 = CARTESIAN_POINT ( 'NONE',  ( 0.6824146981627303710, 0.2306618581243847221, -0.2411417322834647770 ) ) ;
#11576 = CARTESIAN_POINT ( 'NONE',  ( -0.4724409448818895907, -0.1265901696524993070, -2.723097112860892288 ) ) ;
#11577 = CIRCLE ( 'NONE', #29050, 3.937007874015748143 ) ;
#11578 = CARTESIAN_POINT ( 'NONE',  ( -0.3460692066303958092, -0.1998031496062994683, -2.257217847769029007 ) ) ;
#11579 = CARTESIAN_POINT ( 'NONE',  ( 1.555118110236221041, 0.1660481256975883668, -0.3530559997133364547 ) ) ;
#11580 = AXIS2_PLACEMENT_3D ( 'NONE', #73981, #68078, #16327 ) ;
#11581 = CARTESIAN_POINT ( 'NONE',  ( 1.062992125984252745, -0.6692913385826771977, 8.415575281601705876E-17 ) ) ;
#11582 = CARTESIAN_POINT ( 'NONE',  ( 0.5380577427821529035, 0.05413385826771626580, -0.4176697321401330321 ) ) ;
#11583 = CARTESIAN_POINT ( 'NONE',  ( 1.240157480314961314, -0.4536011799217367080, 0.2665933059059888421 ) ) ;
#11585 = CARTESIAN_POINT ( 'NONE',  ( -1.614173228346455824, 0.2952755905511811885, 0.000000000000000000 ) ) ;
#11584 = CARTESIAN_POINT ( 'NONE',  ( -1.423884514435694859, -0.08942795157528024563, -0.3641732283464568787 ) ) ;
#11586 = CARTESIAN_POINT ( 'NONE',  ( -0.1049643490035302024, -0.3917322834645671215, -0.1568241469816273603 ) ) ;
#11587 = CYLINDRICAL_SURFACE ( 'NONE', #13077, 1.181102362204724310 ) ;
#11588 = CARTESIAN_POINT ( 'NONE',  ( 0.7939632545931766261, -0.3162353388693409650, -0.4822834645669289433 ) ) ;
#11589 = FACE_OUTER_BOUND ( 'NONE', #50870, .T. ) ;
#11590 = CARTESIAN_POINT ( 'NONE',  ( -0.3346456692913377662, -0.5400638737290844871, 0.3530559997133364547 ) ) ;
#11591 = CARTESIAN_POINT ( 'NONE',  ( -0.9776902887139098386, -0.6692913385826771977, 0.1292274648535927661 ) ) ;
#11592 = CARTESIAN_POINT ( 'NONE',  ( 1.023622047244095112, -0.1870078740157480879, -0.4822834645669291653 ) ) ;
#11593 = CARTESIAN_POINT ( 'NONE',  ( 0.1049643490035304938, -0.3917322834645669549, -0.4849081364829396779 ) ) ;
#11594 = CARTESIAN_POINT ( 'NONE',  ( -0.3917322834645671215, 0.1049643490035301469, -1.442257217847769057 ) ) ;
#11595 = CARTESIAN_POINT ( 'NONE',  ( 0.1958661417322836440, -0.3392501089628017219, -2.918635170603674389 ) ) ;
#11596 = CARTESIAN_POINT ( 'NONE',  ( 1.548556430446194954, 0.2306618581243847221, -0.2411417322834647770 ) ) ;
#11597 = ORIENTED_EDGE ( 'NONE', *, *, #35215, .F. ) ;
#11598 = CARTESIAN_POINT ( 'NONE',  ( 0.1974969037888704704, 0.3420746716998660508, -2.664041994750656173 ) ) ;
#11599 = ORIENTED_EDGE ( 'NONE', *, *, #73594, .F. ) ;
#11600 = CARTESIAN_POINT ( 'NONE',  ( 0.000000000000000000, 2.559055118110236560, 0.000000000000000000 ) ) ;
#11601 = CIRCLE ( 'NONE', #73426, 0.3149606299212597271 ) ;
#11602 = CARTESIAN_POINT ( 'NONE',  ( 1.450131233595801428, 0.1771653543307087630, 0.09757992244046791164 ) ) ;
#11603 = CARTESIAN_POINT ( 'NONE',  ( 0.3996062992125986035, 0.1070741851644054776, -1.384514435695537671 ) ) ;
#11604 = CARTESIAN_POINT ( 'NONE',  ( 1.614173228346457378, -0.5511811023622047445, 6.969142054262312111E-17 ) ) ;
#11605 = CARTESIAN_POINT ( 'NONE',  ( -0.1938976377952756625, -0.1938976377952756625, -0.3740157480314971750 ) ) ;
#11606 = DIRECTION ( 'NONE',  ( -0.000000000000000000, 1.000000000000000000, -0.000000000000000000 ) ) ;
#11607 = CARTESIAN_POINT ( 'NONE',  ( -0.6299212598425059095, 2.165354330708661568, -3.937007874015764131 ) ) ;
#11608 = CARTESIAN_POINT ( 'NONE',  ( 0.3392501089628018884, -0.1958661417322834220, -0.5045931758530184386 ) ) ;
#11609 = CARTESIAN_POINT ( 'NONE',  ( -0.9120734908136475250, -0.5511811023622048555, -0.09757992244046775898 ) ) ;
#11610 = CARTESIAN_POINT ( 'NONE',  ( -1.266404199475064773, -0.2845877964562159024, 0.3641732283464567677 ) ) ;
#11611 = CARTESIAN_POINT ( 'NONE',  ( -1.089238845144356427, -0.4281496062992127816, -0.4176697321401328100 ) ) ;
#11612 = CARTESIAN_POINT ( 'NONE',  ( 0.3083989501312343062, -0.3162353388693405765, 0.4822834645669290543 ) ) ;
#11613 = CARTESIAN_POINT ( 'NONE',  ( -1.404199475065615932, -0.4281496062992127816, -0.4176697321401328100 ) ) ;
#11614 = VERTEX_POINT ( 'NONE', #54039 ) ;
#11615 = CARTESIAN_POINT ( 'NONE',  ( 1.469816272965879911, 0.2306618581243847221, -0.2411417322834647770 ) ) ;
#11616 = CARTESIAN_POINT ( 'NONE',  ( -1.157146581871515012E-16, 0.4724409448818898682, -2.204724409448818978 ) ) ;
#11617 = DIRECTION ( 'NONE',  ( -3.491481338843132961E-15, -0.000000000000000000, 1.000000000000000000 ) ) ;
#11618 = CARTESIAN_POINT ( 'NONE',  ( -0.6299212598425188991, -0.1870078740157480601, -0.3641732283464567677 ) ) ;
#11619 = CARTESIAN_POINT ( 'NONE',  ( -1.122047244094487306, 0.1660481256975883668, -0.3530559997133364547 ) ) ;
#11620 = CARTESIAN_POINT ( 'NONE',  ( 0.9448818897637802916, -0.1870078740157480879, -0.4822834645669291653 ) ) ;
#11621 = VERTEX_POINT ( 'NONE', #53208 ) ;
#11623 = DIRECTION ( 'NONE',  ( 0.000000000000000000, 1.000000000000000000, -0.000000000000000000 ) ) ;
#11622 = CARTESIAN_POINT ( 'NONE',  ( -0.4724409448818880364, -0.1265901696525023323, -2.250656167979002920 ) ) ;
#11624 = ADVANCED_FACE ( 'NONE', ( #72177 ), #57252, .F. ) ;
#11625 = CARTESIAN_POINT ( 'NONE',  ( -3.937007874015748143, 2.559055118110236560, 0.3149606299212596716 ) ) ;
#11626 = CARTESIAN_POINT ( 'NONE',  ( -1.069553805774277722, 0.2952755905511811885, 0.1292274648535926551 ) ) ;
#11627 = CARTESIAN_POINT ( 'NONE',  ( -0.3917322834645668994, -0.1049643490035306742, -0.2834452511472947966 ) ) ;
#11628 = CARTESIAN_POINT ( 'NONE',  ( 0.1837270341207354329, 0.1283753931104748280, 0.1820866141732283561 ) ) ;
#11629 = CARTESIAN_POINT ( 'NONE',  ( -0.3392501089628017219, -0.1958661417322836718, -0.7670603674540683592 ) ) ;
#11630 = EDGE_CURVE ( 'NONE', #33945, #30219, #10257, .T. ) ;
#11631 = CARTESIAN_POINT ( 'NONE',  ( 0.05905511811023709395, -0.4536011799217367080, 0.2665933059059888421 ) ) ;
#11632 = CARTESIAN_POINT ( 'NONE',  ( 0.5183727034120741983, 0.1771653543307087075, -0.09757992244046823083 ) ) ;
#11633 = CARTESIAN_POINT ( 'NONE',  ( 0.5446194225721792126, -0.05778040916215560624, -0.4822834645669293319 ) ) ;
#11634 = CARTESIAN_POINT ( 'NONE',  ( -0.8202099737532799750, 0.1771653543307087075, -0.09757992244046823083 ) ) ;
#11635 = CARTESIAN_POINT ( 'NONE',  ( 0.3917322834645669549, 0.1049643490035304660, -2.636482939632545985 ) ) ;
#11636 = CARTESIAN_POINT ( 'NONE',  ( 1.062992125984252745, -0.6692913385826771977, 8.415575281601705876E-17 ) ) ;
#11637 = VECTOR ( 'NONE', #58811, 39.37007874015748143 ) ;
#11638 = CARTESIAN_POINT ( 'NONE',  ( -1.167979002624671470, 0.05413385826771666132, 0.4176697321401328100 ) ) ;
#11639 = AXIS2_PLACEMENT_3D ( 'NONE', #7922, #15906, #33583 ) ;
#11640 = CARTESIAN_POINT ( 'NONE',  ( -0.4091458600556405756, 0.2362204724409446288, -0.5754593175853018883 ) ) ;
#11641 = AXIS2_PLACEMENT_3D ( 'NONE', #61675, #4016, #29270 ) ;
#11642 = CARTESIAN_POINT ( 'NONE',  ( 0.02624671916010564918, 0.2306618581243848609, 0.2411417322834645549 ) ) ;
#11643 = CARTESIAN_POINT ( 'NONE',  ( -0.4265091863517051496, -0.6692913385826771977, 0.1292274648535927661 ) ) ;
#11644 = CARTESIAN_POINT ( 'NONE',  ( 1.391076115485564868, 0.1283753931104746893, -0.1820866141732285504 ) ) ;
#11645 = CARTESIAN_POINT ( 'NONE',  ( 0.2427821522309716595, -0.2845877964562161244, -0.3641732283464567121 ) ) ;
#11646 = CARTESIAN_POINT ( 'NONE',  ( -0.1509186351706028884, -0.05778040916215522460, 0.4822834645669289988 ) ) ;
#11647 = CARTESIAN_POINT ( 'NONE',  ( -1.161417322834644716, 0.1660481256975885056, 0.3530559997133364547 ) ) ;
#11648 = CARTESIAN_POINT ( 'NONE',  ( -3.821484228344193657, 2.755905511811024056, 0.5314960629921260393 ) ) ;
#11649 = CARTESIAN_POINT ( 'NONE',  ( 0.4724409448818897017, 0.1265901696524990294, -0.2821522309711286258 ) ) ;
#11650 = CARTESIAN_POINT ( 'NONE',  ( -0.2099737532808391705, 0.2306618581243848609, 0.2411417322834645549 ) ) ;
#11651 = CARTESIAN_POINT ( 'NONE',  ( -1.194225721784776262, 0.05413385826771626580, -0.4176697321401330321 ) ) ;
#11652 = ORIENTED_EDGE ( 'NONE', *, *, #66673, .F. ) ;
#11653 = CARTESIAN_POINT ( 'NONE',  ( 4.893765752498283308E-17, -0.3996062992125985480, -1.887795275590550936 ) ) ;
#11654 = CARTESIAN_POINT ( 'NONE',  ( 1.154855643044620184, 0.2306618581243847221, -0.2411417322834647770 ) ) ;
#11655 = CARTESIAN_POINT ( 'NONE',  ( -0.6627296587926503335, -0.5511811023622046335, 0.09757992244046803654 ) ) ;
#11656 = AXIS2_PLACEMENT_3D ( 'NONE', #8390, #34055, #8801 ) ;
#11657 = CARTESIAN_POINT ( 'NONE',  ( -0.6496062992125976043, -0.5400638737290844871, 0.3530559997133364547 ) ) ;
#11658 = CARTESIAN_POINT ( 'NONE',  ( 1.227034120734908917, 0.2952755905511810774, -0.1292274648535930714 ) ) ;
#11659 = CARTESIAN_POINT ( 'NONE',  ( 0.8989501312335964611, 0.2952755905511811885, 0.1292274648535926551 ) ) ;
#11660 = CARTESIAN_POINT ( 'NONE',  ( -0.3503937007874015630, 0.3733313776025731778, -0.01968503937007957602 ) ) ;
#11661 = CARTESIAN_POINT ( 'NONE',  ( -1.233595800524933894, 0.1283753931104748280, 0.1820866141732283561 ) ) ;
#11662 = CARTESIAN_POINT ( 'NONE',  ( -0.3996062992125986035, 0.1070741851644051584, -0.5820209973753279753 ) ) ;
#11664 = ADVANCED_FACE ( 'NONE', ( #65869 ), #34465, .F. ) ;
#11663 = CARTESIAN_POINT ( 'NONE',  ( 0.2925321140481932369, 0.2925321140481932369, -1.082677165354330562 ) ) ;
#11665 = CARTESIAN_POINT ( 'NONE',  ( -0.3949938075777409963, -7.255918531996591613E-17, -0.3543307086614174151 ) ) ;
#11666 = CARTESIAN_POINT ( 'NONE',  ( 0.3304432287027126991, 1.196939817260626926, -1.404940052879173118 ) ) ;
#11667 = CARTESIAN_POINT ( 'NONE',  ( 1.181102362204725198, -0.1870078740157479769, 0.3641732283464567677 ) ) ;
#11668 = CARTESIAN_POINT ( 'NONE',  ( 0.6036745406824153282, -0.5023911411419708095, 0.1820866141732285504 ) ) ;
#11669 = CARTESIAN_POINT ( 'NONE',  ( 0.6758530183727039509, 0.2952755905511810774, -0.1292274648535930714 ) ) ;
#11670 = DIRECTION ( 'NONE',  ( 0.000000000000000000, -1.000000000000000000, 0.000000000000000000 ) ) ;
#11671 = CARTESIAN_POINT ( 'NONE',  ( -0.3949938075777409963, -7.255918531996591613E-17, -1.218503937007874072 ) ) ;
#11672 = CARTESIAN_POINT ( 'NONE',  ( 0.8398950131233602345, -0.5023911411419708095, 0.1820866141732285504 ) ) ;
#11673 = CARTESIAN_POINT ( 'NONE',  ( -0.3149606299212590610, -0.1870078740157480879, -0.4822834645669291653 ) ) ;
#11674 = CARTESIAN_POINT ( 'NONE',  ( -1.423884514435694859, -0.05778040916215560624, -0.4822834645669293319 ) ) ;
#11675 = CARTESIAN_POINT ( 'NONE',  ( 1.076115485564305141, 0.2306618581243847221, -0.2411417322834647770 ) ) ;
#11676 = CARTESIAN_POINT ( 'NONE',  ( 0.4724409448818898682, 2.892866454678787531E-17, -1.377952755905511806 ) ) ;
#11677 = CARTESIAN_POINT ( 'NONE',  ( -0.1998031496062994683, 0.3460692066303958092, -2.532808398950130879 ) ) ;
#11678 = CARTESIAN_POINT ( 'NONE',  ( -0.1771653543307080136, -0.4536011799217367080, 0.2665933059059888421 ) ) ;
#11679 =( BOUNDED_CURVE ( )  B_SPLINE_CURVE ( 2, ( #59803, #2988, #53894, #60226, #2157, #48003, #53484, #40869, #72860, #54313, #79194, #22343, #27402 ),
 .UNSPECIFIED., .F., .F. ) 
 B_SPLINE_CURVE_WITH_KNOTS ( ( 3, 2, 2, 2, 2, 2, 3 ),
 ( 0.7124999999999999112, 0.7166666666666665630, 0.7208333333333332149, 0.7249999999999998668, 0.7291666666666665186, 0.7333333333333331705, 0.7374999999999999334 ),
 .UNSPECIFIED. ) 
 CURVE ( )  GEOMETRIC_REPRESENTATION_ITEM ( )  RATIONAL_B_SPLINE_CURVE ( ( 1.000000000000000888, 0.9659258262890674240, 1.000000000000000000, 0.9659258262890683122, 1.000000000000000000, 0.9659258262890683122, 1.000000000000000000, 0.9659258262890683122, 1.000000000000000000, 0.9659258262890683122, 1.000000000000000000, 0.9659258262890692004, 0.9999999999999991118 ) ) 
 REPRESENTATION_ITEM ( '' )  );
#11680 = ORIENTED_EDGE ( 'NONE', *, *, #16612, .F. ) ;
#11681 = ORIENTED_EDGE ( 'NONE', *, *, #41165, .T. ) ;
#11682 = CARTESIAN_POINT ( 'NONE',  ( -0.9186351706036736120, 0.2306618581243848609, 0.2411417322834645549 ) ) ;
#11683 = CARTESIAN_POINT ( 'NONE',  ( -0.6167979002624665030, -0.4281496062992127816, -0.4176697321401328100 ) ) ;
#11684 = CARTESIAN_POINT ( 'NONE',  ( -0.4133858267716528645, -0.5400638737290844871, 0.3530559997133364547 ) ) ;
#11685 = CARTESIAN_POINT ( 'NONE',  ( 0.2887139107611556010, 0.2306618581243847221, -0.2411417322834647770 ) ) ;
#11686 = CARTESIAN_POINT ( 'NONE',  ( -0.5839895013123351797, -0.6692913385826771977, 0.1292274648535927661 ) ) ;
#11687 = CARTESIAN_POINT ( 'NONE',  ( -1.509186351706035767, -0.4281496062992124485, 0.4176697321401328655 ) ) ;
#11688 = CARTESIAN_POINT ( 'NONE',  ( -0.9711286089238838626, -0.6046776061558807314, 0.2411417322834647770 ) ) ;
#11689 = CARTESIAN_POINT ( 'NONE',  ( 0.5511811023622054106, -0.1870078740157480879, -0.4822834645669291653 ) ) ;
#11690 = VECTOR ( 'NONE', #22114, 39.37007874015748143 ) ;
#11691 = CARTESIAN_POINT ( 'NONE',  ( 0.3917322834645669549, 0.1049643490035304660, -1.061679790026246462 ) ) ;
#11692 = CARTESIAN_POINT ( 'NONE',  ( -0.3412073490813641308, 0.1283753931104746893, -0.1820866141732285504 ) ) ;
#11693 = ORIENTED_EDGE ( 'NONE', *, *, #70646, .F. ) ;
#11694 = CARTESIAN_POINT ( 'NONE',  ( 0.2891555358219910499, 0.2891555358219910499, -1.555118110236220375 ) ) ;
#11695 = AXIS2_PLACEMENT_3D ( 'NONE', #73945, #54559, #17122 ) ;
#11696 = ORIENTED_EDGE ( 'NONE', *, *, #80626, .F. ) ;
#11697 = CARTESIAN_POINT ( 'NONE',  ( -1.161417322834644716, -0.4536011799217368745, -0.2665933059059886201 ) ) ;
#11698 = VECTOR ( 'NONE', #9418, 39.37007874015748143 ) ;
#11699 = VECTOR ( 'NONE', #52150, 39.37007874015748854 ) ;
#11700 = CARTESIAN_POINT ( 'NONE',  ( -0.9383202099737524282, -0.3162353388693409650, -0.4822834645669289433 ) ) ;
#11701 = CARTESIAN_POINT ( 'NONE',  ( -1.023622047244093558, -0.1870078740157479769, 0.4822834645669291653 ) ) ;
#11702 = CARTESIAN_POINT ( 'NONE',  ( -0.1998031496062991907, -0.3460692066303959757, -0.3805774278215223183 ) ) ;
#11703 = CARTESIAN_POINT ( 'NONE',  ( -0.7874015748031489847, -0.1870078740157479769, 0.4822834645669291653 ) ) ;
#11704 = CARTESIAN_POINT ( 'NONE',  ( -0.6955380577427815458, -0.4281496062992127816, -0.4176697321401328100 ) ) ;
#11705 = CARTESIAN_POINT ( 'NONE',  ( -1.548556430446193399, -0.6046776061558809534, -0.2411417322834644161 ) ) ;
#11706 = DIRECTION ( 'NONE',  ( -1.000000000000000000, -0.000000000000000000, -0.000000000000000000 ) ) ;
#11707 = CARTESIAN_POINT ( 'NONE',  ( 0.4986876640419954376, -0.5023911411419708095, -0.1820866141732282451 ) ) ;
#11708 = DIRECTION ( 'NONE',  ( -3.096699300667737957E-16, 1.000000000000000000, -0.000000000000000000 ) ) ;
#11709 = CARTESIAN_POINT ( 'NONE',  ( 0.3917322834645670104, 2.398668435337828261E-17, 0.1122047244094487306 ) ) ;
#11710 = CARTESIAN_POINT ( 'NONE',  ( 0.07874015748031558404, -0.1870078740157480601, -0.3641732283464567677 ) ) ;
#11711 = CARTESIAN_POINT ( 'NONE',  ( -0.2427821522309703550, -0.3162353388693405765, 0.4822834645669290543 ) ) ;
#11712 = CARTESIAN_POINT ( 'NONE',  ( 1.332020997375328974, -0.05778040916215560624, -0.4822834645669293319 ) ) ;
#11713 = CARTESIAN_POINT ( 'NONE',  ( -0.05905511811023545637, 0.1660481256975885056, 0.3530559997133364547 ) ) ;
#11714 = VERTEX_POINT ( 'NONE', #1890 ) ;
#11715 = CARTESIAN_POINT ( 'NONE',  ( -0.3996062992125986035, -7.340648628747425578E-17, -2.244094488188976388 ) ) ;
#11716 = LINE ( 'NONE', #18437, #61434 ) ;
#11717 = ORIENTED_EDGE ( 'NONE', *, *, #27675, .T. ) ;
#11718 = CARTESIAN_POINT ( 'NONE',  ( -0.3996062992125984925, -0.1070741851644056858, -1.540026246719159886 ) ) ;
#11719 = LINE ( 'NONE', #5384, #3256 ) ;
#11720 = CARTESIAN_POINT ( 'NONE',  ( -1.240157480314959759, 0.07958543189024085140, 0.2665933059059887866 ) ) ;
#11721 = CARTESIAN_POINT ( 'NONE',  ( -1.555118110236219930, 0.1660481256975885056, 0.3530559997133364547 ) ) ;
#11722 = CARTESIAN_POINT ( 'NONE',  ( -0.2362204724409447953, -0.4091458600556404646, -0.5380577427821522374 ) ) ;
#11723 = DIRECTION ( 'NONE',  ( 0.000000000000000000, 0.000000000000000000, -1.000000000000000000 ) ) ;
#11724 = CARTESIAN_POINT ( 'NONE',  ( -0.1958661417322836718, 0.3392501089628017219, -2.774934383202099841 ) ) ;
#11725 = CARTESIAN_POINT ( 'NONE',  ( 1.332020997375329197, -0.3162353388693405765, 0.4822834645669290543 ) ) ;
#11726 = CARTESIAN_POINT ( 'NONE',  ( 0.5577427821522314977, -0.3162353388693409650, -0.4822834645669289433 ) ) ;
#11727 = CARTESIAN_POINT ( 'NONE',  ( -0.1115485564304453947, -0.6692913385826771977, 0.1292274648535927661 ) ) ;
#11728 = CARTESIAN_POINT ( 'NONE',  ( -0.8792650918635160906, -0.3690944881889763329, 0.3153832671262228327 ) ) ;
#11729 = CARTESIAN_POINT ( 'NONE',  ( -0.1574803149606292529, -0.1870078740157479769, 0.4822834645669291653 ) ) ;
#11730 = CARTESIAN_POINT ( 'NONE',  ( -0.4091458600556405756, 0.2362204724409446288, -2.150262467191601079 ) ) ;
#11731 = CARTESIAN_POINT ( 'NONE',  ( -1.003937007874015297, -0.5400638737290845981, -0.3530559997133363437 ) ) ;
#11732 = ADVANCED_FACE ( 'NONE', ( #15355 ), #40597, .F. ) ;
#11733 = CARTESIAN_POINT ( 'NONE',  ( 0.1058382717557499880, 0.3949938075777409408, -2.117454068241470200 ) ) ;
#11734 = CARTESIAN_POINT ( 'NONE',  ( 1.351706036745407458, -0.3690944881889765550, -0.3153832671262227771 ) ) ;
#11735 = CARTESIAN_POINT ( 'NONE',  ( -0.2034120734908131112, -0.5511811023622048555, -0.09757992244046775898 ) ) ;
#11736 = CARTESIAN_POINT ( 'NONE',  ( 1.167979002624672580, -0.3690944881889763329, 0.3153832671262228327 ) ) ;
#11737 = CARTESIAN_POINT ( 'NONE',  ( -1.384514435695537005, 0.2952755905511811885, 0.1292274648535926551 ) ) ;
#11738 = CARTESIAN_POINT ( 'NONE',  ( -0.9645669291338575535, 0.07958543189024071263, -0.2665933059059888421 ) ) ;
#11739 = CARTESIAN_POINT ( 'NONE',  ( 0.4768059346183038394, 1.738380701482456381, 0.5050996235782295729 ) ) ;
#11740 = CARTESIAN_POINT ( 'NONE',  ( 0.5577427821522316087, -0.08942795157527998196, 0.3641732283464567121 ) ) ;
#11741 = CARTESIAN_POINT ( 'NONE',  ( -0.8989501312335946848, -0.6692913385826771977, 0.1292274648535927661 ) ) ;
#11742 = CARTESIAN_POINT ( 'NONE',  ( 0.2559055118110243887, 0.1660481256975885056, 0.3530559997133364547 ) ) ;
#11743 = CARTESIAN_POINT ( 'NONE',  ( 0.1115485564304470323, 0.1771653543307087630, 0.09757992244046791164 ) ) ;
#11744 = CARTESIAN_POINT ( 'NONE',  ( -1.482939632545930975, -0.3690944881889765550, -0.3153832671262227771 ) ) ;
#11745 = CARTESIAN_POINT ( 'NONE',  ( 0.6561679790026253567, -0.6046776061558809534, -0.2411417322834644161 ) ) ;
#11746 = DIRECTION ( 'NONE',  ( 1.000000000000000000, 0.000000000000000000, 0.000000000000000000 ) ) ;
#11747 = CARTESIAN_POINT ( 'NONE',  ( 1.200787401574803681, -0.4536011799217368745, -0.2665933059059886201 ) ) ;
#11748 = CARTESIAN_POINT ( 'NONE',  ( -0.8661417322834640276, -0.1870078740157480879, -0.4822834645669291653 ) ) ;
#11749 = CARTESIAN_POINT ( 'NONE',  ( -0.3871391076115476282, -0.08942795157527998196, 0.3641732283464567121 ) ) ;
#11750 = CARTESIAN_POINT ( 'NONE',  ( 0.3438254193631122835, 0.3704879858182167918, -0.01311675794578955577 ) ) ;
#11751 = CARTESIAN_POINT ( 'NONE',  ( 0.4133858267716541968, -0.4536011799217368745, -0.2665933059059886201 ) ) ;
#11752 = CARTESIAN_POINT ( 'NONE',  ( -0.9842519685039365918, -0.6692913385826771977, 8.415575281601705876E-17 ) ) ;
#11753 = CARTESIAN_POINT ( 'NONE',  ( -0.4724409448818890911, -0.1870078740157480879, -0.4822834645669291653 ) ) ;
#11754 = CARTESIAN_POINT ( 'NONE',  ( 0.1998031496062994128, -0.3460692066303957537, -0.6410761154855643129 ) ) ;
#11755 = AXIS2_PLACEMENT_3D ( 'NONE', #72906, #2625, #79656 ) ;
#11756 = CARTESIAN_POINT ( 'NONE',  ( -0.1049643490035307020, 0.3917322834645669549, -2.453412073490813139 ) ) ;
#11757 = CARTESIAN_POINT ( 'NONE',  ( 0.8136482939632553313, 0.1283753931104748280, 0.1820866141732283561 ) ) ;
#11759 = CIRCLE ( 'NONE', #41320, 0.4822834645669291653 ) ;
#11758 = CARTESIAN_POINT ( 'NONE',  ( -0.1837270341207340729, 0.2306618581243847221, -0.2411417322834647770 ) ) ;
#11760 = CARTESIAN_POINT ( 'NONE',  ( -0.7545931758530176614, -0.6692913385826773087, -0.1292274648535924053 ) ) ;
#11761 = CARTESIAN_POINT ( 'NONE',  ( -0.8202099737532799750, 0.1771653543307087075, -0.09757992244046823083 ) ) ;
#11762 = CARTESIAN_POINT ( 'NONE',  ( 0.000000000000000000, 2.755905511811024056, 0.000000000000000000 ) ) ;
#11763 = CARTESIAN_POINT ( 'NONE',  ( 0.09186351706036827158, 0.05413385826771666132, 0.4176697321401328100 ) ) ;
#11764 = CARTESIAN_POINT ( 'NONE',  ( -1.627296587926508442, -0.5023911411419708095, -0.1820866141732282451 ) ) ;
#11765 = CARTESIAN_POINT ( 'NONE',  ( -1.574803149606298192, -0.1870078740157480879, -0.4822834645669291653 ) ) ;
#11766 = DIRECTION ( 'NONE',  ( -0.000000000000000000, -1.000000000000000000, -0.000000000000000000 ) ) ;
#11767 = ORIENTED_EDGE ( 'NONE', *, *, #63922, .F. ) ;
#11768 = CARTESIAN_POINT ( 'NONE',  ( 0.000000000000000000, 2.677165354330708791, 0.000000000000000000 ) ) ;
#11769 = CARTESIAN_POINT ( 'NONE',  ( -1.437007874015747477, -0.5400638737290844871, 0.3530559997133364547 ) ) ;
#11770 = CARTESIAN_POINT ( 'NONE',  ( -0.9645669291338575535, -0.5400638737290844871, 0.3530559997133364547 ) ) ;
#11771 = B_SPLINE_CURVE_WITH_KNOTS ( 'NONE', 3,
 ( #77512, #34560, #33725, #65731, #66135, #21098, #73280, #72450, #28654, #14799, #46757, #41285, #22750, #78774, #80024, #8064, #28235, #61051, #66971, #21925, #35386, #72031 ),
 .UNSPECIFIED., .F., .F.,
 ( 4, 2, 2, 2, 2, 2, 2, 2, 2, 2, 4 ),
 ( 0.002118322035362868189, 0.002486146450160856784, 0.002853970864958844944, 0.003589619694554808255, 0.004325268524150771565, 0.005060917353746734876, 0.005796566183342697319, 0.006532215012938659762, 0.006900039427736632744, 0.007267863842534605726, 0.008003512672130536076 ),
 .UNSPECIFIED. ) ;
#11772 = CARTESIAN_POINT ( 'NONE',  ( 1.528871391076116026, -0.6692913385826773087, -0.1292274648535924053 ) ) ;
#11773 = CARTESIAN_POINT ( 'NONE',  ( -0.3392501089628017219, -0.1958661417322836718, -1.869422572178477848 ) ) ;
#11774 = DIRECTION ( 'NONE',  ( -1.000000000000000000, 0.000000000000000000, 0.000000000000000000 ) ) ;
#11775 = CARTESIAN_POINT ( 'NONE',  ( 0.9055118110236227702, 0.2952755905511811885, 0.000000000000000000 ) ) ;
#11776 = CARTESIAN_POINT ( 'NONE',  ( 0.4986876640419954376, -0.6046776061558809534, -0.2411417322834644161 ) ) ;
#11777 = CARTESIAN_POINT ( 'NONE',  ( -0.3458507752293909498, 0.3458507752293908388, -0.4921259842519684624 ) ) ;
#11778 = CARTESIAN_POINT ( 'NONE',  ( 0.1070741851644053527, 0.3996062992125985480, -2.589895013123359568 ) ) ;
#11779 = CARTESIAN_POINT ( 'NONE',  ( 1.213910761154856299, -0.5511811023622048555, -0.09757992244046775898 ) ) ;
#11780 = CARTESIAN_POINT ( 'NONE',  ( 0.1998031496062992740, 0.3460692066303959757, -1.089238845144356871 ) ) ;
#11781 = ORIENTED_EDGE ( 'NONE', *, *, #79349, .T. ) ;
#11782 = CARTESIAN_POINT ( 'NONE',  ( 0.1049643490035303689, 0.3917322834645670104, -2.662729658792650778 ) ) ;
#11783 = VERTEX_POINT ( 'NONE', #78920 ) ;
#11784 = CARTESIAN_POINT ( 'NONE',  ( 0.4068241469816279987, -0.4281496062992127816, -0.4176697321401328100 ) ) ;
#11785 = CARTESIAN_POINT ( 'NONE',  ( -0.7808398950131225646, -0.05778040916215522460, 0.4822834645669289988 ) ) ;
#11786 = CARTESIAN_POINT ( 'NONE',  ( 1.607611548556431069, 0.2952755905511811885, 0.1292274648535926551 ) ) ;
#11787 = CARTESIAN_POINT ( 'NONE',  ( 1.200787401574803681, 0.1660481256975885056, 0.3530559997133364547 ) ) ;
#11788 = CARTESIAN_POINT ( 'NONE',  ( -1.601049868766403650, 0.1283753931104746893, -0.1820866141732285504 ) ) ;
#11789 = CYLINDRICAL_SURFACE ( 'NONE', #50718, 0.4724409448818898682 ) ;
#11790 = CARTESIAN_POINT ( 'NONE',  ( -0.1771653543307080136, 0.1660481256975883668, -0.3530559997133364547 ) ) ;
#11791 = CARTESIAN_POINT ( 'NONE',  ( -1.417322834645668772, -0.1870078740157480879, -0.4822834645669291653 ) ) ;
#11792 = CARTESIAN_POINT ( 'NONE',  ( -1.568241469816272105, -0.3162353388693409650, -0.4822834645669289433 ) ) ;
#11793 = CARTESIAN_POINT ( 'NONE',  ( 1.391076115485564868, 0.2306618581243847221, -0.2411417322834647770 ) ) ;
#11794 = CARTESIAN_POINT ( 'NONE',  ( -0.1958661417322836718, 0.3392501089628017219, -2.617454068241469756 ) ) ;
#11795 = CARTESIAN_POINT ( 'NONE',  ( 0.8727034120734913358, -0.08942795157527998196, 0.3641732283464567121 ) ) ;
#11796 = EDGE_LOOP ( 'NONE', ( #61593, #52239, #30726, #27108 ) ) ;
#11797 = CARTESIAN_POINT ( 'NONE',  ( -0.1058382717557497937, -0.3949938075777411628, -0.3871391076115485719 ) ) ;
#11798 = ORIENTED_EDGE ( 'NONE', *, *, #58932, .T. ) ;
#11799 = CARTESIAN_POINT ( 'NONE',  ( -0.1443569553805768291, -0.004921259842519576551, 0.3153832671262227771 ) ) ;
#11800 = CARTESIAN_POINT ( 'NONE',  ( 0.7677165354330716118, -0.5400638737290844871, 0.3530559997133364547 ) ) ;
#11801 = CARTESIAN_POINT ( 'NONE',  ( 0.4330708661417329575, -0.6692913385826771977, 8.415575281601705876E-17 ) ) ;
#11802 = CARTESIAN_POINT ( 'NONE',  ( -0.6692913385826764205, -0.6692913385826771977, 8.415575281601705876E-17 ) ) ;
#11803 = CARTESIAN_POINT ( 'NONE',  ( 0.1958661417322836718, -0.3392501089628017219, -1.663405142553492810 ) ) ;
#11804 = CARTESIAN_POINT ( 'NONE',  ( -1.377952755905511140, -0.6692913385826771977, 8.415575281601705876E-17 ) ) ;
#11805 = CARTESIAN_POINT ( 'NONE',  ( 0.1049643490035303689, 0.3917322834645670104, -2.755249343832020248 ) ) ;
#11806 = CARTESIAN_POINT ( 'NONE',  ( 1.345144356955381593, -0.2845877964562161244, -0.3641732283464567121 ) ) ;
#11807 = CARTESIAN_POINT ( 'NONE',  ( -1.522309711286088607, -0.6046776061558807314, 0.2411417322834647770 ) ) ;
#11808 = CARTESIAN_POINT ( 'NONE',  ( 0.9448818897637802916, -0.1870078740157480879, -0.4822834645669291653 ) ) ;
#11809 = CARTESIAN_POINT ( 'NONE',  ( 0.9908136482939640111, -0.6692913385826771977, 0.1292274648535927661 ) ) ;
#11810 = CARTESIAN_POINT ( 'NONE',  ( 4.893765752498283924E-17, -0.3996062992125986035, -1.023622047244094446 ) ) ;
#11811 = CARTESIAN_POINT ( 'NONE',  ( -1.371391076115484831, 0.2952755905511810774, -0.1292274648535930714 ) ) ;
#11812 = CARTESIAN_POINT ( 'NONE',  ( -0.3996062992125985480, -7.340648628747423112E-17, -0.2736220472440945017 ) ) ;
#11813 = CARTESIAN_POINT ( 'NONE',  ( -0.1968503937007867743, -0.6692913385826771977, 8.415575281601705876E-17 ) ) ;
#11814 = CARTESIAN_POINT ( 'NONE',  ( -0.2925321140481932924, 0.2925321140481931814, -2.224409448818897239 ) ) ;
#11815 = EDGE_CURVE ( 'NONE', #37563, #63010, #55945, .T. ) ;
#11816 =( BOUNDED_CURVE ( )  B_SPLINE_CURVE ( 2, ( #44683, #64912, #44277, #64073, #19882, #45105, #6410, #77550, #69566, #58160, #50596, #31664, #69967 ),
 .UNSPECIFIED., .F., .F. ) 
 B_SPLINE_CURVE_WITH_KNOTS ( ( 3, 2, 2, 2, 2, 2, 3 ),
 ( 0.1625000000000000056, 0.1666666666666666574, 0.1708333333333333370, 0.1749999999999999889, 0.1791666666666666685, 0.1833333333333333204, 0.1875000000000000000 ),
 .UNSPECIFIED. ) 
 CURVE ( )  GEOMETRIC_REPRESENTATION_ITEM ( )  RATIONAL_B_SPLINE_CURVE ( ( 1.000000000000000000, 0.9659258262890683122, 1.000000000000000000, 0.9659258262890683122, 1.000000000000000000, 0.9659258262890683122, 1.000000000000000000, 0.9659258262890683122, 1.000000000000000000, 0.9659258262890683122, 1.000000000000000000, 0.9659258262890683122, 1.000000000000000000 ) ) 
 REPRESENTATION_ITEM ( '' )  );
#11817 = CARTESIAN_POINT ( 'NONE',  ( 0.1958661417322836440, -0.3392501089628017219, -1.593832020997375531 ) ) ;
#11818 = VECTOR ( 'NONE', #21480, 39.37007874015748143 ) ;
#11819 = CARTESIAN_POINT ( 'NONE',  ( 1.299212598425197429, -0.6692913385826771977, 8.415575281601705876E-17 ) ) ;
#11820 = CARTESIAN_POINT ( 'NONE',  ( 0.09842519685039434474, 0.07958543189024085140, 0.2665933059059887866 ) ) ;
#11821 = CARTESIAN_POINT ( 'NONE',  ( 0.8070866141732288002, 0.1660481256975885056, 0.3530559997133364547 ) ) ;
#11822 = CARTESIAN_POINT ( 'NONE',  ( 0.4091458600556403535, 0.2362204724409449896, -1.152887139107611425 ) ) ;
#11823 = CARTESIAN_POINT ( 'NONE',  ( 0.8202099737532814183, -0.5511811023622048555, -0.09757992244046775898 ) ) ;
#11824 = CARTESIAN_POINT ( 'NONE',  ( 0.3740157480314966754, 0.1660481256975883668, -0.3530559997133364547 ) ) ;
#11825 = CARTESIAN_POINT ( 'NONE',  ( 0.3949938075777408852, 0.1058382717557500435, -1.146325459317585338 ) ) ;
#11826 = CARTESIAN_POINT ( 'NONE',  ( -0.6889763779527552368, -0.5400638737290845981, -0.3530559997133363437 ) ) ;
#11827 = CARTESIAN_POINT ( 'NONE',  ( -0.2099737532808391705, 0.2306618581243848609, 0.2411417322834645549 ) ) ;
#11828 = CARTESIAN_POINT ( 'NONE',  ( 1.115485564304462551, -0.004921259842519576551, 0.3153832671262227771 ) ) ;
#11829 = FACE_OUTER_BOUND ( 'NONE', #33927, .T. ) ;
#11830 = CARTESIAN_POINT ( 'NONE',  ( -0.2230971128608915943, -0.4281496062992127816, -0.4176697321401328100 ) ) ;
#11831 = CARTESIAN_POINT ( 'NONE',  ( 0.2493438320209980519, -0.004921259842519576551, 0.3153832671262227771 ) ) ;
#11832 = CARTESIAN_POINT ( 'NONE',  ( -2.856580783922622047, 1.081851677178485405, -0.1334749385307413549 ) ) ;
#11833 = CARTESIAN_POINT ( 'NONE',  ( -0.4790026246719154557, -0.3162353388693405765, 0.4822834645669290543 ) ) ;
#11834 = CARTESIAN_POINT ( 'NONE',  ( 0.5380577427821529035, -0.004921259842519870586, -0.3153832671262229437 ) ) ;
#11835 = CARTESIAN_POINT ( 'NONE',  ( -0.2925321140481932369, 0.2925321140481931259, -1.671259842519685179 ) ) ;
#11836 = CARTESIAN_POINT ( 'NONE',  ( 0.1509186351706045259, -0.05778040916215560624, -0.4822834645669293319 ) ) ;
#11837 = CARTESIAN_POINT ( 'NONE',  ( 1.384514435695538559, 0.1771653543307087075, -0.09757992244046823083 ) ) ;
#11838 = CARTESIAN_POINT ( 'NONE',  ( 0.4839371108951637801, 2.606013654608237919E-15, 0.3791475997938224540 ) ) ;
#11839 = CARTESIAN_POINT ( 'NONE',  ( -0.3608923884514428360, -0.5511811023622048555, -0.09757992244046775898 ) ) ;
#11840 = CARTESIAN_POINT ( 'NONE',  ( -0.5380577427821514602, -0.3690944881889765550, -0.3153832671262227771 ) ) ;
#11841 = CARTESIAN_POINT ( 'NONE',  ( -0.2230971128608915943, 0.05413385826771666132, 0.4176697321401328100 ) ) ;
#11842 = CARTESIAN_POINT ( 'NONE',  ( 0.1377952755905518800, -0.5400638737290844871, 0.3530559997133364547 ) ) ;
#11843 = CARTESIAN_POINT ( 'NONE',  ( 0.8792650918635177559, -0.004921259842519576551, 0.3153832671262227771 ) ) ;
#11844 = CARTESIAN_POINT ( 'NONE',  ( 0.3461855724062893880, 1.212665435597622965, -1.067367761115870728 ) ) ;
#11845 = CARTESIAN_POINT ( 'NONE',  ( -1.679790026246718693, 0.2306618581243847221, -0.2411417322834647770 ) ) ;
#11846 = CARTESIAN_POINT ( 'NONE',  ( 0.7480314960629927956, 0.2952755905511811885, 0.000000000000000000 ) ) ;
#11847 = CARTESIAN_POINT ( 'NONE',  ( 2.154527559055117170, 0.03937007874015747977, 0.4677827689124997024 ) ) ;
#11848 = CARTESIAN_POINT ( 'NONE',  ( -0.3149606299212590610, -0.1870078740157479769, 0.4822834645669291653 ) ) ;
#11849 = CARTESIAN_POINT ( 'NONE',  ( 0.1049643490035303689, 0.3917322834645670104, -1.022965879265091749 ) ) ;
#11850 = CARTESIAN_POINT ( 'NONE',  ( 0.8005249343832028242, -0.4281496062992127816, -0.4176697321401328100 ) ) ;
#11851 = CARTESIAN_POINT ( 'NONE',  ( 0.5643044619422579178, 0.05413385826771666132, 0.4176697321401328100 ) ) ;
#11852 = CARTESIAN_POINT ( 'NONE',  ( -0.4591627418635558788, 1.414127833138721035, -3.910145517416460770 ) ) ;
#11853 = CARTESIAN_POINT ( 'NONE',  ( 0.5643044619422579178, -0.004921259842519576551, 0.3153832671262227771 ) ) ;
#11854 = CARTESIAN_POINT ( 'NONE',  ( 0.9973753280839902091, -0.6046776061558807314, 0.2411417322834647770 ) ) ;
#11855 = CARTESIAN_POINT ( 'NONE',  ( 0.01968503937007930540, 0.07958543189024085140, 0.2665933059059887866 ) ) ;
#11856 = CARTESIAN_POINT ( 'NONE',  ( -0.3280839895013117347, 0.05413385826771626580, -0.4176697321401330321 ) ) ;
#11857 = DIRECTION ( 'NONE',  ( -0.000000000000000000, 0.000000000000000000, 1.000000000000000000 ) ) ;
#11858 = CARTESIAN_POINT ( 'NONE',  ( 0.4724409448818904789, -0.1870078740157479769, 0.4822834645669291653 ) ) ;
#11859 = CARTESIAN_POINT ( 'NONE',  ( -0.9580052493438311334, 0.05413385826771626580, -0.4176697321401330321 ) ) ;
#11860 = CARTESIAN_POINT ( 'NONE',  ( -0.4133858267716528645, 0.07958543189024071263, -0.2665933059059888421 ) ) ;
#11861 = CARTESIAN_POINT ( 'NONE',  ( 0.2755905511811031494, -0.6692913385826771977, 8.415575281601705876E-17 ) ) ;
#11862 = CARTESIAN_POINT ( 'NONE',  ( 0.8530183727034128527, -0.3690944881889763329, 0.3153832671262228327 ) ) ;
#11863 = CARTESIAN_POINT ( 'NONE',  ( -0.3871391076115476282, -0.05778040916215522460, 0.4822834645669289988 ) ) ;
#11864 = CARTESIAN_POINT ( 'NONE',  ( 0.4091458600556404646, -0.2362204724409448231, -0.5774278215223097588 ) ) ;
#11866 = CARTESIAN_POINT ( 'NONE',  ( 1.502624671916010790, -0.3162353388693409650, -0.4822834645669289433 ) ) ;
#11865 = CARTESIAN_POINT ( 'NONE',  ( -2.142213561789879428, 0.02617651024168221943, 0.4623158380715322036 ) ) ;
#11867 = LINE ( 'NONE', #17772, #46636 ) ;
#11868 = CARTESIAN_POINT ( 'NONE',  ( -0.2867679344610366554, 0.2867679344610365444, -2.216535433070866201 ) ) ;
#11869 = CIRCLE ( 'NONE', #50650, 0.3129921259842521897 ) ;
#11870 = CARTESIAN_POINT ( 'NONE',  ( -1.463254593175852492, 0.2952755905511811885, 0.1292274648535926551 ) ) ;
#11871 = CARTESIAN_POINT ( 'NONE',  ( -0.7480314960629914633, 0.2952755905511811885, 0.000000000000000000 ) ) ;
#11872 = CARTESIAN_POINT ( 'NONE',  ( 0.1265901696524989462, 0.4724409448818897572, -0.1509186351706036378 ) ) ;
#11873 = CARTESIAN_POINT ( 'NONE',  ( -0.3420746716998659953, -0.1974969037888706647, -2.887139107611548461 ) ) ;
#11874 = VERTEX_POINT ( 'NONE', #39341 ) ;
#11875 = CARTESIAN_POINT ( 'NONE',  ( 0.5183727034120741983, -0.5511811023622046335, 0.09757992244046803654 ) ) ;
#11876 = CARTESIAN_POINT ( 'NONE',  ( 0.3917322834645670104, 2.398668435337828261E-17, -1.212598425196850238 ) ) ;
#11877 = CARTESIAN_POINT ( 'NONE',  ( 0.8464566929133865436, 0.1660481256975883668, -0.3530559997133364547 ) ) ;
#11878 = CARTESIAN_POINT ( 'NONE',  ( 0.2362204724409449064, 0.4091458600556404646, -2.821522309711286258 ) ) ;
#11879 = CARTESIAN_POINT ( 'NONE',  ( -1.614173228346457378, 1.818966223839196372, 0.1372047244094476981 ) ) ;
#11880 = CARTESIAN_POINT ( 'NONE',  ( -0.2624671916010490880, -0.5023911411419708095, 0.1820866141732285504 ) ) ;
#11881 = CARTESIAN_POINT ( 'NONE',  ( -1.646981627296586703, -0.2845877964562161244, -0.3641732283464567121 ) ) ;
#11882 = CARTESIAN_POINT ( 'NONE',  ( 1.187664041994751285, -0.05778040916215522460, 0.4822834645669289988 ) ) ;
#11883 = CARTESIAN_POINT ( 'NONE',  ( 1.377952755905512472, -0.5511811023622047445, 6.969142054262312111E-17 ) ) ;
#11884 = CARTESIAN_POINT ( 'NONE',  ( 0.03280839895013198948, -0.6692913385826773087, -0.1292274648535924053 ) ) ;
#11885 = CARTESIAN_POINT ( 'NONE',  ( -0.3392501089628019439, 0.1958661417322832554, -0.7362011566591059042 ) ) ;
#11886 = CARTESIAN_POINT ( 'NONE',  ( -0.2230971128608915943, 0.05413385826771666132, 0.4176697321401328100 ) ) ;
#11887 = CARTESIAN_POINT ( 'NONE',  ( -1.502624671916009680, -0.08942795157528024563, -0.3641732283464568787 ) ) ;
#11888 = CARTESIAN_POINT ( 'NONE',  ( -0.3937007874015740483, -0.1870078740157480879, -0.4822834645669291653 ) ) ;
#11889 = DIRECTION ( 'NONE',  ( 0.000000000000000000, 0.000000000000000000, -1.000000000000000000 ) ) ;
#11890 = DIRECTION ( 'NONE',  ( -1.000000000000000000, 0.000000000000000000, 0.000000000000000000 ) ) ;
#11891 = ORIENTED_EDGE ( 'NONE', *, *, #3865, .T. ) ;
#11892 = CARTESIAN_POINT ( 'NONE',  ( -9.594673741351313045E-17, 0.3917322834645670659, -2.201462885335645048 ) ) ;
#11893 = CARTESIAN_POINT ( 'NONE',  ( 0.2952755905511819101, 0.1660481256975883668, -0.3530559997133364547 ) ) ;
#11894 = ORIENTED_EDGE ( 'NONE', *, *, #57231, .F. ) ;
#11895 = CARTESIAN_POINT ( 'NONE',  ( -0.3871391076115479057, -0.3162353388693409650, -0.4822834645669289433 ) ) ;
#11896 = CARTESIAN_POINT ( 'NONE',  ( -1.587926509186350810, 0.05413385826771626580, -0.4176697321401330321 ) ) ;
#11897 = CARTESIAN_POINT ( 'NONE',  ( 0.7414698162729663755, -0.6692913385826773087, -0.1292274648535924053 ) ) ;
#11898 = CARTESIAN_POINT ( 'NONE',  ( 0.1509186351706045259, -0.05778040916215560624, -0.4822834645669293319 ) ) ;
#11899 = CARTESIAN_POINT ( 'NONE',  ( 0.3392501089628018329, 0.1958661417322835607, -1.475721784776902856 ) ) ;
#11900 = CARTESIAN_POINT ( 'NONE',  ( -0.7545931758530177724, 0.2952755905511811885, 0.1292274648535926551 ) ) ;
#11901 = CARTESIAN_POINT ( 'NONE',  ( 0.3543307086614181922, -0.6692913385826771977, 8.415575281601705876E-17 ) ) ;
#11902 = CARTESIAN_POINT ( 'NONE',  ( -0.3346456692913377662, 0.1660481256975883668, -0.3530559997133364547 ) ) ;
#11903 = CARTESIAN_POINT ( 'NONE',  ( 0.3346456692913393205, -0.4536011799217368745, -0.2665933059059886201 ) ) ;
#11904 = CARTESIAN_POINT ( 'NONE',  ( -0.2896968578984297493, -0.05818598865049063457, 5.869712490931005888 ) ) ;
#11905 = CARTESIAN_POINT ( 'NONE',  ( -0.1509186351706028884, -0.05778040916215522460, 0.4822834645669289988 ) ) ;
#11906 = CYLINDRICAL_SURFACE ( 'NONE', #29173, 0.09842519685039351207 ) ;
#11907 = CARTESIAN_POINT ( 'NONE',  ( 1.515748031496063186, -0.5400638737290845981, -0.3530559997133363437 ) ) ;
#11908 = CARTESIAN_POINT ( 'NONE',  ( -0.1049643490035307020, 0.3917322834645669549, -2.833333333333333037 ) ) ;
#11909 = ORIENTED_EDGE ( 'NONE', *, *, #47802, .F. ) ;
#11910 = ORIENTED_EDGE ( 'NONE', *, *, #21817, .F. ) ;
#11911 = CARTESIAN_POINT ( 'NONE',  ( 0.5905511811023629321, 0.2952755905511811885, 0.000000000000000000 ) ) ;
#11912 = CARTESIAN_POINT ( 'NONE',  ( 0.06561679790026316017, -0.004921259842519870586, -0.3153832671262229437 ) ) ;
#11914 = PLANE ( 'NONE',  #58567 ) ;
#11913 = CARTESIAN_POINT ( 'NONE',  ( 1.272965879265092637, -0.3690944881889765550, -0.3153832671262227771 ) ) ;
#11915 = CARTESIAN_POINT ( 'NONE',  ( -0.1049643490035307020, 0.3917322834645669549, -1.351049868766404538 ) ) ;
#11916 = CARTESIAN_POINT ( 'NONE',  ( -0.2362204724409451284, 0.4091458600556402425, 0.06758530183727033680 ) ) ;
#11917 = SURFACE_STYLE_USAGE ( .BOTH. , #24527 ) ;
#11918 = CARTESIAN_POINT ( 'NONE',  ( 0.1058382717557499880, 0.3949938075777409408, 0.08727034120734906975 ) ) ;
#11919 = CARTESIAN_POINT ( 'NONE',  ( 0.3083989501312343062, -0.3162353388693405765, 0.4822834645669290543 ) ) ;
#11920 = CARTESIAN_POINT ( 'NONE',  ( -1.417322834645668772, -0.1870078740157480879, -0.4822834645669291653 ) ) ;
#11921 = CARTESIAN_POINT ( 'NONE',  ( -1.220472440944881054, 0.2952755905511811885, 0.000000000000000000 ) ) ;
#11922 = CARTESIAN_POINT ( 'NONE',  ( 0.2887139107611556010, -0.6046776061558807314, 0.2411417322834647770 ) ) ;
#11923 = CARTESIAN_POINT ( 'NONE',  ( 0.9842519685039375910, 0.2952755905511811885, 0.000000000000000000 ) ) ;
#11924 = CARTESIAN_POINT ( 'NONE',  ( 1.305774278215223960, -0.5511811023622046335, 0.09757992244046803654 ) ) ;
#11925 = CARTESIAN_POINT ( 'NONE',  ( 0.8070866141732289112, -0.4536011799217368745, -0.2665933059059886201 ) ) ;
#11926 = CARTESIAN_POINT ( 'NONE',  ( -0.6889763779527552368, 0.1660481256975885056, 0.3530559997133364547 ) ) ;
#11927 = CARTESIAN_POINT ( 'NONE',  ( 0.1070741851644053388, 0.3996062992125986035, -0.3851706036745406458 ) ) ;
#11928 = CARTESIAN_POINT ( 'NONE',  ( 1.489501312335958172, -0.3162353388693405765, 0.4822834645669290543 ) ) ;
#11929 = CARTESIAN_POINT ( 'NONE',  ( 0.3917322834645669549, 0.1049643490035304660, -0.1167979002624671692 ) ) ;
#11931 = PLANE ( 'NONE',  #56012 ) ;
#11930 = CARTESIAN_POINT ( 'NONE',  ( 1.161417322834646493, -0.5400638737290844871, 0.3530559997133364547 ) ) ;
#11932 = CARTESIAN_POINT ( 'NONE',  ( -1.627296587926508442, -0.5023911411419708095, -0.1820866141732282451 ) ) ;
#11933 = CARTESIAN_POINT ( 'NONE',  ( 0.1706036745406830368, -0.4281496062992127816, -0.4176697321401328100 ) ) ;
#11934 = CARTESIAN_POINT ( 'NONE',  ( 0.9251968503937015864, -0.4536011799217367080, 0.2665933059059888421 ) ) ;
#11935 = CARTESIAN_POINT ( 'NONE',  ( -1.673228346456691717, 0.07958543189024071263, -0.2665933059059888421 ) ) ;
#11936 = CARTESIAN_POINT ( 'NONE',  ( 0.8989501312335964611, 0.2952755905511811885, 0.1292274648535926551 ) ) ;
#11937 = CARTESIAN_POINT ( 'NONE',  ( -0.5052493438320202479, 0.2952755905511810219, -0.1292274648535930437 ) ) ;
#11938 = CARTESIAN_POINT ( 'NONE',  ( -0.4002624671916004129, -0.08942795157528024563, -0.3641732283464568787 ) ) ;
#11939 = CARTESIAN_POINT ( 'NONE',  ( -0.4002624671916004129, -0.05778040916215560624, -0.4822834645669293319 ) ) ;
#11940 = CARTESIAN_POINT ( 'NONE',  ( 1.489501312335958172, -0.3162353388693405765, 0.4822834645669290543 ) ) ;
#11941 = ADVANCED_FACE ( 'NONE', ( #2306 ), #30424, .F. ) ;
#11942 = CARTESIAN_POINT ( 'NONE',  ( -1.062992125984250968, 0.2952755905511811885, 0.000000000000000000 ) ) ;
#11943 = CARTESIAN_POINT ( 'NONE',  ( 1.194225721784777594, 0.05413385826771666132, 0.4176697321401328100 ) ) ;
#11944 = CARTESIAN_POINT ( 'NONE',  ( -0.2867679344610365444, -0.2867679344610367664, -0.8431951688002119472 ) ) ;
#11945 = CARTESIAN_POINT ( 'NONE',  ( -1.141732283464566011, 0.1771653543307087630, 0.000000000000000000 ) ) ;
#11946 = CARTESIAN_POINT ( 'NONE',  ( 0.2017716535433070613, 0.2017716535433070613, -0.3937007874015748254 ) ) ;
#11947 = CARTESIAN_POINT ( 'NONE',  ( 1.607611548556431069, 0.2952755905511811885, 0.1292274648535926551 ) ) ;
#11948 = CARTESIAN_POINT ( 'NONE',  ( -0.1265901696524993347, 0.4724409448818895907, -2.288057742782152015 ) ) ;
#11949 = CARTESIAN_POINT ( 'NONE',  ( -1.456692913385826182, -0.6692913385826771977, 8.415575281601705876E-17 ) ) ;
#11950 = CARTESIAN_POINT ( 'NONE',  ( -1.568241469816272105, -0.2845877964562161244, -0.3641732283464567121 ) ) ;
#11951 = CARTESIAN_POINT ( 'NONE',  ( -1.069553805774277722, 0.1771653543307087630, 0.09757992244046791164 ) ) ;
#11952 = CARTESIAN_POINT ( 'NONE',  ( 1.640419947506562393, -0.3690944881889763329, 0.3153832671262228327 ) ) ;
#11953 = CARTESIAN_POINT ( 'NONE',  ( -0.5052493438320203589, 0.2952755905511810774, -0.1292274648535930714 ) ) ;
#11954 = CARTESIAN_POINT ( 'NONE',  ( 0.1377952755905518800, 0.07958543189024071263, -0.2665933059059888421 ) ) ;
#11955 = CARTESIAN_POINT ( 'NONE',  ( -1.371391076115484831, 0.1771653543307087075, -0.09757992244046823083 ) ) ;
#11956 = CARTESIAN_POINT ( 'NONE',  ( 1.299212598425197429, 0.1771653543307087630, 0.000000000000000000 ) ) ;
#11957 = CARTESIAN_POINT ( 'NONE',  ( 0.9448818897637802916, -0.1870078740157480879, -0.4822834645669291653 ) ) ;
#11958 = CARTESIAN_POINT ( 'NONE',  ( 1.443569553805774897, 0.2306618581243848609, 0.2411417322834645549 ) ) ;
#11959 = CARTESIAN_POINT ( 'NONE',  ( 0.03937007874015833325, -0.5511811023622047445, 6.969142054262312111E-17 ) ) ;
#11960 = CARTESIAN_POINT ( 'NONE',  ( 0.5446194225721792126, -0.3162353388693405765, 0.4822834645669290543 ) ) ;
#11961 = CARTESIAN_POINT ( 'NONE',  ( 1.141732283464567566, 0.1771653543307087630, 0.000000000000000000 ) ) ;
#11962 = VERTEX_POINT ( 'NONE', #65028 ) ;
#11963 = CARTESIAN_POINT ( 'NONE',  ( 1.594488188976378673, 0.1660481256975885056, 0.3530559997133364547 ) ) ;
#11964 = EDGE_CURVE ( 'NONE', #48318, #67810, #7363, .T. ) ;
#11965 = CARTESIAN_POINT ( 'NONE',  ( -1.154855643044618851, 0.2306618581243848609, 0.2411417322834645549 ) ) ;
#11966 = CARTESIAN_POINT ( 'NONE',  ( -0.2952755905511804668, 0.1660481256975885056, 0.3530559997133364547 ) ) ;
#11967 = CARTESIAN_POINT ( 'NONE',  ( -0.1998031496062991907, -0.3460692066303959757, -0.5380577427821522374 ) ) ;
#11968 = CARTESIAN_POINT ( 'NONE',  ( -0.3996062992125986590, 0.1070741851644051723, -2.786745406824146620 ) ) ;
#11969 = CARTESIAN_POINT ( 'NONE',  ( 0.3149606299212603933, -0.1870078740157479769, 0.4822834645669291653 ) ) ;
#11970 = CARTESIAN_POINT ( 'NONE',  ( 1.036745406824147508, -0.3690944881889765550, -0.3153832671262227771 ) ) ;
#11971 = CARTESIAN_POINT ( 'NONE',  ( 0.1312335958005257930, 0.2306618581243847221, -0.2411417322834647770 ) ) ;
#11972 = CARTESIAN_POINT ( 'NONE',  ( 0.2230971128608929543, 0.05413385826771626580, -0.4176697321401330321 ) ) ;
#11973 = CARTESIAN_POINT ( 'NONE',  ( -0.3996062992125986035, -0.1070741851644056997, -2.093175853018372834 ) ) ;
#11974 = CARTESIAN_POINT ( 'NONE',  ( -0.2891555358219908833, -0.2891555358219912164, -1.476377952755905332 ) ) ;
#11975 = CARTESIAN_POINT ( 'NONE',  ( -0.2771898661223743954, 1.152090366371692154, 1.087348617264907169 ) ) ;
#11976 = CARTESIAN_POINT ( 'NONE',  ( -0.4724409448818898682, -8.678599364036362592E-17, -2.559055118110236560 ) ) ;
#11977 = CARTESIAN_POINT ( 'NONE',  ( 0.3917322834645670104, -0.1049643490035303273, -0.7335958005249343383 ) ) ;
#11978 = CARTESIAN_POINT ( 'NONE',  ( -0.3412073490813641308, -0.5023911411419708095, 0.1820866141732285504 ) ) ;
#11979 = CARTESIAN_POINT ( 'NONE',  ( -0.6167979002624665030, 0.05413385826771666132, 0.4176697321401328100 ) ) ;
#11980 = EDGE_CURVE ( 'NONE', #54857, #36796, #42578, .T. ) ;
#11981 = CARTESIAN_POINT ( 'NONE',  ( 0.1974969037888706092, -0.3420746716998660508, -2.530839895013123453 ) ) ;
#11982 = CARTESIAN_POINT ( 'NONE',  ( 0.9580052493438327987, -0.4281496062992127816, -0.4176697321401328100 ) ) ;
#11983 = CARTESIAN_POINT ( 'NONE',  ( -1.528871391076114250, -0.6692913385826771977, 0.1292274648535927661 ) ) ;
#11984 = CARTESIAN_POINT ( 'NONE',  ( 0.7939632545931766261, -0.05778040916215522460, 0.4822834645669289988 ) ) ;
#11985 = DIRECTION ( 'NONE',  ( 0.000000000000000000, 0.000000000000000000, 1.000000000000000000 ) ) ;
#11986 = CARTESIAN_POINT ( 'NONE',  ( 0.1070741851644053527, 0.3996062992125986590, -2.355643044619422533 ) ) ;
#11987 = CARTESIAN_POINT ( 'NONE',  ( 1.574803149606299746, -0.1870078740157480879, -0.4822834645669291653 ) ) ;
#11988 = CARTESIAN_POINT ( 'NONE',  ( 1.036745406824147508, -0.4281496062992127816, -0.4176697321401328100 ) ) ;
#11989 = CARTESIAN_POINT ( 'NONE',  ( 0.7808398950131240079, -0.3162353388693405765, 0.4822834645669290543 ) ) ;
#11990 = CARTESIAN_POINT ( 'NONE',  ( 0.9842519685039375910, 0.1771653543307087630, 0.000000000000000000 ) ) ;
#11991 = CARTESIAN_POINT ( 'NONE',  ( 1.253280839895013710, -0.05778040916215560624, -0.4822834645669293319 ) ) ;
#11992 = CARTESIAN_POINT ( 'NONE',  ( 0.3917322834645669549, 0.1049643490035304660, -0.2093175853018373611 ) ) ;
#11993 = DIRECTION ( 'NONE',  ( 0.000000000000000000, 1.000000000000000000, 0.000000000000000000 ) ) ;
#11994 = CARTESIAN_POINT ( 'NONE',  ( 0.8202099737532814183, -0.6692913385826773087, -0.1292274648535924053 ) ) ;
#11995 = CARTESIAN_POINT ( 'NONE',  ( 1.686351706036745890, 0.1771653543307087630, 0.09757992244046791164 ) ) ;
#11996 = CARTESIAN_POINT ( 'NONE',  ( -0.3280839895013117347, -0.4281496062992124485, 0.4176697321401328655 ) ) ;
#11997 = CARTESIAN_POINT ( 'NONE',  ( -0.9514435695538050464, -0.3162353388693405765, 0.4822834645669290543 ) ) ;
#11998 = CARTESIAN_POINT ( 'NONE',  ( 1.364829396325459854, -0.6046776061558809534, -0.2411417322834644161 ) ) ;
#11999 = CARTESIAN_POINT ( 'NONE',  ( 0.1049643490035303689, 0.3917322834645670104, -0.7080052493438320216 ) ) ;
#12000 = CARTESIAN_POINT ( 'NONE',  ( 0.1049643490035304938, -0.3917322834645669549, -1.652230971128608505 ) ) ;
#12001 = CARTESIAN_POINT ( 'NONE',  ( 0.1049643490035304938, -0.3917322834645669549, -2.597112860892388131 ) ) ;
#12002 = CARTESIAN_POINT ( 'NONE',  ( 1.443569553805774897, -0.6046776061558809534, -0.2411417322834644161 ) ) ;
#12003 = ORIENTED_EDGE ( 'NONE', *, *, #21276, .T. ) ;
#12004 = CARTESIAN_POINT ( 'NONE',  ( -0.3420746716998659953, -0.1974969037888706647, -2.729658792650918819 ) ) ;
#12005 = ORIENTED_EDGE ( 'NONE', *, *, #76979, .F. ) ;
#12006 = CARTESIAN_POINT ( 'NONE',  ( -2.154527559055123831, 0.03937007874015747977, 0.4677827689124697264 ) ) ;
#12007 = CARTESIAN_POINT ( 'NONE',  ( 1.410761154855643795, -0.2845877964562159024, 0.3641732283464567677 ) ) ;
#12008 = CARTESIAN_POINT ( 'NONE',  ( 0.3996062992125986035, 2.446882876249141962E-17, -1.535433070866141669 ) ) ;
#12009 = CARTESIAN_POINT ( 'NONE',  ( 1.391076115485564868, 0.1283753931104746893, -0.1820866141732285504 ) ) ;
#12010 = CARTESIAN_POINT ( 'NONE',  ( -0.7754685323813622633, -1.146068349578384814E-15, 0.3627985898453520153 ) ) ;
#12011 = DIRECTION ( 'NONE',  ( -1.000000000000000000, -3.083952846180989294E-16, 0.000000000000000000 ) ) ;
#12012 = DIRECTION ( 'NONE',  ( -0.000000000000000000, -1.000000000000000000, -8.673617379884024625E-16 ) ) ;
#12013 = CARTESIAN_POINT ( 'NONE',  ( -0.1958661417322834220, -0.3392501089628018884, -0.4652230971128609727 ) ) ;
#12014 = CARTESIAN_POINT ( 'NONE',  ( -0.7611548556430438595, -0.5023911411419708095, -0.1820866141732282451 ) ) ;
#12015 = CARTESIAN_POINT ( 'NONE',  ( -1.391076115485563758, 0.1283753931104748280, 0.1820866141732283561 ) ) ;
#12016 = CARTESIAN_POINT ( 'NONE',  ( -1.371391076115484609, -0.6692913385826771977, 0.1292274648535927661 ) ) ;
#12017 = CARTESIAN_POINT ( 'NONE',  ( 0.1049868766404206816, -0.6046776061558809534, -0.2411417322834644161 ) ) ;
#12018 = CARTESIAN_POINT ( 'NONE',  ( 1.502624671916010790, -0.3162353388693409650, -0.4822834645669289433 ) ) ;
#12019 = ORIENTED_EDGE ( 'NONE', *, *, #62545, .T. ) ;
#12020 = CARTESIAN_POINT ( 'NONE',  ( -1.620734908136482577, 0.2952755905511811885, 0.1292274648535926551 ) ) ;
#12021 = CARTESIAN_POINT ( 'NONE',  ( -1.607539944893438655, 0.2919301301068724097, 0.05787806847778405317 ) ) ;
#12022 = DIRECTION ( 'NONE',  ( 1.000000000000000000, 0.000000000000000000, 0.000000000000000000 ) ) ;
#12023 = CARTESIAN_POINT ( 'NONE',  ( 0.2362204724409449064, 0.4091458600556404646, -2.034120734908136718 ) ) ;
#12024 = CARTESIAN_POINT ( 'NONE',  ( 0.1938976377952755792, 0.1938976377952755792, -0.3740157480314971750 ) ) ;
#12025 = CARTESIAN_POINT ( 'NONE',  ( -0.5774278215223089816, -0.5023911411419708095, 0.1820866141732285504 ) ) ;
#12026 = CARTESIAN_POINT ( 'NONE',  ( -1.358267716535432434, -0.5400638737290844871, 0.3530559997133364547 ) ) ;
#12027 = CARTESIAN_POINT ( 'NONE',  ( 1.115485564304462551, -0.4281496062992127816, -0.4176697321401328100 ) ) ;
#12028 = ORIENTED_EDGE ( 'NONE', *, *, #43363, .T. ) ;
#12030 = DIRECTION ( 'NONE',  ( 0.000000000000000000, 0.000000000000000000, -1.000000000000000000 ) ) ;
#12029 = CARTESIAN_POINT ( 'NONE',  ( -0.4724409448818898682, -8.678599364036362592E-17, -2.478346456692913868 ) ) ;
#12031 = CARTESIAN_POINT ( 'NONE',  ( 1.174540682414699111, -0.3162353388693405765, 0.4822834645669290543 ) ) ;
#12032 = CARTESIAN_POINT ( 'NONE',  ( -1.102362204724408601, -0.1870078740157479769, 0.4822834645669291653 ) ) ;
#12033 = CARTESIAN_POINT ( 'NONE',  ( 0.3392501089628018329, -0.1958661417322834497, -0.3425003692575309677 ) ) ;
#12034 = CARTESIAN_POINT ( 'NONE',  ( -0.3871391076115479057, -0.2845877964562161244, -0.3641732283464567121 ) ) ;
#12035 = CARTESIAN_POINT ( 'NONE',  ( 0.1049643490035304799, -0.3917322834645669549, -0.9573490813648293241 ) ) ;
#12036 = CARTESIAN_POINT ( 'NONE',  ( -0.6627296587926501115, 0.1771653543307087075, -0.09757992244046823083 ) ) ;
#12037 = CARTESIAN_POINT ( 'NONE',  ( 0.6889763779527563470, 0.07958543189024071263, -0.2665933059059888421 ) ) ;
#12038 = CARTESIAN_POINT ( 'NONE',  ( 0.07874015748031558404, -0.1870078740157480879, -0.4822834645669291653 ) ) ;
#12039 = B_SPLINE_CURVE_WITH_KNOTS ( 'NONE', 3,
 ( #9529, #41100, #60037, #15439 ),
 .UNSPECIFIED., .F., .F.,
 ( 4, 4 ),
 ( 0.05078239113848836972, 0.05222574548756768464 ),
 .UNSPECIFIED. ) ;
#12040 = CARTESIAN_POINT ( 'NONE',  ( -0.6758530183727028406, 0.1771653543307087630, 0.09757992244046791164 ) ) ;
#12041 = CARTESIAN_POINT ( 'NONE',  ( 0.3392501089628018884, -0.1958661417322834220, -2.774278215223096922 ) ) ;
#12042 = CARTESIAN_POINT ( 'NONE',  ( 0.9580052493438326877, 0.05413385826771666132, 0.4176697321401328100 ) ) ;
#12043 = CARTESIAN_POINT ( 'NONE',  ( -0.8530183727034112984, 0.05413385826771666132, 0.4176697321401328100 ) ) ;
#12044 = CARTESIAN_POINT ( 'NONE',  ( 0.1265901696524990294, -0.4724409448818896462, -0.6345144356955381149 ) ) ;
#12045 = CARTESIAN_POINT ( 'NONE',  ( -0.3149606299212590610, -0.1870078740157479769, 0.4822834645669291653 ) ) ;
#12046 = CARTESIAN_POINT ( 'NONE',  ( -0.8398950131233585692, 0.2306618581243848609, 0.2411417322834645549 ) ) ;
#12047 = CARTESIAN_POINT ( 'NONE',  ( 1.148293963254593875, -0.5511811023622046335, 0.09757992244046803654 ) ) ;
#12048 = CARTESIAN_POINT ( 'NONE',  ( 0.3149606299212603933, -0.1870078740157479769, 0.3641732283464567677 ) ) ;
#12049 = CARTESIAN_POINT ( 'NONE',  ( -0.5774278215223089816, 0.2306618581243847221, -0.2411417322834647770 ) ) ;
#12050 = B_SPLINE_CURVE_WITH_KNOTS ( 'NONE', 3,
 ( #62486, #4820, #30498, #56161 ),
 .UNSPECIFIED., .F., .F.,
 ( 4, 4 ),
 ( 1.009931976291010463E-06, 0.001444423380196054128 ),
 .UNSPECIFIED. ) ;
#12051 = CARTESIAN_POINT ( 'NONE',  ( -1.220472440944881054, -0.6692913385826771977, 8.415575281601705876E-17 ) ) ;
#12052 = PLANE ( 'NONE',  #17062 ) ;
#12053 = CARTESIAN_POINT ( 'NONE',  ( 1.646981627296588035, -0.2845877964562159024, 0.3641732283464567677 ) ) ;
#12054 = CARTESIAN_POINT ( 'NONE',  ( -0.4068241469816264999, -0.4281496062992124485, 0.4176697321401328655 ) ) ;
#12055 = CARTESIAN_POINT ( 'NONE',  ( -1.056430446194224881, 0.2952755905511810774, -0.1292274648535930714 ) ) ;
#12056 = EDGE_LOOP ( 'NONE', ( #55436, #10363, #21935, #2965 ) ) ;
#12057 = CARTESIAN_POINT ( 'NONE',  ( -0.1070741851644056997, 0.3996062992125984925, -1.973097112860892510 ) ) ;
#12058 = CARTESIAN_POINT ( 'NONE',  ( 1.036745406824147508, -0.4281496062992127816, -0.4176697321401328100 ) ) ;
#12059 = CARTESIAN_POINT ( 'NONE',  ( -0.5249343832020990641, -0.5023911411419708095, -0.1820866141732282451 ) ) ;
#12060 = CARTESIAN_POINT ( 'NONE',  ( -0.8267716535433065062, -0.6692913385826771977, 8.415575281601705876E-17 ) ) ;
#12061 = CARTESIAN_POINT ( 'NONE',  ( 1.089238845144357759, 0.05413385826771626580, -0.4176697321401330321 ) ) ;
#12062 = CARTESIAN_POINT ( 'NONE',  ( 0.7152230971128616943, -0.05778040916215522460, 0.4822834645669289988 ) ) ;
#12063 = CARTESIAN_POINT ( 'NONE',  ( -0.3458507752293906723, -0.3458507752293910609, -0.05905511811023621271 ) ) ;
#12064 = CARTESIAN_POINT ( 'NONE',  ( -1.240157480314959759, 0.07958543189024085140, 0.2665933059059887866 ) ) ;
#12065 = CARTESIAN_POINT ( 'NONE',  ( -0.3996062992125985480, -7.340648628747423112E-17, -0.7460629921259841479 ) ) ;
#12066 = CARTESIAN_POINT ( 'NONE',  ( 0.3996062992125986035, 0.1070741851644054776, -0.9120734908136483021 ) ) ;
#12067 = CARTESIAN_POINT ( 'NONE',  ( 0.2891555358219910499, -0.2891555358219909944, -0.4133858267716535861 ) ) ;
#12068 = PRODUCT_DEFINITION ( 'UNKNOWN', '', #12785, #20945 ) ;
#12069 = CARTESIAN_POINT ( 'NONE',  ( 0.4741706889230142830, 1.520077057622761574, 2.554855216661410910 ) ) ;
#12070 = CARTESIAN_POINT ( 'NONE',  ( 1.017060367454068803, -0.2845877964562159024, 0.3641732283464567677 ) ) ;
#12071 = CARTESIAN_POINT ( 'NONE',  ( 0.6692913385826777528, 0.1771653543307087630, 0.000000000000000000 ) ) ;
#12072 = CARTESIAN_POINT ( 'NONE',  ( 0.6955380577427828781, 0.05413385826771626580, -0.4176697321401330321 ) ) ;
#12073 = DIRECTION ( 'NONE',  ( -3.491481338843132961E-15, -0.000000000000000000, 1.000000000000000000 ) ) ;
#12074 = CARTESIAN_POINT ( 'NONE',  ( -0.2891555358219911054, 0.2891555358219909388, -1.356299212598425230 ) ) ;
#12075 = CARTESIAN_POINT ( 'NONE',  ( 0.8661417322834653598, -0.1870078740157479769, 0.3641732283464567677 ) ) ;
#12076 = CARTESIAN_POINT ( 'NONE',  ( -0.1640419947506553400, -0.05778040916215560624, -0.4822834645669293319 ) ) ;
#12077 = CARTESIAN_POINT ( 'NONE',  ( -1.181102362204723644, -0.1870078740157479769, 0.4822834645669291653 ) ) ;
#12078 = CARTESIAN_POINT ( 'NONE',  ( 1.351706036745407680, 0.05413385826771666132, 0.4176697321401328100 ) ) ;
#12079 = CARTESIAN_POINT ( 'NONE',  ( 0.4091458600556403535, 0.2362204724409449896, -1.548556430446194287 ) ) ;
#12080 = CARTESIAN_POINT ( 'NONE',  ( -0.2925321140481930704, -0.2925321140481933480, -2.578740157480315265 ) ) ;
#12081 = CARTESIAN_POINT ( 'NONE',  ( -0.1902887139107604098, -0.5511811023622046335, 0.09757992244046803654 ) ) ;
#12082 = EDGE_CURVE ( 'NONE', #46955, #61268, #20535, .T. ) ;
#12083 = ORIENTED_EDGE ( 'NONE', *, *, #52130, .T. ) ;
#12084 = ORIENTED_EDGE ( 'NONE', *, *, #34230, .F. ) ;
#12085 = CARTESIAN_POINT ( 'NONE',  ( -1.003937007874015297, -0.5400638737290845981, -0.3530559997133363437 ) ) ;
#12086 = CARTESIAN_POINT ( 'NONE',  ( -0.4790026246719152336, -0.05778040916215560624, -0.4822834645669293319 ) ) ;
#12087 = CARTESIAN_POINT ( 'NONE',  ( -0.7152230971128602510, -0.3162353388693405765, 0.4822834645669290543 ) ) ;
#12088 = CARTESIAN_POINT ( 'NONE',  ( 0.3805774278215230400, -0.4281496062992124485, 0.4176697321401328655 ) ) ;
#12089 = EDGE_CURVE ( 'NONE', #62837, #21784, #71758, .T. ) ;
#12090 = CARTESIAN_POINT ( 'NONE',  ( -0.4855643044619415427, 0.05413385826771626580, -0.4176697321401330321 ) ) ;
#12091 = CARTESIAN_POINT ( 'NONE',  ( -1.279527559055116948, 0.1660481256975883668, -0.3530559997133364547 ) ) ;
#12092 = CARTESIAN_POINT ( 'NONE',  ( -1.023622047244094002, -0.1870078740157480879, -0.4822834645669291653 ) ) ;
#12093 = CARTESIAN_POINT ( 'NONE',  ( 0.8727034120734912248, -0.3162353388693409650, -0.4822834645669289433 ) ) ;
#12094 = CARTESIAN_POINT ( 'NONE',  ( -0.1049643490035302024, -0.3917322834645671215, -1.324146981627296826 ) ) ;
#12095 = CARTESIAN_POINT ( 'NONE',  ( -0.4527559055118102749, -0.4536011799217368745, -0.2665933059059886201 ) ) ;
#12096 = EDGE_LOOP ( 'NONE', ( #26023, #79408, #34061, #29889 ) ) ;
#12097 = CARTESIAN_POINT ( 'NONE',  ( -0.1974969037888706647, 0.3420746716998658843, -1.430446194225722056 ) ) ;
#12098 = EDGE_LOOP ( 'NONE', ( #48182, #39828, #41598, #2062 ) ) ;
#12099 = CARTESIAN_POINT ( 'NONE',  ( -1.174540682414697335, -0.2845877964562161244, -0.3641732283464567121 ) ) ;
#12100 = CARTESIAN_POINT ( 'NONE',  ( -1.076115485564303809, -0.6046776061558809534, -0.2411417322834644161 ) ) ;
#12101 = CARTESIAN_POINT ( 'NONE',  ( -1.043307086614172041, -0.5400638737290844871, 0.3530559997133364547 ) ) ;
#12102 = CARTESIAN_POINT ( 'NONE',  ( -0.2925321140481932924, 0.2925321140481931814, -0.1771653543307086520 ) ) ;
#12103 = CARTESIAN_POINT ( 'NONE',  ( -1.312335958005248715, -0.6046776061558809534, -0.2411417322834644161 ) ) ;
#12104 = CARTESIAN_POINT ( 'NONE',  ( -0.9514435695538050464, -0.3162353388693405765, 0.4822834645669290543 ) ) ;
#12105 = CARTESIAN_POINT ( 'NONE',  ( 0.3503937007874015075, 0.000000000000000000, 0.000000000000000000 ) ) ;
#12106 = CARTESIAN_POINT ( 'NONE',  ( -1.559171609364246924, 0.3937007874015748254, 0.4177787735906735578 ) ) ;
#12107 = CARTESIAN_POINT ( 'NONE',  ( 0.3871391076115493490, -0.2845877964562159024, 0.3641732283464567677 ) ) ;
#12108 = CYLINDRICAL_SURFACE ( 'NONE', #72, 0.3937007874015748254 ) ;
#12109 = CARTESIAN_POINT ( 'NONE',  ( -0.3917322834645670104, -7.196005306013484475E-17, 0.03346456692913377107 ) ) ;
#12110 = CARTESIAN_POINT ( 'NONE',  ( 0.05905511811023681640, 0.07958543189024071263, -0.2665933059059888421 ) ) ;
#12111 = CARTESIAN_POINT ( 'NONE',  ( -0.5314960629921250401, 0.1660481256975885056, 0.3530559997133364547 ) ) ;
#12112 = CARTESIAN_POINT ( 'NONE',  ( 1.227034120734908917, -0.6692913385826771977, 0.1292274648535927661 ) ) ;
#12113 = CARTESIAN_POINT ( 'NONE',  ( -0.4265091863517051496, -0.6692913385826771977, 0.1292274648535927661 ) ) ;
#12114 = ORIENTED_EDGE ( 'NONE', *, *, #1376, .F. ) ;
#12115 = CARTESIAN_POINT ( 'NONE',  ( 0.1070741851644053527, 0.3996062992125986590, -2.040682414698162361 ) ) ;
#12116 = CARTESIAN_POINT ( 'NONE',  ( -0.8537221893815262197, -2.294479370626195693E-15, 0.3464511005275217603 ) ) ;
#12117 = ORIENTED_EDGE ( 'NONE', *, *, #46853, .T. ) ;
#12118 = CARTESIAN_POINT ( 'NONE',  ( 0.2925321140481932369, -0.2925321140481931814, -1.592519685039370358 ) ) ;
#12119 = CARTESIAN_POINT ( 'NONE',  ( -0.3871391076115476282, -0.05778040916215522460, 0.4822834645669289988 ) ) ;
#12120 = CARTESIAN_POINT ( 'NONE',  ( 1.299212598425197429, 0.2952755905511811885, 0.000000000000000000 ) ) ;
#12121 = CARTESIAN_POINT ( 'NONE',  ( -1.023622047244094002, -0.1870078740157480601, -0.3641732283464567677 ) ) ;
#12122 = CARTESIAN_POINT ( 'NONE',  ( -1.410761154855642463, -0.05778040916215522460, 0.4822834645669289988 ) ) ;
#12123 = CARTESIAN_POINT ( 'NONE',  ( 0.3458507752293908943, -0.3458507752293908943, -0.7283464566929134243 ) ) ;
#12124 = EDGE_CURVE ( 'NONE', #55951, #34868, #81815, .T. ) ;
#12125 = CARTESIAN_POINT ( 'NONE',  ( -0.7137454485294948414, 2.165354330708661124, 0.4917280318828577412 ) ) ;
#12126 = CARTESIAN_POINT ( 'NONE',  ( 0.3392501089628018329, 0.1958661417322835607, 0.03412073490813653104 ) ) ;
#12127 = CARTESIAN_POINT ( 'NONE',  ( 1.272965879265092637, -0.4281496062992127816, -0.4176697321401328100 ) ) ;
#12128 = CARTESIAN_POINT ( 'NONE',  ( -0.1049643490035307020, 0.3917322834645669549, -2.138451443569553412 ) ) ;
#12129 = CARTESIAN_POINT ( 'NONE',  ( 0.09186351706036827158, 0.05413385826771666132, 0.4176697321401328100 ) ) ;
#12130 = CARTESIAN_POINT ( 'NONE',  ( -1.122047244094487306, 0.07958543189024071263, -0.2665933059059888421 ) ) ;
#12131 = CARTESIAN_POINT ( 'NONE',  ( -0.3149606299212590610, -0.1870078740157479769, 0.4822834645669291653 ) ) ;
#12132 = CARTESIAN_POINT ( 'NONE',  ( -0.4091458600556402980, -0.2362204724409451284, -2.648950131233595684 ) ) ;
#12133 = CARTESIAN_POINT ( 'NONE',  ( -0.8136482939632537770, -0.6046776061558807314, 0.2411417322834647770 ) ) ;
#12134 = ADVANCED_FACE ( 'NONE', ( #4773 ), #77544, .F. ) ;
#12135 = CARTESIAN_POINT ( 'NONE',  ( 0.3949938075777408852, 0.1058382717557500435, -2.091207349081364519 ) ) ;
#12136 = CARTESIAN_POINT ( 'NONE',  ( 0.7217847769028878924, -0.3690944881889765550, -0.3153832671262227771 ) ) ;
#12137 = CARTESIAN_POINT ( 'NONE',  ( -0.2493438320209966919, -0.004921259842519870586, -0.3153832671262229437 ) ) ;
#12138 = CARTESIAN_POINT ( 'NONE',  ( 0.8398950131233602345, -0.5023911411419708095, 0.1820866141732285504 ) ) ;
#12139 = CARTESIAN_POINT ( 'NONE',  ( -1.404199475065615932, 0.05413385826771666132, 0.4176697321401328100 ) ) ;
#12140 = CARTESIAN_POINT ( 'NONE',  ( 0.3458507752293908943, -0.3458507752293908943, -2.222440944881889813 ) ) ;
#12141 = CARTESIAN_POINT ( 'NONE',  ( 0.7414698162729663755, 0.1771653543307087630, 0.09757992244046791164 ) ) ;
#12142 = CARTESIAN_POINT ( 'NONE',  ( -0.8070866141732276899, 0.1660481256975883668, -0.3530559997133364547 ) ) ;
#12143 = ADVANCED_FACE ( 'NONE', ( #60780 ), #64067, .F. ) ;
#12144 = CARTESIAN_POINT ( 'NONE',  ( 1.141392835773559211, 0.3937007874015748254, 0.8264322058523028147 ) ) ;
#12145 = CARTESIAN_POINT ( 'NONE',  ( 0.04593175853018440641, -0.5511811023622046335, 0.09757992244046803654 ) ) ;
#12146 = CARTESIAN_POINT ( 'NONE',  ( -1.719160104986876103, -0.004921259842519576551, 0.3153832671262227771 ) ) ;
#12147 = CARTESIAN_POINT ( 'NONE',  ( 0.5643044619422579178, 0.05413385826771666132, 0.4176697321401328100 ) ) ;
#12148 = CARTESIAN_POINT ( 'NONE',  ( 0.2379288306351265703, 0.1751536117528152414, 0.1496817530000226493 ) ) ;
#12149 = CARTESIAN_POINT ( 'NONE',  ( 1.541994750656168645, -0.5511811023622046335, 0.09757992244046803654 ) ) ;
#12150 = AXIS2_PLACEMENT_3D ( 'NONE', #10185, #9351, #53945 ) ;
#12151 = CARTESIAN_POINT ( 'NONE',  ( -1.456692913385826182, -0.6692913385826771977, 8.415575281601705876E-17 ) ) ;
#12152 = CARTESIAN_POINT ( 'NONE',  ( -0.4330708661417315697, -0.5511811023622047445, 6.969142054262312111E-17 ) ) ;
#12153 = CARTESIAN_POINT ( 'NONE',  ( 0.4606732211678789546, 1.763126522798926343, 0.5309055118110234117 ) ) ;
#12154 = CARTESIAN_POINT ( 'NONE',  ( 0.1902887139107617975, 0.1771653543307087630, 0.09757992244046791164 ) ) ;
#12155 = CARTESIAN_POINT ( 'NONE',  ( -0.9580052493438311334, -0.4281496062992124485, 0.4176697321401328655 ) ) ;
#12156 = B_SPLINE_CURVE_WITH_KNOTS ( 'NONE', 3,
 ( #21634, #40578, #66259, #79315 ),
 .UNSPECIFIED., .F., .F.,
 ( 4, 4 ),
 ( 0.1818586053347995835, 0.1832800580269401680 ),
 .UNSPECIFIED. ) ;
#12157 = CARTESIAN_POINT ( 'NONE',  ( -0.6955380577427815458, 0.05413385826771666132, 0.4176697321401328100 ) ) ;
#12158 = CARTESIAN_POINT ( 'NONE',  ( 0.3996062992125985480, 2.446882876249141654E-17, -0.6673228346456693272 ) ) ;
#12159 = CARTESIAN_POINT ( 'NONE',  ( 0.1958661417322834775, 0.3392501089628018884, -2.118766404199475151 ) ) ;
#12160 = CARTESIAN_POINT ( 'NONE',  ( 0.5905511811023629321, -0.5511811023622047445, 6.969142054262312111E-17 ) ) ;
#12161 = CARTESIAN_POINT ( 'NONE',  ( -0.3346456692913377662, 0.1660481256975883668, -0.3530559997133364547 ) ) ;
#12162 = CARTESIAN_POINT ( 'NONE',  ( -0.6561679790026240244, 0.2306618581243847221, -0.2411417322834647770 ) ) ;
#12163 = CARTESIAN_POINT ( 'NONE',  ( -1.017060367454067249, -0.08942795157527998196, 0.3641732283464567121 ) ) ;
#12164 = CARTESIAN_POINT ( 'NONE',  ( 0.000000000000000000, -0.04921259842519688094, 0.08523872084492505052 ) ) ;
#12165 = CARTESIAN_POINT ( 'NONE',  ( -0.05249343832020911260, 0.2306618581243848609, 0.2411417322834645549 ) ) ;
#12166 = CARTESIAN_POINT ( 'NONE',  ( -1.410761154855642463, -0.08942795157527998196, 0.3641732283464567121 ) ) ;
#12167 = CARTESIAN_POINT ( 'NONE',  ( 1.154855643044620184, 0.2306618581243847221, -0.2411417322834647770 ) ) ;
#12168 = CARTESIAN_POINT ( 'NONE',  ( 3.224202737261815166, 2.716535433070866645, -0.5314960629921260393 ) ) ;
#12169 = CARTESIAN_POINT ( 'NONE',  ( -0.2867679344610367109, 0.2867679344610365444, -1.906187294784464026 ) ) ;
#12170 = ORIENTED_EDGE ( 'NONE', *, *, #66747, .F. ) ;
#12171 = CARTESIAN_POINT ( 'NONE',  ( 2.362204724409448620, 0.03937007874015751446, -0.5118110236220390075 ) ) ;
#12172 = CARTESIAN_POINT ( 'NONE',  ( -1.325459317585300889, -0.4281496062992127816, -0.4176697321401328100 ) ) ;
#12173 = CARTESIAN_POINT ( 'NONE',  ( -1.076115485564303809, 0.2306618581243848609, 0.2411417322834645549 ) ) ;
#12174 = CARTESIAN_POINT ( 'NONE',  ( 1.482939632545932307, 0.05413385826771626580, -0.4176697321401330321 ) ) ;
#12175 = CARTESIAN_POINT ( 'NONE',  ( -0.3917322834645669549, -0.1049643490035306603, -1.862860892388451761 ) ) ;
#12176 = PLANE ( 'NONE',  #20287 ) ;
#12177 = CARTESIAN_POINT ( 'NONE',  ( 0.8267716535433078384, -0.6692913385826771977, 8.415575281601705876E-17 ) ) ;
#12178 = CARTESIAN_POINT ( 'NONE',  ( 0.1312335958005257930, 0.2306618581243847221, -0.2411417322834647770 ) ) ;
#12179 = CARTESIAN_POINT ( 'NONE',  ( -0.4091458600556405756, 0.2362204724409446288, -0.4986876640419947715 ) ) ;
#12180 = CARTESIAN_POINT ( 'NONE',  ( 1.614173228346456712, 0.000000000000000000, -0.5309055118110239668 ) ) ;
#12181 = CARTESIAN_POINT ( 'NONE',  ( 1.095800524934383846, -0.2845877964562159024, 0.3641732283464567677 ) ) ;
#12182 = ADVANCED_FACE ( 'NONE', ( #48561 ), #7608, .F. ) ;
#12183 = CARTESIAN_POINT ( 'NONE',  ( -0.1070741851644056997, 0.3996062992125986035, -0.7939632545931758489 ) ) ;
#12184 = ORIENTED_EDGE ( 'NONE', *, *, #76206, .T. ) ;
#12185 = CARTESIAN_POINT ( 'NONE',  ( -9.594673741351313045E-17, 0.3917322834645670104, -2.511811023622047223 ) ) ;
#12186 = EDGE_LOOP ( 'NONE', ( #63043, #81650, #52429, #62629 ) ) ;
#12187 = CARTESIAN_POINT ( 'NONE',  ( 0.2034120734908142214, 0.2952755905511810774, -0.1292274648535930714 ) ) ;
#12188 = CARTESIAN_POINT ( 'NONE',  ( -0.8661417322834640276, -0.1870078740157480879, -0.4822834645669291653 ) ) ;
#12189 = CARTESIAN_POINT ( 'NONE',  ( -1.607611548556429737, 0.2952755905511810774, -0.1292274648535930714 ) ) ;
#12190 = CARTESIAN_POINT ( 'NONE',  ( 0.8136482939632553313, -0.6046776061558809534, -0.2411417322834644161 ) ) ;
#12191 = CARTESIAN_POINT ( 'NONE',  ( -1.548556430446193399, -0.5023911411419708095, -0.1820866141732282451 ) ) ;
#12192 = CARTESIAN_POINT ( 'NONE',  ( 1.240157480314961314, -0.5400638737290844871, 0.3530559997133364547 ) ) ;
#12193 = CARTESIAN_POINT ( 'NONE',  ( -0.1509186351706028884, -0.3162353388693409650, -0.4822834645669289433 ) ) ;
#12194 = CARTESIAN_POINT ( 'NONE',  ( -1.384514435695537005, -0.6692913385826773087, -0.1292274648535924053 ) ) ;
#12195 = CARTESIAN_POINT ( 'NONE',  ( -1.463254593175852492, 0.2952755905511811885, 0.1292274648535926551 ) ) ;
#12196 = B_SPLINE_CURVE_WITH_KNOTS ( 'NONE', 3,
 ( #39198, #21105, #27830, #28241 ),
 .UNSPECIFIED., .F., .F.,
 ( 4, 4 ),
 ( 0.07610408314619478143, 0.07753336624204336391 ),
 .UNSPECIFIED. ) ;
#12197 = CARTESIAN_POINT ( 'NONE',  ( 1.555118110236221041, 0.1660481256975883668, -0.3530559997133364547 ) ) ;
#12198 = CARTESIAN_POINT ( 'NONE',  ( 0.1049643490035303689, 0.3917322834645670104, -0.1430446194225721002 ) ) ;
#12199 = CARTESIAN_POINT ( 'NONE',  ( 0.9711286089238851948, -0.5023911411419708095, -0.1820866141732282451 ) ) ;
#12200 = VERTEX_POINT ( 'NONE', #23306 ) ;
#12201 = CARTESIAN_POINT ( 'NONE',  ( 0.1058382717557500713, -0.3949938075777409408, -0.4002624671916010235 ) ) ;
#12202 = VERTEX_POINT ( 'NONE', #48976 ) ;
#12203 = CARTESIAN_POINT ( 'NONE',  ( -0.1771653543307080136, -0.4536011799217367080, 0.2665933059059888421 ) ) ;
#12204 = CARTESIAN_POINT ( 'NONE',  ( 0.9285414500055709786, 1.724409448818897905, -0.6299212598425196763 ) ) ;
#12205 = CARTESIAN_POINT ( 'NONE',  ( 0.01312335958005323398, 0.05413385826771666132, 0.4176697321401328100 ) ) ;
#12206 = CARTESIAN_POINT ( 'NONE',  ( 0.6036745406824153282, -0.6046776061558807314, 0.2411417322834647770 ) ) ;
#12207 = CARTESIAN_POINT ( 'NONE',  ( -0.4396325459317579898, 0.2952755905511811885, 0.1292274648535926551 ) ) ;
#12208 = B_SPLINE_CURVE_WITH_KNOTS ( 'NONE', 3,
 ( #51869, #65371, #14447, #38836, #40098, #20322, #20745, #59037, #64515, #58184 ),
 .UNSPECIFIED., .F., .F.,
 ( 4, 2, 2, 2, 4 ),
 ( 0.000000000000000000, 0.0007778963758021331535, 0.001555792751604266307, 0.002333689127406399569, 0.003111585503208532614 ),
 .UNSPECIFIED. ) ;
#12209 = CARTESIAN_POINT ( 'NONE',  ( 0.3917322834645670104, 0.1049643490035304660, -1.853693856464253997 ) ) ;
#12210 = CARTESIAN_POINT ( 'NONE',  ( -1.417322834645668772, -0.1870078740157480879, -0.4822834645669291653 ) ) ;
#12211 = CARTESIAN_POINT ( 'NONE',  ( 0.2867679344610365999, 0.2867679344610365999, -2.584645669291338876 ) ) ;
#12212 = CARTESIAN_POINT ( 'NONE',  ( 1.240157480314961314, -0.4536011799217367080, 0.2665933059059888421 ) ) ;
#12213 = CARTESIAN_POINT ( 'NONE',  ( -1.581364829396324945, -0.05778040916215560624, -0.4822834645669293319 ) ) ;
#12214 = CARTESIAN_POINT ( 'NONE',  ( 0.7283464566929143125, 0.1660481256975885056, 0.3530559997133364547 ) ) ;
#12215 = CARTESIAN_POINT ( 'NONE',  ( 1.115485564304462551, -0.4281496062992127816, -0.4176697321401328100 ) ) ;
#12216 = AXIS2_PLACEMENT_3D ( 'NONE', #58794, #43044, #67922 ) ;
#12217 = CARTESIAN_POINT ( 'NONE',  ( -0.3996062992125986035, -7.340648628747425578E-17, -0.6692913385826770867 ) ) ;
#12218 = CARTESIAN_POINT ( 'NONE',  ( -1.246719160104986512, 0.05413385826771666132, 0.4176697321401328100 ) ) ;
#12219 = CARTESIAN_POINT ( 'NONE',  ( 0.3996062992125986035, -0.1070741851644052972, -0.5032808398950130435 ) ) ;
#12220 = CARTESIAN_POINT ( 'NONE',  ( -0.2925321140481932369, 0.2925321140481931259, -0.09645669291338584972 ) ) ;
#12221 = CARTESIAN_POINT ( 'NONE',  ( -0.2887139107611542133, 0.2306618581243848609, 0.2411417322834645549 ) ) ;
#12222 = CARTESIAN_POINT ( 'NONE',  ( -0.3996062992125986035, -7.340648628747425578E-17, -2.874015748031495843 ) ) ;
#12223 = CARTESIAN_POINT ( 'NONE',  ( -0.3917322834645669549, -0.1049643490035306603, -1.705380577427821898 ) ) ;
#12224 = CARTESIAN_POINT ( 'NONE',  ( 1.102362204724410155, -0.1870078740157479769, 0.4822834645669291653 ) ) ;
#12225 = CARTESIAN_POINT ( 'NONE',  ( 1.496062992125985147, -0.1870078740157479769, 0.4822834645669291653 ) ) ;
#12226 = CARTESIAN_POINT ( 'NONE',  ( 0.1246719160104994284, 0.1771653543307087075, -0.09757992244046823083 ) ) ;
#12227 = CARTESIAN_POINT ( 'NONE',  ( 0.7020997375328090762, -0.05778040916215560624, -0.4822834645669293319 ) ) ;
#12228 = CARTESIAN_POINT ( 'NONE',  ( -0.4724409448818895907, -0.1265901696524993070, -1.697506561679789971 ) ) ;
#12229 = CARTESIAN_POINT ( 'NONE',  ( 0.4068241469816281097, -0.004921259842519576551, 0.3153832671262227771 ) ) ;
#12230 = CARTESIAN_POINT ( 'NONE',  ( 0.3543307086614179147, 0.2952755905511811885, 0.000000000000000000 ) ) ;
#12231 = CARTESIAN_POINT ( 'NONE',  ( 0.3420746716998660508, -0.1974969037888704149, -0.8116797900262466836 ) ) ;
#12232 = CARTESIAN_POINT ( 'NONE',  ( -0.8267716535433065062, -0.6692913385826771977, 8.415575281601705876E-17 ) ) ;
#12233 = CARTESIAN_POINT ( 'NONE',  ( 0.7283464566929140904, -0.4536011799217368745, -0.2665933059059886201 ) ) ;
#12234 = VECTOR ( 'NONE', #9699, 39.37007874015748143 ) ;
#12235 = CARTESIAN_POINT ( 'NONE',  ( -2.620897244026447304, 1.710976477253048245, -0.4417575354491495299 ) ) ;
#12236 = CARTESIAN_POINT ( 'NONE',  ( -0.1968503937007867743, -0.6692913385826771977, 8.415575281601705876E-17 ) ) ;
#12237 = CARTESIAN_POINT ( 'NONE',  ( 0.2427821522309719648, -0.08942795157527998196, 0.3641732283464567121 ) ) ;
#12238 = CARTESIAN_POINT ( 'NONE',  ( -2.647175254740916639, 1.326002914239465147, -0.4256865378621351170 ) ) ;
#12239 = CARTESIAN_POINT ( 'NONE',  ( -0.2034120734908131112, -0.6692913385826773087, -0.1292274648535924053 ) ) ;
#12240 = CARTESIAN_POINT ( 'NONE',  ( 0.3215223097112867578, -0.08942795157527998196, 0.3641732283464567121 ) ) ;
#12241 = CARTESIAN_POINT ( 'NONE',  ( 0.1998031496062994128, -0.3460692066303957537, -1.900918635170603999 ) ) ;
#12242 = CARTESIAN_POINT ( 'NONE',  ( 0.3805774278215230400, -0.4281496062992124485, 0.4176697321401328655 ) ) ;
#12243 = CARTESIAN_POINT ( 'NONE',  ( 0.9711286089238851948, -0.5023911411419708095, -0.1820866141732282451 ) ) ;
#12244 = CARTESIAN_POINT ( 'NONE',  ( -0.1681795077207344780, 5.625543525484885637E-15, -0.4118477457932931962 ) ) ;
#12245 = CARTESIAN_POINT ( 'NONE',  ( -0.5183727034120726440, -0.5511811023622048555, -0.09757992244046775898 ) ) ;
#12246 = CARTESIAN_POINT ( 'NONE',  ( -0.5774278215223089816, 0.1283753931104746893, -0.1820866141732285504 ) ) ;
#12247 = CARTESIAN_POINT ( 'NONE',  ( -0.2952755905511803003, -0.5400638737290845981, -0.3530559997133363437 ) ) ;
#12248 = CARTESIAN_POINT ( 'NONE',  ( 5.463695987328526437E-16, -0.1870078740157479769, 0.4822834645669291653 ) ) ;
#12249 = CARTESIAN_POINT ( 'NONE',  ( 1.069553805774278832, 0.1771653543307087075, -0.09757992244046823083 ) ) ;
#12250 = CARTESIAN_POINT ( 'NONE',  ( -1.568241469816272105, -0.08942795157527998196, 0.3641732283464567121 ) ) ;
#12251 = CARTESIAN_POINT ( 'NONE',  ( 1.561679790026247350, -0.3690944881889763329, 0.3153832671262228327 ) ) ;
#12252 = CARTESIAN_POINT ( 'NONE',  ( 0.5643044619422579178, 0.05413385826771666132, 0.4176697321401328100 ) ) ;
#12253 = DIRECTION ( 'NONE',  ( 1.000000000000000000, 0.000000000000000000, 3.455050906509825972E-15 ) ) ;
#12254 = CARTESIAN_POINT ( 'NONE',  ( -0.1509186351706028884, -0.05778040916215522460, 0.4822834645669289988 ) ) ;
#12255 = CARTESIAN_POINT ( 'NONE',  ( -0.1958661417322834220, -0.3392501089628018884, -0.9376640419947508409 ) ) ;
#12256 = CARTESIAN_POINT ( 'NONE',  ( 1.062992125984252745, 0.2952755905511811885, 0.000000000000000000 ) ) ;
#12257 = CARTESIAN_POINT ( 'NONE',  ( 0.6102362204724416372, 0.1660481256975883668, -0.3530559997133364547 ) ) ;
#12258 = CARTESIAN_POINT ( 'NONE',  ( -1.600415083108464254, 2.375314266909943406, -0.1324231768467337145 ) ) ;
#12259 = CARTESIAN_POINT ( 'NONE',  ( 0.3018372703412079971, -0.004921259842519870586, -0.3153832671262229437 ) ) ;
#12260 = CARTESIAN_POINT ( 'NONE',  ( 1.240157480314961314, 0.1660481256975883668, -0.3530559997133364547 ) ) ;
#12261 = CARTESIAN_POINT ( 'NONE',  ( -0.1443569553805768291, -0.004921259842519576551, 0.3153832671262227771 ) ) ;
#12262 = CARTESIAN_POINT ( 'NONE',  ( -0.1246719160104980823, -0.6692913385826773087, -0.1292274648535924053 ) ) ;
#12263 = DIRECTION ( 'NONE',  ( 0.000000000000000000, 0.000000000000000000, 1.000000000000000000 ) ) ;
#12264 = CARTESIAN_POINT ( 'NONE',  ( 0.4068241469816279987, -0.4281496062992127816, -0.4176697321401328100 ) ) ;
#12265 = CARTESIAN_POINT ( 'NONE',  ( -0.8464566929133852113, 0.1660481256975885056, 0.3530559997133364547 ) ) ;
#12266 = CARTESIAN_POINT ( 'NONE',  ( -0.4986876640419942164, -0.5023911411419708095, 0.1820866141732285504 ) ) ;
#12267 = CARTESIAN_POINT ( 'NONE',  ( 0.3477690288713918276, 0.2952755905511811885, 0.1292274648535926551 ) ) ;
#12268 = CARTESIAN_POINT ( 'NONE',  ( -1.351706036745406347, 0.05413385826771626580, -0.4176697321401330321 ) ) ;
#12269 = CARTESIAN_POINT ( 'NONE',  ( -0.1706036745406816491, 0.05413385826771626580, -0.4176697321401330321 ) ) ;
#12270 =( LENGTH_UNIT ( ) NAMED_UNIT ( * ) SI_UNIT ( $, .METRE. ) );
#12272 = CARTESIAN_POINT ( 'NONE',  ( 1.305774278215223960, 0.2952755905511810774, -0.1292274648535930714 ) ) ;
#12271 = DIRECTION ( 'NONE',  ( 0.000000000000000000, -1.000000000000000000, 0.000000000000000000 ) ) ;
#12273 = CARTESIAN_POINT ( 'NONE',  ( 1.364829396325460076, 0.2306618581243848609, 0.2411417322834645549 ) ) ;
#12274 = CARTESIAN_POINT ( 'NONE',  ( -0.3392501089628019995, 0.1958661417322832277, -2.065616797900262647 ) ) ;
#12275 = CARTESIAN_POINT ( 'NONE',  ( -1.594488188976377119, 0.1660481256975883668, -0.3530559997133364547 ) ) ;
#12276 = B_SPLINE_CURVE_WITH_KNOTS ( 'NONE', 3,
 ( #64905, #14827, #27430, #51413, #59007, #33754, #20293, #40487, #1362, #27014, #52676, #78383, #20714, #14417, #40070, #65757, #59416, #53091, #78803, #6404, #32074, #97, #2187, #34171, #81999, #2606, #30637, #27855, #28264, #41317, #79223, #8505, #28683, #79638, #53515, #62209, #81591, #34591, #30217, #24313, #47614, #73734, #17612, #49983, #55880, #62627, #4971, #21956 ),
 .UNSPECIFIED., .F., .F.,
 ( 4, 2, 2, 1, 2, 2, 2, 2, 2, 2, 2, 2, 2, 2, 2, 2, 2, 2, 2, 2, 2, 1, 2, 2, 4 ),
 ( 0.03770802486988159008, 0.04006421406960428144, 0.04124230866946564100, 0.04242040326932700056, 0.04359849786918835318, 0.04477659246904971274, 0.04713278166877243880, 0.04831087626863381224, 0.04948897086849517180, 0.05184516006821790479, 0.05302325466807927823, 0.05420134926794065167, 0.05655753846766339854, 0.05891372766738613848, 0.06009182226724750497, 0.06126991686710887841, 0.06362610606683162529, 0.06480420066669299872, 0.06598229526655435828, 0.06833848446627711903, 0.06951657906613849247, 0.07069467366599987979, 0.07187276826586125322, 0.07305086286572262666, 0.07540705206544537353 ),
 .UNSPECIFIED. ) ;
#12277 = CARTESIAN_POINT ( 'NONE',  ( -0.7611548556430438595, 0.2306618581243848609, 0.2411417322834645549 ) ) ;
#12278 = CARTESIAN_POINT ( 'NONE',  ( -0.3458507752293906723, -0.3458507752293910609, -0.2165354330708661734 ) ) ;
#12279 = ADVANCED_FACE ( 'NONE', ( #81819 ), #15777, .F. ) ;
#12280 = CARTESIAN_POINT ( 'NONE',  ( -9.674558042662121740E-17, 0.3949938075777409963, -2.677165354330708347 ) ) ;
#12281 = ORIENTED_EDGE ( 'NONE', *, *, #17250, .T. ) ;
#12282 = CARTESIAN_POINT ( 'NONE',  ( -0.2952755905511803003, -0.4536011799217368745, -0.2665933059059886201 ) ) ;
#12283 = CARTESIAN_POINT ( 'NONE',  ( 0.1958661417322836440, -0.3392501089628017219, -1.501312335958005173 ) ) ;
#12284 = CARTESIAN_POINT ( 'NONE',  ( 0.6299212598425204535, -0.1870078740157479769, 0.4822834645669291653 ) ) ;
#12285 = CARTESIAN_POINT ( 'NONE',  ( 0.009287274676459343278, 0.3937527723457945328, -2.755905511811026276 ) ) ;
#12286 = DIRECTION ( 'NONE',  ( 0.000000000000000000, 0.000000000000000000, -1.000000000000000000 ) ) ;
#12287 = CARTESIAN_POINT ( 'NONE',  ( -0.6364829396325453192, -0.08942795157528024563, -0.3641732283464568787 ) ) ;
#12288 = VECTOR ( 'NONE', #50504, 39.37007874015748143 ) ;
#12289 = CARTESIAN_POINT ( 'NONE',  ( 1.023622047244095334, -0.1870078740157479769, 0.4822834645669291653 ) ) ;
#12290 = CARTESIAN_POINT ( 'NONE',  ( 0.9383202099737536495, -0.2845877964562159024, 0.3641732283464567677 ) ) ;
#12291 = CARTESIAN_POINT ( 'NONE',  ( 0.1968503937007881344, -0.6692913385826771977, 8.415575281601705876E-17 ) ) ;
#12292 = CARTESIAN_POINT ( 'NONE',  ( -0.3392501089628018329, -0.1958661417322836440, -0.9199281907798407820 ) ) ;
#12293 = CARTESIAN_POINT ( 'NONE',  ( -0.4068241469816264999, -0.4281496062992124485, 0.4176697321401328655 ) ) ;
#12294 = CARTESIAN_POINT ( 'NONE',  ( -1.456692913385826182, -0.5511811023622047445, 6.969142054262312111E-17 ) ) ;
#12295 = CARTESIAN_POINT ( 'NONE',  ( -0.5971128608923877978, 0.2952755905511811885, 0.1292274648535926551 ) ) ;
#12296 = CARTESIAN_POINT ( 'NONE',  ( 1.653543307086614789, -0.1870078740157479769, 0.4822834645669291653 ) ) ;
#12297 = PLANE ( 'NONE',  #48961 ) ;
#12298 = ORIENTED_EDGE ( 'NONE', *, *, #52130, .F. ) ;
#12299 = CARTESIAN_POINT ( 'NONE',  ( -0.2867679344610365444, -0.2867679344610367664, -1.945557373524620992 ) ) ;
#12300 = CARTESIAN_POINT ( 'NONE',  ( 0.5577427821522316087, -0.05778040916215522460, 0.4822834645669289988 ) ) ;
#12301 = ORIENTED_EDGE ( 'NONE', *, *, #22171, .T. ) ;
#12302 = CARTESIAN_POINT ( 'NONE',  ( -0.9055118110236215490, 0.2952755905511811885, 0.000000000000000000 ) ) ;
#12303 = CARTESIAN_POINT ( 'NONE',  ( -1.463254593175852492, 0.2952755905511811885, 0.1292274648535926551 ) ) ;
#12304 = CARTESIAN_POINT ( 'NONE',  ( 0.8398950131233602345, 0.2306618581243847221, -0.2411417322834647770 ) ) ;
#12305 = CARTESIAN_POINT ( 'NONE',  ( 0.2559055118110243332, 0.1660481256975885056, 0.3530559997133364547 ) ) ;
#12306 = CARTESIAN_POINT ( 'NONE',  ( 0.3917322834645670104, -0.1049643490035303411, -1.298556430446194510 ) ) ;
#12307 = CARTESIAN_POINT ( 'NONE',  ( -0.7677165354330699465, 0.1660481256975885056, 0.3530559997133364547 ) ) ;
#12308 = CARTESIAN_POINT ( 'NONE',  ( -0.2952755905511803003, -0.5400638737290845981, -0.3530559997133363437 ) ) ;
#12309 = CARTESIAN_POINT ( 'NONE',  ( -1.017060367454067249, -0.05778040916215522460, 0.4822834645669289988 ) ) ;
#12310 = CARTESIAN_POINT ( 'NONE',  ( -0.1902887139107604098, 0.1771653543307087075, -0.09757992244046823083 ) ) ;
#12311 = CARTESIAN_POINT ( 'NONE',  ( -5.237264738830231135E-17, 0.3992723400743281581, -1.920830620545185538E-17 ) ) ;
#12312 = CARTESIAN_POINT ( 'NONE',  ( -0.05905511811023545637, -0.5400638737290845981, -0.3530559997133363437 ) ) ;
#12313 = FACE_OUTER_BOUND ( 'NONE', #81380, .T. ) ;
#12314 = CARTESIAN_POINT ( 'NONE',  ( 1.299212598425197429, 0.2952755905511811885, 0.000000000000000000 ) ) ;
#12315 = CARTESIAN_POINT ( 'NONE',  ( 0.3917322834645670104, -0.1049643490035303411, -2.623359580052493367 ) ) ;
#12316 = ORIENTED_EDGE ( 'NONE', *, *, #31050, .T. ) ;
#12317 = ORIENTED_EDGE ( 'NONE', *, *, #69731, .T. ) ;
#12318 = CARTESIAN_POINT ( 'NONE',  ( 0.1771653543307093182, -0.5400638737290845981, -0.3530559997133363437 ) ) ;
#12319 = CARTESIAN_POINT ( 'NONE',  ( -0.08530183727034056085, -0.08942795157528024563, -0.3641732283464568787 ) ) ;
#12321 = CARTESIAN_POINT ( 'NONE',  ( -1.646051170424378096, 0.000000000000000000, 0.3464511005275205946 ) ) ;
#12320 = CARTESIAN_POINT ( 'NONE',  ( 1.502624671916010790, -0.08942795157527998196, 0.3641732283464567121 ) ) ;
#12322 = CARTESIAN_POINT ( 'NONE',  ( 0.2867679344610365999, 0.2867679344610365999, -1.009842519685039353 ) ) ;
#12323 = CARTESIAN_POINT ( 'NONE',  ( -0.9548908091195642545, -2.567464376874931580E-15, -0.4445507791589072832 ) ) ;
#12324 = CARTESIAN_POINT ( 'NONE',  ( 0.7210809602247731931, 4.888820689338890882E-16, 0.3464511005275202615 ) ) ;
#12325 = CARTESIAN_POINT ( 'NONE',  ( -1.548556430446193399, -0.6046776061558809534, -0.2411417322834644161 ) ) ;
#12326 = CARTESIAN_POINT ( 'NONE',  ( -0.2925321140481932369, 0.2925321140481931259, -2.773622047244094002 ) ) ;
#12327 = CARTESIAN_POINT ( 'NONE',  ( 0.3477690288713918276, 0.2952755905511811885, 0.1292274648535926551 ) ) ;
#12328 = CARTESIAN_POINT ( 'NONE',  ( -1.325459317585300889, 0.05413385826771666132, 0.4176697321401328100 ) ) ;
#12329 = CARTESIAN_POINT ( 'NONE',  ( -1.174540682414697335, -0.3162353388693409650, -0.4822834645669289433 ) ) ;
#12330 = CARTESIAN_POINT ( 'NONE',  ( 0.05249343832021075018, 0.2306618581243847221, -0.2411417322834647770 ) ) ;
#12331 = VECTOR ( 'NONE', #19551, 39.37007874015748143 ) ;
#12332 = CARTESIAN_POINT ( 'NONE',  ( 0.9645669291338588858, 0.1660481256975885056, 0.3530559997133364547 ) ) ;
#12333 = CARTESIAN_POINT ( 'NONE',  ( 1.423884514435696413, -0.2845877964562161244, -0.3641732283464567121 ) ) ;
#12334 = CONTEXT_DEPENDENT_SHAPE_REPRESENTATION ( #21290, #33896 ) ;
#12335 = CARTESIAN_POINT ( 'NONE',  ( 0.8923884514435703741, 0.1283753931104748280, 0.1820866141732283561 ) ) ;
#12336 = CARTESIAN_POINT ( 'NONE',  ( -0.8923884514435688198, -0.6046776061558807314, 0.2411417322834647770 ) ) ;
#12337 = CARTESIAN_POINT ( 'NONE',  ( 0.3460692066303958092, 0.1998031496062993018, -0.6804461942257218343 ) ) ;
#12338 = CARTESIAN_POINT ( 'NONE',  ( 1.653543307086614789, -0.1870078740157479769, 0.4822834645669291653 ) ) ;
#12339 = CARTESIAN_POINT ( 'NONE',  ( 0.1958661417322836440, -0.3392501089628017219, -0.2414698162729658204 ) ) ;
#12341 = DIRECTION ( 'NONE',  ( 0.000000000000000000, 0.000000000000000000, 1.000000000000000000 ) ) ;
#12340 = CARTESIAN_POINT ( 'NONE',  ( 0.8005249343832028242, -0.4281496062992127816, -0.4176697321401328100 ) ) ;
#12342 = CARTESIAN_POINT ( 'NONE',  ( -1.732283464566928277, -0.1870078740157479769, 0.3641732283464567677 ) ) ;
#12343 = CARTESIAN_POINT ( 'NONE',  ( -0.05249343832020911260, 0.2306618581243848609, 0.2411417322834645549 ) ) ;
#12344 = CARTESIAN_POINT ( 'NONE',  ( 1.017060367454068581, -0.08942795157528024563, -0.3641732283464568787 ) ) ;
#12345 = CARTESIAN_POINT ( 'NONE',  ( -1.561679790026246017, -0.004921259842519576551, 0.3153832671262227771 ) ) ;
#12346 = CARTESIAN_POINT ( 'NONE',  ( 0.8267716535433078384, -0.6692913385826771977, 8.415575281601705876E-17 ) ) ;
#12347 = CARTESIAN_POINT ( 'NONE',  ( 1.614173228346456712, 2.401574803149606474, -0.1372047244094476703 ) ) ;
#12348 = CARTESIAN_POINT ( 'NONE',  ( -0.3477690288713905509, -0.5511811023622046335, 0.09757992244046803654 ) ) ;
#12349 = CARTESIAN_POINT ( 'NONE',  ( -0.5446194225721777693, -0.3162353388693409650, -0.4822834645669289433 ) ) ;
#12350 = CARTESIAN_POINT ( 'NONE',  ( -1.561679790026246017, -0.3690944881889765550, -0.3153832671262227771 ) ) ;
#12351 = CARTESIAN_POINT ( 'NONE',  ( -1.345144356955379816, -0.05778040916215560624, -0.4822834645669293319 ) ) ;
#12352 = CARTESIAN_POINT ( 'NONE',  ( 1.240157480314961314, 0.1660481256975883668, -0.3530559997133364547 ) ) ;
#12353 = CARTESIAN_POINT ( 'NONE',  ( 0.3917322834645670104, 0.1049643490035304660, -0.7513316517398445082 ) ) ;
#12354 = CARTESIAN_POINT ( 'NONE',  ( -1.417322834645668772, -0.1870078740157480601, -0.3641732283464567677 ) ) ;
#12355 = CARTESIAN_POINT ( 'NONE',  ( 2.563288228875796992, 1.597527518877483343, 0.4706608522957233531 ) ) ;
#12356 = CARTESIAN_POINT ( 'NONE',  ( 0.8267716535433077274, 0.2952755905511811885, 0.000000000000000000 ) ) ;
#12357 = CARTESIAN_POINT ( 'NONE',  ( -0.4091458600556402980, -0.2362204724409451284, -2.333989501312335957 ) ) ;
#12358 = CARTESIAN_POINT ( 'NONE',  ( -1.607611548556429737, -0.6692913385826771977, 0.1292274648535927661 ) ) ;
#12359 = CARTESIAN_POINT ( 'NONE',  ( -1.410761154855641575, -0.2845877964562161244, -0.3641732283464567121 ) ) ;
#12360 = CARTESIAN_POINT ( 'NONE',  ( -0.8333333333333323711, -0.5511811023622048555, -0.09757992244046775898 ) ) ;
#12361 = CARTESIAN_POINT ( 'NONE',  ( 1.673228346456693494, 0.07958543189024085140, 0.2665933059059887866 ) ) ;
#12362 = CARTESIAN_POINT ( 'NONE',  ( -0.3149606299212590610, -0.1870078740157480879, -0.4822834645669291653 ) ) ;
#12363 = CARTESIAN_POINT ( 'NONE',  ( -0.1640419947506553400, -0.08942795157528024563, -0.3641732283464568787 ) ) ;
#12364 = CARTESIAN_POINT ( 'NONE',  ( -1.712598425196849572, 0.07958543189024085140, 0.2665933059059887866 ) ) ;
#12365 = CARTESIAN_POINT ( 'NONE',  ( 1.135170603674541256, 0.1771653543307087630, 0.09757992244046791164 ) ) ;
#12366 = CARTESIAN_POINT ( 'NONE',  ( 1.135170603674541256, -0.6692913385826773087, -0.1292274648535924053 ) ) ;
#12367 = CARTESIAN_POINT ( 'NONE',  ( 1.476377952755906220, 0.1660481256975883668, -0.3530559997133364547 ) ) ;
#12368 = CARTESIAN_POINT ( 'NONE',  ( 0.1640419947506569498, -0.2845877964562161244, -0.3641732283464567121 ) ) ;
#12369 = CARTESIAN_POINT ( 'NONE',  ( 0.4790026246719168435, -0.3162353388693409650, -0.4822834645669289433 ) ) ;
#12370 = CARTESIAN_POINT ( 'NONE',  ( 0.3871391076115492380, -0.08942795157528024563, -0.3641732283464568787 ) ) ;
#12371 = CARTESIAN_POINT ( 'NONE',  ( -1.640419947506561060, 0.05413385826771666132, 0.4176697321401328100 ) ) ;
#12372 = ADVANCED_FACE ( 'NONE', ( #28796 ), #80173, .F. ) ;
#12373 = CARTESIAN_POINT ( 'NONE',  ( -1.220472440944881054, -0.6692913385826771977, 8.415575281601705876E-17 ) ) ;
#12374 = CARTESIAN_POINT ( 'NONE',  ( -0.3346456692913377662, -0.5400638737290844871, 0.3530559997133364547 ) ) ;
#12375 = CARTESIAN_POINT ( 'NONE',  ( 0.1070741851644054915, -0.3996062992125985480, -0.4002624671916010235 ) ) ;
#12376 = CARTESIAN_POINT ( 'NONE',  ( -9.787531504996566615E-17, 0.3996062992125985480, -2.438976377952756014 ) ) ;
#12377 = CARTESIAN_POINT ( 'NONE',  ( 0.3018372703412079971, -0.4281496062992124485, 0.4176697321401328655 ) ) ;
#12378 = CARTESIAN_POINT ( 'NONE',  ( 0.9908136482939640111, 0.1771653543307087075, -0.09757992244046823083 ) ) ;
#12379 = CARTESIAN_POINT ( 'NONE',  ( -0.4068241469816264999, -0.4281496062992124485, 0.4176697321401328655 ) ) ;
#12380 = CARTESIAN_POINT ( 'NONE',  ( 0.2690288713910767848, -0.6692913385826773087, -0.1292274648535924053 ) ) ;
#12381 = CARTESIAN_POINT ( 'NONE',  ( 0.3996062992125986035, 2.446882876249141962E-17, -2.322834645669291209 ) ) ;
#12382 = CARTESIAN_POINT ( 'NONE',  ( -0.3420746716998661618, 0.1974969037888702206, -1.443569553805774230 ) ) ;
#12383 = CARTESIAN_POINT ( 'NONE',  ( -0.2925321140481930704, -0.2925321140481933480, -2.736220472440944018 ) ) ;
#12384 = DIRECTION ( 'NONE',  ( 0.000000000000000000, 0.000000000000000000, 1.000000000000000000 ) ) ;
#12385 = CARTESIAN_POINT ( 'NONE',  ( 0.3392501089628018884, -0.1958661417322834220, -0.7270341207349080292 ) ) ;
#12386 = CARTESIAN_POINT ( 'NONE',  ( -0.6889763779527552368, -0.4536011799217368745, -0.2665933059059886201 ) ) ;
#12387 = CARTESIAN_POINT ( 'NONE',  ( -1.003937007874015297, -0.5400638737290845981, -0.3530559997133363437 ) ) ;
#12388 = AXIS2_PLACEMENT_3D ( 'NONE', #56152, #10321, #49430 ) ;
#12389 = CARTESIAN_POINT ( 'NONE',  ( -0.3420746716998660508, -0.1974969037888706924, -2.491469816272965598 ) ) ;
#12390 = CARTESIAN_POINT ( 'NONE',  ( 0.6561679790026253567, -0.6046776061558809534, -0.2411417322834644161 ) ) ;
#12391 = CARTESIAN_POINT ( 'NONE',  ( 1.220472440944882386, -0.6692913385826771977, 8.415575281601705876E-17 ) ) ;
#12392 = CARTESIAN_POINT ( 'NONE',  ( 0.9645669291338588858, 0.1660481256975885056, 0.3530559997133364547 ) ) ;
#12393 = CARTESIAN_POINT ( 'NONE',  ( 0.2362204724409449064, 0.4091458600556404646, -2.821522309711286258 ) ) ;
#12394 = CARTESIAN_POINT ( 'NONE',  ( 0.2925321140481932369, -0.2925321140481932369, -2.145669291338581974 ) ) ;
#12395 = CARTESIAN_POINT ( 'NONE',  ( 1.601049868766404982, -0.6046776061558809534, -0.2411417322834644161 ) ) ;
#12396 = CARTESIAN_POINT ( 'NONE',  ( 0.9776902887139113929, 0.2952755905511811885, 0.1292274648535926551 ) ) ;
#12397 = CARTESIAN_POINT ( 'NONE',  ( 0.7480314960629927956, -0.6692913385826771977, 8.415575281601705876E-17 ) ) ;
#12398 = CARTESIAN_POINT ( 'NONE',  ( 0.7086614173228352742, -0.1870078740157480601, -0.3641732283464567677 ) ) ;
#12399 = CARTESIAN_POINT ( 'NONE',  ( 1.122047244094488860, -0.5400638737290845981, -0.3530559997133363437 ) ) ;
#12400 = CARTESIAN_POINT ( 'NONE',  ( 0.3392501089628018329, 0.1958661417322835607, -0.2158792650918636147 ) ) ;
#12401 = CARTESIAN_POINT ( 'NONE',  ( 0.5183727034120741983, 0.2952755905511810774, -0.1292274648535930714 ) ) ;
#12402 = CARTESIAN_POINT ( 'NONE',  ( 1.135170603674541256, -0.6692913385826773087, -0.1292274648535924053 ) ) ;
#12403 = CARTESIAN_POINT ( 'NONE',  ( 0.4068241469816281097, 0.05413385826771666132, 0.4176697321401328100 ) ) ;
#12404 = CARTESIAN_POINT ( 'NONE',  ( 1.410761154855643795, -0.08942795157528024563, -0.3641732283464568787 ) ) ;
#12405 = CARTESIAN_POINT ( 'NONE',  ( -0.8005249343832013809, -0.4281496062992124485, 0.4176697321401328655 ) ) ;
#12406 = CARTESIAN_POINT ( 'NONE',  ( -1.187664041994750175, -0.05778040916215560624, -0.4822834645669293319 ) ) ;
#12407 = CARTESIAN_POINT ( 'NONE',  ( 1.246719160104987623, -0.4281496062992124485, 0.4176697321401328655 ) ) ;
#12408 = CARTESIAN_POINT ( 'NONE',  ( 0.1958661417322834775, 0.3392501089628018884, -0.3864829396325459854 ) ) ;
#12409 = CARTESIAN_POINT ( 'NONE',  ( 0.3917322834645669549, 0.1049643490035304660, -1.534120734908136052 ) ) ;
#12410 = CARTESIAN_POINT ( 'NONE',  ( -9.594673741351313045E-17, 0.3917322834645670104, -2.511811023622047223 ) ) ;
#12411 = EDGE_LOOP ( 'NONE', ( #77639, #27414 ) ) ;
#12412 = CARTESIAN_POINT ( 'NONE',  ( -0.3460692066303960868, 0.1998031496062990242, -0.1837270341207349333 ) ) ;
#12413 = ORIENTED_EDGE ( 'NONE', *, *, #12082, .F. ) ;
#12414 = CARTESIAN_POINT ( 'NONE',  ( 1.614173228346457378, -0.6692913385826771977, 8.415575281601705876E-17 ) ) ;
#12415 = CARTESIAN_POINT ( 'NONE',  ( 1.541994750656168645, -0.5511811023622046335, 0.09757992244046803654 ) ) ;
#12416 = CARTESIAN_POINT ( 'NONE',  ( 0.3460692066303959202, 0.1998031496062993295, -1.391076115485564424 ) ) ;
#12417 = CARTESIAN_POINT ( 'NONE',  ( 1.404199475065617708, -0.004921259842519870586, -0.3153832671262229437 ) ) ;
#12418 = DIRECTION ( 'NONE',  ( -0.000000000000000000, -1.000000000000000000, -0.000000000000000000 ) ) ;
#12419 = CONICAL_SURFACE ( 'NONE', #22562, 1.220472440944881942, 0.7853981633974621568 ) ;
#12420 = DIRECTION ( 'NONE',  ( 0.000000000000000000, 0.000000000000000000, -1.000000000000000000 ) ) ;
#12421 = CARTESIAN_POINT ( 'NONE',  ( -0.1887375355206090954, 1.924695534443318090, 0.2501427588384230183 ) ) ;
#12422 = CARTESIAN_POINT ( 'NONE',  ( -0.2867679344610365999, 0.2867679344610364889, -0.8917322834645667884 ) ) ;
#12423 = CARTESIAN_POINT ( 'NONE',  ( -0.9448818897637790704, -0.1870078740157480601, -0.3641732283464567677 ) ) ;
#12424 = CARTESIAN_POINT ( 'NONE',  ( -1.679790026246718693, 0.1283753931104746893, -0.1820866141732285504 ) ) ;
#12425 = CARTESIAN_POINT ( 'NONE',  ( -1.358267716535432434, -0.5400638737290844871, 0.3530559997133364547 ) ) ;
#12426 = CARTESIAN_POINT ( 'NONE',  ( 0.07217847769028949700, -0.05778040916215560624, -0.4822834645669293319 ) ) ;
#12427 = CARTESIAN_POINT ( 'NONE',  ( 1.338582677165355062, -0.1870078740157480879, -0.4822834645669291653 ) ) ;
#12428 = ORIENTED_EDGE ( 'NONE', *, *, #64537, .F. ) ;
#12429 = CARTESIAN_POINT ( 'NONE',  ( -1.168682819302786058, -2.294479370626195693E-15, 0.3464511005275217603 ) ) ;
#12430 = CARTESIAN_POINT ( 'NONE',  ( 0.2362204724409451007, -0.4091458600556402980, -1.981627296587926690 ) ) ;
#12431 = CARTESIAN_POINT ( 'NONE',  ( 0.4177787735906999811, 1.312623414240995157, -1.714017618091133288 ) ) ;
#12432 = CARTESIAN_POINT ( 'NONE',  ( -0.6036745406824141069, -0.5023911411419708095, -0.1820866141732282451 ) ) ;
#12433 = CARTESIAN_POINT ( 'NONE',  ( -0.9973753280839886548, 0.2306618581243848609, 0.2411417322834645549 ) ) ;
#12434 = CARTESIAN_POINT ( 'NONE',  ( 0.9973753280839902091, -0.6046776061558807314, 0.2411417322834647770 ) ) ;
#12435 = ORIENTED_EDGE ( 'NONE', *, *, #63766, .F. ) ;
#12437 = CARTESIAN_POINT ( 'NONE',  ( -1.604771003085130543, 0.7690346235818137366, 0.1466069496707740338 ) ) ;
#12436 = CARTESIAN_POINT ( 'NONE',  ( -3.264097702071373064, 2.755905511811024056, -0.5314960629921260393 ) ) ;
#12438 = CARTESIAN_POINT ( 'NONE',  ( 1.259842519685040019, -0.1870078740157480879, -0.4822834645669291653 ) ) ;
#12439 = CARTESIAN_POINT ( 'NONE',  ( -1.253280839895012377, -0.05778040916215522460, 0.4822834645669289988 ) ) ;
#12440 = CARTESIAN_POINT ( 'NONE',  ( 0.3392501089628018329, 0.1958661417322835052, -0.2112667734570061184 ) ) ;
#12441 = VECTOR ( 'NONE', #62049, 39.37007874015749564 ) ;
#12442 = CARTESIAN_POINT ( 'NONE',  ( -0.4855643044619415427, -0.3690944881889763329, 0.3153832671262228327 ) ) ;
#12443 = CARTESIAN_POINT ( 'NONE',  ( -0.2867679344610364334, -0.2867679344610367109, -0.7736220472440945573 ) ) ;
#12444 = CARTESIAN_POINT ( 'NONE',  ( -0.5971128608923877978, -0.5511811023622048555, -0.09757992244046775898 ) ) ;
#12445 = CARTESIAN_POINT ( 'NONE',  ( 0.4461942257217855201, -0.5023911411419708095, 0.1820866141732285504 ) ) ;
#12446 = CARTESIAN_POINT ( 'NONE',  ( 0.2362204724409456558, -0.1870078740157480879, -0.4822834645669291653 ) ) ;
#12447 = CARTESIAN_POINT ( 'NONE',  ( -0.8136482939632537770, 0.1283753931104746893, -0.1820866141732285504 ) ) ;
#12448 = CARTESIAN_POINT ( 'NONE',  ( -0.2867679344610365999, 0.2867679344610364889, -2.846456692913385655 ) ) ;
#12449 = CARTESIAN_POINT ( 'NONE',  ( 0.9514435695538062676, -0.05778040916215522460, 0.4822834645669289988 ) ) ;
#12450 = CARTESIAN_POINT ( 'NONE',  ( -1.325459317585300889, 0.05413385826771666132, 0.4176697321401328100 ) ) ;
#12451 = CARTESIAN_POINT ( 'NONE',  ( 0.4091458600556403535, 0.2362204724409449896, -0.9954068241469815614 ) ) ;
#12452 = CARTESIAN_POINT ( 'NONE',  ( -0.2755905511811018171, 0.2952755905511811885, 0.000000000000000000 ) ) ;
#12453 = CARTESIAN_POINT ( 'NONE',  ( -0.7414698162729651543, -0.6692913385826771977, 0.1292274648535927661 ) ) ;
#12454 = CARTESIAN_POINT ( 'NONE',  ( 1.423884514435696413, -0.2845877964562161244, -0.3641732283464567121 ) ) ;
#12455 = CARTESIAN_POINT ( 'NONE',  ( -0.1574803149606292529, -0.1870078740157479769, 0.3641732283464567677 ) ) ;
#12456 = CARTESIAN_POINT ( 'NONE',  ( -0.7939632545931754048, -0.3162353388693405765, 0.4822834645669290543 ) ) ;
#12457 = CARTESIAN_POINT ( 'NONE',  ( -1.076115485564303809, -0.6046776061558809534, -0.2411417322834644161 ) ) ;
#12458 = CARTESIAN_POINT ( 'NONE',  ( 0.000000000000000000, 2.755905511811024056, 0.000000000000000000 ) ) ;
#12459 = CARTESIAN_POINT ( 'NONE',  ( 1.364829396325460076, 0.1283753931104748280, 0.1820866141732283561 ) ) ;
#12460 = CARTESIAN_POINT ( 'NONE',  ( -0.3018372703412066094, -0.4281496062992127816, -0.4176697321401328100 ) ) ;
#12461 = CARTESIAN_POINT ( 'NONE',  ( -1.023622047244094002, -0.1870078740157480879, -0.4822834645669291653 ) ) ;
#12462 = ORIENTED_EDGE ( 'NONE', *, *, #47715, .T. ) ;
#12463 = CARTESIAN_POINT ( 'NONE',  ( -0.1070741851644056997, 0.3996062992125984925, -2.288057742782152015 ) ) ;
#12464 = CARTESIAN_POINT ( 'NONE',  ( -0.6824146981627288167, 0.1283753931104748280, 0.1820866141732283561 ) ) ;
#12465 = CARTESIAN_POINT ( 'NONE',  ( 1.194225721784777594, -0.4281496062992127816, -0.4176697321401328100 ) ) ;
#12466 = CARTESIAN_POINT ( 'NONE',  ( -0.8792650918635160906, -0.004921259842519870586, -0.3153832671262229437 ) ) ;
#12467 = CARTESIAN_POINT ( 'NONE',  ( 4.893765752498283308E-17, -0.3996062992125985480, -1.257874015748031482 ) ) ;
#12468 = CARTESIAN_POINT ( 'NONE',  ( -0.9514435695538050464, -0.3162353388693405765, 0.4822834645669290543 ) ) ;
#12469 = CARTESIAN_POINT ( 'NONE',  ( 1.049868766404200349, 0.2306618581243848609, 0.2411417322834645549 ) ) ;
#12470 = CARTESIAN_POINT ( 'NONE',  ( 0.9842519685039378130, -0.6692913385826771977, 8.415575281601705876E-17 ) ) ;
#12471 = CARTESIAN_POINT ( 'NONE',  ( -0.5120078740157480990, 6.270288040516270789E-17, -1.512162153811850596 ) ) ;
#12472 = CARTESIAN_POINT ( 'NONE',  ( -1.397637795275589623, 0.07958543189024085140, 0.2665933059059887866 ) ) ;
#12473 = CARTESIAN_POINT ( 'NONE',  ( 0.2925321140481931814, -0.2925321140481931259, -0.8051181102362204856 ) ) ;
#12474 = CARTESIAN_POINT ( 'NONE',  ( 0.2925321140481932369, 0.2925321140481932369, -0.9251968503937008093 ) ) ;
#12475 = CARTESIAN_POINT ( 'NONE',  ( 0.1974969037888706369, -0.3420746716998659953, -0.09186351706036749443 ) ) ;
#12476 = CARTESIAN_POINT ( 'NONE',  ( 0.4606233198248834704, 1.422786159591913568, 2.585446969423548680 ) ) ;
#12477 = CARTESIAN_POINT ( 'NONE',  ( 1.253280839895013710, -0.08942795157528024563, -0.3641732283464568787 ) ) ;
#12478 = CARTESIAN_POINT ( 'NONE',  ( 0.6824146981627303710, 0.1283753931104746893, -0.1820866141732285504 ) ) ;
#12479 = CARTESIAN_POINT ( 'NONE',  ( 0.6561679790026253567, 0.2306618581243848609, 0.2411417322834645549 ) ) ;
#12480 = CARTESIAN_POINT ( 'NONE',  ( 1.607611548556431069, 0.2952755905511811885, 0.1292274648535926551 ) ) ;
#12481 = CARTESIAN_POINT ( 'NONE',  ( 0.3949938075777408852, 0.1058382717557500435, -1.303805774278215424 ) ) ;
#12482 = CARTESIAN_POINT ( 'NONE',  ( 0.6627296587926517768, -0.5511811023622048555, -0.09757992244046775898 ) ) ;
#12483 = CARTESIAN_POINT ( 'NONE',  ( -0.4724409448818890911, -0.1870078740157480879, -0.4822834645669291653 ) ) ;
#12484 = CARTESIAN_POINT ( 'NONE',  ( -1.030183727034119867, -0.3162353388693405765, 0.4822834645669290543 ) ) ;
#12485 = CARTESIAN_POINT ( 'NONE',  ( 0.8267716535433078384, -0.6692913385826771977, 8.415575281601705876E-17 ) ) ;
#12486 = CARTESIAN_POINT ( 'NONE',  ( -0.4091458600556402980, -0.2362204724409451284, -1.627296587926509330 ) ) ;
#12487 = CARTESIAN_POINT ( 'NONE',  ( -0.2925321140481932369, 0.2925321140481931814, -2.539370078740157410 ) ) ;
#12488 = ORIENTED_EDGE ( 'NONE', *, *, #73660, .F. ) ;
#12489 = ORIENTED_EDGE ( 'NONE', *, *, #53092, .T. ) ;
#12490 = VECTOR ( 'NONE', #60809, 39.37007874015748143 ) ;
#12491 = CARTESIAN_POINT ( 'NONE',  ( -1.207349081364828880, 0.2306618581243847221, -0.2411417322834647770 ) ) ;
#12492 = CARTESIAN_POINT ( 'NONE',  ( -0.7020997375328074108, -0.05778040916215522460, 0.4822834645669289988 ) ) ;
#12494 = CARTESIAN_POINT ( 'NONE',  ( -0.8858267716535425107, -0.5400638737290844871, 0.3530559997133364547 ) ) ;
#12493 = CARTESIAN_POINT ( 'NONE',  ( -0.8136482939632537770, 0.1283753931104746893, -0.1820866141732285504 ) ) ;
#12495 = CARTESIAN_POINT ( 'NONE',  ( 0.3917322834645668994, 0.1049643490035304522, -2.094468873194538450 ) ) ;
#12496 = CARTESIAN_POINT ( 'NONE',  ( 0.5314960629921267055, -0.5400638737290844871, 0.3530559997133364547 ) ) ;
#12497 = CARTESIAN_POINT ( 'NONE',  ( -0.3674540682414689785, 0.2306618581243848609, 0.2411417322834645549 ) ) ;
#12498 = CARTESIAN_POINT ( 'NONE',  ( 1.587926509186352142, 0.05413385826771666132, 0.4176697321401328100 ) ) ;
#12499 = CARTESIAN_POINT ( 'NONE',  ( -0.8136482939632537770, -0.6046776061558807314, 0.2411417322834647770 ) ) ;
#12500 = CARTESIAN_POINT ( 'NONE',  ( 0.3608923884514443348, 0.2952755905511810774, -0.1292274648535930714 ) ) ;
#12501 = ADVANCED_FACE ( 'NONE', ( #23720 ), #74259, .T. ) ;
#12502 = EDGE_CURVE ( 'NONE', #21089, #39954, #48151, .T. ) ;
#12503 = CARTESIAN_POINT ( 'NONE',  ( 0.2867679344610365999, -0.2867679344610365444, -1.350393700787401619 ) ) ;
#12504 = CARTESIAN_POINT ( 'NONE',  ( -0.9842519685039360366, 0.1771653543307087630, 0.000000000000000000 ) ) ;
#12505 = EDGE_LOOP ( 'NONE', ( #52785, #23977, #23496, #42750 ) ) ;
#12506 = CARTESIAN_POINT ( 'NONE',  ( -0.1974969037888703871, -0.3420746716998661063, -1.955380577427821454 ) ) ;
#12507 = EDGE_LOOP ( 'NONE', ( #80146, #43724, #23079, #52852 ) ) ;
#12508 = CARTESIAN_POINT ( 'NONE',  ( -1.135170603674539924, -0.5511811023622046335, 0.09757992244046803654 ) ) ;
#12509 = CARTESIAN_POINT ( 'NONE',  ( -1.122047244094487306, 0.1660481256975883668, -0.3530559997133364547 ) ) ;
#12510 = CARTESIAN_POINT ( 'NONE',  ( -0.7545931758530176614, -0.6692913385826773087, -0.1292274648535924053 ) ) ;
#12511 = CARTESIAN_POINT ( 'NONE',  ( 0.1070741851644054915, -0.3996062992125986035, -0.2427821522309711322 ) ) ;
#12512 = CARTESIAN_POINT ( 'NONE',  ( -1.036745406824146176, 0.05413385826771626580, -0.4176697321401330321 ) ) ;
#12513 = CARTESIAN_POINT ( 'NONE',  ( -1.227034120734907585, 0.2952755905511811885, 0.1292274648535926551 ) ) ;
#12514 = CARTESIAN_POINT ( 'NONE',  ( -1.568241469816272105, -0.3162353388693409650, -0.4822834645669289433 ) ) ;
#12515 = CARTESIAN_POINT ( 'NONE',  ( 0.4744094488189065095, 1.537401574803149984, -2.554262525012259477 ) ) ;
#12516 = CARTESIAN_POINT ( 'NONE',  ( 0.6955380577427828781, -0.3690944881889763329, 0.3153832671262228327 ) ) ;
#12517 = CARTESIAN_POINT ( 'NONE',  ( 0.000000000000000000, 0.04488074079120789317, -1.244489337948954555 ) ) ;
#12518 = CARTESIAN_POINT ( 'NONE',  ( -0.3917322834645669549, -0.1049643490035306603, 0.1843832020997374643 ) ) ;
#12519 = CARTESIAN_POINT ( 'NONE',  ( -0.4658792650918627265, -0.08942795157527998196, 0.3641732283464567121 ) ) ;
#12520 = CARTESIAN_POINT ( 'NONE',  ( -0.1837270341207340729, 0.2306618581243847221, -0.2411417322834647770 ) ) ;
#12521 = CARTESIAN_POINT ( 'NONE',  ( 1.509186351706037543, -0.4281496062992127816, -0.4176697321401328100 ) ) ;
#12522 = CARTESIAN_POINT ( 'NONE',  ( -0.4986876640419939388, 0.2306618581243847221, -0.2411417322834647770 ) ) ;
#12523 = ORIENTED_EDGE ( 'NONE', *, *, #60460, .F. ) ;
#12524 = ORIENTED_EDGE ( 'NONE', *, *, #24992, .F. ) ;
#12525 = CARTESIAN_POINT ( 'NONE',  ( -0.2925321140481930149, -0.2925321140481933480, -2.025590551181101873 ) ) ;
#12526 = CARTESIAN_POINT ( 'NONE',  ( -0.4724409448818890911, -0.1870078740157480879, -0.4822834645669291653 ) ) ;
#12527 = CARTESIAN_POINT ( 'NONE',  ( 1.456692913385827515, 0.2952755905511811885, 0.000000000000000000 ) ) ;
#12528 = CARTESIAN_POINT ( 'NONE',  ( -1.108923884514435132, -0.2845877964562159024, 0.3641732283464567677 ) ) ;
#12529 = CARTESIAN_POINT ( 'NONE',  ( -1.312335958005248715, -0.6046776061558809534, -0.2411417322834644161 ) ) ;
#12530 = CARTESIAN_POINT ( 'NONE',  ( 0.4091458600556403535, 0.2362204724409449896, -0.9186351706036745002 ) ) ;
#12531 = CARTESIAN_POINT ( 'NONE',  ( 2.169555354231010202, 1.520093187801265344, 0.4741711390158128703 ) ) ;
#12532 = EDGE_CURVE ( 'NONE', #12831, #11346, #16600, .T. ) ;
#12533 = CARTESIAN_POINT ( 'NONE',  ( 0.2867679344610365999, -0.2867679344610365444, -0.09055118110236216877 ) ) ;
#12534 = CARTESIAN_POINT ( 'NONE',  ( 1.581364829396326277, -0.05778040916215522460, 0.4822834645669289988 ) ) ;
#12535 = CARTESIAN_POINT ( 'NONE',  ( 0.1049643490035303689, 0.3917322834645670104, -2.125328083989501238 ) ) ;
#12536 = CARTESIAN_POINT ( 'NONE',  ( -0.01968503937007793844, 0.1660481256975883668, -0.3530559997133364547 ) ) ;
#12537 = CARTESIAN_POINT ( 'NONE',  ( -1.161417322834644716, 0.07958543189024085140, 0.2665933059059887866 ) ) ;
#12538 = CARTESIAN_POINT ( 'NONE',  ( -0.3871391076115479057, -0.3162353388693409650, -0.4822834645669289433 ) ) ;
#12539 = CARTESIAN_POINT ( 'NONE',  ( -0.4724409448818899238, 0.1265901696524986686, -2.786745406824146620 ) ) ;
#12540 = EDGE_CURVE ( 'NONE', #21842, #11553, #17432, .T. ) ;
#12541 = CARTESIAN_POINT ( 'NONE',  ( -0.7939632545931754048, -0.3162353388693405765, 0.4822834645669290543 ) ) ;
#12542 = CARTESIAN_POINT ( 'NONE',  ( -0.9251968503937002541, 0.1660481256975885056, 0.3530559997133364547 ) ) ;
#12543 = CARTESIAN_POINT ( 'NONE',  ( -0.2891555358219909388, -0.2891555358219912164, -2.340551181102362488 ) ) ;
#12544 = CARTESIAN_POINT ( 'NONE',  ( 1.049868766404200127, -0.5023911411419708095, -0.1820866141732282451 ) ) ;
#12545 = CARTESIAN_POINT ( 'NONE',  ( -0.8923884514435688198, 0.1283753931104746893, -0.1820866141732285504 ) ) ;
#12546 = AXIS2_PLACEMENT_3D ( 'NONE', #74485, #47545, #54688 ) ;
#12547 = CARTESIAN_POINT ( 'NONE',  ( 0.8989501312335964611, 0.1771653543307087630, 0.09757992244046791164 ) ) ;
#12548 = CARTESIAN_POINT ( 'NONE',  ( -1.620734908136482577, -0.6692913385826773087, -0.1292274648535924053 ) ) ;
#12549 = CARTESIAN_POINT ( 'NONE',  ( 1.417322834645670104, -0.1870078740157479769, 0.4822834645669291653 ) ) ;
#12550 = CARTESIAN_POINT ( 'NONE',  ( 0.7086614173228353852, -0.1870078740157479769, 0.3641732283464567677 ) ) ;
#12551 = CARTESIAN_POINT ( 'NONE',  ( -0.7152230971128602510, -0.3162353388693405765, 0.4822834645669290543 ) ) ;
#12552 = CARTESIAN_POINT ( 'NONE',  ( 1.154855643044620184, 0.2306618581243847221, -0.2411417322834647770 ) ) ;
#12553 = CARTESIAN_POINT ( 'NONE',  ( -0.4724409448818895907, -0.1265901696524993070, -0.1227034120734908362 ) ) ;
#12554 = CARTESIAN_POINT ( 'NONE',  ( -0.2296587926509179312, -0.08942795157527998196, 0.3641732283464567121 ) ) ;
#12555 = LINE ( 'NONE', #63889, #5013 ) ;
#12556 = CARTESIAN_POINT ( 'NONE',  ( 0.3018372703412079971, 0.05413385826771626580, -0.4176697321401330321 ) ) ;
#12557 = CARTESIAN_POINT ( 'NONE',  ( 0.6889763779527563470, 0.1660481256975883391, -0.3530559997133364547 ) ) ;
#12558 = AXIS2_PLACEMENT_3D ( 'NONE', #11056, #79711, #22027 ) ;
#12559 = CARTESIAN_POINT ( 'NONE',  ( 0.9448818897637802916, -0.1870078740157479769, 0.3641732283464567677 ) ) ;
#12560 = CARTESIAN_POINT ( 'NONE',  ( 0.2690288713910767848, -0.5511811023622048555, -0.09757992244046775898 ) ) ;
#12561 = CARTESIAN_POINT ( 'NONE',  ( -0.05249343832020911260, 0.2306618581243848609, 0.2411417322834645549 ) ) ;
#12562 = CARTESIAN_POINT ( 'NONE',  ( -1.555118110236219930, 0.1660481256975885056, 0.3530559997133364547 ) ) ;
#12563 = CARTESIAN_POINT ( 'NONE',  ( -0.6430446194225712953, -0.004921259842519870586, -0.3153832671262229437 ) ) ;
#12564 = CARTESIAN_POINT ( 'NONE',  ( 3.886287458032462006, 2.755905511811024056, -0.6299212598425196763 ) ) ;
#12565 = CARTESIAN_POINT ( 'NONE',  ( -0.6692913385826764205, 0.2952755905511811885, 0.000000000000000000 ) ) ;
#12566 = CARTESIAN_POINT ( 'NONE',  ( 0.1070741851644053388, 0.3996062992125986035, -1.172572178477690352 ) ) ;
#12567 = CARTESIAN_POINT ( 'NONE',  ( -9.594673741351313045E-17, 0.3917322834645670104, -2.289370078740157410 ) ) ;
#12568 = CARTESIAN_POINT ( 'NONE',  ( 0.1312335958005255154, -0.5023911411419708095, 0.1820866141732285504 ) ) ;
#12569 = CARTESIAN_POINT ( 'NONE',  ( -0.4396325459317577122, -0.6692913385826773087, -0.1292274648535924053 ) ) ;
#12570 = CARTESIAN_POINT ( 'NONE',  ( -0.9514435695538050464, -0.05778040916215560624, -0.4822834645669293319 ) ) ;
#12571 = CARTESIAN_POINT ( 'NONE',  ( -0.9383202099737524282, -0.2845877964562161244, -0.3641732283464567121 ) ) ;
#12572 = CARTESIAN_POINT ( 'NONE',  ( -3.908320185825791437, 1.506315459106587040, 0.4744094488188971837 ) ) ;
#12573 = EDGE_CURVE ( 'NONE', #23460, #58699, #31796, .T. ) ;
#12574 = CARTESIAN_POINT ( 'NONE',  ( -0.1246719160104980823, -0.6692913385826773087, -0.1292274648535924053 ) ) ;
#12575 = CARTESIAN_POINT ( 'NONE',  ( -1.502624671916009680, -0.08942795157528024563, -0.3641732283464568787 ) ) ;
#12576 = CARTESIAN_POINT ( 'NONE',  ( 1.292650918635171564, 0.2952755905511811885, 0.1292274648535926551 ) ) ;
#12577 = CARTESIAN_POINT ( 'NONE',  ( -0.4580699644866061959, 1.664928367767637418, 1.024310904178314718 ) ) ;
#12578 = CARTESIAN_POINT ( 'NONE',  ( -0.2867679344610367109, 0.2867679344610365444, -2.063667609745093667 ) ) ;
#12579 = ORIENTED_EDGE ( 'NONE', *, *, #783, .F. ) ;
#12580 = CARTESIAN_POINT ( 'NONE',  ( 1.403614904275686858E-14, 1.537401574803149984, -3.937007874015761910 ) ) ;
#12581 = CARTESIAN_POINT ( 'NONE',  ( -1.456692913385826182, -0.6692913385826771977, 8.415575281601705876E-17 ) ) ;
#12582 = CARTESIAN_POINT ( 'NONE',  ( -0.9908136482939626788, -0.6692913385826773087, -0.1292274648535924053 ) ) ;
#12583 = EDGE_CURVE ( 'NONE', #36535, #11377, #52713, .T. ) ;
#12584 = CARTESIAN_POINT ( 'NONE',  ( -1.541994750656167090, -0.6692913385826773087, -0.1292274648535924053 ) ) ;
#12585 = CARTESIAN_POINT ( 'NONE',  ( -9.594673741351313045E-17, 0.3917322834645670104, -1.816929133858267820 ) ) ;
#12586 = CARTESIAN_POINT ( 'NONE',  ( 0.4177787735907000366, 1.299212598425196985, -1.559171609364239375 ) ) ;
#12587 = CARTESIAN_POINT ( 'NONE',  ( 0.8398950131233602345, -0.6046776061558807314, 0.2411417322834647770 ) ) ;
#12588 = CARTESIAN_POINT ( 'NONE',  ( 0.04593175853018440641, -0.6692913385826771977, 0.1292274648535927661 ) ) ;
#12589 = CARTESIAN_POINT ( 'NONE',  ( 0.4600214019799526155, 2.784432375088962958E-17, -0.3464511005275205946 ) ) ;
#12590 = CARTESIAN_POINT ( 'NONE',  ( -0.2925321140481932369, 0.2925321140481930704, -2.616141732283464361 ) ) ;
#12591 = CARTESIAN_POINT ( 'NONE',  ( 1.325459317585302665, -0.004921259842519870586, -0.3153832671262229437 ) ) ;
#12592 = CARTESIAN_POINT ( 'NONE',  ( 0.3996062992125986035, 0.1070741851644054776, -1.227034120734908029 ) ) ;
#12593 = VERTEX_POINT ( 'NONE', #55283 ) ;
#12594 = CARTESIAN_POINT ( 'NONE',  ( -9.594673741351313045E-17, 0.3917322834645670659, 0.1607418390738039049 ) ) ;
#12595 = ORIENTED_EDGE ( 'NONE', *, *, #57238, .F. ) ;
#12596 = CARTESIAN_POINT ( 'NONE',  ( -0.1640419947506555343, -0.3162353388693405765, 0.4822834645669290543 ) ) ;
#12597 = CARTESIAN_POINT ( 'NONE',  ( -0.7020997375328076329, -0.3162353388693409650, -0.4822834645669289433 ) ) ;
#12598 = CARTESIAN_POINT ( 'NONE',  ( -1.633858267716534529, 0.1660481256975885056, 0.3530559997133364547 ) ) ;
#12599 = CARTESIAN_POINT ( 'NONE',  ( 0.4658792650918641698, -0.05778040916215560624, -0.4822834645669293319 ) ) ;
#12600 = AXIS2_PLACEMENT_3D ( 'NONE', #15907, #47444, #41556 ) ;
#12601 = CARTESIAN_POINT ( 'NONE',  ( 1.607611548556431069, -0.6692913385826773087, -0.1292274648535924053 ) ) ;
#12602 = CARTESIAN_POINT ( 'NONE',  ( 1.509186351706037543, -0.4281496062992127816, -0.4176697321401328100 ) ) ;
#12603 = CARTESIAN_POINT ( 'NONE',  ( -0.05905511811023545637, 0.1660481256975885056, 0.3530559997133364547 ) ) ;
#12604 = CARTESIAN_POINT ( 'NONE',  ( -1.318897637795274802, 0.1660481256975885056, 0.3530559997133364547 ) ) ;
#12605 = CARTESIAN_POINT ( 'NONE',  ( 1.135170603674541256, 0.2952755905511811885, 0.1292274648535926551 ) ) ;
#12606 = CARTESIAN_POINT ( 'NONE',  ( 1.594488188976378673, -0.5400638737290845981, -0.3530559997133363437 ) ) ;
#12607 = CARTESIAN_POINT ( 'NONE',  ( -0.04593175853018302557, -0.6692913385826773087, -0.1292274648535924053 ) ) ;
#12608 = CARTESIAN_POINT ( 'NONE',  ( 0.2867679344610365999, -0.2867679344610365444, -0.09055118110236216877 ) ) ;
#12609 = CARTESIAN_POINT ( 'NONE',  ( 0.4199475065616805614, 0.1283753931104748280, 0.1820866141732283561 ) ) ;
#12610 = ORIENTED_EDGE ( 'NONE', *, *, #51722, .F. ) ;
#12611 = CARTESIAN_POINT ( 'NONE',  ( 0.1058382717557500713, -0.3949938075777409408, -0.7152230971128611392 ) ) ;
#12612 = EDGE_LOOP ( 'NONE', ( #10729, #35292, #78563, #68792, #17278, #4126, #53409, #82299 ) ) ;
#12613 = CARTESIAN_POINT ( 'NONE',  ( -0.02624671916010428221, -0.5023911411419708095, 0.1820866141732285504 ) ) ;
#12614 = CARTESIAN_POINT ( 'NONE',  ( 2.808244076867902450, 1.134815007188468838, -0.2514610820057333607 ) ) ;
#12615 = CARTESIAN_POINT ( 'NONE',  ( -0.01312335958005186876, -0.4281496062992124485, 0.4176697321401328655 ) ) ;
#12616 = CARTESIAN_POINT ( 'NONE',  ( -0.1246719160104980823, 0.2952755905511811885, 0.1292274648535926551 ) ) ;
#12617 = CARTESIAN_POINT ( 'NONE',  ( -0.7611548556430438595, 0.2306618581243848609, 0.2411417322834645549 ) ) ;
#12618 = AXIS2_PLACEMENT_3D ( 'NONE', #67291, #62617, #55868 ) ;
#12619 = CARTESIAN_POINT ( 'NONE',  ( -0.1958661417322833942, -0.3392501089628018884, -1.794638738354017660 ) ) ;
#12620 = CARTESIAN_POINT ( 'NONE',  ( -1.148293963254592542, 0.2952755905511811885, 0.1292274648535926551 ) ) ;
#12621 = CARTESIAN_POINT ( 'NONE',  ( -0.2867679344610364334, -0.2867679344610367109, -2.820866141732283339 ) ) ;
#12622 = CARTESIAN_POINT ( 'NONE',  ( 1.423884514435696191, -0.08942795157527998196, 0.3641732283464567121 ) ) ;
#12623 = CARTESIAN_POINT ( 'NONE',  ( 1.030183727034121421, -0.05778040916215522460, 0.4822834645669289988 ) ) ;
#12624 = CARTESIAN_POINT ( 'NONE',  ( 0.9383202099737538715, -0.05778040916215560624, -0.4822834645669293319 ) ) ;
#12625 = CARTESIAN_POINT ( 'NONE',  ( -0.2925321140481930704, -0.2925321140481933480, -0.8464566929133857665 ) ) ;
#12626 = CARTESIAN_POINT ( 'NONE',  ( -1.233595800524933894, 0.2306618581243848609, 0.2411417322834645549 ) ) ;
#12627 = CARTESIAN_POINT ( 'NONE',  ( 0.3996062992125985480, 2.446882876249141654E-17, -0.3523622047244094335 ) ) ;
#12628 = CARTESIAN_POINT ( 'NONE',  ( 0.2925321140481932369, 0.2925321140481932369, -0.2145669291338583029 ) ) ;
#12629 = CARTESIAN_POINT ( 'NONE',  ( -0.2821522309711278487, 0.2952755905511811885, 0.1292274648535926551 ) ) ;
#12630 = CARTESIAN_POINT ( 'NONE',  ( 0.1070741851644053527, 0.3996062992125986590, -2.828083989501312345 ) ) ;
#12631 = CARTESIAN_POINT ( 'NONE',  ( 0.3917322834645670104, -0.1049643490035303411, -1.613517060367454237 ) ) ;
#12632 = CARTESIAN_POINT ( 'NONE',  ( 1.456692913385827515, 0.2952755905511811885, 0.000000000000000000 ) ) ;
#12633 = CARTESIAN_POINT ( 'NONE',  ( 1.318897637795276356, -0.5400638737290844871, 0.3530559997133364547 ) ) ;
#12634 = CARTESIAN_POINT ( 'NONE',  ( 0.3477690288713918276, -0.5511811023622048555, -0.09757992244046775898 ) ) ;
#12635 = CARTESIAN_POINT ( 'NONE',  ( 1.108923884514436242, -0.05778040916215522460, 0.4822834645669289988 ) ) ;
#12636 = CARTESIAN_POINT ( 'NONE',  ( -0.4724409448818895907, -0.1265901696524993070, -1.540026246719159886 ) ) ;
#12637 = CARTESIAN_POINT ( 'NONE',  ( 0.5446194225721792126, -0.2845877964562159024, 0.3641732283464567677 ) ) ;
#12638 = CARTESIAN_POINT ( 'NONE',  ( 0.5643044619422579178, -0.4281496062992127816, -0.4176697321401328100 ) ) ;
#12639 = CARTESIAN_POINT ( 'NONE',  ( -0.1974969037888706924, 0.3420746716998658843, -0.8772965879265093303 ) ) ;
#12640 = CARTESIAN_POINT ( 'NONE',  ( -1.036745406824146176, 0.05413385826771626580, -0.4176697321401330321 ) ) ;
#12641 = CARTESIAN_POINT ( 'NONE',  ( 1.010498687664042716, -0.004921259842519870586, -0.3153832671262229437 ) ) ;
#12642 = DIRECTION ( 'NONE',  ( 0.000000000000000000, 0.000000000000000000, 1.000000000000000000 ) ) ;
#12643 = CARTESIAN_POINT ( 'NONE',  ( -0.4396325459317579898, 0.2952755905511811885, 0.1292274648535926551 ) ) ;
#12644 = CARTESIAN_POINT ( 'NONE',  ( -0.1246719160104980823, -0.5511811023622048555, -0.09757992244046775898 ) ) ;
#12645 = CARTESIAN_POINT ( 'NONE',  ( 0.4581548244795011215, 1.775897344681688805, 0.5309055118110234117 ) ) ;
#12646 = CARTESIAN_POINT ( 'NONE',  ( -0.2690288713910754526, 0.2952755905511810774, -0.1292274648535930714 ) ) ;
#12647 = CARTESIAN_POINT ( 'NONE',  ( 0.5183727034120741983, 0.1771653543307087075, -0.09757992244046823083 ) ) ;
#12648 = B_SPLINE_CURVE_WITH_KNOTS ( 'NONE', 3,
 ( #3173, #80214, #28837, #67569 ),
 .UNSPECIFIED., .F., .F.,
 ( 4, 4 ),
 ( 3.210432057656183116E-07, 0.001287787053612039377 ),
 .UNSPECIFIED. ) ;
#12649 = CARTESIAN_POINT ( 'NONE',  ( 0.3996062992125984925, 0.1070741851644054637, -2.248687664041995049 ) ) ;
#12650 = CARTESIAN_POINT ( 'NONE',  ( 0.1246719160104994284, 0.2952755905511810774, -0.1292274648535930714 ) ) ;
#12651 = CARTESIAN_POINT ( 'NONE',  ( 0.3392501089628018329, 0.1958661417322835052, -1.471109293142045304 ) ) ;
#12652 = CARTESIAN_POINT ( 'NONE',  ( 1.279527559055118724, -0.4536011799217368745, -0.2665933059059886201 ) ) ;
#12653 = CARTESIAN_POINT ( 'NONE',  ( 0.3830016109920622025, 1.809133623825372073E-16, -0.4118484887281974038 ) ) ;
#12654 = CARTESIAN_POINT ( 'NONE',  ( -0.9580052493438311334, -0.3690944881889763329, 0.3153832671262228327 ) ) ;
#12655 = EDGE_CURVE ( 'NONE', #19415, #66357, #34525, .T. ) ;
#12656 = CARTESIAN_POINT ( 'NONE',  ( -0.7152230971128602510, -0.08942795157528024563, -0.3641732283464568787 ) ) ;
#12657 = CARTESIAN_POINT ( 'NONE',  ( -0.1181102362204717315, -0.6692913385826771977, 8.415575281601705876E-17 ) ) ;
#12658 = CARTESIAN_POINT ( 'NONE',  ( -0.2755905511811018171, 0.2952755905511811885, 0.000000000000000000 ) ) ;
#12659 = CARTESIAN_POINT ( 'NONE',  ( 0.4068241469816281097, -0.004921259842519576551, 0.3153832671262227771 ) ) ;
#12660 = CARTESIAN_POINT ( 'NONE',  ( -1.587926509186350810, -0.3690944881889763329, 0.3153832671262228327 ) ) ;
#12661 = CARTESIAN_POINT ( 'NONE',  ( -1.725721784776902190, -0.05778040916215522460, 0.4822834645669289988 ) ) ;
#12662 = CIRCLE ( 'NONE', #535, 0.1968503937007874405 ) ;
#12663 = EDGE_CURVE ( 'NONE', #23658, #62570, #6506, .T. ) ;
#12664 = CARTESIAN_POINT ( 'NONE',  ( 0.7545931758530189937, 0.2952755905511810774, -0.1292274648535930714 ) ) ;
#12665 = CARTESIAN_POINT ( 'NONE',  ( 0.1938976377952755792, -0.1938976377952756069, -0.3740157480314971750 ) ) ;
#12666 = CARTESIAN_POINT ( 'NONE',  ( -0.1181102362204717315, 0.2952755905511811885, 0.000000000000000000 ) ) ;
#12667 = CARTESIAN_POINT ( 'NONE',  ( -0.2867679344610365999, 0.2867679344610364889, -0.8917322834645667884 ) ) ;
#12668 = CARTESIAN_POINT ( 'NONE',  ( -1.469816272965878357, -0.6046776061558809534, -0.2411417322834644161 ) ) ;
#12669 = CARTESIAN_POINT ( 'NONE',  ( 1.076115485564305141, 0.2306618581243847221, -0.2411417322834647770 ) ) ;
#12670 = CARTESIAN_POINT ( 'NONE',  ( 0.7480314960629927956, 0.2952755905511811885, 0.000000000000000000 ) ) ;
#12671 = DIRECTION ( 'NONE',  ( 0.000000000000000000, 0.000000000000000000, 1.000000000000000000 ) ) ;
#12672 = CARTESIAN_POINT ( 'NONE',  ( 0.1902887139107617975, -0.5511811023622048555, -0.09757992244046775898 ) ) ;
#12673 = CARTESIAN_POINT ( 'NONE',  ( 1.371391076115485941, 0.2952755905511811885, 0.1292274648535926551 ) ) ;
#12674 = CARTESIAN_POINT ( 'NONE',  ( -0.2099737532808391705, -0.5023911411419708095, -0.1820866141732282451 ) ) ;
#12675 = AXIS2_PLACEMENT_3D ( 'NONE', #38369, #62391, #62817 ) ;
#12676 = CARTESIAN_POINT ( 'NONE',  ( -0.5446194225721777693, -0.05778040916215522460, 0.4822834645669289988 ) ) ;
#12677 = DIRECTION ( 'NONE',  ( 0.000000000000000000, 1.000000000000000000, -1.734723475976805862E-16 ) ) ;
#12678 = CARTESIAN_POINT ( 'NONE',  ( 0.09186351706036799403, -0.4281496062992127816, -0.4176697321401328100 ) ) ;
#12679 = APPLICATION_CONTEXT ( 'automotive_design' ) ;
#12680 = CARTESIAN_POINT ( 'NONE',  ( -0.8661417322834640276, -0.1870078740157479769, 0.4822834645669291653 ) ) ;
#12681 = CARTESIAN_POINT ( 'NONE',  ( -0.6889763779527552368, -0.4536011799217368745, -0.2665933059059886201 ) ) ;
#12682 = CARTESIAN_POINT ( 'NONE',  ( 0.4396325459317590445, -0.6692913385826771977, 0.1292274648535927661 ) ) ;
#12683 = CARTESIAN_POINT ( 'NONE',  ( -1.089238845144356427, 0.05413385826771666132, 0.4176697321401328100 ) ) ;
#12684 = CARTESIAN_POINT ( 'NONE',  ( -0.2821522309711278487, -0.6692913385826773087, -0.1292274648535924053 ) ) ;
#12685 = SURFACE_STYLE_USAGE ( .BOTH. , #24061 ) ;
#12687 = CARTESIAN_POINT ( 'NONE',  ( 1.213910761154856299, -0.6692913385826773087, -0.1292274648535924053 ) ) ;
#12686 = LINE ( 'NONE', #13107, #35232 ) ;
#12688 = CARTESIAN_POINT ( 'NONE',  ( 1.253280839895013710, -0.05778040916215560624, -0.4822834645669293319 ) ) ;
#12689 = CARTESIAN_POINT ( 'NONE',  ( 0.3392501089628018884, -0.1958661417322834220, -2.144356955380577467 ) ) ;
#12690 = DIRECTION ( 'NONE',  ( 0.7071067811865477948, 0.000000000000000000, -0.7071067811865473507 ) ) ;
#12691 = CARTESIAN_POINT ( 'NONE',  ( -1.043307086614172707, 0.1660481256975883668, -0.3530559997133364547 ) ) ;
#12692 = CARTESIAN_POINT ( 'NONE',  ( 0.2362204724409449064, 0.4091458600556404646, -0.3018372703412073310 ) ) ;
#12693 = CARTESIAN_POINT ( 'NONE',  ( -0.2925321140481930704, -0.2925321140481933480, -0.05905511811023622659 ) ) ;
#12694 = ORIENTED_EDGE ( 'NONE', *, *, #47802, .T. ) ;
#12695 = CARTESIAN_POINT ( 'NONE',  ( -0.1377952755905504645, -0.4536011799217368745, -0.2665933059059886201 ) ) ;
#12696 = CARTESIAN_POINT ( 'NONE',  ( 0.1049643490035303689, 0.3917322834645670104, -1.875328083989501460 ) ) ;
#12697 = CARTESIAN_POINT ( 'NONE',  ( 0.7152230971128614723, -0.3162353388693409650, -0.4822834645669289433 ) ) ;
#12698 = CARTESIAN_POINT ( 'NONE',  ( -1.157146581871515012E-16, 0.4724409448818898682, -2.834645669291338432 ) ) ;
#12699 = CARTESIAN_POINT ( 'NONE',  ( -1.614173228346457378, 1.881821177735609085, -0.1372047244094477536 ) ) ;
#12700 = CARTESIAN_POINT ( 'NONE',  ( -0.3805774278215216522, -0.004921259842519576551, 0.3153832671262227771 ) ) ;
#12701 = CARTESIAN_POINT ( 'NONE',  ( 0.3836918680457899744, 8.471767977567108961E-16, -0.4445507791589058955 ) ) ;
#12702 = CARTESIAN_POINT ( 'NONE',  ( 1.332020997375329197, -0.3162353388693405765, 0.4822834645669290543 ) ) ;
#12703 = CARTESIAN_POINT ( 'NONE',  ( 0.7611548556430451917, -0.5023911411419708095, 0.1820866141732285504 ) ) ;
#12704 = CARTESIAN_POINT ( 'NONE',  ( -0.2034120734908128059, 0.2952755905511811885, 0.1292274648535926551 ) ) ;
#12705 = CARTESIAN_POINT ( 'NONE',  ( 0.3917322834645668994, -0.1049643490035303134, -0.8215029939294470340 ) ) ;
#12706 = CARTESIAN_POINT ( 'NONE',  ( -1.003937007874014853, 0.1660481256975885056, 0.3530559997133364547 ) ) ;
#12707 = CARTESIAN_POINT ( 'NONE',  ( -1.194225721784776262, -0.004921259842519870586, -0.3153832671262229437 ) ) ;
#12708 = CARTESIAN_POINT ( 'NONE',  ( -0.4724409448818890911, -0.1870078740157479769, 0.4822834645669291653 ) ) ;
#12709 = LINE ( 'NONE', #75455, #5874 ) ;
#12710 = CARTESIAN_POINT ( 'NONE',  ( 0.4531182788721080934, 1.771653543307086354, -0.5309055118110237448 ) ) ;
#12711 = EDGE_LOOP ( 'NONE', ( #79365, #14090, #71316, #31641, #37257 ) ) ;
#12712 = CARTESIAN_POINT ( 'NONE',  ( 0.3392501089628018329, 0.1958661417322835607, -2.017735851214910170 ) ) ;
#12713 = CARTESIAN_POINT ( 'NONE',  ( 0.5511811023622055217, -0.1870078740157479769, 0.4822834645669291653 ) ) ;
#12714 = VERTEX_POINT ( 'NONE', #30858 ) ;
#12715 = CARTESIAN_POINT ( 'NONE',  ( -0.9514435695538050464, -0.3162353388693405765, 0.4822834645669290543 ) ) ;
#12716 = CARTESIAN_POINT ( 'NONE',  ( 1.456692913385827515, 0.2952755905511811885, 0.000000000000000000 ) ) ;
#12717 = CARTESIAN_POINT ( 'NONE',  ( 0.8858267716535438430, -0.5400638737290845981, -0.3530559997133363437 ) ) ;
#12718 = CARTESIAN_POINT ( 'NONE',  ( 0.01968503937007957949, -0.5400638737290845981, -0.3530559997133363437 ) ) ;
#12719 = CARTESIAN_POINT ( 'NONE',  ( -0.2867679344610364334, -0.2867679344610367109, -1.246062992125984481 ) ) ;
#12720 = CARTESIAN_POINT ( 'NONE',  ( -0.6102362204724400829, 0.1660481256975885056, 0.3530559997133364547 ) ) ;
#12721 = CARTESIAN_POINT ( 'NONE',  ( -0.05905511811023545637, 0.1660481256975885056, 0.3530559997133364547 ) ) ;
#12722 = CIRCLE ( 'NONE', #59763, 0.5118110236220471121 ) ;
#12723 = CARTESIAN_POINT ( 'NONE',  ( -0.09842519685039295696, -0.4536011799217367080, 0.2665933059059888421 ) ) ;
#12724 = CARTESIAN_POINT ( 'NONE',  ( -0.01218835185196217967, 0.3960428127060656167, -1.229201864173550318E-17 ) ) ;
#12725 = CARTESIAN_POINT ( 'NONE',  ( 0.1181102362204730916, -0.6692913385826771977, 8.415575281601705876E-17 ) ) ;
#12726 = CARTESIAN_POINT ( 'NONE',  ( 1.141392835773559211, 1.299212598425196985, 1.141392835773562764 ) ) ;
#12727 = CARTESIAN_POINT ( 'NONE',  ( 0.9580052493438326877, 0.05413385826771666132, 0.4176697321401328100 ) ) ;
#12728 = CARTESIAN_POINT ( 'NONE',  ( 0.4852136692201463597, 0.004960608223778677044, 0.3437734562760191293 ) ) ;
#12729 = ORIENTED_EDGE ( 'NONE', *, *, #47818, .T. ) ;
#12730 = ORIENTED_EDGE ( 'NONE', *, *, #12540, .F. ) ;
#12731 = CARTESIAN_POINT ( 'NONE',  ( 0.09186351706036827158, 0.05413385826771666132, 0.4176697321401328100 ) ) ;
#12732 = CARTESIAN_POINT ( 'NONE',  ( -0.3608923884514428360, -0.5511811023622048555, -0.09757992244046775898 ) ) ;
#12734 = CARTESIAN_POINT ( 'NONE',  ( 0.000000000000000000, 0.000000000000000000, -1.929133858267716661 ) ) ;
#12733 = CARTESIAN_POINT ( 'NONE',  ( 1.299212598425197429, -0.5511811023622047445, 6.969142054262312111E-17 ) ) ;
#12735 = CARTESIAN_POINT ( 'NONE',  ( -0.3392501089628019995, 0.1958661417322832277, -1.055774278215223294 ) ) ;
#12736 = CARTESIAN_POINT ( 'NONE',  ( -0.2362204724409451284, 0.4091458600556402425, -0.08989501312335958227 ) ) ;
#12737 = CARTESIAN_POINT ( 'NONE',  ( 1.620734908136483465, -0.5511811023622046335, 0.09757992244046803654 ) ) ;
#12738 = CARTESIAN_POINT ( 'NONE',  ( 1.463254593175853824, 0.2952755905511810774, -0.1292274648535930714 ) ) ;
#12739 = VECTOR ( 'NONE', #1130, 39.37007874015748143 ) ;
#12740 = CARTESIAN_POINT ( 'NONE',  ( 0.3949938075777409408, -0.1058382717557499186, 0.1266404199475065773 ) ) ;
#12741 = CARTESIAN_POINT ( 'NONE',  ( -0.09842519685039295696, 0.1660481256975883668, -0.3530559997133364547 ) ) ;
#12742 = CARTESIAN_POINT ( 'NONE',  ( -1.332020997375327642, -0.05778040916215522460, 0.4822834645669289988 ) ) ;
#12743 = CARTESIAN_POINT ( 'NONE',  ( -1.135170603674539924, -0.6692913385826771977, 0.1292274648535927661 ) ) ;
#12744 = CARTESIAN_POINT ( 'NONE',  ( 0.07217847769028949700, -0.05778040916215560624, -0.4822834645669293319 ) ) ;
#12745 = CARTESIAN_POINT ( 'NONE',  ( 0.3420746716998660508, 0.1974969037888705814, -0.2080052493438320771 ) ) ;
#12746 = CARTESIAN_POINT ( 'NONE',  ( 1.515748031496063408, 0.1660481256975885056, 0.3530559997133364547 ) ) ;
#12747 = CARTESIAN_POINT ( 'NONE',  ( 0.7874015748031503170, -0.1870078740157479769, 0.4822834645669291653 ) ) ;
#12748 = CARTESIAN_POINT ( 'NONE',  ( 1.259842519685040019, -0.1870078740157480601, -0.3641732283464567677 ) ) ;
#12749 = CARTESIAN_POINT ( 'NONE',  ( 0.3917322834645670104, 2.398668435337828261E-17, -2.722440944881889369 ) ) ;
#12750 = CONTEXT_DEPENDENT_SHAPE_REPRESENTATION ( #79945, #40624 ) ;
#12751 = CARTESIAN_POINT ( 'NONE',  ( 0.6561679790026253567, -0.5023911411419708095, -0.1820866141732282451 ) ) ;
#12752 = CARTESIAN_POINT ( 'NONE',  ( -1.115485564304461219, 0.05413385826771626580, -0.4176697321401330321 ) ) ;
#12753 = CARTESIAN_POINT ( 'NONE',  ( 0.2925321140481932369, 0.2925321140481932369, -1.001968503937007871 ) ) ;
#12754 = CARTESIAN_POINT ( 'NONE',  ( 1.082677165354331228, 0.1660481256975883668, -0.3530559997133364547 ) ) ;
#12755 = CARTESIAN_POINT ( 'NONE',  ( -0.1049643490035302024, -0.3917322834645671215, -0.2217847769028870319 ) ) ;
#12757 = DIRECTION ( 'NONE',  ( -0.000000000000000000, -1.000000000000000000, -0.000000000000000000 ) ) ;
#12756 = CARTESIAN_POINT ( 'NONE',  ( 0.5643044619422579178, 0.05413385826771666132, 0.4176697321401328100 ) ) ;
#12758 = CARTESIAN_POINT ( 'NONE',  ( -1.725721784776902190, -0.08942795157527998196, 0.3641732283464567121 ) ) ;
#12759 = CARTESIAN_POINT ( 'NONE',  ( 0.1574803149606306130, -0.1870078740157480879, -0.4822834645669291653 ) ) ;
#12760 = CARTESIAN_POINT ( 'NONE',  ( 0.7217847769028878924, -0.3690944881889765550, -0.3153832671262227771 ) ) ;
#12761 = ADVANCED_FACE ( 'NONE', ( #56933 ), #37178, .F. ) ;
#12762 = CARTESIAN_POINT ( 'NONE',  ( 0.9514435695538062676, -0.3162353388693409650, -0.4822834645669289433 ) ) ;
#12763 = CARTESIAN_POINT ( 'NONE',  ( -1.559171609364246924, 0.3937007874015747699, 0.2199441279213821265 ) ) ;
#12764 = CARTESIAN_POINT ( 'NONE',  ( -0.3805774278215216522, -0.3690944881889765550, -0.3153832671262227771 ) ) ;
#12765 = CARTESIAN_POINT ( 'NONE',  ( -0.4921259842519677963, -0.5400638737290844871, 0.3530559997133364547 ) ) ;
#12766 = CARTESIAN_POINT ( 'NONE',  ( -1.607611548556429737, 0.1771653543307087075, -0.09757992244046823083 ) ) ;
#12767 = CARTESIAN_POINT ( 'NONE',  ( -0.9908136482939626788, -0.6692913385826773087, -0.1292274648535924053 ) ) ;
#12768 = CARTESIAN_POINT ( 'NONE',  ( 1.056430446194226658, 0.2952755905511811885, 0.1292274648535926551 ) ) ;
#12769 = CARTESIAN_POINT ( 'NONE',  ( 0.1958661417322834775, 0.3392501089628018884, -0.7710166911099232134 ) ) ;
#12770 = CARTESIAN_POINT ( 'NONE',  ( -1.541994750656167090, -0.5511811023622048555, -0.09757992244046775898 ) ) ;
#12771 = CARTESIAN_POINT ( 'NONE',  ( -1.313877454013331780, 1.062992125984252079, 0.7983292792091805090 ) ) ;
#12772 = CARTESIAN_POINT ( 'NONE',  ( 1.089238845144357537, -0.4281496062992124485, 0.4176697321401328655 ) ) ;
#12773 = CARTESIAN_POINT ( 'NONE',  ( 0.4091458600556403535, 0.2362204724409449896, -2.412729658792650778 ) ) ;
#12774 = CARTESIAN_POINT ( 'NONE',  ( -1.620734908136482577, -0.6692913385826773087, -0.1292274648535924053 ) ) ;
#12775 = CARTESIAN_POINT ( 'NONE',  ( -1.548556430446193399, -0.5023911411419708095, -0.1820866141732282451 ) ) ;
#12776 = CARTESIAN_POINT ( 'NONE',  ( -0.9842519685039365918, -0.5511811023622047445, 6.969142054262312111E-17 ) ) ;
#12777 = DIRECTION ( 'NONE',  ( 1.000000000000000000, 0.000000000000000000, 0.000000000000000000 ) ) ;
#12778 = CARTESIAN_POINT ( 'NONE',  ( -0.3740157480314953431, 0.1660481256975885056, 0.3530559997133364547 ) ) ;
#12779 = CARTESIAN_POINT ( 'NONE',  ( -0.4133858267716528645, -0.4536011799217367080, 0.2665933059059888421 ) ) ;
#12780 = PLANE ( 'NONE',  #22503 ) ;
#12781 = CARTESIAN_POINT ( 'NONE',  ( 1.122047244094488860, 0.07958543189024085140, 0.2665933059059887866 ) ) ;
#12782 = CARTESIAN_POINT ( 'NONE',  ( 0.3937007874015754361, -0.1870078740157479769, 0.4822834645669291653 ) ) ;
#12783 = CARTESIAN_POINT ( 'NONE',  ( 1.358267716535433323, -0.5400638737290845981, -0.3530559997133363437 ) ) ;
#12784 = CARTESIAN_POINT ( 'NONE',  ( -0.03280839895013062252, 0.1771653543307087075, -0.09757992244046823083 ) ) ;
#12785 = PRODUCT_DEFINITION_FORMATION_WITH_SPECIFIED_SOURCE ( 'ANY', '', #38538, .NOT_KNOWN. ) ;
#12786 = CARTESIAN_POINT ( 'NONE',  ( 0.6496062992125991586, -0.5400638737290845981, -0.3530559997133363437 ) ) ;
#12787 = CARTESIAN_POINT ( 'NONE',  ( 0.7742782152230978099, -0.3690944881889763329, 0.3153832671262228327 ) ) ;
#12788 = CARTESIAN_POINT ( 'NONE',  ( -1.437007874015747477, 0.1660481256975883668, -0.3530559997133364547 ) ) ;
#12789 = CARTESIAN_POINT ( 'NONE',  ( -1.141732283464566011, 0.2952755905511811885, 0.000000000000000000 ) ) ;
#12790 = CARTESIAN_POINT ( 'NONE',  ( -0.3543307086614165824, -0.6692913385826771977, 8.415575281601705876E-17 ) ) ;
#12791 = CARTESIAN_POINT ( 'NONE',  ( -0.2925321140481930704, -0.2925321140481933480, -0.5314960629921260393 ) ) ;
#12792 = CARTESIAN_POINT ( 'NONE',  ( -0.3996062992125986590, 0.1070741851644051723, -2.471784776902887337 ) ) ;
#12793 = CARTESIAN_POINT ( 'NONE',  ( 0.4724409448818904789, -0.1870078740157479769, 0.4822834645669291653 ) ) ;
#12794 = CARTESIAN_POINT ( 'NONE',  ( 1.049868766404200127, -0.5023911411419708095, -0.1820866141732282451 ) ) ;
#12795 = CARTESIAN_POINT ( 'NONE',  ( -0.4658792650918627265, -0.3162353388693409650, -0.4822834645669289433 ) ) ;
#12796 = CARTESIAN_POINT ( 'NONE',  ( 0.4790026246719167324, -0.05778040916215522460, 0.4822834645669289988 ) ) ;
#12797 = CARTESIAN_POINT ( 'NONE',  ( -0.1998031496062994683, 0.3460692066303958092, -2.060367454068241511 ) ) ;
#12798 = AXIS2_PLACEMENT_3D ( 'NONE', #44862, #25520, #79397 ) ;
#12799 = CARTESIAN_POINT ( 'NONE',  ( 4.837279021331060870E-17, -0.3949938075777409963, -1.653543307086614123 ) ) ;
#12800 = CARTESIAN_POINT ( 'NONE',  ( 0.3996062992125986035, 2.446882876249141962E-17, -2.795275590551181022 ) ) ;
#12801 = CARTESIAN_POINT ( 'NONE',  ( 0.1265901696524989184, 0.4724409448818898127, -2.513123359580052174 ) ) ;
#12802 = CARTESIAN_POINT ( 'NONE',  ( -0.3392501089628017219, -0.1958661417322836718, -1.146981627296587813 ) ) ;
#12803 = CARTESIAN_POINT ( 'NONE',  ( -1.141732283464566011, -0.5511811023622047445, 6.969142054262312111E-17 ) ) ;
#12804 = CARTESIAN_POINT ( 'NONE',  ( -1.062992125984250968, 0.2952755905511811885, 0.000000000000000000 ) ) ;
#12805 = B_SPLINE_CURVE_WITH_KNOTS ( 'NONE', 3,
 ( #67798, #61466, #10549, #36207, #81673, #56379, #23984 ),
 .UNSPECIFIED., .F., .F.,
 ( 4, 3, 4 ),
 ( 1.734723475976807094E-18, 0.001246232571205268744, 0.002492492258783275856 ),
 .UNSPECIFIED. ) ;
#12806 = CARTESIAN_POINT ( 'NONE',  ( 0.3949938075777409963, 2.418639510665530743E-17, -2.557086614173228689 ) ) ;
#12807 = CARTESIAN_POINT ( 'NONE',  ( 0.6692913385826778638, -0.6692913385826771977, 8.415575281601705876E-17 ) ) ;
#12808 = CARTESIAN_POINT ( 'NONE',  ( 1.292650918635171564, 0.2952755905511811885, 0.1292274648535926551 ) ) ;
#12809 = CARTESIAN_POINT ( 'NONE',  ( 0.8070866141732288002, 0.1660481256975885056, 0.3530559997133364547 ) ) ;
#12810 = CARTESIAN_POINT ( 'NONE',  ( -2.787279214012418738, 0.000000000000000000, 0.000000000000000000 ) ) ;
#12811 = CARTESIAN_POINT ( 'NONE',  ( 0.3996062992125986035, 2.446882876249141962E-17, -2.007874015748031482 ) ) ;
#12812 = CARTESIAN_POINT ( 'NONE',  ( -0.1049643490035302301, -0.3917322834645671770, -0.8563185283802644543 ) ) ;
#12813 = DIRECTION ( 'NONE',  ( -0.000000000000000000, -1.000000000000000000, -0.000000000000000000 ) ) ;
#12814 = CARTESIAN_POINT ( 'NONE',  ( 0.5118110236220478892, 0.2952755905511811885, 0.000000000000000000 ) ) ;
#12815 = CARTESIAN_POINT ( 'NONE',  ( 0.4921259842519691285, 0.1660481256975885056, 0.3530559997133364547 ) ) ;
#12816 = CARTESIAN_POINT ( 'NONE',  ( 0.8267716535433077274, 0.1771653543307087630, 0.000000000000000000 ) ) ;
#12817 = CARTESIAN_POINT ( 'NONE',  ( 1.423884514435696413, -0.3162353388693409650, -0.4822834645669289433 ) ) ;
#12818 = CARTESIAN_POINT ( 'NONE',  ( -0.2867679344610365999, 0.2867679344610364889, 0.05314960629921249707 ) ) ;
#12819 = CARTESIAN_POINT ( 'NONE',  ( 0.4330708661417329575, -0.6692913385826771977, 8.415575281601705876E-17 ) ) ;
#12820 = CARTESIAN_POINT ( 'NONE',  ( 0.9711286089238851948, -0.6046776061558809534, -0.2411417322834644161 ) ) ;
#12821 = CARTESIAN_POINT ( 'NONE',  ( 0.5314960629921267055, -0.5400638737290844871, 0.3530559997133364547 ) ) ;
#12822 = CARTESIAN_POINT ( 'NONE',  ( 1.089238845144357759, -0.004921259842519870586, -0.3153832671262229437 ) ) ;
#12823 = CARTESIAN_POINT ( 'NONE',  ( -0.9776902887139098386, -0.6692913385826771977, 0.1292274648535927661 ) ) ;
#12824 = CARTESIAN_POINT ( 'NONE',  ( -0.8136482939632537770, -0.6046776061558807314, 0.2411417322834647770 ) ) ;
#12825 = CARTESIAN_POINT ( 'NONE',  ( 1.358267716535433323, -0.5400638737290845981, -0.3530559997133363437 ) ) ;
#12826 = CARTESIAN_POINT ( 'NONE',  ( 0.3392501089628018329, 0.1958661417322835607, -0.5308398950131234528 ) ) ;
#12827 = CARTESIAN_POINT ( 'NONE',  ( 0.3917322834645670104, 2.398668435337828261E-17, -1.685039370078740051 ) ) ;
#12828 = CARTESIAN_POINT ( 'NONE',  ( -0.3392501089628017219, -0.1958661417322836718, -2.721784776902886893 ) ) ;
#12829 = VERTEX_POINT ( 'NONE', #32518 ) ;
#12830 = CARTESIAN_POINT ( 'NONE',  ( -0.3460692066303958092, -0.1998031496062994683, -0.2099737532808399199 ) ) ;
#12831 = VERTEX_POINT ( 'NONE', #50209 ) ;
#12832 = CARTESIAN_POINT ( 'NONE',  ( 1.673228346456693494, 0.1660481256975885056, 0.3530559997133364547 ) ) ;
#12833 = CARTESIAN_POINT ( 'NONE',  ( 0.9186351706036751663, -0.5023911411419708095, 0.1820866141732285504 ) ) ;
#12834 = CARTESIAN_POINT ( 'NONE',  ( 0.3460692066303959202, 0.1998031496062993295, -1.548556430446194287 ) ) ;
#12835 = CARTESIAN_POINT ( 'NONE',  ( 1.272965879265092637, -0.3690944881889765550, -0.3153832671262227771 ) ) ;
#12836 = PLANE ( 'NONE',  #74752 ) ;
#12837 = DIRECTION ( 'NONE',  ( 0.000000000000000000, 1.000000000000000000, 0.000000000000000000 ) ) ;
#12838 = CARTESIAN_POINT ( 'NONE',  ( -1.473278426072732739, 0.2335363939278404244, -0.2780995266831706170 ) ) ;
#12839 = CARTESIAN_POINT ( 'NONE',  ( 0.3917322834645669549, 0.1049643490035304660, -0.9967191601049870675 ) ) ;
#12840 = CARTESIAN_POINT ( 'NONE',  ( -0.6364829396325453192, -0.08942795157528024563, -0.3641732283464568787 ) ) ;
#12841 = CARTESIAN_POINT ( 'NONE',  ( -1.489501312335957062, -0.2845877964562161244, -0.3641732283464567121 ) ) ;
#12842 = CARTESIAN_POINT ( 'NONE',  ( -1.476377952755905110, 0.1660481256975885056, 0.3530559997133364547 ) ) ;
#12843 = CARTESIAN_POINT ( 'NONE',  ( -0.03937007874015669567, -0.6692913385826771977, 8.415575281601705876E-17 ) ) ;
#12844 = CARTESIAN_POINT ( 'NONE',  ( -1.561679790026246017, -0.4281496062992127816, -0.4176697321401328100 ) ) ;
#12845 = EDGE_LOOP ( 'NONE', ( #74539, #1864, #40348, #76061, #80857 ) ) ;
#12846 = DIRECTION ( 'NONE',  ( 0.000000000000000000, -1.000000000000000000, 0.000000000000000000 ) ) ;
#12847 = DIRECTION ( 'NONE',  ( 0.000000000000000000, 1.000000000000000000, 0.000000000000000000 ) ) ;
#12848 = CARTESIAN_POINT ( 'NONE',  ( 0.1265901696524989462, 0.4724409448818897572, -2.040682414698162361 ) ) ;
#12849 = FACE_OUTER_BOUND ( 'NONE', #24694, .T. ) ;
#12850 = CARTESIAN_POINT ( 'NONE',  ( -0.6955380577427815458, -0.004921259842519576551, 0.3153832671262227771 ) ) ;
#12851 = EDGE_CURVE ( 'NONE', #38184, #69360, #39606, .T. ) ;
#12852 = CARTESIAN_POINT ( 'NONE',  ( -1.089238845144356427, -0.4281496062992127816, -0.4176697321401328100 ) ) ;
#12853 = CARTESIAN_POINT ( 'NONE',  ( 1.220472440944882608, 0.2952755905511811885, 0.000000000000000000 ) ) ;
#12854 = ORIENTED_EDGE ( 'NONE', *, *, #845, .T. ) ;
#12856 = DIRECTION ( 'NONE',  ( -1.000000000000000000, -0.000000000000000000, -0.000000000000000000 ) ) ;
#12855 = DIRECTION ( 'NONE',  ( -0.000000000000000000, -1.000000000000000000, -0.000000000000000000 ) ) ;
#12857 = CARTESIAN_POINT ( 'NONE',  ( 1.030183727034121421, -0.05778040916215522460, 0.4822834645669289988 ) ) ;
#12858 = CARTESIAN_POINT ( 'NONE',  ( -1.161417322834644716, -0.5400638737290845981, -0.3530559997133363437 ) ) ;
#12859 = CARTESIAN_POINT ( 'NONE',  ( -0.1049643490035306742, 0.3917322834645668994, -0.7165161172890270880 ) ) ;
#12860 = ADVANCED_FACE ( 'NONE', ( #24545 ), #44705, .T. ) ;
#12861 = CARTESIAN_POINT ( 'NONE',  ( -0.2493438320209966919, -0.004921259842519870586, -0.3153832671262229437 ) ) ;
#12862 = CARTESIAN_POINT ( 'NONE',  ( -0.2867679344610366554, 0.2867679344610365444, -0.8917322834645667884 ) ) ;
#12863 = CARTESIAN_POINT ( 'NONE',  ( -0.6102362204724400829, -0.4536011799217368745, -0.2665933059059886201 ) ) ;
#12864 = CARTESIAN_POINT ( 'NONE',  ( -0.05249343832020938322, -0.5023911411419708095, -0.1820866141732282451 ) ) ;
#12865 = CARTESIAN_POINT ( 'NONE',  ( 0.1509186351706042484, -0.3162353388693405765, 0.4822834645669290543 ) ) ;
#12866 = CARTESIAN_POINT ( 'NONE',  ( -0.9776902887139098386, 0.1771653543307087075, -0.09757992244046823083 ) ) ;
#12867 = CARTESIAN_POINT ( 'NONE',  ( 0.3392501089628018329, 0.1958661417322835607, -2.800524934383201714 ) ) ;
#12868 = CARTESIAN_POINT ( 'NONE',  ( 1.030183727034121421, -0.3162353388693409650, -0.4822834645669289433 ) ) ;
#12869 = CARTESIAN_POINT ( 'NONE',  ( -1.377952755905511140, -0.6692913385826771977, 8.415575281601705876E-17 ) ) ;
#12870 = CARTESIAN_POINT ( 'NONE',  ( -0.4091458600556402980, -0.2362204724409451284, -1.231627296587926468 ) ) ;
#12871 = CARTESIAN_POINT ( 'NONE',  ( -0.4068241469816267775, 0.05413385826771626580, -0.4176697321401330321 ) ) ;
#12872 = CARTESIAN_POINT ( 'NONE',  ( -0.9317585301837263412, -0.4281496062992127816, -0.4176697321401328100 ) ) ;
#12873 = CARTESIAN_POINT ( 'NONE',  ( 0.6430446194225729606, -0.3690944881889765550, -0.3153832671262227771 ) ) ;
#12874 = CARTESIAN_POINT ( 'NONE',  ( -0.4855643044619415427, -0.3690944881889763329, 0.3153832671262228327 ) ) ;
#12875 = CARTESIAN_POINT ( 'NONE',  ( -0.5249343832020990641, -0.6046776061558809534, -0.2411417322834644161 ) ) ;
#12876 = CARTESIAN_POINT ( 'NONE',  ( -1.338582677165353729, -0.1870078740157479769, 0.4822834645669291653 ) ) ;
#12877 = PLANE ( 'NONE',  #40726 ) ;
#12878 = CARTESIAN_POINT ( 'NONE',  ( 1.272965879265092637, -0.3690944881889765550, -0.3153832671262227771 ) ) ;
#12879 = CARTESIAN_POINT ( 'NONE',  ( -0.3543307086614165824, 0.2952755905511811885, 0.000000000000000000 ) ) ;
#12880 = CARTESIAN_POINT ( 'NONE',  ( -1.535433070866141225, 0.2952755905511811885, 0.000000000000000000 ) ) ;
#12881 = ORIENTED_EDGE ( 'NONE', *, *, #13568, .F. ) ;
#12882 = CARTESIAN_POINT ( 'NONE',  ( 0.1070741851644053388, 0.3996062992125986035, -2.274934383202099397 ) ) ;
#12883 = CARTESIAN_POINT ( 'NONE',  ( -0.8727034120734901146, -0.2845877964562159024, 0.3641732283464567677 ) ) ;
#12884 = CARTESIAN_POINT ( 'NONE',  ( 0.7152230971128614723, -0.3162353388693409650, -0.4822834645669289433 ) ) ;
#12885 = CARTESIAN_POINT ( 'NONE',  ( -1.194225721784776262, -0.004921259842519870586, -0.3153832671262229437 ) ) ;
#12886 = CARTESIAN_POINT ( 'NONE',  ( -0.3996062992125984925, -0.1070741851644056858, -1.225065616797899937 ) ) ;
#12887 = CARTESIAN_POINT ( 'NONE',  ( -1.069553805774277722, 0.2952755905511811885, 0.1292274648535926551 ) ) ;
#12888 = AXIS2_PLACEMENT_3D ( 'NONE', #46599, #52068, #60067 ) ;
#12889 = CARTESIAN_POINT ( 'NONE',  ( 0.7349081364829403995, 0.2306618581243848609, 0.2411417322834645549 ) ) ;
#12890 = CARTESIAN_POINT ( 'NONE',  ( 0.2821522309711292364, 0.2952755905511810774, -0.1292274648535930714 ) ) ;
#12891 = CARTESIAN_POINT ( 'NONE',  ( 1.587926509186352142, 0.05413385826771666132, 0.4176697321401328100 ) ) ;
#12892 = CARTESIAN_POINT ( 'NONE',  ( -1.463254593175852492, -0.5511811023622048555, -0.09757992244046775898 ) ) ;
#12893 = CARTESIAN_POINT ( 'NONE',  ( 0.3996062992125985480, 2.446882876249141654E-17, -0.6673228346456693272 ) ) ;
#12894 = CARTESIAN_POINT ( 'NONE',  ( 0.1998031496062992740, 0.3460692066303959757, -0.7742782152230971437 ) ) ;
#12895 = CARTESIAN_POINT ( 'NONE',  ( -0.2891555358219911054, 0.2891555358219909388, -0.3346456692913387099 ) ) ;
#12896 = LINE ( 'NONE', #38555, #80452 ) ;
#12897 = CARTESIAN_POINT ( 'NONE',  ( 1.279527559055118724, -0.4536011799217368745, -0.2665933059059886201 ) ) ;
#12898 = CARTESIAN_POINT ( 'NONE',  ( 0.1049868766404206816, -0.5023911411419708095, -0.1820866141732282451 ) ) ;
#12899 = CARTESIAN_POINT ( 'NONE',  ( 0.09186351706036799403, -0.4281496062992127816, -0.4176697321401328100 ) ) ;
#12900 = CARTESIAN_POINT ( 'NONE',  ( 1.417322834645670104, -0.1870078740157479769, 0.4822834645669291653 ) ) ;
#12901 = CARTESIAN_POINT ( 'NONE',  ( 0.1974969037888706092, -0.3420746716998660508, -1.270997375328083878 ) ) ;
#12902 = CARTESIAN_POINT ( 'NONE',  ( 0.4265091863517067594, 0.1771653543307087630, 0.09757992244046791164 ) ) ;
#12903 = CARTESIAN_POINT ( 'NONE',  ( -0.5708661417322825615, -0.5400638737290844871, 0.3530559997133364547 ) ) ;
#12904 = CARTESIAN_POINT ( 'NONE',  ( -1.122047244094487306, 0.1660481256975883668, -0.3530559997133364547 ) ) ;
#12905 = CARTESIAN_POINT ( 'NONE',  ( 0.6758530183727039509, -0.6692913385826771977, 0.1292274648535927661 ) ) ;
#12906 = CARTESIAN_POINT ( 'NONE',  ( 0.2362204724409451007, -0.4091458600556402980, -1.666666666666666741 ) ) ;
#12907 = CARTESIAN_POINT ( 'NONE',  ( -0.3996062992125986035, -7.340648628747425578E-17, -2.559055118110236560 ) ) ;
#12908 = AXIS2_PLACEMENT_3D ( 'NONE', #12734, #51004, #19036 ) ;
#12909 = ORIENTED_EDGE ( 'NONE', *, *, #30460, .T. ) ;
#12910 = ORIENTED_EDGE ( 'NONE', *, *, #71814, .T. ) ;
#12911 = CARTESIAN_POINT ( 'NONE',  ( -1.108923884514435132, -0.3162353388693405765, 0.4822834645669290543 ) ) ;
#12912 = EDGE_CURVE ( 'NONE', #66112, #199, #51440, .T. ) ;
#12913 = CARTESIAN_POINT ( 'NONE',  ( -0.5380577427821514602, 0.05413385826771666132, 0.4176697321401328100 ) ) ;
#12915 = CARTESIAN_POINT ( 'NONE',  ( -0.5446194225721777693, -0.05778040916215522460, 0.4822834645669289988 ) ) ;
#12914 = CARTESIAN_POINT ( 'NONE',  ( -0.6627296587926501115, 0.1771653543307087075, -0.09757992244046823083 ) ) ;
#12916 = CARTESIAN_POINT ( 'NONE',  ( 0.1049643490035304522, -0.3917322834645668994, -1.897618479493751398 ) ) ;
#12917 = CARTESIAN_POINT ( 'NONE',  ( 0.1070741851644053388, 0.3996062992125986035, -2.747375328083988766 ) ) ;
#12918 = CARTESIAN_POINT ( 'NONE',  ( -1.555118110236219930, -0.4536011799217368745, -0.2665933059059886201 ) ) ;
#12919 = CARTESIAN_POINT ( 'NONE',  ( -1.305774278215222184, -0.6692913385826773087, -0.1292274648535924053 ) ) ;
#12920 = CARTESIAN_POINT ( 'NONE',  ( 0.4921259842519691285, 0.1660481256975885056, 0.3530559997133364547 ) ) ;
#12921 = CARTESIAN_POINT ( 'NONE',  ( -0.9448818897637790704, -0.1870078740157480879, -0.4822834645669291653 ) ) ;
#12922 = CARTESIAN_POINT ( 'NONE',  ( -0.1958661417322834220, -0.3392501089628018884, -1.632545931758530244 ) ) ;
#12923 = CARTESIAN_POINT ( 'NONE',  ( -0.8661417322834640276, -0.1870078740157479769, 0.3641732283464567677 ) ) ;
#12924 = ORIENTED_EDGE ( 'NONE', *, *, #33021, .T. ) ;
#12925 = CARTESIAN_POINT ( 'NONE',  ( -0.1058382717557503211, 0.3949938075777409408, -1.896325459317585116 ) ) ;
#12926 = VERTEX_POINT ( 'NONE', #69585 ) ;
#12927 = CARTESIAN_POINT ( 'NONE',  ( -1.614173228346456268, -0.5511811023622047445, 6.969142054262312111E-17 ) ) ;
#12928 = CARTESIAN_POINT ( 'NONE',  ( -1.023622047244093558, -0.1870078740157479769, 0.4822834645669291653 ) ) ;
#12929 = CARTESIAN_POINT ( 'NONE',  ( -0.8267716535433065062, 0.2952755905511811885, 0.000000000000000000 ) ) ;
#12930 = CARTESIAN_POINT ( 'NONE',  ( -0.3460692066303958092, -0.1998031496062994683, -0.2099737532808398921 ) ) ;
#12931 = CARTESIAN_POINT ( 'NONE',  ( -1.266404199475064773, -0.3162353388693405765, 0.4822834645669290543 ) ) ;
#12932 = CARTESIAN_POINT ( 'NONE',  ( -1.082677165354329896, 0.1660481256975885056, 0.3530559997133364547 ) ) ;
#12933 =( CONVERSION_BASED_UNIT ( 'INCH', #26382 ) LENGTH_UNIT ( ) NAMED_UNIT ( #56145 ) );
#12934 = CARTESIAN_POINT ( 'NONE',  ( -0.8267716535433065062, 0.2952755905511811885, 0.000000000000000000 ) ) ;
#12935 = B_SPLINE_CURVE_WITH_KNOTS ( 'NONE', 3,
 ( #66013, #14262, #2456, #59265, #52525, #33189, #8350, #53363, #78231, #39920, #20565, #66848 ),
 .UNSPECIFIED., .F., .F.,
 ( 4, 2, 2, 2, 2, 4 ),
 ( 0.04729187226826446488, 0.04795755069747583560, 0.04862322912668719938, 0.04995458598510991305, 0.05128594284353263366, 0.05261729970195534734 ),
 .UNSPECIFIED. ) ;
#12936 = CARTESIAN_POINT ( 'NONE',  ( 0.4133858267716541968, 0.07958543189024085140, 0.2665933059059887866 ) ) ;
#12937 = DIRECTION ( 'NONE',  ( -1.000000000000000000, -3.469446951953613696E-16, 0.000000000000000000 ) ) ;
#12938 = CARTESIAN_POINT ( 'NONE',  ( -0.3917322834645671215, 0.1049643490035301469, -0.4324146981627298159 ) ) ;
#12939 = CARTESIAN_POINT ( 'NONE',  ( -0.3018372703412066094, -0.004921259842519576551, 0.3153832671262227771 ) ) ;
#12940 = CARTESIAN_POINT ( 'NONE',  ( -0.9317585301837263412, -0.4281496062992127816, -0.4176697321401328100 ) ) ;
#12941 = CARTESIAN_POINT ( 'NONE',  ( 1.259842519685040019, -0.1870078740157479769, 0.4822834645669291653 ) ) ;
#12942 = CARTESIAN_POINT ( 'NONE',  ( -0.5971128608923877978, -0.6692913385826773087, -0.1292274648535924053 ) ) ;
#12943 = CARTESIAN_POINT ( 'NONE',  ( 0.5314960629921393620, 2.755905511811024056, -3.821484228344191880 ) ) ;
#12944 = ORIENTED_EDGE ( 'NONE', *, *, #82633, .T. ) ;
#12945 = CARTESIAN_POINT ( 'NONE',  ( -0.3460692066303960313, 0.1998031496062989965, -1.992782152230971437 ) ) ;
#12946 = CARTESIAN_POINT ( 'NONE',  ( -0.7939632545931750718, -0.05778040916215560624, -0.4822834645669293319 ) ) ;
#12947 = CARTESIAN_POINT ( 'NONE',  ( 1.325459317585302665, 0.05413385826771626580, -0.4176697321401330321 ) ) ;
#12948 = CARTESIAN_POINT ( 'NONE',  ( -1.082677165354329896, 0.07958543189024085140, 0.2665933059059887866 ) ) ;
#12949 = CARTESIAN_POINT ( 'NONE',  ( -1.568241469816272105, -0.05778040916215522460, 0.4822834645669289988 ) ) ;
#12950 = CARTESIAN_POINT ( 'NONE',  ( 0.1265901696524990294, -0.4724409448818896462, -0.8727034120734907807 ) ) ;
#12951 = CARTESIAN_POINT ( 'NONE',  ( 2.170146923806594685, 1.528804020127597640, 0.4744094488188974612 ) ) ;
#12952 = CARTESIAN_POINT ( 'NONE',  ( -0.2867679344610364334, -0.2867679344610367109, -0.5236220472440944462 ) ) ;
#12953 = DIRECTION ( 'NONE',  ( -3.491481338843133355E-15, -0.000000000000000000, 1.000000000000000000 ) ) ;
#12954 = CARTESIAN_POINT ( 'NONE',  ( 0.1246719160104994284, 0.2952755905511810774, -0.1292274648535930714 ) ) ;
#12955 = CARTESIAN_POINT ( 'NONE',  ( -1.076115485564303809, -0.5023911411419708095, -0.1820866141732282451 ) ) ;
#12956 = CIRCLE ( 'NONE', #21007, 0.5120078740157480990 ) ;
#12957 = CARTESIAN_POINT ( 'NONE',  ( -0.6627296587926503335, -0.6692913385826771977, 0.1292274648535927661 ) ) ;
#12958 = CARTESIAN_POINT ( 'NONE',  ( 0.4724409448818897572, -0.1265901696524988906, -2.865485564304462329 ) ) ;
#12959 = CARTESIAN_POINT ( 'NONE',  ( -1.233595800524933894, 0.2306618581243848609, 0.2411417322834645549 ) ) ;
#12960 = CARTESIAN_POINT ( 'NONE',  ( -1.043307086614172707, 0.1660481256975883668, -0.3530559997133364547 ) ) ;
#12961 = CARTESIAN_POINT ( 'NONE',  ( 0.006561679790026889343, -0.05778040916215522460, 0.4822834645669289988 ) ) ;
#12962 = CARTESIAN_POINT ( 'NONE',  ( 0.1974969037888706092, -0.3420746716998660508, -2.530839895013123453 ) ) ;
#12963 = CARTESIAN_POINT ( 'NONE',  ( 0.8792650918635177559, -0.3690944881889765550, -0.3153832671262227771 ) ) ;
#12964 = CARTESIAN_POINT ( 'NONE',  ( -0.5708661417322828946, 0.07958543189024071263, -0.2665933059059888421 ) ) ;
#12965 = CARTESIAN_POINT ( 'NONE',  ( -0.1092078379430496404, 1.075719315424584543, -1.514693649293256117 ) ) ;
#12966 = CARTESIAN_POINT ( 'NONE',  ( 0.6955380577427828781, -0.3690944881889763329, 0.3153832671262228327 ) ) ;
#12967 = CARTESIAN_POINT ( 'NONE',  ( 1.174540682414699111, -0.08942795157528024563, -0.3641732283464568787 ) ) ;
#12968 = CARTESIAN_POINT ( 'NONE',  ( 1.404199475065617264, -0.4281496062992124485, 0.4176697321401328655 ) ) ;
#12969 = CARTESIAN_POINT ( 'NONE',  ( 0.3608923884514443348, -0.5511811023622046335, 0.09757992244046803654 ) ) ;
#12970 = CARTESIAN_POINT ( 'NONE',  ( 0.3917322834645670104, 2.398668435337828261E-17, -1.685039370078740051 ) ) ;
#12971 = CARTESIAN_POINT ( 'NONE',  ( -0.9383202099737524282, -0.3162353388693409650, -0.4822834645669289433 ) ) ;
#12972 = CARTESIAN_POINT ( 'NONE',  ( 1.292650918635171564, 0.2952755905511811885, 0.1292274648535926551 ) ) ;
#12973 = AXIS2_PLACEMENT_3D ( 'NONE', #74771, #5290, #56213 ) ;
#12974 = CARTESIAN_POINT ( 'NONE',  ( -0.4091458600556402980, -0.2362204724409451284, -0.1292650918635170620 ) ) ;
#12975 = CARTESIAN_POINT ( 'NONE',  ( -0.6430446194225712953, -0.004921259842519870586, -0.3153832671262229437 ) ) ;
#12976 = CARTESIAN_POINT ( 'NONE',  ( 0.02624671916010564918, 0.2306618581243848609, 0.2411417322834645549 ) ) ;
#12977 = CARTESIAN_POINT ( 'NONE',  ( 0.4921259842519691285, -0.5400638737290845981, -0.3530559997133363437 ) ) ;
#12978 = DIRECTION ( 'NONE',  ( 0.000000000000000000, -1.000000000000000000, -0.000000000000000000 ) ) ;
#12979 = CARTESIAN_POINT ( 'NONE',  ( 1.095800524934383846, -0.2845877964562159024, 0.3641732283464567677 ) ) ;
#12980 = CARTESIAN_POINT ( 'NONE',  ( 0.03280839895013198948, 0.1771653543307087630, 0.09757992244046791164 ) ) ;
#12981 = CARTESIAN_POINT ( 'NONE',  ( 0.07217847769028949700, -0.3162353388693405765, 0.4822834645669290543 ) ) ;
#12982 = CARTESIAN_POINT ( 'NONE',  ( -1.489501312335957062, -0.3162353388693409650, -0.4822834645669289433 ) ) ;
#12983 = CARTESIAN_POINT ( 'NONE',  ( -0.6627296587926501115, 0.1771653543307087075, -0.09757992244046823083 ) ) ;
#12984 = FACE_OUTER_BOUND ( 'NONE', #29777, .T. ) ;
#12985 = ADVANCED_FACE ( 'NONE', ( #75500 ), #11931, .F. ) ;
#12986 = CARTESIAN_POINT ( 'NONE',  ( -0.4921259842519677963, 0.1660481256975883668, -0.3530559997133364547 ) ) ;
#12987 = CARTESIAN_POINT ( 'NONE',  ( 0.1998031496062992463, 0.3460692066303959202, -1.323490813648294129 ) ) ;
#12988 = CARTESIAN_POINT ( 'NONE',  ( 0.3392501089628018884, -0.1958661417322834220, -2.551837270341207109 ) ) ;
#12989 = CARTESIAN_POINT ( 'NONE',  ( 0.3477690288713918276, 0.1771653543307087630, 0.09757992244046791164 ) ) ;
#12990 = CARTESIAN_POINT ( 'NONE',  ( -0.8727034120734901146, -0.3162353388693405765, 0.4822834645669290543 ) ) ;
#12991 = CARTESIAN_POINT ( 'NONE',  ( -1.056430446194224881, -0.6692913385826771977, 0.1292274648535927661 ) ) ;
#12992 = CARTESIAN_POINT ( 'NONE',  ( -1.194225721784776262, -0.3690944881889763329, 0.3153832671262228327 ) ) ;
#12993 = LINE ( 'NONE', #52516, #6447 ) ;
#12994 = CARTESIAN_POINT ( 'NONE',  ( -0.5511811023622038563, -0.1870078740157479769, 0.4822834645669291653 ) ) ;
#12995 = CARTESIAN_POINT ( 'NONE',  ( -0.7611548556430438595, -0.5023911411419708095, -0.1820866141732282451 ) ) ;
#12996 = CARTESIAN_POINT ( 'NONE',  ( -1.699475065616797398, 0.1771653543307087630, 0.09757992244046791164 ) ) ;
#12997 = CARTESIAN_POINT ( 'NONE',  ( 1.384514435695538337, -0.6692913385826771977, 0.1292274648535927661 ) ) ;
#12998 = CARTESIAN_POINT ( 'NONE',  ( 0.3458507752293908943, -0.3458507752293908943, -0.7283464566929134243 ) ) ;
#12999 = CARTESIAN_POINT ( 'NONE',  ( -0.3917322834645670104, -0.1049643490035307020, -2.089914328905198904 ) ) ;
#13000 = ORIENTED_EDGE ( 'NONE', *, *, #52169, .F. ) ;
#13001 = DIRECTION ( 'NONE',  ( 0.000000000000000000, -1.000000000000000000, -0.000000000000000000 ) ) ;
#13002 = CARTESIAN_POINT ( 'NONE',  ( -1.404199475065615932, 0.05413385826771666132, 0.4176697321401328100 ) ) ;
#13003 = CARTESIAN_POINT ( 'NONE',  ( -0.8070866141732276899, -0.5400638737290844871, 0.3530559997133364547 ) ) ;
#13004 = CARTESIAN_POINT ( 'NONE',  ( -1.528871391076114250, -0.6692913385826771977, 0.1292274648535927661 ) ) ;
#13005 = CARTESIAN_POINT ( 'NONE',  ( -0.3917322834645671215, 0.1049643490035301469, -2.164698162729658648 ) ) ;
#13006 = CARTESIAN_POINT ( 'NONE',  ( 1.607611548556431069, -0.5511811023622048555, -0.09757992244046775898 ) ) ;
#13007 = EDGE_CURVE ( 'NONE', #25136, #58442, #83040, .T. ) ;
#13008 = CARTESIAN_POINT ( 'NONE',  ( 0.4855643044619430415, -0.4281496062992127816, -0.4176697321401328100 ) ) ;
#13009 = CARTESIAN_POINT ( 'NONE',  ( 0.07217847769028949700, -0.3162353388693405765, 0.4822834645669290543 ) ) ;
#13010 = CYLINDRICAL_SURFACE ( 'NONE', #36887, 0.4724409448818898682 ) ;
#13011 = AXIS2_PLACEMENT_3D ( 'NONE', #63673, #53538, #52284 ) ;
#13012 = AXIS2_PLACEMENT_3D ( 'NONE', #54652, #54233, #22263 ) ;
#13013 = CARTESIAN_POINT ( 'NONE',  ( 0.7480314960629927956, -0.5511811023622047445, 6.969142054262312111E-17 ) ) ;
#13014 = CARTESIAN_POINT ( 'NONE',  ( 0.1070741851644054915, -0.3996062992125986035, -1.345144356955380704 ) ) ;
#13015 = ORIENTED_EDGE ( 'NONE', *, *, #50027, .F. ) ;
#13016 = CARTESIAN_POINT ( 'NONE',  ( -0.2867679344610367109, 0.2867679344610365444, 0.1410567997037251442 ) ) ;
#13017 = VERTEX_POINT ( 'NONE', #31685 ) ;
#13018 = CARTESIAN_POINT ( 'NONE',  ( -0.07217847769028813698, -0.3162353388693409650, -0.4822834645669289433 ) ) ;
#13019 = CARTESIAN_POINT ( 'NONE',  ( -0.6364829396325453192, -0.3162353388693405765, 0.4822834645669290543 ) ) ;
#13020 = CARTESIAN_POINT ( 'NONE',  ( -1.482939632545930975, 0.05413385826771666132, 0.4176697321401328100 ) ) ;
#13021 = CARTESIAN_POINT ( 'NONE',  ( 0.6561679790026253567, -0.6046776061558809534, -0.2411417322834644161 ) ) ;
#13022 = CARTESIAN_POINT ( 'NONE',  ( -1.633858267716534529, 0.07958543189024085140, 0.2665933059059887866 ) ) ;
#13023 = CARTESIAN_POINT ( 'NONE',  ( 1.227034120734908917, -0.6692913385826771977, 0.1292274648535927661 ) ) ;
#13024 = CARTESIAN_POINT ( 'NONE',  ( -0.4658792650918627265, -0.3162353388693409650, -0.4822834645669289433 ) ) ;
#13025 = CARTESIAN_POINT ( 'NONE',  ( 0.4790026246719167324, -0.05778040916215522460, 0.4822834645669289988 ) ) ;
#13026 = CARTESIAN_POINT ( 'NONE',  ( 1.541994750656168645, -0.6692913385826771977, 0.1292274648535927661 ) ) ;
#13027 = CARTESIAN_POINT ( 'NONE',  ( 1.122047244094488860, 0.1660481256975885056, 0.3530559997133364547 ) ) ;
#13028 = CARTESIAN_POINT ( 'NONE',  ( 1.607611548556431069, -0.6692913385826773087, -0.1292274648535924053 ) ) ;
#13029 =( BOUNDED_CURVE ( )  B_SPLINE_CURVE ( 2, ( #20420, #27974, #648, #26726, #27557, #1897, #46488, #77671, #78512, #58708, #39349, #52380, #14541 ),
 .UNSPECIFIED., .F., .F. ) 
 B_SPLINE_CURVE_WITH_KNOTS ( ( 3, 2, 2, 2, 2, 2, 3 ),
 ( 0.2875000000000000333, 0.2916666666666667407, 0.2958333333333333925, 0.3000000000000000444, 0.3041666666666666408, 0.3083333333333333481, 0.3125000000000000000 ),
 .UNSPECIFIED. ) 
 CURVE ( )  GEOMETRIC_REPRESENTATION_ITEM ( )  RATIONAL_B_SPLINE_CURVE ( ( 0.9999999999999995559, 0.9659258262890687563, 1.000000000000000000, 0.9659258262890683122, 1.000000000000000000, 0.9659258262890683122, 1.000000000000000000, 0.9659258262890683122, 1.000000000000000000, 0.9659258262890683122, 1.000000000000000000, 0.9659258262890683122, 1.000000000000000000 ) ) 
 REPRESENTATION_ITEM ( '' )  );
#13030 = CARTESIAN_POINT ( 'NONE',  ( -0.1181102362204717315, 0.2952755905511811885, 0.000000000000000000 ) ) ;
#13031 = CARTESIAN_POINT ( 'NONE',  ( -0.3917322834645670104, -7.196005306013484475E-17, -0.3464566929133857665 ) ) ;
#13032 = CARTESIAN_POINT ( 'NONE',  ( 0.3412073490813655186, -0.5023911411419708095, -0.1820866141732282451 ) ) ;
#13033 = EDGE_LOOP ( 'NONE', ( #43711, #13139, #1921, #77840, #46885 ) ) ;
#13034 = CARTESIAN_POINT ( 'NONE',  ( 0.1058382717557499880, 0.3949938075777411073, -0.4658792650918635592 ) ) ;
#13035 = EDGE_LOOP ( 'NONE', ( #30710, #49518, #14708, #38124 ) ) ;
#13036 = CARTESIAN_POINT ( 'NONE',  ( -0.4921259842519677963, -0.4536011799217367080, 0.2665933059059888421 ) ) ;
#13037 = PLANE ( 'NONE',  #81130 ) ;
#13038 = CARTESIAN_POINT ( 'NONE',  ( 0.05249343832021075018, 0.2306618581243847221, -0.2411417322834647770 ) ) ;
#13039 = CARTESIAN_POINT ( 'NONE',  ( -0.1574803149606292529, -0.1870078740157479769, 0.4822834645669291653 ) ) ;
#13040 = CARTESIAN_POINT ( 'NONE',  ( -0.9186351706036736120, 0.2306618581243848609, 0.2411417322834645549 ) ) ;
#13041 = CARTESIAN_POINT ( 'NONE',  ( -0.2867679344610367109, 0.2867679344610365444, -1.748706979823833718 ) ) ;
#13042 = CARTESIAN_POINT ( 'NONE',  ( -1.154855643044618851, 0.2306618581243848609, 0.2411417322834645549 ) ) ;
#13043 = CARTESIAN_POINT ( 'NONE',  ( 0.02439311036560904908, 1.075073066373593234, 0.2372510453448407330 ) ) ;
#13044 = CARTESIAN_POINT ( 'NONE',  ( 0.9973753280839902091, 0.1283753931104746893, -0.1820866141732285504 ) ) ;
#13045 = CARTESIAN_POINT ( 'NONE',  ( 0.5708661417322842269, 0.1660481256975885056, 0.3530559997133364547 ) ) ;
#13046 = CARTESIAN_POINT ( 'NONE',  ( 0.8267716535433078384, -0.6692913385826771977, 8.415575281601705876E-17 ) ) ;
#13047 = CARTESIAN_POINT ( 'NONE',  ( -0.1998031496062994683, 0.3460692066303958092, -1.430446194225721834 ) ) ;
#13048 = CARTESIAN_POINT ( 'NONE',  ( -1.706036745406823485, 0.2306618581243848609, 0.2411417322834645549 ) ) ;
#13049 = CARTESIAN_POINT ( 'NONE',  ( -0.3460692066303960313, 0.1998031496062989965, -0.8904199475065617264 ) ) ;
#13050 = CARTESIAN_POINT ( 'NONE',  ( -0.3996062992125984925, -0.1070741851644056858, -0.2801837270341207553 ) ) ;
#13051 = CARTESIAN_POINT ( 'NONE',  ( -0.1640419947506555343, -0.3162353388693405765, 0.4822834645669290543 ) ) ;
#13052 = CARTESIAN_POINT ( 'NONE',  ( 0.2925321140481932369, 0.2925321140481932369, -2.657480314960630530 ) ) ;
#13053 = CARTESIAN_POINT ( 'NONE',  ( 0.1958661417322834775, 0.3392501089628018884, -1.488845144356955252 ) ) ;
#13054 = CARTESIAN_POINT ( 'NONE',  ( -1.279527559055116948, 0.07958543189024071263, -0.2665933059059888421 ) ) ;
#13055 = CARTESIAN_POINT ( 'NONE',  ( 1.194225721784777594, -0.4281496062992127816, -0.4176697321401328100 ) ) ;
#13056 = CARTESIAN_POINT ( 'NONE',  ( 1.482939632545932307, -0.4281496062992124485, 0.4176697321401328655 ) ) ;
#13057 = CARTESIAN_POINT ( 'NONE',  ( -0.006561679790025524116, -0.08942795157528024563, -0.3641732283464568787 ) ) ;
#13058 = CARTESIAN_POINT ( 'NONE',  ( 0.4199475065616803948, -0.6046776061558809534, -0.2411417322834644161 ) ) ;
#13059 = CARTESIAN_POINT ( 'NONE',  ( 0.4724409448818897572, -0.1265901696524988906, -1.605643044619422977 ) ) ;
#13060 = CARTESIAN_POINT ( 'NONE',  ( 0.4658792650918641698, -0.08942795157528024563, -0.3641732283464568787 ) ) ;
#13061 = CARTESIAN_POINT ( 'NONE',  ( 0.2952755905511816326, -0.5400638737290844871, 0.3530559997133364547 ) ) ;
#13062 = CARTESIAN_POINT ( 'NONE',  ( 0.1058382717557500852, -0.3949938075777408852, -1.421916010498688099 ) ) ;
#13063 = CARTESIAN_POINT ( 'NONE',  ( -1.371391076115484831, 0.2952755905511810774, -0.1292274648535930714 ) ) ;
#13064 = CARTESIAN_POINT ( 'NONE',  ( 0.6299212598425204535, -0.1870078740157479769, 0.3641732283464567677 ) ) ;
#13065 = CARTESIAN_POINT ( 'NONE',  ( 0.4768132735438208591, 1.796500554427756802, 0.5050878842330650542 ) ) ;
#13066 = CARTESIAN_POINT ( 'NONE',  ( -0.6102362204724400829, 0.1660481256975885056, 0.3530559997133364547 ) ) ;
#13067 = CARTESIAN_POINT ( 'NONE',  ( -0.3018372703412066094, -0.3690944881889765550, -0.3153832671262227771 ) ) ;
#13068 = CARTESIAN_POINT ( 'NONE',  ( -0.7080320533160963103, 1.900312960331933976, -0.5309055118110235227 ) ) ;
#13069 = CARTESIAN_POINT ( 'NONE',  ( -0.2296587926509179312, -0.3162353388693409650, -0.4822834645669289433 ) ) ;
#13070 = CARTESIAN_POINT ( 'NONE',  ( -0.1771653543307080136, 0.1660481256975883668, -0.3530559997133364547 ) ) ;
#13071 = CARTESIAN_POINT ( 'NONE',  ( 0.2427821522309716595, -0.2845877964562161244, -0.3641732283464567121 ) ) ;
#13072 = CIRCLE ( 'NONE', #19793, 0.4724409448818898682 ) ;
#13073 = CARTESIAN_POINT ( 'NONE',  ( -0.1998031496062994405, 0.3460692066303957537, -2.137139107611548905 ) ) ;
#13074 = CARTESIAN_POINT ( 'NONE',  ( -0.06561679790026180015, 0.05413385826771666132, 0.4176697321401328100 ) ) ;
#13075 = AXIS2_PLACEMENT_3D ( 'NONE', #48356, #74054, #30245 ) ;
#13077 = AXIS2_PLACEMENT_3D ( 'NONE', #69239, #4842, #37247 ) ;
#13076 = CARTESIAN_POINT ( 'NONE',  ( 0.3917322834645668994, -0.1049643490035303134, -1.766384883693226771 ) ) ;
#13078 = CARTESIAN_POINT ( 'NONE',  ( 1.220472440944882608, 0.1771653543307087630, 0.000000000000000000 ) ) ;
#13079 = CARTESIAN_POINT ( 'NONE',  ( 1.351706036745407458, -0.4281496062992127816, -0.4176697321401328100 ) ) ;
#13080 = CARTESIAN_POINT ( 'NONE',  ( -0.6692913385826764205, -0.5511811023622047445, 6.969142054262312111E-17 ) ) ;
#13081 = CARTESIAN_POINT ( 'NONE',  ( -0.5314960629921254842, -0.4536011799217368745, -0.2665933059059886201 ) ) ;
#13082 = CARTESIAN_POINT ( 'NONE',  ( -0.6561679790026240244, 0.2306618581243847221, -0.2411417322834647770 ) ) ;
#13083 = CARTESIAN_POINT ( 'NONE',  ( 0.006561679790026889343, -0.05778040916215522460, 0.4822834645669289988 ) ) ;
#13084 = CARTESIAN_POINT ( 'NONE',  ( 0.5183727034120741983, -0.5511811023622046335, 0.09757992244046803654 ) ) ;
#13085 = CARTESIAN_POINT ( 'NONE',  ( 0.4724409448818898682, 2.892866454678787531E-17, -2.322834645669291209 ) ) ;
#13086 = CARTESIAN_POINT ( 'NONE',  ( 1.115485564304462551, -0.004921259842519576551, 0.3153832671262227771 ) ) ;
#13087 = EDGE_CURVE ( 'NONE', #24482, #66439, #24541, .T. ) ;
#13088 = CARTESIAN_POINT ( 'NONE',  ( 0.7939632545931766261, -0.3162353388693409650, -0.4822834645669289433 ) ) ;
#13089 = CARTESIAN_POINT ( 'NONE',  ( -9.787531504996566615E-17, 0.3996062992125985480, 0.2381889763779527491 ) ) ;
#13090 = CARTESIAN_POINT ( 'NONE',  ( -0.1246719160104980823, 0.2952755905511811885, 0.1292274648535926551 ) ) ;
#13091 = CARTESIAN_POINT ( 'NONE',  ( 0.3392501089628018884, -0.1958661417322834220, -1.134514435695538115 ) ) ;
#13092 = CARTESIAN_POINT ( 'NONE',  ( 1.482939632545932307, -0.004921259842519870586, -0.3153832671262229437 ) ) ;
#13093 = CARTESIAN_POINT ( 'NONE',  ( 0.7349081364829403995, 0.2306618581243848609, 0.2411417322834645549 ) ) ;
#13094 = CARTESIAN_POINT ( 'NONE',  ( -0.07217847769028787330, -0.05778040916215522460, 0.4822834645669289988 ) ) ;
#13095 = FACE_OUTER_BOUND ( 'NONE', #35506, .T. ) ;
#13096 = CARTESIAN_POINT ( 'NONE',  ( 0.4724409448818904789, -0.1870078740157480601, -0.3641732283464567677 ) ) ;
#13097 = CARTESIAN_POINT ( 'NONE',  ( 0.7152230971128616943, -0.05778040916215522460, 0.4822834645669289988 ) ) ;
#13098 = CARTESIAN_POINT ( 'NONE',  ( -0.5183727034120726440, -0.5511811023622048555, -0.09757992244046775898 ) ) ;
#13099 = CARTESIAN_POINT ( 'NONE',  ( -0.9251968503937002541, -0.5400638737290845981, -0.3530559997133363437 ) ) ;
#13100 = CARTESIAN_POINT ( 'NONE',  ( 0.4658792650918640033, -0.3162353388693405765, 0.4822834645669290543 ) ) ;
#13101 = CARTESIAN_POINT ( 'NONE',  ( -1.391076115485563314, -0.6046776061558809534, -0.2411417322834644161 ) ) ;
#13102 = CARTESIAN_POINT ( 'NONE',  ( -0.5577427821522301654, -0.08942795157528024563, -0.3641732283464568787 ) ) ;
#13103 = CARTESIAN_POINT ( 'NONE',  ( 0.2362204724409456558, -0.1870078740157480879, -0.4822834645669291653 ) ) ;
#13104 = CARTESIAN_POINT ( 'NONE',  ( -1.332020997375327642, -0.3162353388693409650, -0.4822834645669289433 ) ) ;
#13105 = CARTESIAN_POINT ( 'NONE',  ( -0.3477690288713902178, 0.2952755905511810774, -0.1292274648535930714 ) ) ;
#13106 = CARTESIAN_POINT ( 'NONE',  ( 1.115485564304462551, 0.009842519685039463617, 0.3409548833797002576 ) ) ;
#13108 = CARTESIAN_POINT ( 'NONE',  ( 1.410761154855643795, -0.3162353388693405765, 0.4822834645669290543 ) ) ;
#13107 = CARTESIAN_POINT ( 'NONE',  ( -0.8478501267249380913, 2.401574803149606474, 0.8478501267249375362 ) ) ;
#13109 = CARTESIAN_POINT ( 'NONE',  ( 1.450131233595801428, -0.6692913385826773087, -0.1292274648535924053 ) ) ;
#13110 = CARTESIAN_POINT ( 'NONE',  ( 0.3392501089628018329, 0.1958661417322835607, -2.328083989501312345 ) ) ;
#13111 = CARTESIAN_POINT ( 'NONE',  ( -1.220472440944881054, 2.401574803149606474, 0.5309055118110237448 ) ) ;
#13112 = CARTESIAN_POINT ( 'NONE',  ( -1.076115485564303809, 0.2306618581243848609, 0.2411417322834645549 ) ) ;
#13113 = B_SPLINE_CURVE_WITH_KNOTS ( 'NONE', 3,
 ( #2750, #75830, #21682, #41045 ),
 .UNSPECIFIED., .F., .F.,
 ( 4, 4 ),
 ( 0.06998245282297338443, 0.07142600748853988879 ),
 .UNSPECIFIED. ) ;
#13114 = CARTESIAN_POINT ( 'NONE',  ( -0.1265901696524993347, 0.4724409448818895907, -0.9514435695538056015 ) ) ;
#13115 = CARTESIAN_POINT ( 'NONE',  ( 0.2925321140481932369, 0.2925321140481932369, -0.1377952755905512139 ) ) ;
#13116 = ORIENTED_EDGE ( 'NONE', *, *, #50670, .T. ) ;
#13117 = CARTESIAN_POINT ( 'NONE',  ( -0.2165354330708654795, 0.07958543189024085140, 0.2665933059059887866 ) ) ;
#13118 = CARTESIAN_POINT ( 'NONE',  ( -0.3392501089628017219, -0.1958661417322836718, -1.619422572178477848 ) ) ;
#13119 = ORIENTED_EDGE ( 'NONE', *, *, #58308, .F. ) ;
#13120 = CARTESIAN_POINT ( 'NONE',  ( 0.1377952755905518800, -0.5400638737290844871, 0.3530559997133364547 ) ) ;
#13121 = EDGE_CURVE ( 'NONE', #8593, #5432, #42563, .T. ) ;
#13122 = CARTESIAN_POINT ( 'NONE',  ( 0.5905511811023629321, -0.6692913385826771977, 8.415575281601705876E-17 ) ) ;
#13123 = CARTESIAN_POINT ( 'NONE',  ( 0.1265901696524989462, 0.4724409448818897572, -2.828083989501312345 ) ) ;
#13124 = DIRECTION ( 'NONE',  ( 0.000000000000000000, 0.000000000000000000, -1.000000000000000000 ) ) ;
#13125 = CARTESIAN_POINT ( 'NONE',  ( -0.5052493438320203589, 0.1771653543307087075, -0.09757992244046823083 ) ) ;
#13126 = CARTESIAN_POINT ( 'NONE',  ( 0.4177787735907000366, 0.3937007874015747699, -1.559171609364239375 ) ) ;
#13127 = CARTESIAN_POINT ( 'NONE',  ( 0.6824146981627303710, -0.6046776061558807314, 0.2411417322834647770 ) ) ;
#13128 = CARTESIAN_POINT ( 'NONE',  ( 1.023622047244095112, -0.1870078740157480601, -0.3641732283464567677 ) ) ;
#13129 = CARTESIAN_POINT ( 'NONE',  ( -0.5905511811023613777, -0.6692913385826771977, 8.415575281601705876E-17 ) ) ;
#13130 = CARTESIAN_POINT ( 'NONE',  ( -0.3392501089628019439, 0.1958661417322832554, -1.208642101540995606 ) ) ;
#13131 = CARTESIAN_POINT ( 'NONE',  ( -0.8136482939632537770, 0.2306618581243847221, -0.2411417322834647770 ) ) ;
#13132 = CARTESIAN_POINT ( 'NONE',  ( -1.332020997375327642, -0.2845877964562161244, -0.3641732283464567121 ) ) ;
#13133 = CARTESIAN_POINT ( 'NONE',  ( -0.8005249343832013809, -0.4281496062992124485, 0.4176697321401328655 ) ) ;
#13134 = CARTESIAN_POINT ( 'NONE',  ( 1.679790026246720025, 0.2306618581243848609, 0.2411417322834645549 ) ) ;
#13135 = CARTESIAN_POINT ( 'NONE',  ( -0.4117837489889357716, 1.301386200251876124, -2.058030895701184804 ) ) ;
#13136 = ORIENTED_EDGE ( 'NONE', *, *, #27456, .T. ) ;
#13137 = CARTESIAN_POINT ( 'NONE',  ( -0.1958661417322833942, -0.3392501089628018884, -2.267079683235907694 ) ) ;
#13138 = CARTESIAN_POINT ( 'NONE',  ( -0.1706036745406816491, 0.05413385826771626580, -0.4176697321401330321 ) ) ;
#13139 = ORIENTED_EDGE ( 'NONE', *, *, #29595, .F. ) ;
#13140 = CARTESIAN_POINT ( 'NONE',  ( -0.7939632545931754048, -0.3162353388693405765, 0.4822834645669290543 ) ) ;
#13141 = CARTESIAN_POINT ( 'NONE',  ( 1.482939632545932307, 0.05413385826771626580, -0.4176697321401330321 ) ) ;
#13142 = CARTESIAN_POINT ( 'NONE',  ( 1.167979002624672580, 0.05413385826771626580, -0.4176697321401330321 ) ) ;
#13143 = ADVANCED_FACE ( 'NONE', ( #77989 ), #21561, .F. ) ;
#13144 = CARTESIAN_POINT ( 'NONE',  ( 0.6758530183727039509, 0.2952755905511810774, -0.1292274648535930714 ) ) ;
#13145 = CARTESIAN_POINT ( 'NONE',  ( 0.2493438320209980519, 0.05413385826771666132, 0.4176697321401328100 ) ) ;
#13146 = CARTESIAN_POINT ( 'NONE',  ( -0.1958661417322834220, -0.3392501089628018884, -1.252624671916010568 ) ) ;
#13147 = CARTESIAN_POINT ( 'NONE',  ( -1.036745406824146176, 0.05413385826771626580, -0.4176697321401330321 ) ) ;
#13148 = CARTESIAN_POINT ( 'NONE',  ( -0.08530183727034056085, -0.3162353388693405765, 0.4822834645669290543 ) ) ;
#13149 = EDGE_CURVE ( 'NONE', #79410, #57515, #8614, .T. ) ;
#13150 = CARTESIAN_POINT ( 'NONE',  ( 0.09186351706036827158, -0.004921259842519576551, 0.3153832671262227771 ) ) ;
#13151 = LINE ( 'NONE', #40481, #79919 ) ;
#13152 = CARTESIAN_POINT ( 'NONE',  ( -0.2099737532808391705, -0.6046776061558809534, -0.2411417322834644161 ) ) ;
#13153 = CARTESIAN_POINT ( 'NONE',  ( -0.5314960629921394730, 2.736617272820978108, 3.873860110281695412 ) ) ;
#13154 = CARTESIAN_POINT ( 'NONE',  ( 0.9251968503937015864, -0.5400638737290844871, 0.3530559997133364547 ) ) ;
#13155 = DIRECTION ( 'NONE',  ( 0.000000000000000000, -1.000000000000000000, 0.000000000000000000 ) ) ;
#13156 = ORIENTED_EDGE ( 'NONE', *, *, #74163, .F. ) ;
#13157 = EDGE_LOOP ( 'NONE', ( #41189, #28473, #58016, #54435 ) ) ;
#13158 = CARTESIAN_POINT ( 'NONE',  ( 0.3608923884514443348, -0.6692913385826771977, 0.1292274648535927661 ) ) ;
#13159 = CARTESIAN_POINT ( 'NONE',  ( -0.2427821522309703550, -0.08942795157528024563, -0.3641732283464568787 ) ) ;
#13161 = CARTESIAN_POINT ( 'NONE',  ( 1.614173228346457378, 0.5038684218300975015, 0.1372047244094478369 ) ) ;
#13160 = CARTESIAN_POINT ( 'NONE',  ( 1.443569553805774897, -0.5023911411419708095, -0.1820866141732282451 ) ) ;
#13162 = CARTESIAN_POINT ( 'NONE',  ( 0.4724409448818896462, 0.1265901696524990294, -0.04396325459317586282 ) ) ;
#13163 = CARTESIAN_POINT ( 'NONE',  ( 3.937007874015748143, 1.537401574803149984, 0.4744094488188975722 ) ) ;
#13164 = CARTESIAN_POINT ( 'NONE',  ( -1.476377952755905110, 0.1660481256975885056, 0.3530559997133364547 ) ) ;
#13165 = CARTESIAN_POINT ( 'NONE',  ( 0.1998031496062994128, -0.3460692066303957537, -2.688320209973753538 ) ) ;
#13166 = CARTESIAN_POINT ( 'NONE',  ( -0.1443569553805768291, 0.05413385826771666132, 0.4176697321401328100 ) ) ;
#13167 = CARTESIAN_POINT ( 'NONE',  ( -1.646051170424378096, 0.000000000000000000, 0.3464511005275205946 ) ) ;
#13168 = CARTESIAN_POINT ( 'NONE',  ( -1.561679790026246017, 0.05413385826771666132, 0.4176697321401328100 ) ) ;
#13169 = CARTESIAN_POINT ( 'NONE',  ( 0.3280839895013130669, 0.05413385826771666132, 0.4176697321401328100 ) ) ;
#13170 = CARTESIAN_POINT ( 'NONE',  ( -0.3949938075777411073, 0.1058382717557497660, 0.04790026246719160385 ) ) ;
#13171 = CARTESIAN_POINT ( 'NONE',  ( 1.555118110236221041, 0.1660481256975883668, -0.3530559997133364547 ) ) ;
#13172 = CARTESIAN_POINT ( 'NONE',  ( 0.8530183727034126306, 0.05413385826771626580, -0.4176697321401330321 ) ) ;
#13173 = CARTESIAN_POINT ( 'NONE',  ( 1.102362204724410155, -0.1870078740157480601, -0.3641732283464567677 ) ) ;
#13174 = CARTESIAN_POINT ( 'NONE',  ( 0.000000000000000000, 2.755905511811024056, 0.000000000000000000 ) ) ;
#13175 = CARTESIAN_POINT ( 'NONE',  ( 0.7939632545931766261, -0.2845877964562161244, -0.3641732283464567121 ) ) ;
#13176 = CARTESIAN_POINT ( 'NONE',  ( -1.292650918635170010, 0.2952755905511810774, -0.1292274648535930714 ) ) ;
#13177 = EDGE_CURVE ( 'NONE', #2851, #51988, #5888, .T. ) ;
#13178 = CARTESIAN_POINT ( 'NONE',  ( 0.3460692066303959202, -0.1998031496062991630, -0.9691601049868766582 ) ) ;
#13179 = CARTESIAN_POINT ( 'NONE',  ( 1.364829396325460076, 0.2306618581243848609, 0.2411417322834645549 ) ) ;
#13180 = CARTESIAN_POINT ( 'NONE',  ( 0.3917322834645670104, 2.398668435337828261E-17, -0.7401574803149605364 ) ) ;
#13182 = CARTESIAN_POINT ( 'NONE',  ( -0.3334193678581739984, 1.199601195606727844, 1.973660451468200350 ) ) ;
#13181 = CARTESIAN_POINT ( 'NONE',  ( 0.7217847769028878924, 0.05413385826771666132, 0.4176697321401328100 ) ) ;
#13183 = CARTESIAN_POINT ( 'NONE',  ( -1.377952755905511140, 0.1771653543307087630, 0.000000000000000000 ) ) ;
#13184 = CARTESIAN_POINT ( 'NONE',  ( 0.4133858267716541968, -0.4536011799217368745, -0.2665933059059886201 ) ) ;
#13185 = EDGE_CURVE ( 'NONE', #66439, #51179, #8994, .T. ) ;
#13186 = CARTESIAN_POINT ( 'NONE',  ( 0.6102362204724416372, 0.1660481256975883668, -0.3530559997133364547 ) ) ;
#13187 = CARTESIAN_POINT ( 'NONE',  ( 0.7480314960629927956, 0.2066929133858268208, 0.000000000000000000 ) ) ;
#13188 = CARTESIAN_POINT ( 'NONE',  ( -0.8398950131233589023, -0.5023911411419708095, -0.1820866141732282451 ) ) ;
#13189 = CARTESIAN_POINT ( 'NONE',  ( -0.5839895013123351797, 0.2952755905511810774, -0.1292274648535930714 ) ) ;
#13190 = CARTESIAN_POINT ( 'NONE',  ( 1.568241469816273659, -0.05778040916215560624, -0.4822834645669293319 ) ) ;
#13191 = CARTESIAN_POINT ( 'NONE',  ( -1.148293963254592542, -0.6692913385826773087, -0.1292274648535924053 ) ) ;
#13192 = CARTESIAN_POINT ( 'NONE',  ( 0.7939632545931766261, -0.3162353388693409650, -0.4822834645669289433 ) ) ;
#13193 = CARTESIAN_POINT ( 'NONE',  ( -1.200787401574802349, -0.4536011799217367080, 0.2665933059059888421 ) ) ;
#13194 = ADVANCED_FACE ( 'NONE', ( #2212 ), #39249, .F. ) ;
#13195 = CARTESIAN_POINT ( 'NONE',  ( 0.1341536278048623410, 0.7086614173228346081, 0.2827841492639508458 ) ) ;
#13196 = CARTESIAN_POINT ( 'NONE',  ( 0.9448818897637802916, -0.1870078740157479769, 0.4822834645669291653 ) ) ;
#13197 = AXIS2_PLACEMENT_3D ( 'NONE', #83272, #30265, #57581 ) ;
#13198 = CARTESIAN_POINT ( 'NONE',  ( -0.3458507752293906723, -0.3458507752293910609, -2.498031496062992574 ) ) ;
#13199 = CARTESIAN_POINT ( 'NONE',  ( -1.653543307086613234, -0.1870078740157480879, -0.4822834645669291653 ) ) ;
#13200 = CARTESIAN_POINT ( 'NONE',  ( 1.423884514435696413, -0.3162353388693409650, -0.4822834645669289433 ) ) ;
#13201 = CARTESIAN_POINT ( 'NONE',  ( -1.089238845144356427, -0.004921259842519576551, 0.3153832671262227771 ) ) ;
#13202 = CARTESIAN_POINT ( 'NONE',  ( 1.574803149606299746, -0.1870078740157480601, -0.3641732283464567677 ) ) ;
#13203 = CARTESIAN_POINT ( 'NONE',  ( -0.3674540682414689785, 0.2306618581243848609, 0.2411417322834645549 ) ) ;
#13204 = CARTESIAN_POINT ( 'NONE',  ( -0.4527559055118102749, -0.4536011799217368745, -0.2665933059059886201 ) ) ;
#13205 = CARTESIAN_POINT ( 'NONE',  ( -1.719160104986876103, -0.004921259842519576551, 0.3153832671262227771 ) ) ;
#13206 = CARTESIAN_POINT ( 'NONE',  ( 0.7874015748031503170, -0.1870078740157479769, 0.3641732283464567677 ) ) ;
#13207 = CARTESIAN_POINT ( 'NONE',  ( 0.7217847769028878924, 0.05413385826771666132, 0.4176697321401328100 ) ) ;
#13208 = CARTESIAN_POINT ( 'NONE',  ( 1.332020997375328974, -0.05778040916215560624, -0.4822834645669293319 ) ) ;
#13209 = CARTESIAN_POINT ( 'NONE',  ( 0.5774278215223104249, 0.2306618581243848609, 0.2411417322834645549 ) ) ;
#13210 = CARTESIAN_POINT ( 'NONE',  ( 0.3674540682414705883, 0.1283753931104746893, -0.1820866141732285504 ) ) ;
#13211 = B_SPLINE_CURVE_WITH_KNOTS ( 'NONE', 3,
 ( #17415, #48539, #9839, #30012 ),
 .UNSPECIFIED., .F., .F.,
 ( 4, 4 ),
 ( 0.1191888912451262300, 0.1206125572960974335 ),
 .UNSPECIFIED. ) ;
#13212 = CARTESIAN_POINT ( 'NONE',  ( -1.535433070866141225, -0.6692913385826771977, 8.415575281601705876E-17 ) ) ;
#13213 = CARTESIAN_POINT ( 'NONE',  ( -1.272965879265091305, 0.05413385826771626580, -0.4176697321401330321 ) ) ;
#13214 = CARTESIAN_POINT ( 'NONE',  ( -0.6496062992125976043, -0.5400638737290844871, 0.3530559997133364547 ) ) ;
#13215 = CARTESIAN_POINT ( 'NONE',  ( 0.3996062992125985480, 0.1070741851644054637, -0.4396325459317584894 ) ) ;
#13216 = CARTESIAN_POINT ( 'NONE',  ( -0.3130110660353679908, 1.444485302887537514, 0.002040369744756952066 ) ) ;
#13217 = CARTESIAN_POINT ( 'NONE',  ( 0.1181102362204730916, -0.6692913385826771977, 8.415575281601705876E-17 ) ) ;
#13218 = CARTESIAN_POINT ( 'NONE',  ( 1.240157480314961314, -0.4536011799217367080, 0.2665933059059888421 ) ) ;
#13219 = CARTESIAN_POINT ( 'NONE',  ( -0.2821522309711278487, -0.6692913385826773087, -0.1292274648535924053 ) ) ;
#13220 = CARTESIAN_POINT ( 'NONE',  ( 0.4068241469816279987, -0.4281496062992127816, -0.4176697321401328100 ) ) ;
#13221 = CARTESIAN_POINT ( 'NONE',  ( -0.3996062992125986035, -0.1070741851644056997, -2.723097112860892288 ) ) ;
#13222 = CARTESIAN_POINT ( 'NONE',  ( -0.3949938075777411628, 0.1058382717557497937, -1.765091863517060267 ) ) ;
#13223 = CARTESIAN_POINT ( 'NONE',  ( -0.3917322834645669549, -0.1049643490035306603, -0.5104986876640419391 ) ) ;
#13224 = CARTESIAN_POINT ( 'NONE',  ( 0.2490243534527243618, -0.1587552710309117210, 5.781441956045568986 ) ) ;
#13225 = CARTESIAN_POINT ( 'NONE',  ( 0.3917322834645670104, -0.1049643490035303273, -0.8910761154855640909 ) ) ;
#13226 = CARTESIAN_POINT ( 'NONE',  ( -0.9711286089238838626, -0.5023911411419708095, 0.1820866141732285504 ) ) ;
#13227 = CARTESIAN_POINT ( 'NONE',  ( -1.246719160104986512, 0.05413385826771666132, 0.4176697321401328100 ) ) ;
#13228 = CARTESIAN_POINT ( 'NONE',  ( -0.3917322834645670659, 0.1049643490035301607, 0.2021190533146474677 ) ) ;
#13229 = CARTESIAN_POINT ( 'NONE',  ( 0.3674540682414705883, -0.6046776061558807314, 0.2411417322834647770 ) ) ;
#13230 = CARTESIAN_POINT ( 'NONE',  ( 1.345144356955381593, -0.3162353388693409650, -0.4822834645669289433 ) ) ;
#13231 = CARTESIAN_POINT ( 'NONE',  ( 0.9120734908136489683, -0.6692913385826771977, 0.1292274648535927661 ) ) ;
#13232 = CARTESIAN_POINT ( 'NONE',  ( 0.4724409448818896462, 0.1265901696524990294, -2.801837270341207553 ) ) ;
#13233 = CARTESIAN_POINT ( 'NONE',  ( 0.1998031496062992740, 0.3460692066303959757, -2.664041994750656173 ) ) ;
#13234 = CARTESIAN_POINT ( 'NONE',  ( -9.594673741351313045E-17, 0.3917322834645670659, -1.099100680611235559 ) ) ;
#13235 = CARTESIAN_POINT ( 'NONE',  ( 1.502624671916010790, -0.05778040916215522460, 0.4822834645669289988 ) ) ;
#13236 = CARTESIAN_POINT ( 'NONE',  ( 0.4002624671916016896, -0.3162353388693409650, -0.4822834645669289433 ) ) ;
#13237 = ADVANCED_FACE ( 'NONE', ( #26630 ), #46586, .T. ) ;
#13238 = CARTESIAN_POINT ( 'NONE',  ( 0.3149606299212603933, -0.1870078740157479769, 0.4822834645669291653 ) ) ;
#13239 = CARTESIAN_POINT ( 'NONE',  ( 0.7939632545931766261, -0.08942795157527998196, 0.3641732283464567121 ) ) ;
#13240 = CARTESIAN_POINT ( 'NONE',  ( 1.167979002624672580, -0.4281496062992124485, 0.4176697321401328655 ) ) ;
#13241 = CARTESIAN_POINT ( 'NONE',  ( 0.1049643490035304938, -0.3917322834645669549, -0.01246719160104995359 ) ) ;
#13242 = CARTESIAN_POINT ( 'NONE',  ( 0.2559055118110243332, -0.5400638737290845981, -0.3530559997133363437 ) ) ;
#13243 = CARTESIAN_POINT ( 'NONE',  ( 0.9383202099737538715, -0.05778040916215560624, -0.4822834645669293319 ) ) ;
#13244 = CARTESIAN_POINT ( 'NONE',  ( 0.4199475065616805614, 0.2306618581243848609, 0.2411417322834645549 ) ) ;
#13245 = CARTESIAN_POINT ( 'NONE',  ( 1.069553805774278832, 0.1771653543307087075, -0.09757992244046823083 ) ) ;
#13246 = CARTESIAN_POINT ( 'NONE',  ( -0.9055118110236215490, 0.2952755905511811885, 0.000000000000000000 ) ) ;
#13247 = CARTESIAN_POINT ( 'NONE',  ( -1.069553805774277722, 0.2952755905511811885, 0.1292274648535926551 ) ) ;
#13248 = CARTESIAN_POINT ( 'NONE',  ( 1.036745406824147508, -0.4281496062992127816, -0.4176697321401328100 ) ) ;
#13249 = CARTESIAN_POINT ( 'NONE',  ( 0.1049643490035303689, 0.3917322834645670104, -0.5505249343832020470 ) ) ;
#13250 = CARTESIAN_POINT ( 'NONE',  ( -0.1958661417322834220, -0.3392501089628018884, -1.947506561679789971 ) ) ;
#13251 = CARTESIAN_POINT ( 'NONE',  ( -0.1049643490035302024, -0.3917322834645671215, -2.898950131233595684 ) ) ;
#13252 = VERTEX_POINT ( 'NONE', #71666 ) ;
#13253 = CARTESIAN_POINT ( 'NONE',  ( 0.1998031496062992740, 0.3460692066303959757, 0.01312335958005247417 ) ) ;
#13254 = VERTEX_POINT ( 'NONE', #20740 ) ;
#13255 = CARTESIAN_POINT ( 'NONE',  ( 1.679790026246720025, 0.2306618581243848609, 0.2411417322834645549 ) ) ;
#13256 = CARTESIAN_POINT ( 'NONE',  ( 0.9645669291338588858, 0.07958543189024085140, 0.2665933059059887866 ) ) ;
#13257 = CARTESIAN_POINT ( 'NONE',  ( -0.2925321140481930704, -0.2925321140481933480, -1.633858267716534973 ) ) ;
#13258 = CARTESIAN_POINT ( 'NONE',  ( 1.489501312335958172, -0.2845877964562159024, 0.3641732283464567677 ) ) ;
#13259 = CARTESIAN_POINT ( 'NONE',  ( 2.362204724409448620, 1.929133858267716661, 8.247593713802677664E-15 ) ) ;
#13260 = CARTESIAN_POINT ( 'NONE',  ( -0.1246719160104980684, 0.2952755905511811885, 0.1292274648535926551 ) ) ;
#13261 = CARTESIAN_POINT ( 'NONE',  ( -9.594673741351313045E-17, 0.3917322834645670104, -0.7145669291338584417 ) ) ;
#13262 = CARTESIAN_POINT ( 'NONE',  ( -1.220472440944881054, -0.5511811023622047445, 6.969142054262312111E-17 ) ) ;
#13263 = CARTESIAN_POINT ( 'NONE',  ( -1.541994750656167090, 0.1771653543307087630, 0.09757992244046791164 ) ) ;
#13264 = CARTESIAN_POINT ( 'NONE',  ( -1.266404199475064773, -0.05778040916215560624, -0.4822834645669293319 ) ) ;
#13265 = CARTESIAN_POINT ( 'NONE',  ( 0.1574803149606306130, -0.1870078740157479769, 0.4822834645669291653 ) ) ;
#13266 = CARTESIAN_POINT ( 'NONE',  ( 1.345144356955381593, -0.3162353388693409650, -0.4822834645669289433 ) ) ;
#13267 = ORIENTED_EDGE ( 'NONE', *, *, #31580, .F. ) ;
#13268 = CARTESIAN_POINT ( 'NONE',  ( -1.116861235539043928, 1.075383049963962279, -0.1088361571701338959 ) ) ;
#13269 = CARTESIAN_POINT ( 'NONE',  ( 0.000000000000000000, 0.000000000000000000, -2.755905511811024056 ) ) ;
#13270 = CARTESIAN_POINT ( 'NONE',  ( -0.9580052493438311334, -0.004921259842519870586, -0.3153832671262229437 ) ) ;
#13271 = LINE ( 'NONE', #7359, #79940 ) ;
#13272 = CARTESIAN_POINT ( 'NONE',  ( 0.7611548556430454138, 0.2306618581243847221, -0.2411417322834647770 ) ) ;
#13273 = ORIENTED_EDGE ( 'NONE', *, *, #74631, .T. ) ;
#13275 = FACE_OUTER_BOUND ( 'NONE', #43228, .T. ) ;
#13274 = CARTESIAN_POINT ( 'NONE',  ( 0.4724409448818898682, 2.892866454678787531E-17, -2.557086614173228689 ) ) ;
#13276 = CARTESIAN_POINT ( 'NONE',  ( 1.430446194225722500, -0.4281496062992127816, -0.4176697321401328100 ) ) ;
#13277 = CARTESIAN_POINT ( 'NONE',  ( 1.522309711286089939, -0.5023911411419708095, -0.1820866141732282451 ) ) ;
#13278 = CARTESIAN_POINT ( 'NONE',  ( 0.1958661417322834497, 0.3392501089628018329, -0.6968310779189482718 ) ) ;
#13279 = CARTESIAN_POINT ( 'NONE',  ( -0.2624671916010490880, 0.1283753931104746893, -0.1820866141732285504 ) ) ;
#13280 = CARTESIAN_POINT ( 'NONE',  ( -1.299212598425196097, 0.1771653543307087630, 0.000000000000000000 ) ) ;
#13281 = CARTESIAN_POINT ( 'NONE',  ( -0.2867679344610364334, -0.2867679344610367109, -1.088582677165354173 ) ) ;
#13282 = CARTESIAN_POINT ( 'NONE',  ( -0.4527559055118102749, -0.4536011799217368745, -0.2665933059059886201 ) ) ;
#13283 = CARTESIAN_POINT ( 'NONE',  ( 0.2559055118110243332, -0.4536011799217368745, -0.2665933059059886201 ) ) ;
#13284 = CARTESIAN_POINT ( 'NONE',  ( 0.2427821522309716595, -0.3162353388693409650, -0.4822834645669289433 ) ) ;
#13285 = CARTESIAN_POINT ( 'NONE',  ( -0.9908136482939626788, 0.1771653543307087630, 0.09757992244046791164 ) ) ;
#13286 = CARTESIAN_POINT ( 'NONE',  ( 0.2867679344610365999, 0.2867679344610365999, -2.807086614173227357 ) ) ;
#13287 = CARTESIAN_POINT ( 'NONE',  ( 1.174540682414699111, -0.05778040916215560624, -0.4822834645669293319 ) ) ;
#13288 = CARTESIAN_POINT ( 'NONE',  ( -1.227034120734907141, -0.6692913385826773087, -0.1292274648535924053 ) ) ;
#13289 = CARTESIAN_POINT ( 'NONE',  ( 0.4724409448818896462, 0.1265901696524990294, -1.303805774278215202 ) ) ;
#13290 = CARTESIAN_POINT ( 'NONE',  ( -0.4527559055118102749, 0.1660481256975885056, 0.3530559997133364547 ) ) ;
#13291 = CARTESIAN_POINT ( 'NONE',  ( -0.8792650918635160906, -0.4281496062992124485, 0.4176697321401328655 ) ) ;
#13292 = CARTESIAN_POINT ( 'NONE',  ( 0.8464566929133866546, -0.4536011799217367080, 0.2665933059059888421 ) ) ;
#13293 = CARTESIAN_POINT ( 'NONE',  ( -0.2952755905511804668, 0.07958543189024085140, 0.2665933059059887866 ) ) ;
#13294 = CARTESIAN_POINT ( 'NONE',  ( -0.7874015748031489847, -0.1870078740157479769, 0.4822834645669291653 ) ) ;
#13295 = CARTESIAN_POINT ( 'NONE',  ( -1.469816272965878357, 0.2306618581243848609, 0.2411417322834645549 ) ) ;
#13296 = CARTESIAN_POINT ( 'NONE',  ( 0.4330708661417329575, 1.488513638086841118, 0.000000000000000000 ) ) ;
#13297 = CARTESIAN_POINT ( 'NONE',  ( 1.233595800524935227, 0.1283753931104746893, -0.1820866141732285504 ) ) ;
#13298 = CARTESIAN_POINT ( 'NONE',  ( -1.509186351706035767, -0.4281496062992124485, 0.4176697321401328655 ) ) ;
#13299 = CARTESIAN_POINT ( 'NONE',  ( -1.522309711286088607, 0.2306618581243847221, -0.2411417322834647770 ) ) ;
#13300 = VERTEX_POINT ( 'NONE', #59032 ) ;
#13301 = CARTESIAN_POINT ( 'NONE',  ( -0.3996062992125986590, 0.1070741851644051723, -2.471784776902887337 ) ) ;
#13302 = CARTESIAN_POINT ( 'NONE',  ( -0.9317585301837263412, -0.3690944881889765550, -0.3153832671262227771 ) ) ;
#13303 = CARTESIAN_POINT ( 'NONE',  ( 0.6167979002624678353, -0.4281496062992124485, 0.4176697321401328655 ) ) ;
#13304 = CARTESIAN_POINT ( 'NONE',  ( -0.9645669291338575535, -0.4536011799217367080, 0.2665933059059888421 ) ) ;
#13305 = CARTESIAN_POINT ( 'NONE',  ( 0.1070741851644054776, -0.3996062992125984925, -1.421916010498687877 ) ) ;
#13306 = CARTESIAN_POINT ( 'NONE',  ( -0.9645669291338575535, -0.5400638737290844871, 0.3530559997133364547 ) ) ;
#13307 = CARTESIAN_POINT ( 'NONE',  ( 0.6692913385826778638, -0.6692913385826771977, 8.415575281601705876E-17 ) ) ;
#13308 = CARTESIAN_POINT ( 'NONE',  ( 0.4593175853018380828, 0.05413385826771626580, -0.4176697321401330321 ) ) ;
#13309 = CARTESIAN_POINT ( 'NONE',  ( 1.574803149606299746, -0.1870078740157479769, 0.4822834645669291653 ) ) ;
#13310 = CARTESIAN_POINT ( 'NONE',  ( -1.614173228346456268, -0.5511811023622047445, 6.969142054262312111E-17 ) ) ;
#13311 = CARTESIAN_POINT ( 'NONE',  ( 0.1998031496062992463, 0.3460692066303959202, -0.8510498687664042050 ) ) ;
#13312 = CARTESIAN_POINT ( 'NONE',  ( 0.2925321140481932369, 0.2925321140481932369, -0.7677165354330709457 ) ) ;
#13313 = CARTESIAN_POINT ( 'NONE',  ( 0.3949938075777409408, 0.1058382717557500574, -0.7545931758530185496 ) ) ;
#13314 = CARTESIAN_POINT ( 'NONE',  ( 1.348312163386739426, 0.2755905511811023723, 0.8371118098809627872 ) ) ;
#13315 = CARTESIAN_POINT ( 'NONE',  ( 1.003937007874016407, -0.4536011799217367080, 0.2665933059059888421 ) ) ;
#13316 = CARTESIAN_POINT ( 'NONE',  ( 0.2493438320209980519, -0.3690944881889765550, -0.3153832671262227771 ) ) ;
#13317 = CARTESIAN_POINT ( 'NONE',  ( 0.2493438320209980519, -0.4281496062992127816, -0.4176697321401328100 ) ) ;
#13318 = CARTESIAN_POINT ( 'NONE',  ( 1.345144356955381593, -0.3162353388693409650, -0.4822834645669289433 ) ) ;
#13319 = CARTESIAN_POINT ( 'NONE',  ( -0.1058382717557503072, 0.3949938075777408852, -1.343175853018372834 ) ) ;
#13320 = CARTESIAN_POINT ( 'NONE',  ( 0.3083989501312343062, -0.08942795157528024563, -0.3641732283464568787 ) ) ;
#13321 = CARTESIAN_POINT ( 'NONE',  ( -0.6561679790026240244, 0.2306618581243847221, -0.2411417322834647770 ) ) ;
#13322 = CARTESIAN_POINT ( 'NONE',  ( -1.286089238845143479, 0.2306618581243847221, -0.2411417322834647770 ) ) ;
#13323 = CARTESIAN_POINT ( 'NONE',  ( 0.8070866141732289112, -0.5400638737290845981, -0.3530559997133363437 ) ) ;
#13324 = CARTESIAN_POINT ( 'NONE',  ( 0.4091458600556404646, -0.2362204724409448231, -1.522309711286089273 ) ) ;
#13325 = CARTESIAN_POINT ( 'NONE',  ( -0.7545931758530176614, 0.2952755905511811885, 0.1292274648535926551 ) ) ;
#13326 = ORIENTED_EDGE ( 'NONE', *, *, #56357, .T. ) ;
#13327 = ORIENTED_EDGE ( 'NONE', *, *, #59249, .T. ) ;
#13328 = CARTESIAN_POINT ( 'NONE',  ( -1.161417322834644716, -0.5400638737290845981, -0.3530559997133363437 ) ) ;
#13329 = CARTESIAN_POINT ( 'NONE',  ( -0.4855643044619415427, 0.05413385826771626580, -0.4176697321401330321 ) ) ;
#13331 = CARTESIAN_POINT ( 'NONE',  ( -0.9120734908136475250, -0.6692913385826773087, -0.1292274648535924053 ) ) ;
#13330 = CARTESIAN_POINT ( 'NONE',  ( -0.8070866141732276899, 0.07958543189024071263, -0.2665933059059888421 ) ) ;
#13332 = CARTESIAN_POINT ( 'NONE',  ( -0.1049643490035306742, 0.3917322834645668994, -1.818878322013436355 ) ) ;
#13333 = CARTESIAN_POINT ( 'NONE',  ( 0.000000000000000000, 1.724409448818897905, 0.000000000000000000 ) ) ;
#13334 = CARTESIAN_POINT ( 'NONE',  ( 1.614173228346457378, -0.6692913385826771977, 8.415575281601705876E-17 ) ) ;
#13335 = CARTESIAN_POINT ( 'NONE',  ( -1.030183727034119867, -0.05778040916215560624, -0.4822834645669293319 ) ) ;
#13336 = CARTESIAN_POINT ( 'NONE',  ( 0.1837270341207354329, 0.2306618581243848609, 0.2411417322834645549 ) ) ;
#13337 = CARTESIAN_POINT ( 'NONE',  ( -0.6496062992125976043, 0.1660481256975883668, -0.3530559997133364547 ) ) ;
#13338 = CARTESIAN_POINT ( 'NONE',  ( -0.2867679344610364334, -0.2867679344610367109, -1.311023622047244430 ) ) ;
#13339 = CARTESIAN_POINT ( 'NONE',  ( -0.8727034120734901146, -0.2845877964562159024, 0.3641732283464567677 ) ) ;
#13340 = ORIENTED_EDGE ( 'NONE', *, *, #49331, .F. ) ;
#13341 = CARTESIAN_POINT ( 'NONE',  ( 0.3949938075777411073, -0.1058382717557499464, -2.001312335958005395 ) ) ;
#13342 = EDGE_LOOP ( 'NONE', ( #70918, #67919, #78918, #48210 ) ) ;
#13343 = LINE ( 'NONE', #32687, #32780 ) ;
#13344 = CARTESIAN_POINT ( 'NONE',  ( -0.9317585301837263412, 0.05413385826771666132, 0.4176697321401328100 ) ) ;
#13345 = CARTESIAN_POINT ( 'NONE',  ( -1.358267716535432434, -0.5400638737290844871, 0.3530559997133364547 ) ) ;
#13346 = CARTESIAN_POINT ( 'NONE',  ( 0.3996062992125986590, -0.1070741851644053111, -0.1115485564304461857 ) ) ;
#13347 = CARTESIAN_POINT ( 'NONE',  ( -1.174540682414697335, -0.3162353388693409650, -0.4822834645669289433 ) ) ;
#13348 = CARTESIAN_POINT ( 'NONE',  ( -1.246719160104986512, 0.05413385826771666132, 0.4176697321401328100 ) ) ;
#13349 = VECTOR ( 'NONE', #58792, 39.37007874015748143 ) ;
#13350 = DIRECTION ( 'NONE',  ( -0.000000000000000000, -1.000000000000000000, -0.000000000000000000 ) ) ;
#13351 = CARTESIAN_POINT ( 'NONE',  ( 1.595398199321655275, 1.288687073698532526, -0.1559797534342494130 ) ) ;
#13352 = CARTESIAN_POINT ( 'NONE',  ( 0.07874015748031558404, -0.1870078740157479769, 0.3641732283464567677 ) ) ;
#13353 = CARTESIAN_POINT ( 'NONE',  ( 0.000000000000000000, 0.5905511811023621549, 0.000000000000000000 ) ) ;
#13354 = CARTESIAN_POINT ( 'NONE',  ( -0.3917322834645669549, -0.1049643490035306603, -0.2880577427821523484 ) ) ;
#13355 = CARTESIAN_POINT ( 'NONE',  ( -0.2099737532808391705, -0.5023911411419708095, -0.1820866141732282451 ) ) ;
#13356 = CARTESIAN_POINT ( 'NONE',  ( -0.8202099737532799750, 0.2952755905511810774, -0.1292274648535930714 ) ) ;
#13357 = CARTESIAN_POINT ( 'NONE',  ( 1.154855643044620184, 0.2306618581243847221, -0.2411417322834647770 ) ) ;
#13358 = CARTESIAN_POINT ( 'NONE',  ( -0.6167979002624665030, -0.4281496062992127816, -0.4176697321401328100 ) ) ;
#13359 = ORIENTED_EDGE ( 'NONE', *, *, #70319, .T. ) ;
#13360 = ORIENTED_EDGE ( 'NONE', *, *, #67540, .F. ) ;
#13361 = CARTESIAN_POINT ( 'NONE',  ( 0.1070741851644053388, 0.3996062992125986035, -2.117454068241469756 ) ) ;
#13362 = CARTESIAN_POINT ( 'NONE',  ( -1.161417322834644716, 0.1660481256975885056, 0.3530559997133364547 ) ) ;
#13363 = CARTESIAN_POINT ( 'NONE',  ( 1.220472440944882386, -0.6692913385826771977, 8.415575281601705876E-17 ) ) ;
#13364 = CARTESIAN_POINT ( 'NONE',  ( -1.292650918635170010, -0.5511811023622046335, 0.09757992244046803654 ) ) ;
#13365 = CARTESIAN_POINT ( 'NONE',  ( -1.476377952755905110, -0.5400638737290845981, -0.3530559997133363437 ) ) ;
#13366 = CARTESIAN_POINT ( 'NONE',  ( -0.4091458600556405756, 0.2362204724409446288, -0.8136482939632546652 ) ) ;
#13367 = DIRECTION ( 'NONE',  ( 0.000000000000000000, 0.000000000000000000, -1.000000000000000000 ) ) ;
#13368 = CARTESIAN_POINT ( 'NONE',  ( 0.1958661417322836440, -0.3392501089628017219, -0.2414698162729658204 ) ) ;
#13369 = CARTESIAN_POINT ( 'NONE',  ( -0.3392501089628017219, -0.1958661417322836718, -2.184383202099737797 ) ) ;
#13370 = CARTESIAN_POINT ( 'NONE',  ( 0.1771653543307093182, -0.5400638737290845981, -0.3530559997133363437 ) ) ;
#13371 = CARTESIAN_POINT ( 'NONE',  ( -1.515748031496062076, -0.4536011799217367080, 0.2665933059059888421 ) ) ;
#13372 = CARTESIAN_POINT ( 'NONE',  ( -0.7349081364829390672, 0.2306618581243847221, -0.2411417322834647770 ) ) ;
#13373 = CARTESIAN_POINT ( 'NONE',  ( -9.787531504996566615E-17, 0.3996062992125985480, 0.2381889763779527491 ) ) ;
#13375 = CARTESIAN_POINT ( 'NONE',  ( -0.2230971128608915943, 0.05413385826771666132, 0.4176697321401328100 ) ) ;
#13374 = CARTESIAN_POINT ( 'NONE',  ( -1.200787401574802349, 0.1660481256975883668, -0.3530559997133364547 ) ) ;
#13376 = CARTESIAN_POINT ( 'NONE',  ( -0.8136482939632537770, -0.6046776061558807314, 0.2411417322834647770 ) ) ;
#13377 = CARTESIAN_POINT ( 'NONE',  ( -0.4855643044619415427, -0.4281496062992124485, 0.4176697321401328655 ) ) ;
#13378 = CARTESIAN_POINT ( 'NONE',  ( 0.2891555358219910499, 0.2891555358219910499, -2.734251968503936592 ) ) ;
#13379 = CARTESIAN_POINT ( 'NONE',  ( 1.062992125984252745, -0.5511811023622047445, 6.969142054262312111E-17 ) ) ;
#13380 = CARTESIAN_POINT ( 'NONE',  ( -0.8464566929133852113, -0.4536011799217368745, -0.2665933059059886201 ) ) ;
#13381 = CARTESIAN_POINT ( 'NONE',  ( 0.01968503937007875723, 0.000000000000000000, 0.000000000000000000 ) ) ;
#13382 = CARTESIAN_POINT ( 'NONE',  ( 0.9186351706036752773, 0.1283753931104746893, -0.1820866141732285504 ) ) ;
#13383 = CARTESIAN_POINT ( 'NONE',  ( 1.318897637795276356, 0.07958543189024071263, -0.2665933059059888421 ) ) ;
#13384 = CARTESIAN_POINT ( 'NONE',  ( 1.555118110236221041, -0.5400638737290844871, 0.3530559997133364547 ) ) ;
#13385 = UNCERTAINTY_MEASURE_WITH_UNIT (LENGTH_MEASURE( 1.000000000000000082E-05 ), #28477, 'distance_accuracy_value', 'NONE');
#13386 = CARTESIAN_POINT ( 'NONE',  ( 0.2952755905511819101, 0.07958543189024071263, -0.2665933059059888421 ) ) ;
#13387 = CARTESIAN_POINT ( 'NONE',  ( -9.594673741351313045E-17, 0.3917322834645670104, -1.409448818897637734 ) ) ;
#13388 = CARTESIAN_POINT ( 'NONE',  ( -0.8136482939632537770, 0.2306618581243847221, -0.2411417322834647770 ) ) ;
#13389 = CARTESIAN_POINT ( 'NONE',  ( 1.332020997375328974, -0.05778040916215560624, -0.4822834645669293319 ) ) ;
#13390 = CARTESIAN_POINT ( 'NONE',  ( -0.3458507752293909498, 0.3458507752293907833, 0.2185039370078740162 ) ) ;
#13391 = CARTESIAN_POINT ( 'NONE',  ( -0.4133858267716528645, -0.4536011799217367080, 0.2665933059059888421 ) ) ;
#13392 = DIRECTION ( 'NONE',  ( 0.000000000000000000, 0.000000000000000000, 1.000000000000000000 ) ) ;
#13393 = CARTESIAN_POINT ( 'NONE',  ( 0.4199475065616805614, 0.2306618581243848609, 0.2411417322834645549 ) ) ;
#13394 = DIRECTION ( 'NONE',  ( 1.000000000000000000, -0.000000000000000000, -0.000000000000000000 ) ) ;
#13395 = CARTESIAN_POINT ( 'NONE',  ( 0.9514435695538062676, -0.08942795157527998196, 0.3641732283464567121 ) ) ;
#13396 = CARTESIAN_POINT ( 'NONE',  ( 0.3674540682414705883, 0.1283753931104746893, -0.1820866141732285504 ) ) ;
#13397 = CARTESIAN_POINT ( 'NONE',  ( -0.2034120734908128059, 0.2952755905511811885, 0.1292274648535926551 ) ) ;
#13398 = CARTESIAN_POINT ( 'NONE',  ( -1.482939632545930975, -0.4281496062992127816, -0.4176697321401328100 ) ) ;
#13399 = CARTESIAN_POINT ( 'NONE',  ( -0.6692913385826764205, 0.1771653543307087630, 0.000000000000000000 ) ) ;
#13400 = LINE ( 'NONE', #12564, #64996 ) ;
#13401 = CARTESIAN_POINT ( 'NONE',  ( -0.7874015748031489847, -0.1870078740157480879, -0.4822834645669291653 ) ) ;
#13402 = CARTESIAN_POINT ( 'NONE',  ( -0.3996062992125986590, 0.1070741851644051723, -1.054461942257217899 ) ) ;
#13403 = CARTESIAN_POINT ( 'NONE',  ( 0.2867679344610365999, -0.2867679344610365444, -2.702755905511810663 ) ) ;
#13404 = CARTESIAN_POINT ( 'NONE',  ( 0.006561679790026889343, -0.08942795157527998196, 0.3641732283464567121 ) ) ;
#13405 = CARTESIAN_POINT ( 'NONE',  ( -0.8530183727034112984, 0.05413385826771666132, 0.4176697321401328100 ) ) ;
#13406 = CARTESIAN_POINT ( 'NONE',  ( -1.141732283464566011, 0.2952755905511811885, 0.000000000000000000 ) ) ;
#13407 = CARTESIAN_POINT ( 'NONE',  ( -1.154855643044618851, 0.1283753931104748280, 0.1820866141732283561 ) ) ;
#13408 = CARTESIAN_POINT ( 'NONE',  ( -3.915497197276881280, 1.300040739893603359, -0.4110563714168837257 ) ) ;
#13409 = CARTESIAN_POINT ( 'NONE',  ( -0.9711286089238838626, 0.1283753931104746893, -0.1820866141732285504 ) ) ;
#13410 = CARTESIAN_POINT ( 'NONE',  ( -1.469816272965878357, -0.5023911411419708095, -0.1820866141732282451 ) ) ;
#13411 = CARTESIAN_POINT ( 'NONE',  ( 1.207349081364829990, -0.6046776061558809534, -0.2411417322834644161 ) ) ;
#13412 = CARTESIAN_POINT ( 'NONE',  ( -0.4091458600556402980, -0.2362204724409451284, -0.6824146981627295938 ) ) ;
#13413 = CARTESIAN_POINT ( 'NONE',  ( 0.3392501089628018884, -0.1958661417322833942, -2.148969447015434575 ) ) ;
#13414 = ORIENTED_EDGE ( 'NONE', *, *, #25974, .F. ) ;
#13415 = CARTESIAN_POINT ( 'NONE',  ( 1.603475055217291612, 1.054977578535739369, -0.04573490813648244807 ) ) ;
#13416 = CARTESIAN_POINT ( 'NONE',  ( -1.614173228346456268, -0.6692913385826771977, 8.415575281601705876E-17 ) ) ;
#13417 = CARTESIAN_POINT ( 'NONE',  ( -1.469816272965878357, -0.6046776061558809534, -0.2411417322834644161 ) ) ;
#13418 = CARTESIAN_POINT ( 'NONE',  ( 1.227034120734908917, -0.6692913385826771977, 0.1292274648535927661 ) ) ;
#13419 = CARTESIAN_POINT ( 'NONE',  ( 0.1958661417322834775, 0.3392501089628018884, -1.961286089238845287 ) ) ;
#13420 = CARTESIAN_POINT ( 'NONE',  ( 1.673228346456693494, 0.07958543189024085140, 0.2665933059059887866 ) ) ;
#13421 = EDGE_CURVE ( 'NONE', #11477, #59797, #78828, .T. ) ;
#13422 = CARTESIAN_POINT ( 'NONE',  ( 0.5052493438320218022, -0.6692913385826773087, -0.1292274648535924053 ) ) ;
#13423 = CARTESIAN_POINT ( 'NONE',  ( -0.1640419947506553400, -0.05778040916215560624, -0.4822834645669293319 ) ) ;
#13424 = CARTESIAN_POINT ( 'NONE',  ( -0.6983222978630787559, 2.320010949979154579E-15, 0.4281993546915509041 ) ) ;
#13425 = CARTESIAN_POINT ( 'NONE',  ( 0.2925321140481931814, 0.2925321140481931814, -2.734251968503936592 ) ) ;
#13426 = CARTESIAN_POINT ( 'NONE',  ( 0.9711286089238851948, 0.1283753931104748280, 0.1820866141732283561 ) ) ;
#13427 = CARTESIAN_POINT ( 'NONE',  ( -0.3460692066303960868, 0.1998031496062990242, -1.128608923884514503 ) ) ;
#13428 = ORIENTED_EDGE ( 'NONE', *, *, #6791, .T. ) ;
#13429 = CARTESIAN_POINT ( 'NONE',  ( 0.3392501089628018329, 0.1958661417322835607, 0.02950824327327895152 ) ) ;
#13430 = ORIENTED_EDGE ( 'NONE', *, *, #40727, .T. ) ;
#13431 = CARTESIAN_POINT ( 'NONE',  ( -0.1968503937007867743, -0.6692913385826771977, 8.415575281601705876E-17 ) ) ;
#13432 = CARTESIAN_POINT ( 'NONE',  ( -1.476377952755905110, 0.1660481256975885056, 0.3530559997133364547 ) ) ;
#13433 = CARTESIAN_POINT ( 'NONE',  ( 0.4461942257217856311, 0.2306618581243847221, -0.2411417322834647770 ) ) ;
#13434 = CARTESIAN_POINT ( 'NONE',  ( 1.377952755905512472, 0.2952755905511811885, 0.000000000000000000 ) ) ;
#13435 = CARTESIAN_POINT ( 'NONE',  ( 1.443569553805774897, 0.2306618581243848609, 0.2411417322834645549 ) ) ;
#13436 = CARTESIAN_POINT ( 'NONE',  ( -0.6627296587926501115, 0.2952755905511810774, -0.1292274648535930714 ) ) ;
#13437 = CARTESIAN_POINT ( 'NONE',  ( 0.1377952755905518800, -0.5400638737290844871, 0.3530559997133364547 ) ) ;
#13438 = CARTESIAN_POINT ( 'NONE',  ( 1.410761154855643795, -0.3162353388693405765, 0.4822834645669290543 ) ) ;
#13439 = CARTESIAN_POINT ( 'NONE',  ( 1.528871391076116026, -0.6692913385826773087, -0.1292274648535924053 ) ) ;
#13440 = CARTESIAN_POINT ( 'NONE',  ( 1.017060367454068803, -0.3162353388693405765, 0.4822834645669290543 ) ) ;
#13441 = CARTESIAN_POINT ( 'NONE',  ( -0.1377952755905504645, 0.1660481256975885056, 0.3530559997133364547 ) ) ;
#13442 = CARTESIAN_POINT ( 'NONE',  ( -0.1049643490035307020, 0.3917322834645669549, -0.1561679790026246351 ) ) ;
#13443 = CARTESIAN_POINT ( 'NONE',  ( 0.2559055118110243332, 0.07958543189024085140, 0.2665933059059887866 ) ) ;
#13444 = ORIENTED_EDGE ( 'NONE', *, *, #61281, .F. ) ;
#13445 = CARTESIAN_POINT ( 'NONE',  ( 0.3949938075777411073, -0.1058382717557499464, -0.7414698162729659314 ) ) ;
#13446 = ORIENTED_EDGE ( 'NONE', *, *, #70713, .F. ) ;
#13447 = CARTESIAN_POINT ( 'NONE',  ( -0.6299212598425188991, -0.1870078740157479769, 0.3641732283464567677 ) ) ;
#13448 = CARTESIAN_POINT ( 'NONE',  ( -0.4724409448818898682, -8.678599364036362592E-17, -0.1968503937007874127 ) ) ;
#13449 = CARTESIAN_POINT ( 'NONE',  ( 0.1312335958005255154, -0.6046776061558807314, 0.2411417322834647770 ) ) ;
#13450 = CARTESIAN_POINT ( 'NONE',  ( -0.2034120734908131112, -0.6692913385826773087, -0.1292274648535924053 ) ) ;
#13451 = CARTESIAN_POINT ( 'NONE',  ( -1.076115485564303809, 0.2306618581243848609, 0.2411417322834645549 ) ) ;
#13452 = CARTESIAN_POINT ( 'NONE',  ( 0.3392501089628018329, 0.1958661417322835607, -1.545294906333020135 ) ) ;
#13453 = CARTESIAN_POINT ( 'NONE',  ( -1.522309711286088607, -0.6046776061558807314, 0.2411417322834647770 ) ) ;
#13454 = CARTESIAN_POINT ( 'NONE',  ( -0.1459841489473561460, -2.624320362099288585E-15, 0.3791475997938241749 ) ) ;
#13455 = CARTESIAN_POINT ( 'NONE',  ( 0.9908136482939640111, 0.1771653543307087075, -0.09757992244046823083 ) ) ;
#13456 = CARTESIAN_POINT ( 'NONE',  ( 0.3937007874015754361, -0.1870078740157479769, 0.4822834645669291653 ) ) ;
#13457 = CARTESIAN_POINT ( 'NONE',  ( 0.8661417322834653598, -0.1870078740157479769, 0.4822834645669291653 ) ) ;
#13458 = CARTESIAN_POINT ( 'NONE',  ( 0.3996062992125986035, 0.1070741851644054776, -1.384514435695537671 ) ) ;
#13459 = CARTESIAN_POINT ( 'NONE',  ( -2.558921551581103682, 1.580736828574225594, 0.4725026149319433433 ) ) ;
#13460 = CARTESIAN_POINT ( 'NONE',  ( 4.893765752498283308E-17, -0.3996062992125985480, -0.9429133858267716439 ) ) ;
#13461 = CARTESIAN_POINT ( 'NONE',  ( 4.893765752498283308E-17, -0.3996062992125985480, -0.3129921259842520231 ) ) ;
#13462 = CARTESIAN_POINT ( 'NONE',  ( -0.09186351706036689768, 0.05413385826771626580, -0.4176697321401330321 ) ) ;
#13463 = CARTESIAN_POINT ( 'NONE',  ( -0.2925321140481932924, 0.2925321140481931814, -2.539370078740157410 ) ) ;
#13464 = CARTESIAN_POINT ( 'NONE',  ( 0.1958661417322836440, -0.3392501089628017219, -1.908792650918635259 ) ) ;
#13465 = CARTESIAN_POINT ( 'NONE',  ( -1.299212598425196097, 0.1771653543307087630, 0.000000000000000000 ) ) ;
#13466 = CARTESIAN_POINT ( 'NONE',  ( 1.332020997375328974, -0.05778040916215560624, -0.4822834645669293319 ) ) ;
#13467 = CARTESIAN_POINT ( 'NONE',  ( 1.154855643044620184, -0.6046776061558807314, 0.2411417322834647770 ) ) ;
#13468 = CARTESIAN_POINT ( 'NONE',  ( 0.2493438320209980519, -0.004921259842519576551, 0.3153832671262227771 ) ) ;
#13469 = CARTESIAN_POINT ( 'NONE',  ( 0.5774278215223103139, -0.6046776061558809534, -0.2411417322834644161 ) ) ;
#13470 = CARTESIAN_POINT ( 'NONE',  ( 0.3458507752293908943, -0.3458507752293908943, -1.435039370078740051 ) ) ;
#13471 = CARTESIAN_POINT ( 'NONE',  ( 0.3805774278215230400, -0.3690944881889763329, 0.3153832671262228327 ) ) ;
#13472 = CARTESIAN_POINT ( 'NONE',  ( -0.006561679790025524116, -0.3162353388693405765, 0.4822834645669290543 ) ) ;
#13473 = CARTESIAN_POINT ( 'NONE',  ( 0.3949938075777409963, 2.418639510665530743E-17, -1.454724409448818756 ) ) ;
#13474 = CARTESIAN_POINT ( 'NONE',  ( -1.410761154855642463, -0.05778040916215522460, 0.4822834645669289988 ) ) ;
#13475 = CARTESIAN_POINT ( 'NONE',  ( 0.4658792650918640033, -0.2845877964562159024, 0.3641732283464567677 ) ) ;
#13476 = DIRECTION ( 'NONE',  ( -3.491481338843132961E-15, -0.000000000000000000, 1.000000000000000000 ) ) ;
#13477 = CARTESIAN_POINT ( 'NONE',  ( -0.6167979002624665030, 0.05413385826771666132, 0.4176697321401328100 ) ) ;
#13478 = CARTESIAN_POINT ( 'NONE',  ( -0.2034120734908128059, 0.1771653543307087630, 0.09757992244046791164 ) ) ;
#13479 = CARTESIAN_POINT ( 'NONE',  ( 3.197598474799423496, 2.742783277647742324, 0.5314960629921260393 ) ) ;
#13480 = CARTESIAN_POINT ( 'NONE',  ( -0.9251968503937002541, 0.1660481256975885056, 0.3530559997133364547 ) ) ;
#13481 = CARTESIAN_POINT ( 'NONE',  ( -0.1968503937007867743, 0.2952755905511811885, 0.000000000000000000 ) ) ;
#13482 = CARTESIAN_POINT ( 'NONE',  ( 0.1640419947506569498, -0.08942795157527998196, 0.3641732283464567121 ) ) ;
#13483 = CARTESIAN_POINT ( 'NONE',  ( 0.1070741851644053388, 0.3996062992125986035, -2.117454068241469756 ) ) ;
#13484 = CARTESIAN_POINT ( 'NONE',  ( 0.07217847769028949700, -0.3162353388693405765, 0.4822834645669290543 ) ) ;
#13485 = EDGE_CURVE ( 'NONE', #44548, #7361, #74807, .T. ) ;
#13486 = CARTESIAN_POINT ( 'NONE',  ( 0.2867679344610365999, -0.2867679344610365999, -2.225702468995064187 ) ) ;
#13487 = CARTESIAN_POINT ( 'NONE',  ( 0.7545931758530189937, 0.1771653543307087075, -0.09757992244046823083 ) ) ;
#13488 = CARTESIAN_POINT ( 'NONE',  ( 1.259842519685040019, -0.1870078740157479769, 0.4822834645669291653 ) ) ;
#13489 = CARTESIAN_POINT ( 'NONE',  ( -0.8333333333333323711, -0.5511811023622048555, -0.09757992244046775898 ) ) ;
#13490 = CARTESIAN_POINT ( 'NONE',  ( -1.332020997375327642, -0.2845877964562161244, -0.3641732283464567121 ) ) ;
#13491 = CARTESIAN_POINT ( 'NONE',  ( -0.6299212598425188991, -0.1870078740157480879, -0.4822834645669291653 ) ) ;
#13492 = CARTESIAN_POINT ( 'NONE',  ( -0.01312335958005186876, -0.4281496062992124485, 0.4176697321401328655 ) ) ;
#13493 = CARTESIAN_POINT ( 'NONE',  ( 0.3740157480314966754, -0.4536011799217367080, 0.2665933059059888421 ) ) ;
#13494 = CARTESIAN_POINT ( 'NONE',  ( -0.4724409448818899238, 0.1265901696524986964, -2.395013123359579943 ) ) ;
#13495 = CARTESIAN_POINT ( 'NONE',  ( 1.017060367454068581, -0.08942795157528024563, -0.3641732283464568787 ) ) ;
#13496 = CARTESIAN_POINT ( 'NONE',  ( 0.4461942257217856311, 0.2306618581243847221, -0.2411417322834647770 ) ) ;
#13497 = CARTESIAN_POINT ( 'NONE',  ( 0.3996062992125986035, -0.1070741851644052972, 0.1266404199475065218 ) ) ;
#13498 = CARTESIAN_POINT ( 'NONE',  ( -0.2887139107611542133, 0.2306618581243848609, 0.2411417322834645549 ) ) ;
#13499 = CARTESIAN_POINT ( 'NONE',  ( 0.3392501089628018329, 0.1958661417322835607, -1.318241469816273215 ) ) ;
#13500 = CARTESIAN_POINT ( 'NONE',  ( -1.699475065616797398, 0.2952755905511811885, 0.1292274648535926551 ) ) ;
#13501 = CARTESIAN_POINT ( 'NONE',  ( 0.4593175853018380828, 0.05413385826771626580, -0.4176697321401330321 ) ) ;
#13502 = CARTESIAN_POINT ( 'NONE',  ( 0.2165354330708668673, -0.5400638737290844871, 0.3530559997133364547 ) ) ;
#13503 = CARTESIAN_POINT ( 'NONE',  ( 0.000000000000000000, 0.03937007874015751446, -2.362204724409448620 ) ) ;
#13504 = CARTESIAN_POINT ( 'NONE',  ( 0.1640419947506569498, -0.2845877964562161244, -0.3641732283464567121 ) ) ;
#13505 = CARTESIAN_POINT ( 'NONE',  ( 0.6496062992125991586, -0.5400638737290845981, -0.3530559997133363437 ) ) ;
#13506 = CARTESIAN_POINT ( 'NONE',  ( -0.3871391076115479057, -0.2845877964562161244, -0.3641732283464567121 ) ) ;
#13507 = CARTESIAN_POINT ( 'NONE',  ( -0.7020997375328074108, -0.05778040916215522460, 0.4822834645669289988 ) ) ;
#13508 = DIRECTION ( 'NONE',  ( 0.000000000000000000, 0.000000000000000000, -1.000000000000000000 ) ) ;
#13509 = CARTESIAN_POINT ( 'NONE',  ( 0.04593175853018440641, 0.2952755905511810774, -0.1292274648535930714 ) ) ;
#13510 = VERTEX_POINT ( 'NONE', #46810 ) ;
#13511 = CARTESIAN_POINT ( 'NONE',  ( -1.010498687664041384, 0.05413385826771666132, 0.4176697321401328100 ) ) ;
#13512 = CARTESIAN_POINT ( 'NONE',  ( -0.5708661417322828946, 0.07958543189024071263, -0.2665933059059888421 ) ) ;
#13513 = CARTESIAN_POINT ( 'NONE',  ( 0.01312335958005323398, 0.05413385826771666132, 0.4176697321401328100 ) ) ;
#13514 = CARTESIAN_POINT ( 'NONE',  ( -1.325459317585300889, -0.4281496062992127816, -0.4176697321401328100 ) ) ;
#13515 = CARTESIAN_POINT ( 'NONE',  ( -0.8792650918635160906, -0.4281496062992124485, 0.4176697321401328655 ) ) ;
#13516 =( BOUNDED_CURVE ( )  B_SPLINE_CURVE ( 2, ( #76210, #49282, #23201, #43361, #68258, #18139, #69062, #10594, #82118, #56824, #69476, #35844, #74572 ),
 .UNSPECIFIED., .F., .F. ) 
 B_SPLINE_CURVE_WITH_KNOTS ( ( 3, 2, 2, 2, 2, 2, 3 ),
 ( 0.4467605387524145044, 0.4469696969696969613, 0.4507575757575757458, 0.4545454545454545303, 0.4583333333333333148, 0.4621212121212120993, 0.4623303703384945562 ),
 .UNSPECIFIED. ) 
 CURVE ( )  GEOMETRIC_REPRESENTATION_ITEM ( )  RATIONAL_B_SPLINE_CURVE ( ( 0.9964447847208428577, 0.9981185001348096275, 1.000000000000000000, 0.9659258262890683122, 1.000000000000000000, 0.9659258262890683122, 1.000000000000000000, 0.9659258262890683122, 1.000000000000000000, 0.9659258262890683122, 1.000000000000000000, 0.9981185001348097385, 0.9964447847208430797 ) ) 
 REPRESENTATION_ITEM ( '' )  );
#13517 = DIRECTION ( 'NONE',  ( 1.000000000000000000, -0.000000000000000000, -0.000000000000000000 ) ) ;
#13519 = CARTESIAN_POINT ( 'NONE',  ( 1.555118110236221041, -0.5400638737290844871, 0.3530559997133364547 ) ) ;
#13518 = CARTESIAN_POINT ( 'NONE',  ( 1.035207913594496709, 0.02791078216816225699, 0.4328096321851905293 ) ) ;
#13520 = CARTESIAN_POINT ( 'NONE',  ( 1.207349081364829990, 0.2306618581243848609, 0.2411417322834645549 ) ) ;
#13521 = CARTESIAN_POINT ( 'NONE',  ( -0.3917322834645671215, 0.1049643490035301469, -2.544619422572177658 ) ) ;
#13522 = DIRECTION ( 'NONE',  ( 0.000000000000000000, 0.000000000000000000, 1.000000000000000000 ) ) ;
#13523 = CARTESIAN_POINT ( 'NONE',  ( -1.174540682414697335, -0.3162353388693409650, -0.4822834645669289433 ) ) ;
#13524 = CARTESIAN_POINT ( 'NONE',  ( -0.2362204724409451284, 0.4091458600556402425, -0.9580052493438320216 ) ) ;
#13525 = CARTESIAN_POINT ( 'NONE',  ( -0.2925321140481932924, 0.2925321140481931814, -0.1771653543307087075 ) ) ;
#13526 = ORIENTED_EDGE ( 'NONE', *, *, #32799, .T. ) ;
#13527 = CARTESIAN_POINT ( 'NONE',  ( -0.1706036745406816491, -0.004921259842519870586, -0.3153832671262229437 ) ) ;
#13528 = CARTESIAN_POINT ( 'NONE',  ( -0.3917322834645670104, -7.196005306013484475E-17, -1.921259842519684957 ) ) ;
#13529 = ORIENTED_EDGE ( 'NONE', *, *, #12532, .T. ) ;
#13530 = CARTESIAN_POINT ( 'NONE',  ( 0.3477690288713918276, 0.2952755905511811885, 0.1292274648535926551 ) ) ;
#13531 = CARTESIAN_POINT ( 'NONE',  ( 0.3477690288713918276, 0.2952755905511811885, 0.1292274648535926551 ) ) ;
#13532 = CARTESIAN_POINT ( 'NONE',  ( -0.4091458600556405756, 0.2362204724409446288, -2.860892388451443669 ) ) ;
#13533 = CARTESIAN_POINT ( 'NONE',  ( -0.5387615594602663815, -2.294479370626195693E-15, 0.3464511005275217603 ) ) ;
#13534 = CARTESIAN_POINT ( 'NONE',  ( -0.7939632545931750718, -0.08942795157528024563, -0.3641732283464568787 ) ) ;
#13535 = DIRECTION ( 'NONE',  ( 1.000000000000000000, -0.000000000000000000, -0.000000000000000000 ) ) ;
#13536 = CARTESIAN_POINT ( 'NONE',  ( 0.8398950131233602345, -0.6046776061558807314, 0.2411417322834647770 ) ) ;
#13537 = CARTESIAN_POINT ( 'NONE',  ( 0.8530183727034126306, -0.004921259842519870586, -0.3153832671262229437 ) ) ;
#13538 = CIRCLE ( 'NONE', #39054, 3.543307086614174484 ) ;
#13539 = CARTESIAN_POINT ( 'NONE',  ( -0.2165354330708654795, 0.1660481256975885056, 0.3530559997133364547 ) ) ;
#13540 = CARTESIAN_POINT ( 'NONE',  ( -0.3917322834645668994, -0.1049643490035306742, -1.228327140911074089 ) ) ;
#13541 = CARTESIAN_POINT ( 'NONE',  ( -0.9383202099737524282, -0.3162353388693409650, -0.4822834645669289433 ) ) ;
#13542 = CARTESIAN_POINT ( 'NONE',  ( -1.614173228346456268, -0.5511811023622047445, 6.969142054262312111E-17 ) ) ;
#13543 = CARTESIAN_POINT ( 'NONE',  ( -0.8595800524934373854, -0.3162353388693409650, -0.4822834645669289433 ) ) ;
#13544 = CARTESIAN_POINT ( 'NONE',  ( 1.377952755905512472, 0.2952755905511811885, 0.000000000000000000 ) ) ;
#13545 = CARTESIAN_POINT ( 'NONE',  ( 1.692913385826772421, 0.1771653543307087630, 0.000000000000000000 ) ) ;
#13546 = ORIENTED_EDGE ( 'NONE', *, *, #8916, .F. ) ;
#13547 = CARTESIAN_POINT ( 'NONE',  ( 0.2867679344610366554, -0.2867679344610365999, -2.457368397146668659 ) ) ;
#13548 = CARTESIAN_POINT ( 'NONE',  ( -0.01968503937007793844, 0.1660481256975883668, -0.3530559997133364547 ) ) ;
#13549 = EDGE_LOOP ( 'NONE', ( #81596, #34769, #54072, #38979 ) ) ;
#13550 = CARTESIAN_POINT ( 'NONE',  ( -0.7414698162729651543, 0.2952755905511810774, -0.1292274648535930714 ) ) ;
#13551 = CARTESIAN_POINT ( 'NONE',  ( 1.450131233595801428, 0.2952755905511811885, 0.1292274648535926551 ) ) ;
#13552 = CARTESIAN_POINT ( 'NONE',  ( 1.200787401574803681, -0.5400638737290845981, -0.3530559997133363437 ) ) ;
#13553 = CARTESIAN_POINT ( 'NONE',  ( 0.4593175853018379162, -0.4281496062992124485, 0.4176697321401328655 ) ) ;
#13554 = CARTESIAN_POINT ( 'NONE',  ( -0.06561679790026180015, 0.05413385826771666132, 0.4176697321401328100 ) ) ;
#13555 = CARTESIAN_POINT ( 'NONE',  ( 0.2867679344610365999, -0.2867679344610365444, -1.757874015748031260 ) ) ;
#13556 = CARTESIAN_POINT ( 'NONE',  ( -1.325459317585300889, -0.4281496062992127816, -0.4176697321401328100 ) ) ;
#13557 = CARTESIAN_POINT ( 'NONE',  ( -0.2690288713910754526, -0.6692913385826771977, 0.1292274648535927661 ) ) ;
#13558 = CARTESIAN_POINT ( 'NONE',  ( -0.2296587926509179312, -0.08942795157527998196, 0.3641732283464567121 ) ) ;
#13559 = CARTESIAN_POINT ( 'NONE',  ( 1.627296587926509996, -0.6046776061558807314, 0.2411417322834647770 ) ) ;
#13560 = CONICAL_SURFACE ( 'NONE', #18947, 0.2755905511811031494, 0.7853981633974284060 ) ;
#13561 = EDGE_CURVE ( 'NONE', #4806, #15637, #27878, .T. ) ;
#13562 = CARTESIAN_POINT ( 'NONE',  ( 1.469816272965879911, -0.6046776061558807314, 0.2411417322834647770 ) ) ;
#13563 = CARTESIAN_POINT ( 'NONE',  ( -0.3018372703412066094, 0.05413385826771666132, 0.4176697321401328100 ) ) ;
#13564 = CARTESIAN_POINT ( 'NONE',  ( 0.000000000000000000, 0.000000000000000000, -1.512162153811850596 ) ) ;
#13565 = CARTESIAN_POINT ( 'NONE',  ( 1.161417322834646271, 0.1660481256975883668, -0.3530559997133364547 ) ) ;
#13566 = CARTESIAN_POINT ( 'NONE',  ( -0.4724409448818898682, 5.785732909357575061E-17, -2.755905511811024056 ) ) ;
#13567 = VERTEX_POINT ( 'NONE', #67432 ) ;
#13568 = EDGE_CURVE ( 'NONE', #82899, #22644, #18587, .T. ) ;
#13569 = ORIENTED_EDGE ( 'NONE', *, *, #57395, .T. ) ;
#13570 = CARTESIAN_POINT ( 'NONE',  ( 0.2755905511811031494, 0.2952755905511811885, 0.000000000000000000 ) ) ;
#13571 = CARTESIAN_POINT ( 'NONE',  ( -0.1640419947506555343, -0.2845877964562159024, 0.3641732283464567677 ) ) ;
#13573 = CARTESIAN_POINT ( 'NONE',  ( -0.7535225988626923499, 2.401574803149606474, -0.4915354330708644470 ) ) ;
#13572 = CARTESIAN_POINT ( 'NONE',  ( 1.358267716535433323, 0.07958543189024085140, 0.2665933059059887866 ) ) ;
#13574 = CARTESIAN_POINT ( 'NONE',  ( -0.4724409448818898682, -8.678599364036362592E-17, -0.4311023622047244208 ) ) ;
#13575 = CARTESIAN_POINT ( 'NONE',  ( 1.548556430446194954, 0.1283753931104746893, -0.1820866141732285504 ) ) ;
#13576 = CARTESIAN_POINT ( 'NONE',  ( 1.181102362204724976, -0.1870078740157480879, -0.4822834645669291653 ) ) ;
#13577 = CARTESIAN_POINT ( 'NONE',  ( 0.3949938075777409963, 2.418639510665530743E-17, -0.3523622047244094335 ) ) ;
#13578 = CARTESIAN_POINT ( 'NONE',  ( 0.1181102362204730916, -0.6692913385826771977, 8.415575281601705876E-17 ) ) ;
#13579 = CARTESIAN_POINT ( 'NONE',  ( -1.476377952755905110, 0.1660481256975885056, 0.3530559997133364547 ) ) ;
#13580 = CARTESIAN_POINT ( 'NONE',  ( -1.692913385826770645, 0.2952755905511811885, 0.000000000000000000 ) ) ;
#13581 = CARTESIAN_POINT ( 'NONE',  ( -0.2296587926509179312, -0.3162353388693409650, -0.4822834645669289433 ) ) ;
#13582 = CARTESIAN_POINT ( 'NONE',  ( -0.1058382717557497660, -0.3949938075777411073, 0.008530183727034110208 ) ) ;
#13583 = CARTESIAN_POINT ( 'NONE',  ( -1.502624671916009680, -0.2845877964562159024, 0.3641732283464567677 ) ) ;
#13584 = CARTESIAN_POINT ( 'NONE',  ( 0.3215223097112867578, -0.05778040916215522460, 0.4822834645669289988 ) ) ;
#13585 = CARTESIAN_POINT ( 'NONE',  ( 0.9711286089238851948, -0.5023911411419708095, -0.1820866141732282451 ) ) ;
#13586 = CARTESIAN_POINT ( 'NONE',  ( -0.06715429112991272431, 0.02791078216816064370, 0.4328096321851915285 ) ) ;
#13587 = CARTESIAN_POINT ( 'NONE',  ( 0.7414698162729663755, 0.1771653543307087630, 0.09757992244046791164 ) ) ;
#13588 = CARTESIAN_POINT ( 'NONE',  ( -1.174540682414697335, -0.05778040916215522460, 0.4822834645669289988 ) ) ;
#13589 = CARTESIAN_POINT ( 'NONE',  ( 0.3996062992125985480, 2.446882876249141654E-17, -0.9822834645669291653 ) ) ;
#13590 = CARTESIAN_POINT ( 'NONE',  ( 1.108923884514436686, -0.3162353388693409650, -0.4822834645669289433 ) ) ;
#13591 = EDGE_CURVE ( 'NONE', #70661, #67145, #54367, .T. ) ;
#13592 = CARTESIAN_POINT ( 'NONE',  ( -0.3917322834645669549, -0.1049643490035306603, -0.5104986876640419391 ) ) ;
#13593 = EDGE_CURVE ( 'NONE', #2797, #5054, #49294, .T. ) ;
#13595 = CARTESIAN_POINT ( 'NONE',  ( 0.9055118110236227702, 0.2952755905511811885, 0.000000000000000000 ) ) ;
#13594 = CARTESIAN_POINT ( 'NONE',  ( 0.6889763779527566800, -0.5400638737290844871, 0.3530559997133364547 ) ) ;
#13596 = CARTESIAN_POINT ( 'NONE',  ( -0.3346456692913378217, 0.1012011053420775880, -0.2882089793578256898 ) ) ;
#13597 = CARTESIAN_POINT ( 'NONE',  ( 0.5314960629921264834, 0.07958543189024071263, -0.2665933059059888421 ) ) ;
#13598 = CARTESIAN_POINT ( 'NONE',  ( 0.4133858267716541968, 0.1660481256975885056, 0.3530559997133364547 ) ) ;
#13599 = CARTESIAN_POINT ( 'NONE',  ( -0.9285414500055708675, 1.724409448818898127, -0.6299212598425202314 ) ) ;
#13600 = CARTESIAN_POINT ( 'NONE',  ( -1.122047244094487306, -0.4536011799217367080, 0.2665933059059888421 ) ) ;
#13601 = CARTESIAN_POINT ( 'NONE',  ( -0.8136482939632537770, -0.6046776061558807314, 0.2411417322834647770 ) ) ;
#13602 = CARTESIAN_POINT ( 'NONE',  ( 1.135170603674541256, -0.6692913385826773087, -0.1292274648535924053 ) ) ;
#13603 = CARTESIAN_POINT ( 'NONE',  ( -1.076115485564303809, 0.2306618581243848609, 0.2411417322834645549 ) ) ;
#13604 = CARTESIAN_POINT ( 'NONE',  ( 0.8398950131233602345, -0.6046776061558807314, 0.2411417322834647770 ) ) ;
#13605 = CARTESIAN_POINT ( 'NONE',  ( -1.167979002624671470, -0.004921259842519576551, 0.3153832671262227771 ) ) ;
#13606 = DIRECTION ( 'NONE',  ( 1.000000000000000000, -0.000000000000000000, -0.000000000000000000 ) ) ;
#13607 = CARTESIAN_POINT ( 'NONE',  ( 1.076115485564305141, -0.6046776061558807314, 0.2411417322834647770 ) ) ;
#13608 = CARTESIAN_POINT ( 'NONE',  ( -0.2362204724409451284, 0.4091458600556402425, -2.609580052493438274 ) ) ;
#13609 = CARTESIAN_POINT ( 'NONE',  ( 1.633858267716535639, -0.5400638737290844871, 0.3530559997133364547 ) ) ;
#13610 = CARTESIAN_POINT ( 'NONE',  ( 1.509186351706037543, 0.05413385826771666132, 0.4176697321401328100 ) ) ;
#13611 = CARTESIAN_POINT ( 'NONE',  ( -1.620734908136482577, -0.5511811023622048555, -0.09757992244046775898 ) ) ;
#13612 = CARTESIAN_POINT ( 'NONE',  ( 1.450131233595801428, -0.5511811023622048555, -0.09757992244046775898 ) ) ;
#13613 = CARTESIAN_POINT ( 'NONE',  ( -1.108923884514435132, -0.08942795157528024563, -0.3641732283464568787 ) ) ;
#13614 = CARTESIAN_POINT ( 'NONE',  ( -0.4724409448818890911, -0.1870078740157480601, -0.3641732283464567677 ) ) ;
#13615 = CARTESIAN_POINT ( 'NONE',  ( -1.423884514435694859, -0.2845877964562159024, 0.3641732283464567677 ) ) ;
#13616 = CARTESIAN_POINT ( 'NONE',  ( 0.9186351706036751663, -0.5023911411419708095, 0.1820866141732285504 ) ) ;
#13617 = CARTESIAN_POINT ( 'NONE',  ( 0.6627296587926517768, -0.6692913385826773087, -0.1292274648535924053 ) ) ;
#13618 = CARTESIAN_POINT ( 'NONE',  ( 1.049868766404200127, -0.6046776061558809534, -0.2411417322834644161 ) ) ;
#13619 = CARTESIAN_POINT ( 'NONE',  ( 0.1706036745406830368, -0.4281496062992127816, -0.4176697321401328100 ) ) ;
#13620 = ADVANCED_FACE ( 'NONE', ( #17340 ), #42995, .F. ) ;
#13621 = AXIS2_PLACEMENT_3D ( 'NONE', #65768, #7688, #71235 ) ;
#13622 = CARTESIAN_POINT ( 'NONE',  ( 0.7020997375328090762, -0.08942795157528024563, -0.3641732283464568787 ) ) ;
#13623 = CARTESIAN_POINT ( 'NONE',  ( 1.528871391076116026, -0.6692913385826773087, -0.1292274648535924053 ) ) ;
#13624 = CARTESIAN_POINT ( 'NONE',  ( -1.541994750656167090, -0.6692913385826773087, -0.1292274648535924053 ) ) ;
#13625 = CARTESIAN_POINT ( 'NONE',  ( -0.5314960629921254842, -0.5400638737290845981, -0.3530559997133363437 ) ) ;
#13626 = CARTESIAN_POINT ( 'NONE',  ( 0.1070741851644054915, -0.3996062992125985480, -0.5577427821522309426 ) ) ;
#13627 = CARTESIAN_POINT ( 'NONE',  ( -1.157146581871515012E-16, 0.4724409448818898682, -1.179133858267716661 ) ) ;
#13628 = CARTESIAN_POINT ( 'NONE',  ( 0.1574803149606306130, -0.1870078740157479769, 0.4822834645669291653 ) ) ;
#13629 = CARTESIAN_POINT ( 'NONE',  ( -0.4330708661417315697, -0.6692913385826771977, 8.415575281601705876E-17 ) ) ;
#13630 = CARTESIAN_POINT ( 'NONE',  ( -0.04593175853018302557, -0.6692913385826773087, -0.1292274648535924053 ) ) ;
#13631 = CARTESIAN_POINT ( 'NONE',  ( -0.1998031496062994683, 0.3460692066303958092, -2.690288713910760965 ) ) ;
#13632 = CARTESIAN_POINT ( 'NONE',  ( -0.1058382717557503211, 0.3949938075777409408, -1.738845144356955696 ) ) ;
#13633 = CARTESIAN_POINT ( 'NONE',  ( -0.1958661417322834220, -0.3392501089628018884, -0.5301837270341206443 ) ) ;
#13634 = CARTESIAN_POINT ( 'NONE',  ( 2.795275590551181466, 2.001539355558160871, 0.000000000000000000 ) ) ;
#13635 = CARTESIAN_POINT ( 'NONE',  ( 0.1049643490035304799, -0.3917322834645669549, -1.179790026246718915 ) ) ;
#13636 = CARTESIAN_POINT ( 'NONE',  ( -0.7545931758530177724, 0.1771653543307087630, 0.09757992244046791164 ) ) ;
#13637 = CARTESIAN_POINT ( 'NONE',  ( -0.2867679344610365999, 0.2867679344610364889, -1.114173228346456712 ) ) ;
#13638 = CARTESIAN_POINT ( 'NONE',  ( -1.128608923884513837, -0.6046776061558807314, 0.2411417322834647770 ) ) ;
#13639 = CARTESIAN_POINT ( 'NONE',  ( 0.1058382717557500852, -0.3949938075777408852, -2.839238845144357093 ) ) ;
#13640 = EDGE_CURVE ( 'NONE', #23562, #14913, #77783, .T. ) ;
#13641 = CARTESIAN_POINT ( 'NONE',  ( 0.2427821522309719648, -0.05778040916215522460, 0.4822834645669289988 ) ) ;
#13642 = CARTESIAN_POINT ( 'NONE',  ( -0.2099737532808391705, -0.5023911411419708095, -0.1820866141732282451 ) ) ;
#13643 = CARTESIAN_POINT ( 'NONE',  ( 1.207349081364829990, -0.6046776061558809534, -0.2411417322834644161 ) ) ;
#13644 = CARTESIAN_POINT ( 'NONE',  ( 0.2559055118110243332, -0.5400638737290845981, -0.3530559997133363437 ) ) ;
#13645 = CARTESIAN_POINT ( 'NONE',  ( -0.4697243008124643016, 1.606021484273580935, -2.158901635429134380 ) ) ;
#13646 = CARTESIAN_POINT ( 'NONE',  ( -0.3460692066303960868, 0.1998031496062990242, -2.703412073490813583 ) ) ;
#13647 = CARTESIAN_POINT ( 'NONE',  ( 0.3917322834645670104, 0.1049643490035304660, -1.381252911582363962 ) ) ;
#13648 = CARTESIAN_POINT ( 'NONE',  ( 1.108923884514436686, -0.3162353388693409650, -0.4822834645669289433 ) ) ;
#13649 = CARTESIAN_POINT ( 'NONE',  ( 0.3608923884514443348, 0.2952755905511810774, -0.1292274648535930714 ) ) ;
#13650 = CARTESIAN_POINT ( 'NONE',  ( 0.1377952755905518800, -0.5400638737290844871, 0.3530559997133364547 ) ) ;
#13651 = CARTESIAN_POINT ( 'NONE',  ( 1.489501312335958172, -0.3162353388693405765, 0.4822834645669290543 ) ) ;
#13652 = CARTESIAN_POINT ( 'NONE',  ( 0.3392501089628018884, -0.1958661417322834220, -0.3471128608923885195 ) ) ;
#13653 = CARTESIAN_POINT ( 'NONE',  ( 0.06561679790026316017, 0.05413385826771626580, -0.4176697321401330321 ) ) ;
#13654 = CARTESIAN_POINT ( 'NONE',  ( 1.279527559055118724, -0.5400638737290845981, -0.3530559997133363437 ) ) ;
#13655 = CARTESIAN_POINT ( 'NONE',  ( 0.2493438320209980519, 0.05413385826771666132, 0.4176697321401328100 ) ) ;
#13656 = CARTESIAN_POINT ( 'NONE',  ( 1.181102362204725198, -0.1870078740157479769, 0.3641732283464567677 ) ) ;
#13657 = CARTESIAN_POINT ( 'NONE',  ( -0.9186351706036736120, 0.2306618581243848609, 0.2411417322834645549 ) ) ;
#13658 = CARTESIAN_POINT ( 'NONE',  ( -1.318897637795274802, -0.5400638737290845981, -0.3530559997133363437 ) ) ;
#13659 = AXIS2_PLACEMENT_3D ( 'NONE', #26280, #51941, #64179 ) ;
#13660 = CARTESIAN_POINT ( 'NONE',  ( 0.8202099737532813073, 0.2952755905511811885, 0.1292274648535926551 ) ) ;
#13661 = CARTESIAN_POINT ( 'NONE',  ( -0.2579773093923122262, -0.2955417804225481393, -1.929133858267716439 ) ) ;
#13662 = CARTESIAN_POINT ( 'NONE',  ( 0.1958661417322834775, 0.3392501089628018884, -2.026246719160105236 ) ) ;
#13663 = CARTESIAN_POINT ( 'NONE',  ( 1.660104986876641320, -0.05778040916215522460, 0.4822834645669289988 ) ) ;
#13664 = EDGE_CURVE ( 'NONE', #64696, #15345, #51655, .T. ) ;
#13665 = ORIENTED_EDGE ( 'NONE', *, *, #46544, .T. ) ;
#13666 = CARTESIAN_POINT ( 'NONE',  ( 0.2925321140481932369, 0.2925321140481932369, 0.01968503937007872254 ) ) ;
#13667 = ORIENTED_EDGE ( 'NONE', *, *, #40392, .F. ) ;
#13668 = CARTESIAN_POINT ( 'NONE',  ( 1.633858267716535639, -0.5400638737290844871, 0.3530559997133364547 ) ) ;
#13669 = CARTESIAN_POINT ( 'NONE',  ( 0.9711286089238851948, 0.1283753931104748280, 0.1820866141732283561 ) ) ;
#13670 = DIRECTION ( 'NONE',  ( 0.000000000000000000, 0.000000000000000000, -1.000000000000000000 ) ) ;
#13671 = LINE ( 'NONE', #26701, #75950 ) ;
#13672 = CARTESIAN_POINT ( 'NONE',  ( 0.1265901696524990572, -0.4724409448818897017, -1.187664041994750619 ) ) ;
#13673 = CARTESIAN_POINT ( 'NONE',  ( 0.1958661417322834775, 0.3392501089628018884, -1.016404199475065662 ) ) ;
#13674 = CARTESIAN_POINT ( 'NONE',  ( -1.299212598425196097, 0.1771653543307087630, 0.000000000000000000 ) ) ;
#13675 = CARTESIAN_POINT ( 'NONE',  ( 1.614173228346457378, 0.2952755905511811885, 0.000000000000000000 ) ) ;
#13676 = CARTESIAN_POINT ( 'NONE',  ( -1.515748031496062076, -0.5400638737290844871, 0.3530559997133364547 ) ) ;
#13677 = CARTESIAN_POINT ( 'NONE',  ( -0.1640419947506555343, -0.3162353388693405765, 0.4822834645669290543 ) ) ;
#13678 = CARTESIAN_POINT ( 'NONE',  ( 1.391076115485564868, -0.6046776061558807314, 0.2411417322834647770 ) ) ;
#13679 = EDGE_LOOP ( 'NONE', ( #75350, #26159, #68618, #27998 ) ) ;
#13680 = DIRECTION ( 'NONE',  ( -1.332267629550188539E-16, -1.000000000000000000, 0.000000000000000000 ) ) ;
#13681 = CARTESIAN_POINT ( 'NONE',  ( 0.2460629921259842590, 0.000000000000000000, 0.000000000000000000 ) ) ;
#13682 = DIRECTION ( 'NONE',  ( 0.000000000000000000, 1.000000000000000000, 0.000000000000000000 ) ) ;
#13683 = CARTESIAN_POINT ( 'NONE',  ( -0.7939632545931750718, -0.08942795157528024563, -0.3641732283464568787 ) ) ;
#13684 = CARTESIAN_POINT ( 'NONE',  ( -1.456692913385826182, 0.2952755905511811885, 0.000000000000000000 ) ) ;
#13685 = CARTESIAN_POINT ( 'NONE',  ( 0.6102362204724416372, 0.1660481256975883668, -0.3530559997133364547 ) ) ;
#13686 = ORIENTED_EDGE ( 'NONE', *, *, #54850, .T. ) ;
#13688 = CARTESIAN_POINT ( 'NONE',  ( 0.6962418744208975774, 2.409604939980833412E-17, -0.3464511005275205946 ) ) ;
#13687 = CARTESIAN_POINT ( 'NONE',  ( -1.646051170424378096, 0.000000000000000000, -0.3464511005275205946 ) ) ;
#13689 = CARTESIAN_POINT ( 'NONE',  ( 1.122047244094488860, -0.5400638737290845981, -0.3530559997133363437 ) ) ;
#13690 = CARTESIAN_POINT ( 'NONE',  ( -1.627296587926508442, -0.6046776061558809534, -0.2411417322834644161 ) ) ;
#13691 = CARTESIAN_POINT ( 'NONE',  ( -0.3392501089628018329, -0.1958661417322836440, -0.9199281907798407820 ) ) ;
#13692 = CARTESIAN_POINT ( 'NONE',  ( -0.4199475065616791736, 0.1283753931104746893, -0.1820866141732285504 ) ) ;
#13693 = CARTESIAN_POINT ( 'NONE',  ( -1.397637795275589623, -0.4536011799217368745, -0.2665933059059886201 ) ) ;
#13694 = CARTESIAN_POINT ( 'NONE',  ( -0.4724409448818898682, -8.678599364036362592E-17, -0.03937007874015747977 ) ) ;
#13695 = CARTESIAN_POINT ( 'NONE',  ( 0.3083989501312343062, -0.3162353388693405765, 0.4822834645669290543 ) ) ;
#13696 = CARTESIAN_POINT ( 'NONE',  ( -0.8858267716535425107, -0.4536011799217367080, 0.2665933059059888421 ) ) ;
#13697 = CARTESIAN_POINT ( 'NONE',  ( 0.01968503937007930540, 0.07958543189024085140, 0.2665933059059887866 ) ) ;
#13698 = CARTESIAN_POINT ( 'NONE',  ( 0.1771653543307093182, 0.1660481256975885056, 0.3530559997133364547 ) ) ;
#13699 = CARTESIAN_POINT ( 'NONE',  ( -0.9383202099737524282, -0.2845877964562161244, -0.3641732283464567121 ) ) ;
#13700 = CARTESIAN_POINT ( 'NONE',  ( -0.3392501089628017219, -0.1958661417322836995, -0.04923191420703601495 ) ) ;
#13701 = CARTESIAN_POINT ( 'NONE',  ( 0.7939632545931766261, -0.05778040916215522460, 0.4822834645669289988 ) ) ;
#13702 =( BOUNDED_CURVE ( )  B_SPLINE_CURVE ( 2, ( #21470, #66094, #47959, #21881, #2116, #8430, #73235, #22712, #15586, #2948, #54270, #73663, #40824 ),
 .UNSPECIFIED., .F., .F. ) 
 B_SPLINE_CURVE_WITH_KNOTS ( ( 3, 2, 2, 2, 2, 2, 3 ),
 ( 0.3125000000000000000, 0.3166666666666666519, 0.3208333333333333592, 0.3250000000000000111, 0.3291666666666666630, 0.3333333333333333148, 0.3375000000000000222 ),
 .UNSPECIFIED. ) 
 CURVE ( )  GEOMETRIC_REPRESENTATION_ITEM ( )  RATIONAL_B_SPLINE_CURVE ( ( 1.000000000000000000, 0.9659258262890683122, 1.000000000000000000, 0.9659258262890683122, 1.000000000000000000, 0.9659258262890683122, 1.000000000000000000, 0.9659258262890683122, 1.000000000000000000, 0.9659258262890683122, 1.000000000000000000, 0.9659258262890683122, 1.000000000000000000 ) ) 
 REPRESENTATION_ITEM ( '' )  );
#13703 = CARTESIAN_POINT ( 'NONE',  ( -1.614173228346455824, 0.2952755905511811885, 0.000000000000000000 ) ) ;
#13704 = CARTESIAN_POINT ( 'NONE',  ( 0.4724409448818896462, 0.1265901696524990294, -1.146325459317585116 ) ) ;
#13705 = CARTESIAN_POINT ( 'NONE',  ( -0.4724409448818890911, -0.1870078740157479769, 0.4822834645669291653 ) ) ;
#13706 = CARTESIAN_POINT ( 'NONE',  ( 0.2755905511811031494, -0.5511811023622047445, 6.969142054262312111E-17 ) ) ;
#13707 = EDGE_CURVE ( 'NONE', #55729, #33736, #19728, .T. ) ;
#13708 = CARTESIAN_POINT ( 'NONE',  ( -1.036745406824146176, -0.4281496062992124485, 0.4176697321401328655 ) ) ;
#13709 = CARTESIAN_POINT ( 'NONE',  ( 0.7217847769028878924, -0.004921259842519576551, 0.3153832671262227771 ) ) ;
#13710 = CARTESIAN_POINT ( 'NONE',  ( -0.1049868766404193215, 0.1283753931104746893, -0.1820866141732285504 ) ) ;
#13711 = CARTESIAN_POINT ( 'NONE',  ( -0.8464566929133852113, -0.5400638737290845981, -0.3530559997133363437 ) ) ;
#13712 = CARTESIAN_POINT ( 'NONE',  ( -1.305774278215222184, -0.6692913385826773087, -0.1292274648535924053 ) ) ;
#13713 = CARTESIAN_POINT ( 'NONE',  ( -1.410761154855641575, -0.3162353388693409650, -0.4822834645669289433 ) ) ;
#13714 = CARTESIAN_POINT ( 'NONE',  ( 0.000000000000000000, 0.000000000000000000, -2.755905511811024056 ) ) ;
#13715 = CARTESIAN_POINT ( 'NONE',  ( 1.200787401574803681, 0.07958543189024085140, 0.2665933059059887866 ) ) ;
#13716 = CARTESIAN_POINT ( 'NONE',  ( 0.3346456692913393205, -0.5400638737290845981, -0.3530559997133363437 ) ) ;
#13717 = ADVANCED_FACE ( 'NONE', ( #19983 ), #45633, .F. ) ;
#13718 = CARTESIAN_POINT ( 'NONE',  ( -1.351706036745406347, -0.4281496062992124485, 0.4176697321401328655 ) ) ;
#13719 = CARTESIAN_POINT ( 'NONE',  ( -1.646981627296586703, -0.3162353388693409650, -0.4822834645669289433 ) ) ;
#13720 = ORIENTED_EDGE ( 'NONE', *, *, #8454, .T. ) ;
#13721 = CARTESIAN_POINT ( 'NONE',  ( 0.3460692066303959202, -0.1998031496062991630, -2.229002624671915900 ) ) ;
#13722 = CARTESIAN_POINT ( 'NONE',  ( -0.6758530183727028406, 0.1771653543307087630, 0.09757992244046791164 ) ) ;
#13723 = CARTESIAN_POINT ( 'NONE',  ( 0.7677165354330716118, -0.5400638737290844871, 0.3530559997133364547 ) ) ;
#13724 = CARTESIAN_POINT ( 'NONE',  ( -1.174540682414697335, -0.2845877964562161244, -0.3641732283464567121 ) ) ;
#13725 = CARTESIAN_POINT ( 'NONE',  ( 0.3460692066303959202, -0.1998031496062991630, -1.599081364829396446 ) ) ;
#13726 = CARTESIAN_POINT ( 'NONE',  ( -0.9120734908136475250, 0.2952755905511811885, 0.1292274648535926551 ) ) ;
#13727 = CARTESIAN_POINT ( 'NONE',  ( 0.8792650918635177559, 0.05413385826771666132, 0.4176697321401328100 ) ) ;
#13728 = CARTESIAN_POINT ( 'NONE',  ( 0.6233595800524942554, -0.05778040916215560624, -0.4822834645669293319 ) ) ;
#13729 = DIRECTION ( 'NONE',  ( 0.000000000000000000, 0.000000000000000000, -1.000000000000000000 ) ) ;
#13730 = CARTESIAN_POINT ( 'NONE',  ( -1.541994750656167090, 0.1771653543307087630, 0.09757992244046791164 ) ) ;
#13731 = CARTESIAN_POINT ( 'NONE',  ( -0.1998031496062991630, -0.3460692066303959202, -1.087270341207349000 ) ) ;
#13732 = CARTESIAN_POINT ( 'NONE',  ( -0.1070741851644056997, 0.3996062992125986035, -1.266404199475065440 ) ) ;
#13733 = CARTESIAN_POINT ( 'NONE',  ( -0.1058382717557503211, 0.3949938075777409408, -0.6364829396325458744 ) ) ;
#13734 = CARTESIAN_POINT ( 'NONE',  ( 1.017216587056826160, 1.569965579892641738, 0.4735649329124862472 ) ) ;
#13735 = CARTESIAN_POINT ( 'NONE',  ( 0.6430446194225729606, -0.3690944881889765550, -0.3153832671262227771 ) ) ;
#13736 = CARTESIAN_POINT ( 'NONE',  ( 0.4593175853018379162, -0.3690944881889763329, 0.3153832671262228327 ) ) ;
#13737 = CARTESIAN_POINT ( 'NONE',  ( -0.05249343832020938322, -0.6046776061558809534, -0.2411417322834644161 ) ) ;
#13738 = CARTESIAN_POINT ( 'NONE',  ( 1.240157480314961314, -0.5400638737290844871, 0.3530559997133364547 ) ) ;
#13739 = CARTESIAN_POINT ( 'NONE',  ( -0.3949938075777408852, -0.1058382717557502933, -1.854986876640420501 ) ) ;
#13740 = CARTESIAN_POINT ( 'NONE',  ( 0.5774278215223104249, 0.1283753931104748280, 0.1820866141732283561 ) ) ;
#13741 = CARTESIAN_POINT ( 'NONE',  ( -0.9251968503937002541, -0.5400638737290845981, -0.3530559997133363437 ) ) ;
#13742 = CARTESIAN_POINT ( 'NONE',  ( 1.450131233595801428, 0.2952755905511811885, 0.1292274648535926551 ) ) ;
#13743 = CARTESIAN_POINT ( 'NONE',  ( 0.8136482939632553313, -0.6046776061558809534, -0.2411417322834644161 ) ) ;
#13744 = CARTESIAN_POINT ( 'NONE',  ( -0.4724409448818898682, -8.678599364036362592E-17, -1.771653543307086576 ) ) ;
#13745 = DIRECTION ( 'NONE',  ( 3.114085624724525612E-16, -1.000000000000000000, -5.270319453084425600E-32 ) ) ;
#13746 = ORIENTED_EDGE ( 'NONE', *, *, #14676, .F. ) ;
#13747 = ORIENTED_EDGE ( 'NONE', *, *, #79456, .T. ) ;
#13748 = CARTESIAN_POINT ( 'NONE',  ( -1.069553805774277722, 0.2952755905511811885, 0.1292274648535926551 ) ) ;
#13749 = CARTESIAN_POINT ( 'NONE',  ( -1.213910761154854745, -0.6692913385826771977, 0.1292274648535927661 ) ) ;
#13751 = CARTESIAN_POINT ( 'NONE',  ( -0.8333333333333323711, 0.2952755905511811885, 0.1292274648535926551 ) ) ;
#13750 = CARTESIAN_POINT ( 'NONE',  ( -0.6496062992125976043, 0.07958543189024071263, -0.2665933059059888421 ) ) ;
#13752 = CARTESIAN_POINT ( 'NONE',  ( 0.1049643490035304522, -0.3917322834645668994, -2.212579109415011569 ) ) ;
#13753 = CARTESIAN_POINT ( 'NONE',  ( -0.4609447788686161229, -1.429000049448402363E-15, 0.3791475997938249520 ) ) ;
#13754 = CARTESIAN_POINT ( 'NONE',  ( 1.581364829396326277, -0.3162353388693409650, -0.4822834645669289433 ) ) ;
#13755 = CARTESIAN_POINT ( 'NONE',  ( -1.108923884514435132, -0.3162353388693405765, 0.4822834645669290543 ) ) ;
#13756 = CARTESIAN_POINT ( 'NONE',  ( 0.5446194225721792126, -0.05778040916215560624, -0.4822834645669293319 ) ) ;
#13757 = CARTESIAN_POINT ( 'NONE',  ( -0.7677165354330699465, -0.5400638737290845981, -0.3530559997133363437 ) ) ;
#13758 = CARTESIAN_POINT ( 'NONE',  ( 0.1958661417322836162, -0.3392501089628018329, -2.849062049047557998 ) ) ;
#13759 = CARTESIAN_POINT ( 'NONE',  ( 0.5446194225721792126, -0.05778040916215560624, -0.4822834645669293319 ) ) ;
#13760 = CARTESIAN_POINT ( 'NONE',  ( -0.3392501089628017219, -0.1958661417322836718, -1.619422572178477848 ) ) ;
#13761 = CARTESIAN_POINT ( 'NONE',  ( -0.7874015748031489847, -0.1870078740157480601, -0.3641732283464567677 ) ) ;
#13762 = ORIENTED_EDGE ( 'NONE', *, *, #20862, .F. ) ;
#13763 = CARTESIAN_POINT ( 'NONE',  ( 0.3949938075777411073, -0.1058382717557499464, -1.843832020997375309 ) ) ;
#13764 = VERTEX_POINT ( 'NONE', #7778 ) ;
#13765 = CARTESIAN_POINT ( 'NONE',  ( -1.601049868766403650, -0.5023911411419708095, 0.1820866141732285504 ) ) ;
#13766 = CARTESIAN_POINT ( 'NONE',  ( -1.141732283464566011, -0.6692913385826771977, 8.415575281601705876E-17 ) ) ;
#13767 = CARTESIAN_POINT ( 'NONE',  ( -1.410761154855641575, -0.3162353388693409650, -0.4822834645669289433 ) ) ;
#13768 = CARTESIAN_POINT ( 'NONE',  ( -0.1070741851644051862, -0.3996062992125987146, -0.5446194225721783244 ) ) ;
#13769 = CARTESIAN_POINT ( 'NONE',  ( -1.049868766404198794, 0.2306618581243847221, -0.2411417322834647770 ) ) ;
#13770 = CARTESIAN_POINT ( 'NONE',  ( -1.351706036745406347, 0.05413385826771626580, -0.4176697321401330321 ) ) ;
#13771 = CARTESIAN_POINT ( 'NONE',  ( -1.528871391076114250, -0.6692913385826771977, 0.1292274648535927661 ) ) ;
#13772 = CARTESIAN_POINT ( 'NONE',  ( 1.586052503253845281, 1.299212598425198095, -0.1653254495020587411 ) ) ;
#13773 = CARTESIAN_POINT ( 'NONE',  ( 0.2230971128608932319, -0.3690944881889763329, 0.3153832671262228327 ) ) ;
#13774 = DIRECTION ( 'NONE',  ( -1.000000000000000000, -0.000000000000000000, -0.000000000000000000 ) ) ;
#13775 = CARTESIAN_POINT ( 'NONE',  ( 0.1958661417322836440, -0.3392501089628017219, -0.1765091863517061210 ) ) ;
#13776 = CARTESIAN_POINT ( 'NONE',  ( -0.2755905511811018171, 0.1771653543307087630, 0.000000000000000000 ) ) ;
#13777 = CARTESIAN_POINT ( 'NONE',  ( -0.9973753280839886548, 0.2306618581243848609, 0.2411417322834645549 ) ) ;
#13778 = CARTESIAN_POINT ( 'NONE',  ( 1.003937007874016185, 0.1660481256975883668, -0.3530559997133364547 ) ) ;
#13779 = CARTESIAN_POINT ( 'NONE',  ( -0.4593175853018364174, -0.4281496062992127816, -0.4176697321401328100 ) ) ;
#13780 = ORIENTED_EDGE ( 'NONE', *, *, #24858, .F. ) ;
#13781 = EDGE_LOOP ( 'NONE', ( #58003, #26326, #69661, #11364 ) ) ;
#13782 = CARTESIAN_POINT ( 'NONE',  ( 0.3996062992125986035, -0.1070741851644052972, -2.078083989501312345 ) ) ;
#13784 = CIRCLE ( 'NONE', #52746, 0.1771653543307085410 ) ;
#13783 = CARTESIAN_POINT ( 'NONE',  ( -0.9645669291338575535, 0.1660481256975883668, -0.3530559997133364547 ) ) ;
#13785 = CARTESIAN_POINT ( 'NONE',  ( 1.312335958005249825, 0.2306618581243847221, -0.2411417322834647770 ) ) ;
#13786 = CARTESIAN_POINT ( 'NONE',  ( -1.673228346456691717, 0.07958543189024071263, -0.2665933059059888421 ) ) ;
#13787 = CARTESIAN_POINT ( 'NONE',  ( 0.1265901696524990294, -0.4724409448818896462, -0.7152230971128609172 ) ) ;
#13788 = CARTESIAN_POINT ( 'NONE',  ( 0.000000000000000000, 1.724409448818897461, 0.000000000000000000 ) ) ;
#13789 = CARTESIAN_POINT ( 'NONE',  ( -0.3392501089628017219, -0.1958661417322836718, -0.2020997375328083545 ) ) ;
#13790 = CARTESIAN_POINT ( 'NONE',  ( -9.594673741351313045E-17, 0.3917322834645670104, -1.974409448818897683 ) ) ;
#13791 = CARTESIAN_POINT ( 'NONE',  ( -0.3805774278215216522, 0.05413385826771666132, 0.4176697321401328100 ) ) ;
#13792 = CARTESIAN_POINT ( 'NONE',  ( -1.640419947506561060, -0.004921259842519576551, 0.3153832671262227771 ) ) ;
#13793 = CARTESIAN_POINT ( 'NONE',  ( -0.8333333333333323711, -0.6692913385826773087, -0.1292274648535924053 ) ) ;
#13794 = CARTESIAN_POINT ( 'NONE',  ( -0.3460692066303957537, -0.1998031496062994405, 0.1856955380577427484 ) ) ;
#13796 = DIRECTION ( 'NONE',  ( 9.381338752702759131E-17, -0.6427876096865364763, 0.7660444431189804559 ) ) ;
#13795 = CARTESIAN_POINT ( 'NONE',  ( -1.299212598425196097, -0.6692913385826771977, 8.415575281601705876E-17 ) ) ;
#13797 = CARTESIAN_POINT ( 'NONE',  ( -1.003937007874015297, -0.5400638737290845981, -0.3530559997133363437 ) ) ;
#13798 = CARTESIAN_POINT ( 'NONE',  ( -0.3083989501312330295, -0.05778040916215522460, 0.4822834645669289988 ) ) ;
#13799 = CARTESIAN_POINT ( 'NONE',  ( -0.2891555358219911054, 0.2891555358219909388, -2.616141732283464805 ) ) ;
#13800 = CARTESIAN_POINT ( 'NONE',  ( 0.8398950131233602345, 0.1283753931104746893, -0.1820866141732285504 ) ) ;
#13801 = APPLICATION_CONTEXT ( 'automotive_design' ) ;
#13802 = CARTESIAN_POINT ( 'NONE',  ( 0.2867679344610366554, -0.2867679344610365444, -0.1830708661417323746 ) ) ;
#13803 = CARTESIAN_POINT ( 'NONE',  ( 0.7480314960629927956, 0.1771653543307087630, 0.000000000000000000 ) ) ;
#13804 = CARTESIAN_POINT ( 'NONE',  ( 1.181102362204724976, -0.1870078740157480601, -0.3641732283464567677 ) ) ;
#13805 = CARTESIAN_POINT ( 'NONE',  ( 1.463254593175853824, 0.2952755905511810774, -0.1292274648535930714 ) ) ;
#13806 = CARTESIAN_POINT ( 'NONE',  ( 0.03937007874015833325, -0.5511811023622047445, 6.969142054262312111E-17 ) ) ;
#13807 = CARTESIAN_POINT ( 'NONE',  ( 0.1958661417322834775, 0.3392501089628018884, -1.868766404199474929 ) ) ;
#13808 = CARTESIAN_POINT ( 'NONE',  ( -1.259842519685038686, -0.1870078740157480879, -0.4822834645669291653 ) ) ;
#13809 = CARTESIAN_POINT ( 'NONE',  ( 1.056430446194226436, -0.6692913385826773087, -0.1292274648535924053 ) ) ;
#13810 = CARTESIAN_POINT ( 'NONE',  ( -0.2362204724409447953, -0.4091458600556404646, 0.01509186351706036204 ) ) ;
#13811 = CARTESIAN_POINT ( 'NONE',  ( -0.3937007874015740483, -0.1870078740157479769, 0.3641732283464567677 ) ) ;
#13812 = CARTESIAN_POINT ( 'NONE',  ( 0.05249343832021075018, 0.2306618581243847221, -0.2411417322834647770 ) ) ;
#13813 = ADVANCED_FACE ( 'NONE', ( #52782 ), #78491, .F. ) ;
#13814 = CARTESIAN_POINT ( 'NONE',  ( 0.3149606299212606708, -0.1870078740157480879, -0.4822834645669291653 ) ) ;
#13815 = CARTESIAN_POINT ( 'NONE',  ( 0.3458507752293908943, 0.3458507752293908943, -0.6870078740157479213 ) ) ;
#13816 = CARTESIAN_POINT ( 'NONE',  ( 1.036745406824147508, -0.3690944881889765550, -0.3153832671262227771 ) ) ;
#13817 = CARTESIAN_POINT ( 'NONE',  ( 0.2624671916010504757, -0.5023911411419708095, -0.1820866141732282451 ) ) ;
#13818 = CARTESIAN_POINT ( 'NONE',  ( -0.2690288713910754526, -0.6692913385826771977, 0.1292274648535927661 ) ) ;
#13819 = CARTESIAN_POINT ( 'NONE',  ( -1.496062992125983815, -0.1870078740157480879, -0.4822834645669291653 ) ) ;
#13820 = CARTESIAN_POINT ( 'NONE',  ( -0.8136482939632537770, 0.1283753931104746893, -0.1820866141732285504 ) ) ;
#13821 = CARTESIAN_POINT ( 'NONE',  ( -2.543486866223389153, 2.716535433070866645, -0.5314960629921260393 ) ) ;
#13822 = CARTESIAN_POINT ( 'NONE',  ( 0.6036745406824154392, 0.2306618581243847221, -0.2411417322834647770 ) ) ;
#13823 = CARTESIAN_POINT ( 'NONE',  ( -0.8595800524934373854, -0.05778040916215522460, 0.4822834645669289988 ) ) ;
#13824 = CARTESIAN_POINT ( 'NONE',  ( 0.1998031496062992463, 0.3460692066303959202, -1.008530183727034180 ) ) ;
#13825 = CARTESIAN_POINT ( 'NONE',  ( 0.3392501089628018884, -0.1958661417322834220, -2.866797900262466836 ) ) ;
#13826 = CARTESIAN_POINT ( 'NONE',  ( 0.2887139107611556010, -0.5023911411419708095, 0.1820866141732285504 ) ) ;
#13827 = CARTESIAN_POINT ( 'NONE',  ( -0.9383202099737524282, -0.3162353388693409650, -0.4822834645669289433 ) ) ;
#13828 = CARTESIAN_POINT ( 'NONE',  ( -1.135170603674539924, 0.2952755905511810774, -0.1292274648535930714 ) ) ;
#13829 = CARTESIAN_POINT ( 'NONE',  ( -1.030183727034119867, -0.2845877964562159024, 0.3641732283464567677 ) ) ;
#13830 = CYLINDRICAL_SURFACE ( 'NONE', #62758, 0.4744094488188972947 ) ;
#13831 = CARTESIAN_POINT ( 'NONE',  ( -0.6889763779527552368, 0.07958543189024085140, 0.2665933059059887866 ) ) ;
#13832 = CARTESIAN_POINT ( 'NONE',  ( -0.7480314960629914633, 0.2066929133858268208, 0.000000000000000000 ) ) ;
#13833 = CARTESIAN_POINT ( 'NONE',  ( 1.437007874015748810, 0.1660481256975885056, 0.3530559997133364547 ) ) ;
#13834 = CARTESIAN_POINT ( 'NONE',  ( 0.2925321140481932369, 0.2925321140481932369, -0.2952755905511811330 ) ) ;
#13835 = TOROIDAL_SURFACE ( 'NONE', #39346, 0.1574803149606295860, 0.01968503937007873988 ) ;
#13836 = CARTESIAN_POINT ( 'NONE',  ( 0.1958661417322836718, -0.3392501089628017219, -2.608287032317271770 ) ) ;
#13837 = VERTEX_POINT ( 'NONE', #83235 ) ;
#13838 = CARTESIAN_POINT ( 'NONE',  ( 0.02578378529929631693, -0.3963884504522709462, -2.713666019656065720E-16 ) ) ;
#13839 = CARTESIAN_POINT ( 'NONE',  ( 1.364829396325459854, -0.5023911411419708095, -0.1820866141732282451 ) ) ;
#13840 = CARTESIAN_POINT ( 'NONE',  ( -1.456692913385826182, -0.6692913385826771977, 8.415575281601705876E-17 ) ) ;
#13841 = CARTESIAN_POINT ( 'NONE',  ( 1.089238845144357537, -0.4281496062992124485, 0.4176697321401328655 ) ) ;
#13842 = CARTESIAN_POINT ( 'NONE',  ( 0.1958661417322836440, -0.3392501089628017219, -2.223753280839895208 ) ) ;
#13843 = CARTESIAN_POINT ( 'NONE',  ( 1.541994750656168645, 0.1771653543307087075, -0.09757992244046823083 ) ) ;
#13844 = CARTESIAN_POINT ( 'NONE',  ( 0.3740157480314966754, -0.5400638737290844871, 0.3530559997133364547 ) ) ;
#13845 = CARTESIAN_POINT ( 'NONE',  ( 0.09842519685039434474, 0.1660481256975885056, 0.3530559997133364547 ) ) ;
#13846 = CARTESIAN_POINT ( 'NONE',  ( -0.3503937007874015630, -0.3044824468161027586, -0.01968503937007903132 ) ) ;
#13847 = CARTESIAN_POINT ( 'NONE',  ( -0.3460692066303957537, -0.1998031496062994405, -2.648950131233595684 ) ) ;
#13848 = CARTESIAN_POINT ( 'NONE',  ( 0.8858267716535438430, -0.4536011799217368745, -0.2665933059059886201 ) ) ;
#13849 = CARTESIAN_POINT ( 'NONE',  ( 0.2925321140481932369, -0.2925321140481932369, -1.358267716535433101 ) ) ;
#13850 = ORIENTED_EDGE ( 'NONE', *, *, #34274, .T. ) ;
#13851 = CARTESIAN_POINT ( 'NONE',  ( -0.3917322834645670104, -0.1049643490035307020, 0.1148100805436201299 ) ) ;
#13852 = EDGE_LOOP ( 'NONE', ( #39012, #43245 ) ) ;
#13853 = CARTESIAN_POINT ( 'NONE',  ( 0.03937007874015806264, 0.2952755905511811885, 0.000000000000000000 ) ) ;
#13854 = CARTESIAN_POINT ( 'NONE',  ( 1.122047244094488860, 0.1660481256975885056, 0.3530559997133364547 ) ) ;
#13855 = CARTESIAN_POINT ( 'NONE',  ( 0.7414698162729663755, 0.2952755905511811885, 0.1292274648535926551 ) ) ;
#13856 = CARTESIAN_POINT ( 'NONE',  ( 1.417322834645670104, -0.1870078740157480879, -0.4822834645669291653 ) ) ;
#13857 = CARTESIAN_POINT ( 'NONE',  ( -0.4199475065616791736, -0.6046776061558807314, 0.2411417322834647770 ) ) ;
#13858 = CARTESIAN_POINT ( 'NONE',  ( 0.01312335958005323398, 0.05413385826771666132, 0.4176697321401328100 ) ) ;
#13859 = CARTESIAN_POINT ( 'NONE',  ( 1.430446194225722500, 0.05413385826771666132, 0.4176697321401328100 ) ) ;
#13860 = CARTESIAN_POINT ( 'NONE',  ( 1.161417322834646271, 0.1660481256975883668, -0.3530559997133364547 ) ) ;
#13861 = CARTESIAN_POINT ( 'NONE',  ( 0.9908136482939640111, -0.6692913385826771977, 0.1292274648535927661 ) ) ;
#13862 = CARTESIAN_POINT ( 'NONE',  ( 0.3917322834645669549, 0.1049643490035304660, -0.1167979002624671414 ) ) ;
#13863 = CARTESIAN_POINT ( 'NONE',  ( 0.5380577427821529035, -0.3690944881889763329, 0.3153832671262228327 ) ) ;
#13864 = ORIENTED_EDGE ( 'NONE', *, *, #9579, .F. ) ;
#13865 = CARTESIAN_POINT ( 'NONE',  ( -0.3420746716998659953, -0.1974969037888706647, -0.5249343832020998413 ) ) ;
#13866 = ORIENTED_EDGE ( 'NONE', *, *, #4866, .F. ) ;
#13867 = CARTESIAN_POINT ( 'NONE',  ( -0.4855643044619415427, -0.3690944881889763329, 0.3153832671262228327 ) ) ;
#13868 = CARTESIAN_POINT ( 'NONE',  ( -0.07217847769028787330, -0.05778040916215522460, 0.4822834645669289988 ) ) ;
#13869 = CARTESIAN_POINT ( 'NONE',  ( 2.759487654322811956, 1.189595890467133987, -0.3229789317950513272 ) ) ;
#13870 = CARTESIAN_POINT ( 'NONE',  ( 0.07217847769028949700, -0.05778040916215560624, -0.4822834645669293319 ) ) ;
#13871 = CARTESIAN_POINT ( 'NONE',  ( 0.09186351706036799403, -0.4281496062992127816, -0.4176697321401328100 ) ) ;
#13872 = CARTESIAN_POINT ( 'NONE',  ( -0.8923884514435688198, -0.6046776061558807314, 0.2411417322834647770 ) ) ;
#13873 = CARTESIAN_POINT ( 'NONE',  ( -0.8595800524934373854, -0.3162353388693409650, -0.4822834645669289433 ) ) ;
#13874 = CARTESIAN_POINT ( 'NONE',  ( 1.423884514435696413, -0.2845877964562161244, -0.3641732283464567121 ) ) ;
#13875 = DIRECTION ( 'NONE',  ( 1.000000000000000000, 0.000000000000000000, 0.000000000000000000 ) ) ;
#13876 = DIRECTION ( 'NONE',  ( 0.000000000000000000, -0.7071067811865437980, -0.7071067811865511255 ) ) ;
#13877 = CARTESIAN_POINT ( 'NONE',  ( 0.7611548556430451917, -0.5023911411419708095, 0.1820866141732285504 ) ) ;
#13878 = VECTOR ( 'NONE', #14560, 39.37007874015748854 ) ;
#13879 = CARTESIAN_POINT ( 'NONE',  ( 0.3083989501312343062, -0.05778040916215560624, -0.4822834645669293319 ) ) ;
#13880 = CARTESIAN_POINT ( 'NONE',  ( 0.8202099737532814183, -0.6692913385826773087, -0.1292274648535924053 ) ) ;
#13881 = CARTESIAN_POINT ( 'NONE',  ( -0.3996062992125986035, -7.340648628747425578E-17, -1.456692913385826849 ) ) ;
#13882 = CARTESIAN_POINT ( 'NONE',  ( 0.000000000000000000, 0.000000000000000000, -1.289370078740159409 ) ) ;
#13883 = CARTESIAN_POINT ( 'NONE',  ( -0.2925321140481930149, -0.2925321140481933480, -0.6082677165354329896 ) ) ;
#13884 = CARTESIAN_POINT ( 'NONE',  ( -0.3460692066303960313, 0.1998031496062989965, 0.05446194225721782967 ) ) ;
#13885 = CARTESIAN_POINT ( 'NONE',  ( -0.6627296587926503335, -0.6692913385826771977, 0.1292274648535927661 ) ) ;
#13886 = CARTESIAN_POINT ( 'NONE',  ( -9.787531504996567848E-17, 0.3996062992125986035, -2.677165354330708347 ) ) ;
#13887 = CARTESIAN_POINT ( 'NONE',  ( 0.1049643490035304938, -0.3917322834645669549, -2.059711286089238591 ) ) ;
#13888 = CARTESIAN_POINT ( 'NONE',  ( -1.240157480314959759, -0.4536011799217368745, -0.2665933059059886201 ) ) ;
#13889 = CARTESIAN_POINT ( 'NONE',  ( 1.384514435695538337, -0.6692913385826771977, 0.1292274648535927661 ) ) ;
#13890 = CARTESIAN_POINT ( 'NONE',  ( 0.9645669291338591078, -0.5400638737290845981, -0.3530559997133363437 ) ) ;
#13891 = CARTESIAN_POINT ( 'NONE',  ( -0.1509186351706028884, -0.2845877964562161244, -0.3641732283464567121 ) ) ;
#13892 = CARTESIAN_POINT ( 'NONE',  ( 0.6627296587926515548, 0.2952755905511811885, 0.1292274648535926551 ) ) ;
#13893 = CARTESIAN_POINT ( 'NONE',  ( -0.4724409448818895907, -0.1265901696524993070, -1.382545931758530022 ) ) ;
#13894 = CARTESIAN_POINT ( 'NONE',  ( 0.2165354330708668673, -0.4536011799217367080, 0.2665933059059888421 ) ) ;
#13895 =( BOUNDED_CURVE ( )  B_SPLINE_CURVE ( 3, ( #13846, #6679, #71081, #38665 ),
 .UNSPECIFIED., .F., .F. ) 
 B_SPLINE_CURVE_WITH_KNOTS ( ( 4, 4 ),
 ( 4.647828011067211662, 4.651745756353172112 ),
 .UNSPECIFIED. ) 
 CURVE ( )  GEOMETRIC_REPRESENTATION_ITEM ( )  RATIONAL_B_SPLINE_CURVE ( ( 1.000000000000000000, 0.9999987209397318555, 0.9999987209397318555, 1.000000000000000000 ) ) 
 REPRESENTATION_ITEM ( '' )  );
#13896 = CARTESIAN_POINT ( 'NONE',  ( -0.03937007874015669567, -0.6692913385826771977, 8.415575281601705876E-17 ) ) ;
#13897 = CIRCLE ( 'NONE', #67668, 0.09842519685039351207 ) ;
#13898 = CARTESIAN_POINT ( 'NONE',  ( -0.1974969037888706924, 0.3420746716998658843, -1.507217847769029007 ) ) ;
#13899 = CARTESIAN_POINT ( 'NONE',  ( -1.292650918635170010, -0.6692913385826771977, 0.1292274648535927661 ) ) ;
#13900 = CARTESIAN_POINT ( 'NONE',  ( 0.3412073490813655186, 0.1283753931104748280, 0.1820866141732283561 ) ) ;
#13901 = CARTESIAN_POINT ( 'NONE',  ( 0.1181102362204724532, 0.04921259842519689481, 0.08523872084492503665 ) ) ;
#13902 = CARTESIAN_POINT ( 'NONE',  ( -0.7414698162729651543, 0.2952755905511810774, -0.1292274648535930714 ) ) ;
#13903 = CARTESIAN_POINT ( 'NONE',  ( -0.2296587926509179312, -0.08942795157527998196, 0.3641732283464567121 ) ) ;
#13904 = CARTESIAN_POINT ( 'NONE',  ( -2.554262525012342966, 1.537401574803149984, -0.4744094488188975722 ) ) ;
#13905 = CARTESIAN_POINT ( 'NONE',  ( -0.6430446194225716283, -0.4281496062992124485, 0.4176697321401328655 ) ) ;
#13906 = CARTESIAN_POINT ( 'NONE',  ( -0.5774278215223089816, -0.6046776061558807314, 0.2411417322834647770 ) ) ;
#13907 = CARTESIAN_POINT ( 'NONE',  ( 0.3740157480314966754, 0.07958543189024071263, -0.2665933059059888421 ) ) ;
#13908 = CARTESIAN_POINT ( 'NONE',  ( -0.3996062992125984925, -0.1070741851644056858, -2.327427821522309870 ) ) ;
#13909 = CARTESIAN_POINT ( 'NONE',  ( 0.1115485564304470323, 0.2952755905511811885, 0.1292274648535926551 ) ) ;
#13910 = EDGE_CURVE ( 'NONE', #15221, #32199, #20096, .T. ) ;
#13911 = CARTESIAN_POINT ( 'NONE',  ( -0.1958661417322836440, 0.3392501089628016664, -1.982920316764092306 ) ) ;
#13912 = DIRECTION ( 'NONE',  ( 0.000000000000000000, -0.5150380749100564870, -0.8571673007021107793 ) ) ;
#13913 = CARTESIAN_POINT ( 'NONE',  ( 0.9514435695538062676, -0.2845877964562161244, -0.3641732283464567121 ) ) ;
#13914 = CARTESIAN_POINT ( 'NONE',  ( 1.410761154855643795, -0.3162353388693405765, 0.4822834645669290543 ) ) ;
#13915 = CARTESIAN_POINT ( 'NONE',  ( -0.8398950131233589023, -0.5023911411419708095, -0.1820866141732282451 ) ) ;
#13916 = CARTESIAN_POINT ( 'NONE',  ( -1.266404199475064773, -0.2845877964562159024, 0.3641732283464567677 ) ) ;
#13917 = EDGE_CURVE ( 'NONE', #48718, #35380, #44901, .T. ) ;
#13918 = CARTESIAN_POINT ( 'NONE',  ( -0.5314960629921250401, 0.1660481256975885056, 0.3530559997133364547 ) ) ;
#13919 = CARTESIAN_POINT ( 'NONE',  ( -0.1246719160104980823, 0.2952755905511811885, 0.1292274648535926551 ) ) ;
#13920 = CARTESIAN_POINT ( 'NONE',  ( 0.3543307086614181922, -0.5511811023622047445, 6.969142054262312111E-17 ) ) ;
#13921 = CARTESIAN_POINT ( 'NONE',  ( -0.2490243534527243618, 0.1587552710309117210, 5.781441956045568986 ) ) ;
#13922 = CARTESIAN_POINT ( 'NONE',  ( 1.227034120734908917, -0.5511811023622046335, 0.09757992244046803654 ) ) ;
#13923 = CARTESIAN_POINT ( 'NONE',  ( 0.5380577427821529035, -0.4281496062992124485, 0.4176697321401328655 ) ) ;
#13924 = CARTESIAN_POINT ( 'NONE',  ( -0.3996062992125985480, -7.340648628747423112E-17, 0.1988188976377952832 ) ) ;
#13925 = CARTESIAN_POINT ( 'NONE',  ( -0.7020997375328076329, -0.3162353388693409650, -0.4822834645669289433 ) ) ;
#13926 = CARTESIAN_POINT ( 'NONE',  ( 0.2867679344610365999, 0.2867679344610365999, -1.324803149606299302 ) ) ;
#13927 = CARTESIAN_POINT ( 'NONE',  ( 1.594488188976378673, 0.07958543189024085140, 0.2665933059059887866 ) ) ;
#13928 = CARTESIAN_POINT ( 'NONE',  ( 0.3805774278215230400, -0.4281496062992124485, 0.4176697321401328655 ) ) ;
#13929 = CARTESIAN_POINT ( 'NONE',  ( 0.1902887139107617975, -0.6692913385826773087, -0.1292274648535924053 ) ) ;
#13930 = DIRECTION ( 'NONE',  ( 0.000000000000000000, 0.000000000000000000, 1.000000000000000000 ) ) ;
#13931 = CARTESIAN_POINT ( 'NONE',  ( 0.06561679790026316017, -0.3690944881889763329, 0.3153832671262228327 ) ) ;
#13932 = CARTESIAN_POINT ( 'NONE',  ( 0.9055118110236227702, 0.2952755905511811885, 0.000000000000000000 ) ) ;
#13933 = CARTESIAN_POINT ( 'NONE',  ( -0.2755905511811018171, 0.1771653543307087630, 0.000000000000000000 ) ) ;
#13934 = CARTESIAN_POINT ( 'NONE',  ( -0.8595800524934373854, -0.05778040916215522460, 0.4822834645669289988 ) ) ;
#13935 = CARTESIAN_POINT ( 'NONE',  ( 1.895394334970792016, 2.755905511811024056, 0.5314960629921260393 ) ) ;
#13936 = CARTESIAN_POINT ( 'NONE',  ( 0.03937007874015806264, 0.2952755905511811885, 0.000000000000000000 ) ) ;
#13937 = EDGE_LOOP ( 'NONE', ( #70644, #22928, #59626, #57301 ) ) ;
#13938 = CARTESIAN_POINT ( 'NONE',  ( -1.069553805774277722, -0.6692913385826773087, -0.1292274648535924053 ) ) ;
#13939 = CIRCLE ( 'NONE', #81117, 3.582677165354331450 ) ;
#13940 = CARTESIAN_POINT ( 'NONE',  ( -0.6496062992125976043, -0.4536011799217367080, 0.2665933059059888421 ) ) ;
#13941 = CARTESIAN_POINT ( 'NONE',  ( -0.08530183727034056085, -0.05778040916215560624, -0.4822834645669293319 ) ) ;
#13942 = CARTESIAN_POINT ( 'NONE',  ( -1.371391076115484831, 0.2952755905511810774, -0.1292274648535930714 ) ) ;
#13943 = CARTESIAN_POINT ( 'NONE',  ( -0.5905511811023613777, -0.6692913385826771977, 8.415575281601705876E-17 ) ) ;
#13944 = CARTESIAN_POINT ( 'NONE',  ( 3.886287458032462006, 1.724409448818898127, 0.6299212598425202314 ) ) ;
#13946 = CARTESIAN_POINT ( 'NONE',  ( 0.7480314960629927956, -0.6692913385826771977, 8.415575281601705876E-17 ) ) ;
#13945 = CARTESIAN_POINT ( 'NONE',  ( -0.8858267716535425107, 0.1660481256975883391, -0.3530559997133364547 ) ) ;
#13947 = CARTESIAN_POINT ( 'NONE',  ( 1.076115485564305141, 0.2306618581243847221, -0.2411417322834647770 ) ) ;
#13948 = CARTESIAN_POINT ( 'NONE',  ( 4.797336870675656522E-17, -0.3917322834645670104, -2.433070866141732402 ) ) ;
#13949 = CARTESIAN_POINT ( 'NONE',  ( 1.476377952755906220, 0.1660481256975883668, -0.3530559997133364547 ) ) ;
#13950 = CARTESIAN_POINT ( 'NONE',  ( -1.272965879265091305, -0.4281496062992124485, 0.4176697321401328655 ) ) ;
#13951 = CARTESIAN_POINT ( 'NONE',  ( 0.4724409448818897572, -0.1265901696524988906, -0.5839895013123358458 ) ) ;
#13952 = CARTESIAN_POINT ( 'NONE',  ( -0.1998031496062994683, 0.3460692066303958092, -0.01312335958005251234 ) ) ;
#13953 = VERTEX_POINT ( 'NONE', #77340 ) ;
#13954 = CARTESIAN_POINT ( 'NONE',  ( 0.02624671916010564918, -0.5023911411419708095, -0.1820866141732282451 ) ) ;
#13956 = CARTESIAN_POINT ( 'NONE',  ( -9.594673741351313045E-17, 0.3917322834645670104, -1.724409448818897683 ) ) ;
#13955 = VECTOR ( 'NONE', #55974, 39.37007874015748854 ) ;
#13957 = ORIENTED_EDGE ( 'NONE', *, *, #57885, .T. ) ;
#13958 = CARTESIAN_POINT ( 'NONE',  ( 0.2755905511811031494, -0.6692913385826771977, 8.415575281601705876E-17 ) ) ;
#13959 = CARTESIAN_POINT ( 'NONE',  ( -0.1312335958005241554, 0.2306618581243848609, 0.2411417322834645549 ) ) ;
#13960 = CARTESIAN_POINT ( 'NONE',  ( -0.7677165354330699465, -0.5400638737290845981, -0.3530559997133363437 ) ) ;
#13961 = DIRECTION ( 'NONE',  ( 0.000000000000000000, 0.000000000000000000, 1.000000000000000000 ) ) ;
#13962 = CARTESIAN_POINT ( 'NONE',  ( -0.9186351706036736120, -0.5023911411419708095, -0.1820866141732282451 ) ) ;
#13963 = CARTESIAN_POINT ( 'NONE',  ( 0.3412073490813655186, 0.2306618581243848609, 0.2411417322834645549 ) ) ;
#13964 = CARTESIAN_POINT ( 'NONE',  ( 0.6430446194225729606, -0.4281496062992127816, -0.4176697321401328100 ) ) ;
#13965 = CARTESIAN_POINT ( 'NONE',  ( 1.108923884514436242, -0.08942795157527998196, 0.3641732283464567121 ) ) ;
#13966 = CARTESIAN_POINT ( 'NONE',  ( -0.3674540682414689785, 0.2306618581243848609, 0.2411417322834645549 ) ) ;
#13967 = CARTESIAN_POINT ( 'NONE',  ( -0.1958661417322836440, 0.3392501089628016664, -1.038038427000312902 ) ) ;
#13968 = CARTESIAN_POINT ( 'NONE',  ( -0.7217847769028863381, -0.4281496062992124485, 0.4176697321401328655 ) ) ;
#13969 = CARTESIAN_POINT ( 'NONE',  ( 1.586052503253845503, 0.7480314960629931287, 0.1653254495020587966 ) ) ;
#13970 = CARTESIAN_POINT ( 'NONE',  ( 1.482939632545932307, -0.4281496062992124485, 0.4176697321401328655 ) ) ;
#13971 = CARTESIAN_POINT ( 'NONE',  ( 1.496062992125985147, -0.1870078740157479769, 0.3641732283464567677 ) ) ;
#13972 = ORIENTED_EDGE ( 'NONE', *, *, #66038, .T. ) ;
#13973 = CARTESIAN_POINT ( 'NONE',  ( 0.3917322834645670104, 0.1049643490035304660, -2.641095431267403537 ) ) ;
#13974 = CARTESIAN_POINT ( 'NONE',  ( -0.1312335958005241554, -0.6046776061558809534, -0.2411417322834644161 ) ) ;
#13975 = ORIENTED_EDGE ( 'NONE', *, *, #5896, .T. ) ;
#13976 = CARTESIAN_POINT ( 'NONE',  ( -0.7611548556430438595, 0.2306618581243848609, 0.2411417322834645549 ) ) ;
#13977 = CARTESIAN_POINT ( 'NONE',  ( 1.561679790026247350, -0.4281496062992124485, 0.4176697321401328655 ) ) ;
#13978 = CARTESIAN_POINT ( 'NONE',  ( 1.404199475065617264, -0.4281496062992124485, 0.4176697321401328655 ) ) ;
#13979 = CARTESIAN_POINT ( 'NONE',  ( 0.2165354330708668673, 0.1660481256975883668, -0.3530559997133364547 ) ) ;
#13980 = EDGE_CURVE ( 'NONE', #69925, #78139, #73535, .T. ) ;
#13981 = CARTESIAN_POINT ( 'NONE',  ( -0.4986876640419939388, 0.2306618581243847221, -0.2411417322834647770 ) ) ;
#13982 = CARTESIAN_POINT ( 'NONE',  ( -0.3392501089628019995, 0.1958661417322832277, -1.685695538057742970 ) ) ;
#13983 = CARTESIAN_POINT ( 'NONE',  ( -1.181102362204723644, -0.1870078740157480879, -0.4822834645669291653 ) ) ;
#13984 = CARTESIAN_POINT ( 'NONE',  ( -0.1771653543307080136, 0.1660481256975883668, -0.3530559997133364547 ) ) ;
#13985 = CARTESIAN_POINT ( 'NONE',  ( -0.1640419947506553400, -0.08942795157528024563, -0.3641732283464568787 ) ) ;
#13986 = CARTESIAN_POINT ( 'NONE',  ( 1.555118110236221041, 0.1660481256975883668, -0.3530559997133364547 ) ) ;
#13987 = CARTESIAN_POINT ( 'NONE',  ( 1.397637795275591177, 0.1660481256975883668, -0.3530559997133364547 ) ) ;
#13988 = CARTESIAN_POINT ( 'NONE',  ( -0.4330708661417315697, 0.2952755905511811885, 0.000000000000000000 ) ) ;
#13989 = CARTESIAN_POINT ( 'NONE',  ( -0.4744094488188832504, 1.537401574803149984, -3.937007874015763687 ) ) ;
#13990 = CARTESIAN_POINT ( 'NONE',  ( 0.9776902887139113929, 0.2952755905511811885, 0.1292274648535926551 ) ) ;
#13991 = CARTESIAN_POINT ( 'NONE',  ( 1.141392835773559211, 0.3937007874015748254, 1.141392835773562764 ) ) ;
#13992 = ORIENTED_EDGE ( 'NONE', *, *, #10205, .T. ) ;
#13993 = CARTESIAN_POINT ( 'NONE',  ( 0.3346456692913393205, -0.5400638737290845981, -0.3530559997133363437 ) ) ;
#13994 = CARTESIAN_POINT ( 'NONE',  ( -0.1377952755905504645, 0.07958543189024085140, 0.2665933059059887866 ) ) ;
#13996 = CARTESIAN_POINT ( 'NONE',  ( -2.583694225513480713, 2.755905511811024056, -0.5314960629921260393 ) ) ;
#13995 = CARTESIAN_POINT ( 'NONE',  ( 0.8989501312335964611, 0.1771653543307087630, 0.09757992244046791164 ) ) ;
#13997 = CARTESIAN_POINT ( 'NONE',  ( -0.4724409448818898682, -8.678599364036362592E-17, -0.2736220472440945017 ) ) ;
#13998 = CARTESIAN_POINT ( 'NONE',  ( 1.574803149606299746, -0.1870078740157480601, -0.3641732283464567677 ) ) ;
#13999 = CARTESIAN_POINT ( 'NONE',  ( 1.049868766404200127, -0.6046776061558809534, -0.2411417322834644161 ) ) ;
#14000 = CARTESIAN_POINT ( 'NONE',  ( -9.674558042662122972E-17, 0.3949938075777409963, -0.07677165354330710290 ) ) ;
#14001 = CARTESIAN_POINT ( 'NONE',  ( -0.05249343832020938322, -0.6046776061558809534, -0.2411417322834644161 ) ) ;
#14002 = CARTESIAN_POINT ( 'NONE',  ( -1.482939632545930975, 0.05413385826771666132, 0.4176697321401328100 ) ) ;
#14003 = VECTOR ( 'NONE', #77498, 39.37007874015748143 ) ;
#14004 = CARTESIAN_POINT ( 'NONE',  ( -1.384514435695537005, 0.2952755905511811885, 0.1292274648535926551 ) ) ;
#14005 = CARTESIAN_POINT ( 'NONE',  ( -0.2755905511811018171, 0.2952755905511811885, 0.000000000000000000 ) ) ;
#14006 = CARTESIAN_POINT ( 'NONE',  ( -0.2891555358219911054, 0.2891555358219909388, -0.09645669291338582196 ) ) ;
#14007 = CARTESIAN_POINT ( 'NONE',  ( 1.601049868766404982, -0.6046776061558809534, -0.2411417322834644161 ) ) ;
#14008 = CARTESIAN_POINT ( 'NONE',  ( 0.7349081364829402885, -0.6046776061558809534, -0.2411417322834644161 ) ) ;
#14009 = CARTESIAN_POINT ( 'NONE',  ( 0.9317585301837276734, -0.004921259842519870586, -0.3153832671262229437 ) ) ;
#14010 = CARTESIAN_POINT ( 'NONE',  ( -0.04593175853018303251, 0.2952755905511811885, 0.1292274648535926551 ) ) ;
#14011 = CARTESIAN_POINT ( 'NONE',  ( 0.2362204724409456558, -0.1870078740157479769, 0.3641732283464567677 ) ) ;
#14012 = CARTESIAN_POINT ( 'NONE',  ( -1.095800524934382292, -0.3162353388693409650, -0.4822834645669289433 ) ) ;
#14013 = CARTESIAN_POINT ( 'NONE',  ( -0.3996062992125986590, 0.1070741851644051723, -0.8969816272965877024 ) ) ;
#14014 = CARTESIAN_POINT ( 'NONE',  ( 1.069553805774278832, 0.2952755905511810774, -0.1292274648535930714 ) ) ;
#14015 = CARTESIAN_POINT ( 'NONE',  ( -0.1049643490035302024, -0.3917322834645671215, -0.8517060367454066805 ) ) ;
#14017 = CARTESIAN_POINT ( 'NONE',  ( 0.5314960629920925106, 2.742783273398276656, 3.197598479107681690 ) ) ;
#14016 = CARTESIAN_POINT ( 'NONE',  ( 0.8333333333333340365, -0.6692913385826771977, 0.1292274648535927661 ) ) ;
#14018 = DIRECTION ( 'NONE',  ( 1.000000000000000000, -0.000000000000000000, -0.000000000000000000 ) ) ;
#14019 = CARTESIAN_POINT ( 'NONE',  ( 0.3805774278215230400, -0.004921259842519870586, -0.3153832671262229437 ) ) ;
#14020 = CIRCLE ( 'NONE', #24744, 0.1574803149606299746 ) ;
#14021 = CARTESIAN_POINT ( 'NONE',  ( 0.5971128608923891301, 0.2952755905511810774, -0.1292274648535930714 ) ) ;
#14022 = CARTESIAN_POINT ( 'NONE',  ( 0.7414698162729664865, 0.2066929133858267931, 0.1054918080437490802 ) ) ;
#14023 = CARTESIAN_POINT ( 'NONE',  ( -1.049868766404198794, 0.1283753931104746893, -0.1820866141732285504 ) ) ;
#14024 = CARTESIAN_POINT ( 'NONE',  ( -0.8923884514435688198, 0.2306618581243847221, -0.2411417322834647770 ) ) ;
#14025 = CARTESIAN_POINT ( 'NONE',  ( -1.568241469816272105, -0.05778040916215522460, 0.4822834645669289988 ) ) ;
#14026 = CARTESIAN_POINT ( 'NONE',  ( 0.8005249343832028242, -0.4281496062992127816, -0.4176697321401328100 ) ) ;
#14027 = CARTESIAN_POINT ( 'NONE',  ( -1.601049868766403650, 0.1283753931104746893, -0.1820866141732285504 ) ) ;
#14028 =( BOUNDED_CURVE ( )  B_SPLINE_CURVE ( 2, ( #20660, #73255, #58953, #27376, #78750, #46733, #72425, #14775, #10111, #75319, #62682, #36584, #74086 ),
 .UNSPECIFIED., .F., .F. ) 
 B_SPLINE_CURVE_WITH_KNOTS ( ( 3, 2, 2, 2, 2, 2, 3 ),
 ( 0.5490332660251417973, 0.5492424242424243097, 0.5530303030303029832, 0.5568181818181818787, 0.5606060606060606633, 0.5643939393939394478, 0.5646030976112219602 ),
 .UNSPECIFIED. ) 
 CURVE ( )  GEOMETRIC_REPRESENTATION_ITEM ( )  RATIONAL_B_SPLINE_CURVE ( ( 0.9964447847208420805, 0.9981185001348091834, 1.000000000000000000, 0.9659258262890683122, 1.000000000000000000, 0.9659258262890683122, 1.000000000000000000, 0.9659258262890683122, 1.000000000000000000, 0.9659258262890683122, 1.000000000000000000, 0.9981185001348091834, 0.9964447847208420805 ) ) 
 REPRESENTATION_ITEM ( '' )  );
#14029 = CARTESIAN_POINT ( 'NONE',  ( 1.023944627548813768, 1.412952001865432239, -0.4588836347674642990 ) ) ;
#14030 = CARTESIAN_POINT ( 'NONE',  ( 0.5446194225721792126, -0.05778040916215560624, -0.4822834645669293319 ) ) ;
#14031 = CARTESIAN_POINT ( 'NONE',  ( -0.3996062992125984925, -0.1070741851644056858, 0.1922572178477689464 ) ) ;
#14032 = CARTESIAN_POINT ( 'NONE',  ( 1.666666666666667185, 0.05413385826771666132, 0.4176697321401328100 ) ) ;
#14033 = CARTESIAN_POINT ( 'NONE',  ( 1.404199475065617708, 0.05413385826771626580, -0.4176697321401330321 ) ) ;
#14034 = CARTESIAN_POINT ( 'NONE',  ( -1.502624671916009680, -0.08942795157528024563, -0.3641732283464568787 ) ) ;
#14035 = CARTESIAN_POINT ( 'NONE',  ( 1.023622047244095334, -0.1870078740157479769, 0.3641732283464567677 ) ) ;
#14036 = CARTESIAN_POINT ( 'NONE',  ( -1.391076115485563314, -0.5023911411419708095, -0.1820866141732282451 ) ) ;
#14037 = CARTESIAN_POINT ( 'NONE',  ( -0.3149606299212590610, -0.1870078740157480601, -0.3641732283464567677 ) ) ;
#14038 = CARTESIAN_POINT ( 'NONE',  ( 0.3458507752293908943, 0.3458507752293908943, -2.027559055118109743 ) ) ;
#14039 = CARTESIAN_POINT ( 'NONE',  ( 0.7283464566929140904, -0.4536011799217368745, -0.2665933059059886201 ) ) ;
#14040 = CARTESIAN_POINT ( 'NONE',  ( 0.6496062992125991586, -0.5400638737290845981, -0.3530559997133363437 ) ) ;
#14041 = CARTESIAN_POINT ( 'NONE',  ( 0.9448818897637802916, -0.1870078740157479769, 0.4822834645669291653 ) ) ;
#14042 = CARTESIAN_POINT ( 'NONE',  ( 0.1968503937007881344, -0.6692913385826771977, 8.415575281601705876E-17 ) ) ;
#14043 = ADVANCED_FACE ( 'NONE', ( #77764 ), #18447, .F. ) ;
#14044 = CARTESIAN_POINT ( 'NONE',  ( 0.7152230971128614723, -0.2845877964562161244, -0.3641732283464567121 ) ) ;
#14045 = CARTESIAN_POINT ( 'NONE',  ( 1.187664041994751285, -0.3162353388693409650, -0.4822834645669289433 ) ) ;
#14046 = EDGE_CURVE ( 'NONE', #18027, #57846, #17238, .T. ) ;
#14047 = EDGE_CURVE ( 'NONE', #64696, #712, #61293, .T. ) ;
#14048 = CARTESIAN_POINT ( 'NONE',  ( -1.594488188976377119, 0.1660481256975883668, -0.3530559997133364547 ) ) ;
#14049 = CARTESIAN_POINT ( 'NONE',  ( -0.5577427821522301654, -0.05778040916215560624, -0.4822834645669293319 ) ) ;
#14050 = CARTESIAN_POINT ( 'NONE',  ( 0.1070741851644053666, 0.3996062992125986035, -0.7808398950131233418 ) ) ;
#14051 = DIRECTION ( 'NONE',  ( 0.000000000000000000, -1.387778780781445676E-15, -1.000000000000000000 ) ) ;
#14052 = CARTESIAN_POINT ( 'NONE',  ( 0.2165354330708668673, 0.1660481256975883668, -0.3530559997133364547 ) ) ;
#14053 = CARTESIAN_POINT ( 'NONE',  ( -0.2887139107611542133, -0.6046776061558809534, -0.2411417322834644161 ) ) ;
#14054 = CARTESIAN_POINT ( 'NONE',  ( -0.2230971128608915943, -0.4281496062992127816, -0.4176697321401328100 ) ) ;
#14055 = CARTESIAN_POINT ( 'NONE',  ( 0.1070741851644054915, -0.3996062992125986035, -2.762467191601049255 ) ) ;
#14056 = CARTESIAN_POINT ( 'NONE',  ( -0.1058382717557503211, 0.3949938075777409408, -1.896325459317585116 ) ) ;
#14057 = CARTESIAN_POINT ( 'NONE',  ( 0.3917322834645669549, 0.1049643490035304660, -0.4317585301837270628 ) ) ;
#14058 = AXIS2_PLACEMENT_3D ( 'NONE', #9859, #60779, #8618 ) ;
#14059 = CARTESIAN_POINT ( 'NONE',  ( 0.3917322834645670104, -0.1049643490035303273, -1.206036745406823929 ) ) ;
#14060 = CARTESIAN_POINT ( 'NONE',  ( -0.8858267716535425107, 0.07958543189024071263, -0.2665933059059888421 ) ) ;
#14061 = CARTESIAN_POINT ( 'NONE',  ( 0.1049643490035303689, 0.3917322834645670104, -1.245406824146981561 ) ) ;
#14062 = CARTESIAN_POINT ( 'NONE',  ( -1.364829396325458521, 0.2306618581243847221, -0.2411417322834647770 ) ) ;
#14063 = CARTESIAN_POINT ( 'NONE',  ( -0.2867679344610364334, -0.2867679344610368219, 0.01839201919391258294 ) ) ;
#14064 = CARTESIAN_POINT ( 'NONE',  ( 0.4068241469816281097, 0.05413385826771666132, 0.4176697321401328100 ) ) ;
#14065 = CARTESIAN_POINT ( 'NONE',  ( -0.3543307086614165824, -0.5511811023622047445, 6.969142054262312111E-17 ) ) ;
#14066 = EDGE_CURVE ( 'NONE', #43230, #24616, #3649, .T. ) ;
#14067 = CARTESIAN_POINT ( 'NONE',  ( 1.082677165354331228, -0.5400638737290844871, 0.3530559997133364547 ) ) ;
#14068 = CARTESIAN_POINT ( 'NONE',  ( 0.1902887139107617975, 0.2952755905511811885, 0.1292274648535926551 ) ) ;
#14069 = CARTESIAN_POINT ( 'NONE',  ( -0.4724409448818899238, 0.1265901696524986964, -0.1095800524934383291 ) ) ;
#14070 = CARTESIAN_POINT ( 'NONE',  ( 4.893765752498283924E-17, -0.3996062992125986035, -2.755905511811023612 ) ) ;
#14071 = CARTESIAN_POINT ( 'NONE',  ( 0.2867679344610366554, 0.2867679344610366554, -1.079415641241156854 ) ) ;
#14072 = CARTESIAN_POINT ( 'NONE',  ( 1.128608923884515169, -0.6046776061558809534, -0.2411417322834644161 ) ) ;
#14073 = CARTESIAN_POINT ( 'NONE',  ( 0.6233595800524939223, -0.3162353388693405765, 0.4822834645669290543 ) ) ;
#14074 = CARTESIAN_POINT ( 'NONE',  ( 0.1706036745406830368, 0.05413385826771666132, 0.4176697321401328100 ) ) ;
#14076 = CARTESIAN_POINT ( 'NONE',  ( -1.601049868766403650, 0.2306618581243847221, -0.2411417322834647770 ) ) ;
#14075 = VECTOR ( 'NONE', #67520, 39.37007874015748854 ) ;
#14077 = CARTESIAN_POINT ( 'NONE',  ( 1.076115485564305141, 0.2306618581243847221, -0.2411417322834647770 ) ) ;
#14078 = CARTESIAN_POINT ( 'NONE',  ( 0.1049643490035303689, 0.3917322834645670104, -0.5505249343832020470 ) ) ;
#14079 = CARTESIAN_POINT ( 'NONE',  ( -0.1246719160104980823, 0.2952755905511811885, 0.1292274648535926551 ) ) ;
#14080 = CARTESIAN_POINT ( 'NONE',  ( 1.023622047244095334, -0.1870078740157479769, 0.4822834645669291653 ) ) ;
#14081 = CARTESIAN_POINT ( 'NONE',  ( 0.3346456692913393205, -0.5400638737290845981, -0.3530559997133363437 ) ) ;
#14082 = CARTESIAN_POINT ( 'NONE',  ( 1.259842519685040019, -0.1870078740157480601, -0.3641732283464567677 ) ) ;
#14083 = CARTESIAN_POINT ( 'NONE',  ( -0.9514435695538050464, -0.3162353388693405765, 0.4822834645669290543 ) ) ;
#14084 = CARTESIAN_POINT ( 'NONE',  ( -1.292650918635170010, -0.6692913385826771977, 0.1292274648535927661 ) ) ;
#14085 = CARTESIAN_POINT ( 'NONE',  ( 0.7480314960629927956, -0.6692913385826771977, 8.415575281601705876E-17 ) ) ;
#14086 = CARTESIAN_POINT ( 'NONE',  ( 0.3808816823641231752, -0.09156050430092187165, -1.929133858267716661 ) ) ;
#14087 = CARTESIAN_POINT ( 'NONE',  ( 0.1958661417322836440, -0.3392501089628017219, -1.973753280839895208 ) ) ;
#14088 = ORIENTED_EDGE ( 'NONE', *, *, #80532, .F. ) ;
#14089 = CARTESIAN_POINT ( 'NONE',  ( -0.1070741851644051862, -0.3996062992125987146, -0.5446194225721783244 ) ) ;
#14090 = ORIENTED_EDGE ( 'NONE', *, *, #52104, .T. ) ;
#14091 = CARTESIAN_POINT ( 'NONE',  ( 1.450131233595801428, -0.6692913385826773087, -0.1292274648535924053 ) ) ;
#14092 = CARTESIAN_POINT ( 'NONE',  ( 1.167979002624672580, -0.004921259842519870586, -0.3153832671262229437 ) ) ;
#14093 = CARTESIAN_POINT ( 'NONE',  ( -0.7773926554473638006, -2.191421614605370878E-15, 0.4445507791589071167 ) ) ;
#14094 = CARTESIAN_POINT ( 'NONE',  ( -0.4744094488189057879, 1.528788477448867367, 2.554262525012262142 ) ) ;
#14095 = DIRECTION ( 'NONE',  ( -0.000000000000000000, -1.000000000000000000, -0.000000000000000000 ) ) ;
#14096 = CARTESIAN_POINT ( 'NONE',  ( -0.3392501089628019995, 0.1958661417322832277, -1.055774278215223294 ) ) ;
#14097 = CARTESIAN_POINT ( 'NONE',  ( 1.555118110236221041, -0.5400638737290844871, 0.3530559997133364547 ) ) ;
#14098 = CARTESIAN_POINT ( 'NONE',  ( -1.633858267716534529, 0.1660481256975885056, 0.3530559997133364547 ) ) ;
#14099 = CARTESIAN_POINT ( 'NONE',  ( -0.3871391076115479057, -0.3162353388693409650, -0.4822834645669289433 ) ) ;
#14100 = CARTESIAN_POINT ( 'NONE',  ( 1.003937007874016185, 0.1660481256975883668, -0.3530559997133364547 ) ) ;
#14101 = VERTEX_POINT ( 'NONE', #3233 ) ;
#14102 = CARTESIAN_POINT ( 'NONE',  ( -1.646981627296586703, -0.3162353388693409650, -0.4822834645669289433 ) ) ;
#14103 = CARTESIAN_POINT ( 'NONE',  ( -1.016821367227983108, 1.506045768764721515, -0.4744094488188973502 ) ) ;
#14104 = DIRECTION ( 'NONE',  ( -1.000000000000000000, 0.000000000000000000, -3.491481338843133355E-15 ) ) ;
#14105 = LINE ( 'NONE', #39757, #69388 ) ;
#14106 = CARTESIAN_POINT ( 'NONE',  ( -3.937007874015748143, 2.755905511811024056, 0.5314960629921260393 ) ) ;
#14107 = CARTESIAN_POINT ( 'NONE',  ( -0.9317585301837263412, -0.3690944881889765550, -0.3153832671262227771 ) ) ;
#14108 = CARTESIAN_POINT ( 'NONE',  ( 0.9321091654255241332, 0.004960608223779158429, -0.3437734562760187962 ) ) ;
#14109 = CARTESIAN_POINT ( 'NONE',  ( 0.6036745406824154392, 0.2306618581243847221, -0.2411417322834647770 ) ) ;
#14110 = EDGE_LOOP ( 'NONE', ( #25948, #34968, #42110, #36183, #36919 ) ) ;
#14112 = CARTESIAN_POINT ( 'NONE',  ( -0.4133858267716528090, 0.1012011053420775880, -0.2882089793578257453 ) ) ;
#14111 = CARTESIAN_POINT ( 'NONE',  ( -0.4091458600556402980, -0.2362204724409451284, -2.491469816272966042 ) ) ;
#14113 = CARTESIAN_POINT ( 'NONE',  ( 0.6758530183727039509, -0.6692913385826771977, 0.1292274648535927661 ) ) ;
#14114 = CARTESIAN_POINT ( 'NONE',  ( -1.469816272965878357, -0.6046776061558809534, -0.2411417322834644161 ) ) ;
#14115 = CARTESIAN_POINT ( 'NONE',  ( -9.594673741351310580E-17, 0.3917322834645669549, -0.8674347524596309755 ) ) ;
#14116 = CARTESIAN_POINT ( 'NONE',  ( -0.6824146981627291497, -0.5023911411419708095, -0.1820866141732282451 ) ) ;
#14117 = CARTESIAN_POINT ( 'NONE',  ( -1.496062992125983815, -0.1870078740157479769, 0.3641732283464567677 ) ) ;
#14118 = CARTESIAN_POINT ( 'NONE',  ( -1.646051170424378096, 0.000000000000000000, 0.3464511005275205946 ) ) ;
#14119 =( GEOMETRIC_REPRESENTATION_CONTEXT ( 3 ) GLOBAL_UNCERTAINTY_ASSIGNED_CONTEXT ( ( #73958 ) ) GLOBAL_UNIT_ASSIGNED_CONTEXT ( ( #215, #25038, #6522 ) ) REPRESENTATION_CONTEXT ( 'NONE', 'WORKASPACE' ) );
#14120 = CARTESIAN_POINT ( 'NONE',  ( 0.4658792650918640033, -0.3162353388693405765, 0.4822834645669290543 ) ) ;
#14121 = CARTESIAN_POINT ( 'NONE',  ( -0.8398950131233585692, 0.1283753931104748280, 0.1820866141732283561 ) ) ;
#14122 = CARTESIAN_POINT ( 'NONE',  ( 0.01312335958005323398, -0.004921259842519576551, 0.3153832671262227771 ) ) ;
#14123 = CARTESIAN_POINT ( 'NONE',  ( -0.3608923884514428360, -0.6692913385826773087, -0.1292274648535924053 ) ) ;
#14124 = CARTESIAN_POINT ( 'NONE',  ( -1.286089238845143479, 0.1283753931104746893, -0.1820866141732285504 ) ) ;
#14125 = CARTESIAN_POINT ( 'NONE',  ( -0.3917322834645670104, -0.1049643490035307020, -0.2001505493776396805 ) ) ;
#14126 = CARTESIAN_POINT ( 'NONE',  ( 0.6430446194225728496, 0.05413385826771666132, 0.4176697321401328100 ) ) ;
#14127 = ADVANCED_FACE ( 'NONE', ( #9961 ), #23406, .F. ) ;
#14128 = CARTESIAN_POINT ( 'NONE',  ( -1.312335958005248715, 0.2306618581243848609, 0.2411417322834645549 ) ) ;
#14129 = CARTESIAN_POINT ( 'NONE',  ( 0.4724409448818896462, 0.1265901696524990294, -1.461286089238844843 ) ) ;
#14130 = CARTESIAN_POINT ( 'NONE',  ( -0.7086614173228339419, -0.1870078740157480879, -0.4822834645669291653 ) ) ;
#14131 = CARTESIAN_POINT ( 'NONE',  ( -0.01312335958005186876, -0.3690944881889763329, 0.3153832671262228327 ) ) ;
#14132 = CARTESIAN_POINT ( 'NONE',  ( -1.299212598425196097, 0.2952755905511811885, 0.000000000000000000 ) ) ;
#14133 = CARTESIAN_POINT ( 'NONE',  ( 1.036745406824147731, -0.004921259842519576551, 0.3153832671262227771 ) ) ;
#14134 = AXIS2_PLACEMENT_3D ( 'NONE', #21736, #60863, #2805 ) ;
#14135 = CARTESIAN_POINT ( 'NONE',  ( -0.3805774278215216522, -0.3690944881889765550, -0.3153832671262227771 ) ) ;
#14136 = CARTESIAN_POINT ( 'NONE',  ( -1.122047244094487306, -0.5400638737290844871, 0.3530559997133364547 ) ) ;
#14137 = CARTESIAN_POINT ( 'NONE',  ( -1.154855643044618851, -0.6046776061558809534, -0.2411417322834644161 ) ) ;
#14138 = CARTESIAN_POINT ( 'NONE',  ( -1.627296587926508442, 0.2306618581243848609, 0.2411417322834645549 ) ) ;
#14139 = CARTESIAN_POINT ( 'NONE',  ( 1.089238845144357759, 0.009842519685039147898, -0.3409548833797004797 ) ) ;
#14140 = CARTESIAN_POINT ( 'NONE',  ( 1.115485564304462551, -0.3690944881889765550, -0.3153832671262227771 ) ) ;
#14141 = CARTESIAN_POINT ( 'NONE',  ( 0.2230971128608932319, -0.4281496062992124485, 0.4176697321401328655 ) ) ;
#14142 = CARTESIAN_POINT ( 'NONE',  ( -1.555118110236219930, -0.5400638737290845981, -0.3530559997133363437 ) ) ;
#14143 = CARTESIAN_POINT ( 'NONE',  ( -1.345144356955379816, -0.05778040916215560624, -0.4822834645669293319 ) ) ;
#14144 = ORIENTED_EDGE ( 'NONE', *, *, #21499, .F. ) ;
#14145 = CARTESIAN_POINT ( 'NONE',  ( -0.1070741851644051862, -0.3996062992125986590, -2.196194225721784576 ) ) ;
#14146 = CARTESIAN_POINT ( 'NONE',  ( -1.089238845144356427, -0.3690944881889765550, -0.3153832671262227771 ) ) ;
#14147 = CARTESIAN_POINT ( 'NONE',  ( 0.7808398950131240079, -0.3162353388693405765, 0.4822834645669290543 ) ) ;
#14148 = CARTESIAN_POINT ( 'NONE',  ( -1.246719160104986512, -0.004921259842519576551, 0.3153832671262227771 ) ) ;
#14149 = CARTESIAN_POINT ( 'NONE',  ( -0.2925321140481932369, 0.2925321140481931259, -1.828740157480315265 ) ) ;
#14150 = CARTESIAN_POINT ( 'NONE',  ( -1.561679790026246017, 0.05413385826771666132, 0.4176697321401328100 ) ) ;
#14151 = CARTESIAN_POINT ( 'NONE',  ( 1.023622047244095334, -0.1870078740157479769, 0.4822834645669291653 ) ) ;
#14152 = CARTESIAN_POINT ( 'NONE',  ( 0.5249343832021005074, -0.6046776061558807314, 0.2411417322834647770 ) ) ;
#14153 = CARTESIAN_POINT ( 'NONE',  ( 1.095800524934383846, -0.3162353388693405765, 0.4822834645669290543 ) ) ;
#14154 = CARTESIAN_POINT ( 'NONE',  ( -1.364829396325458521, 0.1283753931104746893, -0.1820866141732285504 ) ) ;
#14155 = CARTESIAN_POINT ( 'NONE',  ( -0.2925321140481932369, 0.2925321140481930704, -1.198818897637795367 ) ) ;
#14156 = CARTESIAN_POINT ( 'NONE',  ( 0.1998031496062994405, -0.3460692066303958092, -1.509186351706036655 ) ) ;
#14157 = CARTESIAN_POINT ( 'NONE',  ( -0.1974969037888703871, -0.3420746716998661063, -0.6955380577427822120 ) ) ;
#14158 = CARTESIAN_POINT ( 'NONE',  ( 0.4725026149319347391, 1.580736828574228703, 2.558921551581183174 ) ) ;
#14159 = CARTESIAN_POINT ( 'NONE',  ( 0.5708661417322842269, 0.07958543189024085140, 0.2665933059059887866 ) ) ;
#14160 = CARTESIAN_POINT ( 'NONE',  ( 0.3215223097112867578, -0.08942795157527998196, 0.3641732283464567121 ) ) ;
#14161 = CARTESIAN_POINT ( 'NONE',  ( 0.1574803149606306130, -0.1870078740157479769, 0.4822834645669291653 ) ) ;
#14162 = CARTESIAN_POINT ( 'NONE',  ( 1.430446194225722500, 0.05413385826771666132, 0.4176697321401328100 ) ) ;
#14163 = CARTESIAN_POINT ( 'NONE',  ( -0.3420746716998660508, -0.1974969037888706924, -1.546587926509186417 ) ) ;
#14164 = CARTESIAN_POINT ( 'NONE',  ( 0.5380577427821529035, -0.3690944881889763329, 0.3153832671262228327 ) ) ;
#14165 = CARTESIAN_POINT ( 'NONE',  ( -0.5314960629921250401, 0.1660481256975885056, 0.3530559997133364547 ) ) ;
#14166 = CARTESIAN_POINT ( 'NONE',  ( -1.548556430446193399, -0.6046776061558809534, -0.2411417322834644161 ) ) ;
#14167 = CARTESIAN_POINT ( 'NONE',  ( 0.8923884514435703741, 0.2306618581243848609, 0.2411417322834645549 ) ) ;
#14168 = CARTESIAN_POINT ( 'NONE',  ( 5.785732909357575061E-17, -0.4724409448818898682, -1.968503937007873850 ) ) ;
#14169 = CARTESIAN_POINT ( 'NONE',  ( 1.220472440944882386, 0.2952755905511811885, 0.000000000000000000 ) ) ;
#14170 = ORIENTED_EDGE ( 'NONE', *, *, #75948, .T. ) ;
#14171 = VERTEX_POINT ( 'NONE', #4466 ) ;
#14172 = CARTESIAN_POINT ( 'NONE',  ( -1.115485564304461219, -0.4281496062992124485, 0.4176697321401328655 ) ) ;
#14174 = CARTESIAN_POINT ( 'NONE',  ( -1.246719160104985846, -0.4281496062992127816, -0.4176697321401328100 ) ) ;
#14173 = CARTESIAN_POINT ( 'NONE',  ( -0.6430446194225712953, -0.004921259842519870586, -0.3153832671262229437 ) ) ;
#14175 = CARTESIAN_POINT ( 'NONE',  ( -0.3917322834645670659, 0.1049643490035301607, -2.317565986055430738 ) ) ;
#14176 = FACE_OUTER_BOUND ( 'NONE', #30818, .T. ) ;
#14177 = CARTESIAN_POINT ( 'NONE',  ( -1.535433070866141225, -0.5511811023622047445, 6.969142054262312111E-17 ) ) ;
#14178 = CARTESIAN_POINT ( 'NONE',  ( -1.089238845144356427, 0.05413385826771666132, 0.4176697321401328100 ) ) ;
#14179 = CARTESIAN_POINT ( 'NONE',  ( 0.1509186351706042484, -0.3162353388693405765, 0.4822834645669290543 ) ) ;
#14180 = CARTESIAN_POINT ( 'NONE',  ( -1.286089238845143479, 0.2306618581243847221, -0.2411417322834647770 ) ) ;
#14181 = CARTESIAN_POINT ( 'NONE',  ( 0.3392501089628018329, 0.1958661417322835052, -2.730951812827084435 ) ) ;
#14182 = CARTESIAN_POINT ( 'NONE',  ( 0.5905511811023629321, -0.6692913385826771977, 8.415575281601705876E-17 ) ) ;
#14183 = CARTESIAN_POINT ( 'NONE',  ( 0.1049643490035304938, -0.3917322834645669549, -1.809711286089239035 ) ) ;
#14184 = CARTESIAN_POINT ( 'NONE',  ( -0.7677165354330699465, -0.4536011799217368745, -0.2665933059059886201 ) ) ;
#14185 = ORIENTED_EDGE ( 'NONE', *, *, #3063, .T. ) ;
#14186 = CARTESIAN_POINT ( 'NONE',  ( 0.3949938075777409963, 2.418639510665530435E-17, -1.692913385826771533 ) ) ;
#14187 = VERTEX_POINT ( 'NONE', #56217 ) ;
#14188 = CARTESIAN_POINT ( 'NONE',  ( -0.6410189441372351471, -3.721645946415733147E-15, -0.3954974714151476278 ) ) ;
#14189 = VECTOR ( 'NONE', #29537, 39.37007874015748143 ) ;
#14190 = CARTESIAN_POINT ( 'NONE',  ( -1.115485564304461219, -0.4281496062992124485, 0.4176697321401328655 ) ) ;
#14191 = CARTESIAN_POINT ( 'NONE',  ( -1.482939632545930975, 0.05413385826771666132, 0.4176697321401328100 ) ) ;
#14192 = CARTESIAN_POINT ( 'NONE',  ( 0.3460692066303959757, -0.1998031496062991907, -0.5774278215223097588 ) ) ;
#14193 = CARTESIAN_POINT ( 'NONE',  ( -1.679790026246718693, 0.2306618581243847221, -0.2411417322834647770 ) ) ;
#14194 = CARTESIAN_POINT ( 'NONE',  ( -1.364829396325458521, 0.2306618581243847221, -0.2411417322834647770 ) ) ;
#14195 = CARTESIAN_POINT ( 'NONE',  ( -1.548556430446193399, -0.6046776061558809534, -0.2411417322834644161 ) ) ;
#14196 = ADVANCED_FACE ( 'NONE', ( #42756 ), #74773, .F. ) ;
#14197 = DIRECTION ( 'NONE',  ( 0.000000000000000000, -0.5150380749100561539, -0.8571673007021108903 ) ) ;
#14198 = CARTESIAN_POINT ( 'NONE',  ( -0.01312335958005186876, -0.004921259842519870586, -0.3153832671262229437 ) ) ;
#14199 = DIRECTION ( 'NONE',  ( 1.000000000000000000, 0.000000000000000000, 0.000000000000000000 ) ) ;
#14200 = CARTESIAN_POINT ( 'NONE',  ( -0.2867679344610365999, 0.2867679344610364889, -0.2618110236220473341 ) ) ;
#14201 = CARTESIAN_POINT ( 'NONE',  ( -0.1902887139107604098, -0.5511811023622046335, 0.09757992244046803654 ) ) ;
#14202 = CARTESIAN_POINT ( 'NONE',  ( -0.8005249343832011588, 0.05413385826771626580, -0.4176697321401330321 ) ) ;
#14203 = EDGE_CURVE ( 'NONE', #28644, #59098, #66630, .T. ) ;
#14204 = CARTESIAN_POINT ( 'NONE',  ( 0.9580052493438326877, 0.05413385826771666132, 0.4176697321401328100 ) ) ;
#14205 = CARTESIAN_POINT ( 'NONE',  ( -1.089238845144356427, -0.4281496062992127816, -0.4176697321401328100 ) ) ;
#14206 = VERTEX_POINT ( 'NONE', #68041 ) ;
#14207 = EDGE_LOOP ( 'NONE', ( #60952, #75599, #55224, #46243, #18435, #5295, #68335 ) ) ;
#14208 = CARTESIAN_POINT ( 'NONE',  ( -1.036745406824146176, -0.4281496062992124485, 0.4176697321401328655 ) ) ;
#14209 = CARTESIAN_POINT ( 'NONE',  ( 0.8792650918635177559, -0.4281496062992127816, -0.4176697321401328100 ) ) ;
#14210 = CARTESIAN_POINT ( 'NONE',  ( -1.509186351706035767, -0.004921259842519870586, -0.3153832671262229437 ) ) ;
#14211 = CARTESIAN_POINT ( 'NONE',  ( -0.2362204724409451284, 0.4091458600556402425, -1.272965879265091749 ) ) ;
#14212 = CARTESIAN_POINT ( 'NONE',  ( 2.153082335389886026, 1.453547212638085062, 0.4672029448317644440 ) ) ;
#14213 = CARTESIAN_POINT ( 'NONE',  ( -0.1049643490035307020, 0.3917322834645669549, -0.1561679790026246351 ) ) ;
#14214 = CARTESIAN_POINT ( 'NONE',  ( -0.3917322834645669549, -0.1049643490035306603, -2.335301837270341352 ) ) ;
#14215 = CARTESIAN_POINT ( 'NONE',  ( -0.2099737532808391705, 0.2306618581243848609, 0.2411417322834645549 ) ) ;
#14216 = CARTESIAN_POINT ( 'NONE',  ( 1.666666666666667185, 0.05413385826771666132, 0.4176697321401328100 ) ) ;
#14217 = CARTESIAN_POINT ( 'NONE',  ( -0.9055118110236215490, 0.2952755905511811885, 0.000000000000000000 ) ) ;
#14218 = CARTESIAN_POINT ( 'NONE',  ( 0.3996062992125986035, -0.1070741851644052972, -0.03083989501312338344 ) ) ;
#14220 = CARTESIAN_POINT ( 'NONE',  ( -0.5314960629921373636, 2.742781055772889331, 3.250800393950209699 ) ) ;
#14219 = CARTESIAN_POINT ( 'NONE',  ( -1.410761154855642463, -0.05778040916215522460, 0.4822834645669289988 ) ) ;
#14221 = CARTESIAN_POINT ( 'NONE',  ( -1.089238845144356427, 0.05413385826771666132, 0.4176697321401328100 ) ) ;
#14222 = CARTESIAN_POINT ( 'NONE',  ( -0.3937007874015740483, -0.1870078740157480879, -0.4822834645669291653 ) ) ;
#14223 = CARTESIAN_POINT ( 'NONE',  ( -0.1058382717557503072, 0.3949938075777408852, -2.760498687664042716 ) ) ;
#14224 = CARTESIAN_POINT ( 'NONE',  ( 0.5905511811023629321, -0.5511811023622047445, 6.969142054262312111E-17 ) ) ;
#14225 = CYLINDRICAL_SURFACE ( 'NONE', #12888, 2.362204724409449064 ) ;
#14226 = CARTESIAN_POINT ( 'NONE',  ( 0.3871391076115493490, -0.2845877964562159024, 0.3641732283464567677 ) ) ;
#14227 = CARTESIAN_POINT ( 'NONE',  ( 1.233595800524935227, -0.5023911411419708095, 0.1820866141732285504 ) ) ;
#14228 = CARTESIAN_POINT ( 'NONE',  ( 1.338582677165355062, -0.1870078740157480879, -0.4822834645669291653 ) ) ;
#14229 = CARTESIAN_POINT ( 'NONE',  ( 0.2034120734908144990, -0.5511811023622046335, 0.09757992244046803654 ) ) ;
#14230 = CARTESIAN_POINT ( 'NONE',  ( 0.3392501089628018884, -0.1958661417322834220, -1.986876640419947604 ) ) ;
#14231 = CARTESIAN_POINT ( 'NONE',  ( -1.450131233595799651, 0.2952755905511810774, -0.1292274648535930714 ) ) ;
#14232 = CARTESIAN_POINT ( 'NONE',  ( -0.1377952755905504645, 0.07958543189024085140, 0.2665933059059887866 ) ) ;
#14233 = EDGE_CURVE ( 'NONE', #199, #57945, #17558, .T. ) ;
#14234 = CARTESIAN_POINT ( 'NONE',  ( 5.785732909357575061E-17, -0.4724409448818898682, 0.001968503937007862279 ) ) ;
#14235 = CARTESIAN_POINT ( 'NONE',  ( -0.4527559055118102749, -0.4536011799217368745, -0.2665933059059886201 ) ) ;
#14236 = CARTESIAN_POINT ( 'NONE',  ( 0.05905511811023682334, 0.1660481256975883391, -0.3530559997133364547 ) ) ;
#14237 = CARTESIAN_POINT ( 'NONE',  ( 0.4986876640419954376, -0.6046776061558809534, -0.2411417322834644161 ) ) ;
#14238 = CARTESIAN_POINT ( 'NONE',  ( 0.5120078740157480990, 0.000000000000000000, -0.4921259842519685179 ) ) ;
#14239 = EDGE_CURVE ( 'NONE', #69836, #13510, #51018, .T. ) ;
#14240 = CARTESIAN_POINT ( 'NONE',  ( 0.8792650918635177559, -0.3690944881889765550, -0.3153832671262227771 ) ) ;
#14241 = CARTESIAN_POINT ( 'NONE',  ( 0.1902887139107617975, 0.1771653543307087630, 0.09757992244046791164 ) ) ;
#14242 = CARTESIAN_POINT ( 'NONE',  ( -0.1771653543307080136, 0.1660481256975883668, -0.3530559997133364547 ) ) ;
#14243 = DIRECTION ( 'NONE',  ( 0.000000000000000000, -1.000000000000000000, 0.000000000000000000 ) ) ;
#14244 = CARTESIAN_POINT ( 'NONE',  ( -0.5380577427821514602, -0.004921259842519576551, 0.3153832671262227771 ) ) ;
#14245 = CARTESIAN_POINT ( 'NONE',  ( 0.2952755905511810774, 3.616083068348483797E-17, 6.043307086614173151 ) ) ;
#14246 = CARTESIAN_POINT ( 'NONE',  ( 0.3740157480314966754, -0.5400638737290844871, 0.3530559997133364547 ) ) ;
#14247 = CARTESIAN_POINT ( 'NONE',  ( -0.8005249343832011588, 0.05413385826771626580, -0.4176697321401330321 ) ) ;
#14248 = CARTESIAN_POINT ( 'NONE',  ( 0.1070741851644053388, 0.3996062992125986035, -1.015091863517060267 ) ) ;
#14249 = CARTESIAN_POINT ( 'NONE',  ( 0.1049643490035303689, 0.3917322834645670104, -2.755249343832020248 ) ) ;
#14250 = CARTESIAN_POINT ( 'NONE',  ( 0.1640419947506569498, -0.08942795157527998196, 0.3641732283464567121 ) ) ;
#14251 = CARTESIAN_POINT ( 'NONE',  ( -0.9448818897637790704, -0.1870078740157480879, -0.4822834645669291653 ) ) ;
#14252 = VECTOR ( 'NONE', #41812, 39.37007874015748143 ) ;
#14253 = CARTESIAN_POINT ( 'NONE',  ( -1.115485564304461219, 0.05413385826771626580, -0.4176697321401330321 ) ) ;
#14254 = CARTESIAN_POINT ( 'NONE',  ( -1.227034120734907141, -0.5511811023622048555, -0.09757992244046775898 ) ) ;
#14255 = CARTESIAN_POINT ( 'NONE',  ( 1.614173228346457378, 0.5038684218300978346, -0.1372047244094476148 ) ) ;
#14256 = CARTESIAN_POINT ( 'NONE',  ( -0.6955380577427815458, -0.004921259842519576551, 0.3153832671262227771 ) ) ;
#14257 = CARTESIAN_POINT ( 'NONE',  ( 2.795275590551181466, 0.7480314960629931287, -2.695814348275282069E-16 ) ) ;
#14258 = CARTESIAN_POINT ( 'NONE',  ( 1.017060367454068581, -0.05778040916215560624, -0.4822834645669293319 ) ) ;
#14259 = CARTESIAN_POINT ( 'NONE',  ( -0.1070741851644056997, 0.3996062992125986035, -0.006561679790026256169 ) ) ;
#14260 = CARTESIAN_POINT ( 'NONE',  ( 0.3392501089628018329, 0.1958661417322835607, -2.332696481136169453 ) ) ;
#14261 = ORIENTED_EDGE ( 'NONE', *, *, #52608, .F. ) ;
#14262 = CARTESIAN_POINT ( 'NONE',  ( 0.4744094488189063985, 1.546135192374304523, -2.554262525012259033 ) ) ;
#14263 = CARTESIAN_POINT ( 'NONE',  ( 1.522309711286089939, -0.5023911411419708095, -0.1820866141732282451 ) ) ;
#14264 = CARTESIAN_POINT ( 'NONE',  ( -1.259842519685038686, -0.1870078740157479769, 0.4822834645669291653 ) ) ;
#14265 = CARTESIAN_POINT ( 'NONE',  ( 1.049868766404200127, -0.6046776061558809534, -0.2411417322834644161 ) ) ;
#14266 = CARTESIAN_POINT ( 'NONE',  ( -0.2867679344610365999, 0.2867679344610364889, -2.466535433070865757 ) ) ;
#14267 = DIRECTION ( 'NONE',  ( 0.7071067811865495711, -0.000000000000000000, -0.7071067811865454633 ) ) ;
#14268 = CARTESIAN_POINT ( 'NONE',  ( 0.7349081364829403995, 0.2306618581243848609, 0.2411417322834645549 ) ) ;
#14269 = CARTESIAN_POINT ( 'NONE',  ( -0.5314960629921250401, 0.1660481256975885056, 0.3530559997133364547 ) ) ;
#14270 = CARTESIAN_POINT ( 'NONE',  ( 0.4494645459842863122, 1.384795284186596254, -3.911270042648091305 ) ) ;
#14271 = CARTESIAN_POINT ( 'NONE',  ( -0.3460692066303960868, 0.1998031496062990242, -2.073490813648294129 ) ) ;
#14272 = CARTESIAN_POINT ( 'NONE',  ( 0.6824146981627303710, 0.1283753931104746893, -0.1820866141732285504 ) ) ;
#14273 = CARTESIAN_POINT ( 'NONE',  ( -0.3460692066303958092, -0.1998031496062994683, -1.154855643044619518 ) ) ;
#14274 = EDGE_LOOP ( 'NONE', ( #68479, #34347, #75062, #12005 ) ) ;
#14275 = CARTESIAN_POINT ( 'NONE',  ( 0.3917322834645670659, 2.398668435337828261E-17, 0.04263160285333144478 ) ) ;
#14276 = ORIENTED_EDGE ( 'NONE', *, *, #61363, .T. ) ;
#14277 = CARTESIAN_POINT ( 'NONE',  ( -0.02624671916010428221, -0.6046776061558807314, 0.2411417322834647770 ) ) ;
#14278 = CARTESIAN_POINT ( 'NONE',  ( 1.338582677165355062, -0.1870078740157480879, -0.4822834645669291653 ) ) ;
#14279 = CARTESIAN_POINT ( 'NONE',  ( 0.2755905511811031494, 0.2952755905511811885, 0.000000000000000000 ) ) ;
#14280 = CARTESIAN_POINT ( 'NONE',  ( 1.148293963254593875, -0.6692913385826771977, 0.1292274648535927661 ) ) ;
#14281 = CARTESIAN_POINT ( 'NONE',  ( -0.6955380577427815458, 0.05413385826771666132, 0.4176697321401328100 ) ) ;
#14282 = CARTESIAN_POINT ( 'NONE',  ( 0.09186351706036799403, -0.4281496062992127816, -0.4176697321401328100 ) ) ;
#14283 = CARTESIAN_POINT ( 'NONE',  ( 1.463254593175853824, 0.2952755905511810774, -0.1292274648535930714 ) ) ;
#14284 = CARTESIAN_POINT ( 'NONE',  ( 1.181102362204724976, -0.1870078740157480879, -0.4822834645669291653 ) ) ;
#14285 = CARTESIAN_POINT ( 'NONE',  ( 0.9711286089238851948, -0.6046776061558809534, -0.2411417322834644161 ) ) ;
#14286 = CARTESIAN_POINT ( 'NONE',  ( -0.3917322834645671215, 0.1049643490035301469, -0.4973753280839895430 ) ) ;
#14287 = CARTESIAN_POINT ( 'NONE',  ( 0.5314960629921267055, -0.4536011799217367080, 0.2665933059059888421 ) ) ;
#14288 = ORIENTED_EDGE ( 'NONE', *, *, #11333, .F. ) ;
#14289 = CARTESIAN_POINT ( 'NONE',  ( -0.1058382717557503211, 0.3949938075777409408, -0.7939632545931760710 ) ) ;
#14290 = CONICAL_SURFACE ( 'NONE', #7550, 0.1978346456692914035, 0.8726646259971700959 ) ;
#14291 = ORIENTED_EDGE ( 'NONE', *, *, #54265, .F. ) ;
#14292 = CARTESIAN_POINT ( 'NONE',  ( -0.5183727034120726440, -0.5511811023622048555, -0.09757992244046775898 ) ) ;
#14293 = CIRCLE ( 'NONE', #62644, 0.01968503937007875723 ) ;
#14294 = AXIS2_PLACEMENT_3D ( 'NONE', #24136, #81410, #23727 ) ;
#14295 = CARTESIAN_POINT ( 'NONE',  ( -0.2099737532808391705, 0.2306618581243848609, 0.2411417322834645549 ) ) ;
#14296 = CARTESIAN_POINT ( 'NONE',  ( -1.531218781212690727, 1.129506115079992101, 0.2422809976808260046 ) ) ;
#14297 = CARTESIAN_POINT ( 'NONE',  ( -0.4855643044619415427, -0.4281496062992124485, 0.4176697321401328655 ) ) ;
#14298 = CARTESIAN_POINT ( 'NONE',  ( 5.463695987328526437E-16, -0.1870078740157479769, 0.4822834645669291653 ) ) ;
#14299 = CARTESIAN_POINT ( 'NONE',  ( -0.7414698162729651543, -0.6692913385826771977, 0.1292274648535927661 ) ) ;
#14300 = EDGE_CURVE ( 'NONE', #9114, #59294, #10387, .T. ) ;
#14301 = CARTESIAN_POINT ( 'NONE',  ( -1.102362204724408601, -0.1870078740157479769, 0.4822834645669291653 ) ) ;
#14302 = CARTESIAN_POINT ( 'NONE',  ( 1.259842519685040019, -0.1870078740157480601, -0.3641732283464567677 ) ) ;
#14303 = PLANE ( 'NONE',  #11656 ) ;
#14304 = CARTESIAN_POINT ( 'NONE',  ( -2.199130528046420221E-22, 1.075705580628688596, 0.2362204724409449064 ) ) ;
#14305 = CARTESIAN_POINT ( 'NONE',  ( 1.036745406824147508, -0.3690944881889765550, -0.3153832671262227771 ) ) ;
#14306 = CARTESIAN_POINT ( 'NONE',  ( 0.5314960629921267055, -0.5400638737290844871, 0.3530559997133364547 ) ) ;
#14307 = CARTESIAN_POINT ( 'NONE',  ( 0.6102362204724416372, 0.1660481256975883668, -0.3530559997133364547 ) ) ;
#14308 = CARTESIAN_POINT ( 'NONE',  ( -0.3996062992125986035, -7.340648628747425578E-17, -1.299212598425196985 ) ) ;
#14309 = CARTESIAN_POINT ( 'NONE',  ( -1.732283464566928277, -0.1870078740157479769, 0.4822834645669291653 ) ) ;
#14310 = CARTESIAN_POINT ( 'NONE',  ( 0.3996062992125984925, 0.1070741851644054637, -0.8313648293963252778 ) ) ;
#14311 = CARTESIAN_POINT ( 'NONE',  ( -0.3996062992125986590, 0.1070741851644051723, -0.4245406824146981672 ) ) ;
#14312 = CARTESIAN_POINT ( 'NONE',  ( -0.4921259842519677963, -0.5400638737290844871, 0.3530559997133364547 ) ) ;
#14313 = CARTESIAN_POINT ( 'NONE',  ( -0.4091458600556405756, 0.2362204724409446288, -0.02624671916010498651 ) ) ;
#14314 = B_SPLINE_CURVE_WITH_KNOTS ( 'NONE', 3,
 ( #26298, #39340, #57446, #65027 ),
 .UNSPECIFIED., .F., .F.,
 ( 4, 4 ),
 ( 0.07138240964905806507, 0.07282471043319424520 ),
 .UNSPECIFIED. ) ;
#14315 = CARTESIAN_POINT ( 'NONE',  ( -0.1049643490035307020, 0.3917322834645669549, -1.980971128608924214 ) ) ;
#14316 = CARTESIAN_POINT ( 'NONE',  ( -1.148293963254592542, 0.1771653543307087630, 0.09757992244046791164 ) ) ;
#14317 = CARTESIAN_POINT ( 'NONE',  ( 1.062992125984252745, -0.6692913385826771977, 8.415575281601705876E-17 ) ) ;
#14318 = VECTOR ( 'NONE', #28066, 39.37007874015748143 ) ;
#14319 = CARTESIAN_POINT ( 'NONE',  ( 1.076115485564305141, 0.2306618581243847221, -0.2411417322834647770 ) ) ;
#14320 = CARTESIAN_POINT ( 'NONE',  ( -0.3740157480314953431, 0.07958543189024085140, 0.2665933059059887866 ) ) ;
#14321 = CARTESIAN_POINT ( 'NONE',  ( 0.6824146981627303710, 0.2306618581243847221, -0.2411417322834647770 ) ) ;
#14322 = CARTESIAN_POINT ( 'NONE',  ( 0.4724409448818896462, 0.1265901696524990294, -1.933727034120735100 ) ) ;
#14323 = CARTESIAN_POINT ( 'NONE',  ( -0.1837270341207340729, 0.1283753931104746893, -0.1820866141732285504 ) ) ;
#14324 = CARTESIAN_POINT ( 'NONE',  ( 0.1181102362204730916, -0.6692913385826771977, 8.415575281601705876E-17 ) ) ;
#14325 = CARTESIAN_POINT ( 'NONE',  ( -0.2891555358219909388, -0.2891555358219912164, -1.553149606299212504 ) ) ;
#14326 = CARTESIAN_POINT ( 'NONE',  ( -1.194225721784776262, 0.05413385826771626580, -0.4176697321401330321 ) ) ;
#14327 = CARTESIAN_POINT ( 'NONE',  ( 0.4724409448818904789, -0.1870078740157479769, 0.3641732283464567677 ) ) ;
#14328 = CARTESIAN_POINT ( 'NONE',  ( 1.417322834645670104, -0.1870078740157480601, -0.3641732283464567677 ) ) ;
#14329 = CARTESIAN_POINT ( 'NONE',  ( -0.7349081364829390672, 0.2306618581243847221, -0.2411417322834647770 ) ) ;
#14330 = CARTESIAN_POINT ( 'NONE',  ( -0.2493438320209966919, -0.3690944881889763329, 0.3153832671262228327 ) ) ;
#14331 = CARTESIAN_POINT ( 'NONE',  ( -0.7478466213799872531, 1.968503937007873850, -0.5309055118110235227 ) ) ;
#14332 = CARTESIAN_POINT ( 'NONE',  ( -0.7152230971128602510, -0.05778040916215560624, -0.4822834645669293319 ) ) ;
#14333 = CARTESIAN_POINT ( 'NONE',  ( -0.5708661417322825615, -0.5400638737290844871, 0.3530559997133364547 ) ) ;
#14334 = CARTESIAN_POINT ( 'NONE',  ( -0.03280839895013062252, 0.2952755905511810774, -0.1292274648535930714 ) ) ;
#14335 = CARTESIAN_POINT ( 'NONE',  ( 0.1998031496062992463, 0.3460692066303959202, -2.110892388451443669 ) ) ;
#14336 = CARTESIAN_POINT ( 'NONE',  ( 0.1049643490035304522, -0.3917322834645668994, -2.055098794454381927 ) ) ;
#14337 = CARTESIAN_POINT ( 'NONE',  ( -1.489501312335957062, -0.2845877964562161244, -0.3641732283464567121 ) ) ;
#14338 = CARTESIAN_POINT ( 'NONE',  ( 0.6036745406824154392, 0.1283753931104746893, -0.1820866141732285504 ) ) ;
#14339 = CARTESIAN_POINT ( 'NONE',  ( 1.220472440944882386, -0.6692913385826771977, 8.415575281601705876E-17 ) ) ;
#14340 = CARTESIAN_POINT ( 'NONE',  ( -0.6102362204724400829, 0.07958543189024085140, 0.2665933059059887866 ) ) ;
#14341 = CARTESIAN_POINT ( 'NONE',  ( -1.128608923884513837, -0.5023911411419708095, 0.1820866141732285504 ) ) ;
#14342 = CARTESIAN_POINT ( 'NONE',  ( -0.6692913385826764205, 0.2952755905511811885, 0.000000000000000000 ) ) ;
#14343 = CARTESIAN_POINT ( 'NONE',  ( -0.6692913385826764205, -0.6692913385826771977, 8.415575281601705876E-17 ) ) ;
#14344 = CARTESIAN_POINT ( 'NONE',  ( 0.6036745406824154392, 0.1283753931104746893, -0.1820866141732285504 ) ) ;
#14345 = CARTESIAN_POINT ( 'NONE',  ( -0.2405786259268995197, 0.1712252042737591462, 5.748956133594166573 ) ) ;
#14346 = CARTESIAN_POINT ( 'NONE',  ( 1.043307086614173818, -0.4536011799217368745, -0.2665933059059886201 ) ) ;
#14347 = CARTESIAN_POINT ( 'NONE',  ( 0.3674540682414705883, -0.6046776061558807314, 0.2411417322834647770 ) ) ;
#14348 = CARTESIAN_POINT ( 'NONE',  ( 0.03416814150274168765, 1.063911309852949794, -1.851246078702575959 ) ) ;
#14349 = CARTESIAN_POINT ( 'NONE',  ( -0.7283464566929126471, 0.1660481256975883668, -0.3530559997133364547 ) ) ;
#14350 = VECTOR ( 'NONE', #81309, 39.37007874015748143 ) ;
#14351 = CARTESIAN_POINT ( 'NONE',  ( 0.2867679344610365999, -0.2867679344610365444, -1.600393700787401619 ) ) ;
#14352 = CARTESIAN_POINT ( 'NONE',  ( 1.246719160104987623, -0.3690944881889763329, 0.3153832671262228327 ) ) ;
#14354 = CARTESIAN_POINT ( 'NONE',  ( 0.4068241469816281097, 0.05413385826771666132, 0.4176697321401328100 ) ) ;
#14353 = VECTOR ( 'NONE', #6564, 39.37007874015748143 ) ;
#14355 = VECTOR ( 'NONE', #69831, 39.37007874015748143 ) ;
#14356 = CARTESIAN_POINT ( 'NONE',  ( 0.2690288713910767848, 0.2952755905511811885, 0.1292274648535926551 ) ) ;
#14357 = CARTESIAN_POINT ( 'NONE',  ( -0.1443569553805765515, -0.3690944881889765550, -0.3153832671262227771 ) ) ;
#14358 = CARTESIAN_POINT ( 'NONE',  ( 0.6102362204724415262, 0.1012011053420775880, -0.2882089793578256898 ) ) ;
#14359 = CARTESIAN_POINT ( 'NONE',  ( -0.07217847769028787330, -0.08942795157527998196, 0.3641732283464567121 ) ) ;
#14360 = CARTESIAN_POINT ( 'NONE',  ( 0.5905511811023629321, 0.2952755905511811885, 0.000000000000000000 ) ) ;
#14361 = CARTESIAN_POINT ( 'NONE',  ( -0.5577427821522301654, -0.08942795157528024563, -0.3641732283464568787 ) ) ;
#14362 = CARTESIAN_POINT ( 'NONE',  ( -0.6167979002624665030, -0.4281496062992127816, -0.4176697321401328100 ) ) ;
#14363 = CARTESIAN_POINT ( 'NONE',  ( -1.112371124080194340, -2.567464376874931580E-15, -0.4445507791589072832 ) ) ;
#14364 = ORIENTED_EDGE ( 'NONE', *, *, #2818, .T. ) ;
#14365 = CARTESIAN_POINT ( 'NONE',  ( -1.299212598425196097, 0.2952755905511811885, 0.000000000000000000 ) ) ;
#14366 = CARTESIAN_POINT ( 'NONE',  ( -1.017060367454067249, -0.2845877964562161244, -0.3641732283464567121 ) ) ;
#14367 = CARTESIAN_POINT ( 'NONE',  ( -0.05905511811023545637, -0.5400638737290845981, -0.3530559997133363437 ) ) ;
#14368 = CARTESIAN_POINT ( 'NONE',  ( -1.686351706036744558, 0.2952755905511810774, -0.1292274648535930714 ) ) ;
#14369 = CARTESIAN_POINT ( 'NONE',  ( -0.7677165354330699465, -0.5400638737290845981, -0.3530559997133363437 ) ) ;
#14370 = FACE_OUTER_BOUND ( 'NONE', #3226, .T. ) ;
#14372 = CARTESIAN_POINT ( 'NONE',  ( 0.8661417322834652488, -0.1870078740157480879, -0.4822834645669291653 ) ) ;
#14371 = CARTESIAN_POINT ( 'NONE',  ( 0.000000000000000000, 2.755905511811024056, 0.000000000000000000 ) ) ;
#14373 = CARTESIAN_POINT ( 'NONE',  ( 0.9317585301837276734, 0.05413385826771626580, -0.4176697321401330321 ) ) ;
#14374 = CARTESIAN_POINT ( 'NONE',  ( -0.3917322834645669549, -0.1049643490035306603, -2.400262467191600635 ) ) ;
#14375 = CARTESIAN_POINT ( 'NONE',  ( 1.555118110236221041, -0.5400638737290844871, 0.3530559997133364547 ) ) ;
#14376 = CARTESIAN_POINT ( 'NONE',  ( -1.207349081364828880, 0.2306618581243847221, -0.2411417322834647770 ) ) ;
#14377 = CARTESIAN_POINT ( 'NONE',  ( 0.3460692066303959202, 0.1998031496062993295, 0.02624671916010496570 ) ) ;
#14378 = VERTEX_POINT ( 'NONE', #4054 ) ;
#14379 = CARTESIAN_POINT ( 'NONE',  ( -0.4396325459317577122, -0.5511811023622048555, -0.09757992244046775898 ) ) ;
#14380 = CARTESIAN_POINT ( 'NONE',  ( 0.2867679344610365999, -0.2867679344610365444, -1.665354330708661124 ) ) ;
#14381 = ORIENTED_EDGE ( 'NONE', *, *, #14233, .F. ) ;
#14382 = CARTESIAN_POINT ( 'NONE',  ( 0.4724409448818904789, -0.1870078740157479769, 0.4822834645669291653 ) ) ;
#14383 = CARTESIAN_POINT ( 'NONE',  ( -0.1640419947506555343, -0.3162353388693405765, 0.4822834645669290543 ) ) ;
#14384 = CARTESIAN_POINT ( 'NONE',  ( -0.4986876640419939388, 0.2306618581243847221, -0.2411417322834647770 ) ) ;
#14385 = CARTESIAN_POINT ( 'NONE',  ( 1.528871391076116026, 0.2952755905511811885, 0.1292274648535926551 ) ) ;
#14386 = CARTESIAN_POINT ( 'NONE',  ( -0.9776902887139098386, 0.1771653543307087075, -0.09757992244046823083 ) ) ;
#14387 = CARTESIAN_POINT ( 'NONE',  ( -0.4359958488159628165, 1.724409448818897905, -2.630268417803939940 ) ) ;
#14388 = CARTESIAN_POINT ( 'NONE',  ( 0.9711286089238851948, -0.6046776061558809534, -0.2411417322834644161 ) ) ;
#14389 = CARTESIAN_POINT ( 'NONE',  ( 0.6102362204724416372, -0.4536011799217367080, 0.2665933059059888421 ) ) ;
#14390 = CARTESIAN_POINT ( 'NONE',  ( -0.3805774278215216522, 0.05413385826771666132, 0.4176697321401328100 ) ) ;
#14391 = CARTESIAN_POINT ( 'NONE',  ( 0.3917322834645668994, -0.1049643490035303134, -1.293943938811336958 ) ) ;
#14392 = CARTESIAN_POINT ( 'NONE',  ( -0.8267716535433065062, 0.2952755905511811885, 0.000000000000000000 ) ) ;
#14393 = DIRECTION ( 'NONE',  ( 1.000000000000000000, 0.000000000000000000, 0.000000000000000000 ) ) ;
#14394 = EDGE_CURVE ( 'NONE', #53376, #51564, #10320, .T. ) ;
#14395 = CARTESIAN_POINT ( 'NONE',  ( 1.410761154855643795, -0.05778040916215560624, -0.4822834645669293319 ) ) ;
#14396 = DIRECTION ( 'NONE',  ( 1.000000000000000000, -0.000000000000000000, -0.000000000000000000 ) ) ;
#14397 = ORIENTED_EDGE ( 'NONE', *, *, #47459, .F. ) ;
#14398 = CARTESIAN_POINT ( 'NONE',  ( 0.3917322834645670659, 2.398668435337828261E-17, -2.477053436516747364 ) ) ;
#14399 = CARTESIAN_POINT ( 'NONE',  ( -0.1049868766404193215, -0.6046776061558807314, 0.2411417322834647770 ) ) ;
#14400 = ORIENTED_EDGE ( 'NONE', *, *, #56918, .T. ) ;
#14401 = CARTESIAN_POINT ( 'NONE',  ( -1.272965879265091305, -0.4281496062992124485, 0.4176697321401328655 ) ) ;
#14402 = B_SPLINE_CURVE_WITH_KNOTS ( 'NONE', 3,
 ( #80054, #75681, #40899, #22373 ),
 .UNSPECIFIED., .F., .F.,
 ( 4, 4 ),
 ( 3.593986969204291827E-07, 0.001287825409103293597 ),
 .UNSPECIFIED. ) ;
#14403 = CARTESIAN_POINT ( 'NONE',  ( 1.476377952755906220, 0.1660481256975883668, -0.3530559997133364547 ) ) ;
#14404 = CARTESIAN_POINT ( 'NONE',  ( 1.122047244094488860, 0.1660481256975885056, 0.3530559997133364547 ) ) ;
#14405 =( BOUNDED_CURVE ( )  B_SPLINE_CURVE ( 2, ( #61553, #15294, #40955, #16955, #10633, #48911, #60311 ),
 .UNSPECIFIED., .F., .F. ) 
 B_SPLINE_CURVE_WITH_KNOTS ( ( 3, 2, 2, 3 ),
 ( 0.1477272727272727071, 0.1515151515151514916, 0.1553030303030303871, 0.1555121885203128163 ),
 .UNSPECIFIED. ) 
 CURVE ( )  GEOMETRIC_REPRESENTATION_ITEM ( )  RATIONAL_B_SPLINE_CURVE ( ( 1.000000000000000000, 0.9659258262890683122, 1.000000000000000000, 0.9659258262890683122, 1.000000000000000000, 0.9981185001348099606, 0.9964447847208435238 ) ) 
 REPRESENTATION_ITEM ( '' )  );
#14406 = CARTESIAN_POINT ( 'NONE',  ( 0.2952755905511816326, -0.5400638737290844871, 0.3530559997133364547 ) ) ;
#14407 = CARTESIAN_POINT ( 'NONE',  ( -0.3346456692913377662, 0.1660481256975883668, -0.3530559997133364547 ) ) ;
#14408 = CARTESIAN_POINT ( 'NONE',  ( -0.1049643490035307020, 0.3917322834645669549, -1.823490813648294129 ) ) ;
#14409 = CARTESIAN_POINT ( 'NONE',  ( -1.082677165354329896, 0.1660481256975885056, 0.3530559997133364547 ) ) ;
#14410 = CARTESIAN_POINT ( 'NONE',  ( -0.4068241469816264999, -0.4281496062992124485, 0.4176697321401328655 ) ) ;
#14411 = CARTESIAN_POINT ( 'NONE',  ( -0.5446194225721777693, -0.08942795157527998196, 0.3641732283464567121 ) ) ;
#14412 = LINE ( 'NONE', #20286, #53021 ) ;
#14413 = CARTESIAN_POINT ( 'NONE',  ( -0.4855643044619415427, -0.4281496062992124485, 0.4176697321401328655 ) ) ;
#14414 = DIRECTION ( 'NONE',  ( 0.000000000000000000, -1.000000000000000000, 0.000000000000000000 ) ) ;
#14415 = AXIS2_PLACEMENT_3D ( 'NONE', #36493, #24273, #49944 ) ;
#14416 = CARTESIAN_POINT ( 'NONE',  ( 0.8530183727034126306, 0.05413385826771626580, -0.4176697321401330321 ) ) ;
#14417 = CARTESIAN_POINT ( 'NONE',  ( 3.924543106786416935, 1.180793272576371677, -0.3132714499646157003 ) ) ;
#14418 = AXIS2_PLACEMENT_3D ( 'NONE', #47530, #66494, #79552 ) ;
#14419 = CARTESIAN_POINT ( 'NONE',  ( -0.2559055118110227234, -0.5400638737290844871, 0.3530559997133364547 ) ) ;
#14420 = CARTESIAN_POINT ( 'NONE',  ( -0.2952755905511804668, 0.07958543189024085140, 0.2665933059059887866 ) ) ;
#14421 = AXIS2_PLACEMENT_3D ( 'NONE', #35503, #73821, #48949 ) ;
#14423 = CARTESIAN_POINT ( 'NONE',  ( -0.9186351706036736120, 0.1539470093639523085, 0.1968503937007873850 ) ) ;
#14422 = CARTESIAN_POINT ( 'NONE',  ( 0.8792650918635177559, -0.004921259842519576551, 0.3153832671262227771 ) ) ;
#14424 = CARTESIAN_POINT ( 'NONE',  ( -0.4724409448818899238, 0.1265901696524986686, -0.7395013123359580609 ) ) ;
#14425 = CARTESIAN_POINT ( 'NONE',  ( 1.128608923884515169, -0.5023911411419708095, -0.1820866141732282451 ) ) ;
#14426 = CARTESIAN_POINT ( 'NONE',  ( 1.253280839895013710, -0.3162353388693405765, 0.4822834645669290543 ) ) ;
#14427 = CARTESIAN_POINT ( 'NONE',  ( 0.1058382717557499880, 0.3949938075777409408, -0.2276902887139107823 ) ) ;
#14428 = CARTESIAN_POINT ( 'NONE',  ( 0.1837270341207354329, 0.2306618581243848609, 0.2411417322834645549 ) ) ;
#14429 = DIRECTION ( 'NONE',  ( 1.000000000000000000, 0.000000000000000000, -1.692413147294446216E-16 ) ) ;
#14430 = CARTESIAN_POINT ( 'NONE',  ( 1.614173228346457378, 0.1771653543307087630, 0.000000000000000000 ) ) ;
#14431 = CARTESIAN_POINT ( 'NONE',  ( -0.3674540682414692561, -0.6046776061558809534, -0.2411417322834644161 ) ) ;
#14432 = CARTESIAN_POINT ( 'NONE',  ( 0.1974969037888706092, -0.3420746716998660508, 0.1463254593175853102 ) ) ;
#14433 = CARTESIAN_POINT ( 'NONE',  ( 1.574803149606299746, -0.1870078740157480879, -0.4822834645669291653 ) ) ;
#14434 = CARTESIAN_POINT ( 'NONE',  ( 0.6102362204724416372, -0.5400638737290844871, 0.3530559997133364547 ) ) ;
#14435 = CARTESIAN_POINT ( 'NONE',  ( 0.8398950131233602345, -0.5023911411419708095, 0.1820866141732285504 ) ) ;
#14436 = DIRECTION ( 'NONE',  ( -0.7071067811865463515, -2.189697074797793155E-16, -0.7071067811865486830 ) ) ;
#14437 = CARTESIAN_POINT ( 'NONE',  ( 0.2690288713910767848, 0.1771653543307087630, 0.09757992244046791164 ) ) ;
#14438 = CARTESIAN_POINT ( 'NONE',  ( -1.135170603674539924, 0.2952755905511810774, -0.1292274648535930714 ) ) ;
#14439 = CARTESIAN_POINT ( 'NONE',  ( 0.1070741851644053388, 0.3996062992125986035, -0.8576115485564304031 ) ) ;
#14440 = CARTESIAN_POINT ( 'NONE',  ( 1.305774278215223960, -0.6692913385826771977, 0.1292274648535927661 ) ) ;
#14441 = CARTESIAN_POINT ( 'NONE',  ( -0.3917322834645670104, -7.196005306013484475E-17, -0.6614173228346454936 ) ) ;
#14443 = CARTESIAN_POINT ( 'NONE',  ( 0.3503937007874015630, -0.3733313776025731778, -1.512162153811850596 ) ) ;
#14442 = CARTESIAN_POINT ( 'NONE',  ( 0.3149606299212606708, -0.1870078740157480879, -0.4822834645669291653 ) ) ;
#14444 = FACE_OUTER_BOUND ( 'NONE', #43248, .T. ) ;
#14445 = CARTESIAN_POINT ( 'NONE',  ( 0.5905511811023629321, -0.5511811023622047445, 6.969142054262312111E-17 ) ) ;
#14446 = CARTESIAN_POINT ( 'NONE',  ( 0.4593175853018380828, 0.05413385826771626580, -0.4176697321401330321 ) ) ;
#14447 = CARTESIAN_POINT ( 'NONE',  ( -0.2198823481317032369, 0.1972978822260920972, 0.1376690760605703279 ) ) ;
#14448 = CARTESIAN_POINT ( 'NONE',  ( -0.7480314960629914633, 0.1771653543307087630, 0.000000000000000000 ) ) ;
#14449 = CARTESIAN_POINT ( 'NONE',  ( -1.069553805774277722, 0.2952755905511811885, 0.1292274648535926551 ) ) ;
#14450 = CARTESIAN_POINT ( 'NONE',  ( -1.725721784776902190, -0.05778040916215522460, 0.4822834645669289988 ) ) ;
#14451 = CARTESIAN_POINT ( 'NONE',  ( 0.8333333333333340365, -0.6692913385826771977, 0.1292274648535927661 ) ) ;
#14452 = CARTESIAN_POINT ( 'NONE',  ( 1.614173228346457378, -0.6692913385826771977, 8.415575281601705876E-17 ) ) ;
#14453 = CARTESIAN_POINT ( 'NONE',  ( -0.3980111619244106058, -0.03175677952934882753, -1.220472440944883719 ) ) ;
#14454 = CARTESIAN_POINT ( 'NONE',  ( 0.6889763779527563470, 0.1660481256975883668, -0.3530559997133364547 ) ) ;
#14455 = CARTESIAN_POINT ( 'NONE',  ( -0.4724409448818895907, -0.1265901696524993070, -2.799868766404198794 ) ) ;
#14456 = CARTESIAN_POINT ( 'NONE',  ( 1.581364829396326277, -0.3162353388693409650, -0.4822834645669289433 ) ) ;
#14457 = CARTESIAN_POINT ( 'NONE',  ( 1.601049868766404982, -0.6046776061558809534, -0.2411417322834644161 ) ) ;
#14458 = CARTESIAN_POINT ( 'NONE',  ( -1.574803149606298636, -0.1870078740157479769, 0.3641732283464567677 ) ) ;
#14459 = CARTESIAN_POINT ( 'NONE',  ( 1.417322834645670104, -0.1870078740157480601, -0.3641732283464567677 ) ) ;
#14460 = CARTESIAN_POINT ( 'NONE',  ( -1.312335958005248715, 0.1283753931104748280, 0.1820866141732283561 ) ) ;
#14461 = CARTESIAN_POINT ( 'NONE',  ( -0.4593175853018364174, -0.3690944881889765550, -0.3153832671262227771 ) ) ;
#14462 = CARTESIAN_POINT ( 'NONE',  ( 0.000000000000000000, -0.04921259842519685318, -0.08523872084492505052 ) ) ;
#14463 = CARTESIAN_POINT ( 'NONE',  ( 0.3215223097112867578, -0.08942795157527998196, 0.3641732283464567121 ) ) ;
#14464 = CARTESIAN_POINT ( 'NONE',  ( 0.5249343832021005074, -0.6046776061558807314, 0.2411417322834647770 ) ) ;
#14465 = CARTESIAN_POINT ( 'NONE',  ( 0.9055118110236227702, -0.6692913385826771977, 8.415575281601705876E-17 ) ) ;
#14466 = CARTESIAN_POINT ( 'NONE',  ( -0.03280839895013062252, 0.2952755905511810774, -0.1292274648535930714 ) ) ;
#14467 = CARTESIAN_POINT ( 'NONE',  ( 0.05905511811023681640, 0.07958543189024071263, -0.2665933059059888421 ) ) ;
#14468 = CARTESIAN_POINT ( 'NONE',  ( 1.030183727034121421, -0.3162353388693409650, -0.4822834645669289433 ) ) ;
#14469 = CARTESIAN_POINT ( 'NONE',  ( -1.436417322834644850, 2.401574803149606474, 0.3149606299212598381 ) ) ;
#14470 = CARTESIAN_POINT ( 'NONE',  ( -1.148293963254592542, -0.6692913385826773087, -0.1292274648535924053 ) ) ;
#14471 = CARTESIAN_POINT ( 'NONE',  ( -0.1070741851644057135, 0.3996062992125985480, -0.6364829396325458744 ) ) ;
#14472 = CARTESIAN_POINT ( 'NONE',  ( -0.3064070226227782467, 1.250422264350145474, 0.06492945659560576954 ) ) ;
#14473 = CARTESIAN_POINT ( 'NONE',  ( 0.01312335958005323398, 0.05413385826771666132, 0.4176697321401328100 ) ) ;
#14474 = AXIS2_PLACEMENT_3D ( 'NONE', #68212, #30716, #11370 ) ;
#14475 = CARTESIAN_POINT ( 'NONE',  ( -0.8530183727034112984, 0.05413385826771666132, 0.4176697321401328100 ) ) ;
#14476 = CARTESIAN_POINT ( 'NONE',  ( -0.09186351706036689768, 0.05413385826771626580, -0.4176697321401330321 ) ) ;
#14477 = CARTESIAN_POINT ( 'NONE',  ( 0.2925321140481932369, 0.2925321140481932369, -2.657480314960630530 ) ) ;
#14478 = CARTESIAN_POINT ( 'NONE',  ( -0.3949938075777411628, 0.1058382717557497937, -1.922572178477690130 ) ) ;
#14479 = CARTESIAN_POINT ( 'NONE',  ( 4.797336870675656522E-17, -0.3917322834645670104, -0.3858267716535432879 ) ) ;
#14480 = CARTESIAN_POINT ( 'NONE',  ( 0.2867679344610366554, 0.2867679344610366554, -0.9173228346456692162 ) ) ;
#14481 = CARTESIAN_POINT ( 'NONE',  ( -0.9973753280839886548, -0.5023911411419708095, -0.1820866141732282451 ) ) ;
#14482 = CARTESIAN_POINT ( 'NONE',  ( -0.2867679344610364334, -0.2867679344610367109, -0.9960629921259842590 ) ) ;
#14483 = CARTESIAN_POINT ( 'NONE',  ( -1.528871391076114250, 0.2952755905511810774, -0.1292274648535930714 ) ) ;
#14484 = CARTESIAN_POINT ( 'NONE',  ( 0.2867679344610365999, 0.2867679344610365999, -0.06034813828640239741 ) ) ;
#14485 = CARTESIAN_POINT ( 'NONE',  ( 0.4855643044619430415, -0.4281496062992127816, -0.4176697321401328100 ) ) ;
#14486 = CARTESIAN_POINT ( 'NONE',  ( -0.6955380577427815458, -0.3690944881889765550, -0.3153832671262227771 ) ) ;
#14488 = EDGE_CURVE ( 'NONE', #38370, #39166, #63901, .T. ) ;
#14487 = CARTESIAN_POINT ( 'NONE',  ( 0.7283464566929140904, -0.5400638737290845981, -0.3530559997133363437 ) ) ;
#14489 = CARTESIAN_POINT ( 'NONE',  ( 0.4330708661417329575, -0.6692913385826771977, 8.415575281601705876E-17 ) ) ;
#14490 = CARTESIAN_POINT ( 'NONE',  ( -1.559171609364246924, 0.000000000000000000, 0.4177787735906735578 ) ) ;
#14491 = CARTESIAN_POINT ( 'NONE',  ( 4.893765752498283924E-17, -0.3996062992125986035, -2.598425196850393970 ) ) ;
#14492 = CARTESIAN_POINT ( 'NONE',  ( 0.1049643490035303967, 0.3917322834645670659, -1.092539000821209250 ) ) ;
#14493 = CARTESIAN_POINT ( 'NONE',  ( 1.246719160104987623, 0.05413385826771626580, -0.4176697321401330321 ) ) ;
#14494 = CARTESIAN_POINT ( 'NONE',  ( 0.2099737532808405305, 0.2306618581243847221, -0.2411417322834647770 ) ) ;
#14495 = CARTESIAN_POINT ( 'NONE',  ( 0.1115485564304467270, -0.6692913385826773087, -0.1292274648535924053 ) ) ;
#14496 = CARTESIAN_POINT ( 'NONE',  ( 1.561679790026247350, -0.4281496062992124485, 0.4176697321401328655 ) ) ;
#14497 = CARTESIAN_POINT ( 'NONE',  ( 0.9842519685039378130, -0.6692913385826771977, 8.415575281601705876E-17 ) ) ;
#14498 = CARTESIAN_POINT ( 'NONE',  ( -0.3917322834645669549, -0.1049643490035306603, -0.7604986876640419391 ) ) ;
#14499 = CARTESIAN_POINT ( 'NONE',  ( 0.03937007874015806264, 0.2952755905511811885, 0.000000000000000000 ) ) ;
#14500 = CARTESIAN_POINT ( 'NONE',  ( 0.5446194225721792126, -0.3162353388693405765, 0.4822834645669290543 ) ) ;
#14501 = CARTESIAN_POINT ( 'NONE',  ( -0.1968503937007867743, 0.2952755905511811885, 0.000000000000000000 ) ) ;
#14502 = CARTESIAN_POINT ( 'NONE',  ( 1.213910761154856299, 0.1771653543307087630, 0.09757992244046791164 ) ) ;
#14503 = CARTESIAN_POINT ( 'NONE',  ( -1.161417322834644716, -0.5400638737290845981, -0.3530559997133363437 ) ) ;
#14504 = CARTESIAN_POINT ( 'NONE',  ( -1.345144356955379816, -0.05778040916215560624, -0.4822834645669293319 ) ) ;
#14505 = CARTESIAN_POINT ( 'NONE',  ( 0.8333333333333340365, 0.2952755905511810774, -0.1292274648535930714 ) ) ;
#14506 = CARTESIAN_POINT ( 'NONE',  ( -0.3594585737333946263, -0.1614515132150200205, -1.929133858267715773 ) ) ;
#14507 = CARTESIAN_POINT ( 'NONE',  ( 4.797336870675656522E-17, -0.3917322834645670104, -1.960629921259842368 ) ) ;
#14508 = EDGE_LOOP ( 'NONE', ( #38270, #18187, #75997, #81159 ) ) ;
#14509 = CARTESIAN_POINT ( 'NONE',  ( 0.3996062992125986035, 2.446882876249141962E-17, -0.5905511811023621549 ) ) ;
#14510 = EDGE_LOOP ( 'NONE', ( #52032, #79912, #31299, #1158 ) ) ;
#14511 = CARTESIAN_POINT ( 'NONE',  ( 1.030183727034121421, -0.05778040916215522460, 0.4822834645669289988 ) ) ;
#14512 = CARTESIAN_POINT ( 'NONE',  ( 0.9842519685039375910, 0.1771653543307087630, 0.000000000000000000 ) ) ;
#14513 = DIRECTION ( 'NONE',  ( 0.000000000000000000, 0.000000000000000000, -1.000000000000000000 ) ) ;
#14514 = CARTESIAN_POINT ( 'NONE',  ( -0.4698793137518578189, 1.469922167998565676, 2.565145773722669720 ) ) ;
#14515 = CARTESIAN_POINT ( 'NONE',  ( 0.4724409448818898682, 2.892866454678787531E-17, -1.220472440944881942 ) ) ;
#14516 = CARTESIAN_POINT ( 'NONE',  ( 4.797336870675656522E-17, -0.3917322834645670104, -1.108267716535433101 ) ) ;
#14517 = CARTESIAN_POINT ( 'NONE',  ( 1.509186351706037543, -0.4281496062992127816, -0.4176697321401328100 ) ) ;
#14518 = CARTESIAN_POINT ( 'NONE',  ( -1.581364829396324945, -0.05778040916215560624, -0.4822834645669293319 ) ) ;
#14519 = CARTESIAN_POINT ( 'NONE',  ( -0.1443569553805768291, 0.05413385826771666132, 0.4176697321401328100 ) ) ;
#14520 = CARTESIAN_POINT ( 'NONE',  ( 0.9842519685039375910, 0.2952755905511811885, 0.000000000000000000 ) ) ;
#14521 = EDGE_LOOP ( 'NONE', ( #64583, #50377, #65608, #7823 ) ) ;
#14522 = ADVANCED_FACE ( 'NONE', ( #1789 ), #72077, .F. ) ;
#14523 = CARTESIAN_POINT ( 'NONE',  ( -1.443569553805773564, -0.6046776061558807314, 0.2411417322834647770 ) ) ;
#14524 = CARTESIAN_POINT ( 'NONE',  ( 0.5419760673063066525, 1.535433070866141447, 0.4915354330708653907 ) ) ;
#14525 = CARTESIAN_POINT ( 'NONE',  ( 3.523619145740916281, 4.103338224919997224, 8.150284903163555583 ) ) ;
#14526 = CARTESIAN_POINT ( 'NONE',  ( -1.604771003085130543, 0.7690346235818137366, -0.1466069496707740616 ) ) ;
#14527 = DIRECTION ( 'NONE',  ( 0.000000000000000000, 1.000000000000000000, 0.000000000000000000 ) ) ;
#14528 = CARTESIAN_POINT ( 'NONE',  ( -0.7349081364829387342, -0.5023911411419708095, 0.1820866141732285504 ) ) ;
#14529 =( BOUNDED_SURFACE ( )  B_SPLINE_SURFACE ( 1, 2, ( 
 ( #8611, #33862, #1471, #40590, #41422, #78913, #8196, #54033, #22481, #15771, #60364, #41010, #35108, #3125, #16180, #27959, #2711, #22062, #72996, #21234, #59943, #72170, #67517, #72583, #67106, #27125, #52789, #59526, #20821, #1883, #53200, #53618, #46890, #14931, #21646, #47306, #30851, #55688, #35942, #11514, #17425, #30441, #61612, #61186, #42239, #80987, #17832, #43466, #82218, #80580, #23300, #10691, #16594, #69163, #56106, #67934, #18239, #37170, #74252, #68351, #62850, #5186, #29208, #23712, #54874, #49383, #3954, #56515, #17014, #10275, #29616, #75078, #11095, #55277, #48970, #74670, #24537, #50202, #22888, #42654, #75899, #36346, #43880, #69578, #62021, #36753, #4357, #48555, #30025, #81396, #35524, #43056, #68753, #62428, #4766, #3541, #81811, #24122, #49791, #75493, #45963, #7264, #6426, #32512, #37991, #56927, #77137, #57756, #51434, #25773, #64926, #63667, #45545, #6008, #64503, #32095, #45120, #58174, #71243, #76315, #118, #58601, #12335, #44698, #70828, #970, #26624, #52278, #25357, #82622, #19470, #18645, #77564, #77982, #32936, #11925, #31677, #13175, #38825, #20312, #57337, #70395, #51020, #6841, #37580, #13587, #63253, #24937, #31260, #50608, #19051, #39243, #69980, #543, #5594, #83033, #26196, #76719, #12751, #51857, #19898, #44289, #38408, #64089, #40918, #28282, #9350, #27450, #41337, #53944, #65776, #21149, #14844, #53533, #8108, #33363, #59026, #3035, #15676, #59436, #72495, #22391, #21556, #40504, #52695, #2626, #78402, #59853, #80074, #33774, #79241, #35021, #60276, #2205, #47635, #46804, #66186, #46385, #8521, #60685, #20734, #78820, #79657, #21973, #15259, #73329, #71660, #72907, #66600, #1790, #47217, #67017, #72078, #28700, #34189, #34611, #8934, #14437, #40089, #53111, #54362, #27873, #14011, #39668, #65358, #7696, #1381, #27033, #29928, #74989, #62331, #73752, #17334, #16921, #54782, #48876, #42558, #61517, #3862, #10996, #4668, #68658, #4266, #61924, #67427, #30341, #9761, #36656, #68262, #55591, #23205, #81718, #48051, #24028, #56007, #16088, #67844, #10598, #36254, #41733, #10183, #74576, #80892, #81303, #35432, #49696, #61097, #22799, #80485, #16506, #23617, #75392, #35848, #49286, #3448, #42964, #29112, #48458, #74158, #42149, #29522, #55184, #15521, #33621, #9199, #79918, #60942, #79090, #9610, #22235, #34035, #72754, #66443, #21814, #59696, #1641, #27299, #54622, #67277, #27716, #40759, #74004, #73170, #8780, #20993, #54202, #46655, #28132, #48307, #2052, #47478, #3292, #28546, #53787, #15940, #15103, #34453, #14696, #60122, #28957, #72348, #47062, #47890, #73598, #66869, #41587, #39942, #41179, #34872, #53383, #60533, #35279, #40352, #80333, #2473, #2883, #22648, #66031, #8369, #21408, #65628, #79499, #7959, #59284, #52957, #78672, #70558, #51596, #38571, #50777, #78143, #76880, #20053, #7428, #64666, #18804, #14173, #13750, #77298, #12914, #45290, #33098, #19629, #7005, #58764, #282, #63829, #39407, #70986, #58339, #6167, #5755, #70141, #25517, #45706, #71402, #26777, #25104, #51182, #64252, #44449, #13330, #12493, #77724, #1127, #6586, #38156, #63418, #44859, #65090, #83195, #31842, #701, #52433, #20475, #38983, #32673, #46129, #71823, #31425, #32257, #26358, #19211, #57918, #52018, #25937, #76477, #57087, #82783, #57504, #67179, #41078, #78566, #73909, #73496, #53686, #46958, #21713, #9508, #79394, #66767, #35181, #60016, #40245, #15844, #47377, #34773, #65928, #65520, #46545, #1950, #22134, #47792, #3194, #1537, #27612, #15000, #20892, #41493, #60432, #72243, #22551, #60842, #14592, #72650, #28858, #54520, #33517, #28028, #59180, #73068, #8265, #80235, #21305, #33930, #59595, #15417, #9100, #53275, #78985, #40657, #48213, #39831, #27192, #66342, #7851, #8680, #52856, #34350, #2371, #2783, #28443, #54102, #79818, #29275, #11584, #68003, #30096, #3609, #49037, #16249, #67590, #41896, #75560, #74319, #50272, #37244, #10755, #36828, #42305, #61255, #81465, #62088, #55759, #23783, #69236, #10348, #49860, #36009, #68822, #36415, #49454, #62501, #17900, #80645, #4430, #62920, #16666, #74734, #43537, #61679 ),
 ( #4020, #75148, #30514, #22958, #81879, #17493, #4839, #43124, #48624, #29684, #55347, #56176, #81053, #23369, #5253, #24603, #24191, #11167, #17082, #30917, #56584, #82285, #9921, #35592, #54939, #42719, #68415, #32161, #25420, #51085, #77627, #13651, #51922, #45187, #19530, #37645, #39304, #63322, #45610, #57817, #70890, #12817, #32995, #75969, #64991, #7327, #58665, #6072, #5660, #184, #56992, #58239, #1030, #71303, #26683, #70045, #6491, #25837, #18310, #76379, #76782, #31746, #51496, #43951, #26261, #69647, #31327, #11991, #82689, #83100, #19959, #50681, #70460, #25008, #38056, #38474, #57408, #19114, #77200, #64158, #13240, #38889, #18713, #64568, #32576, #44354, #44763, #12399, #605, #63733, #6905, #78885, #34253, #46448, #14077, #39729, #67077, #79718, #40150, #53170, #3097, #2269, #21206, #33424, #66663, #59085, #40562, #60745, #14497, #59914, #15741, #65834, #59499, #22035, #52339, #72967, #14902, #1440, #41395, #34674, #47695, #78046, #60337, #66243, #27097, #8581, #27932, #1852, #27514, #54006, #73390, #28345, #21617, #79299, #65424, #9409, #7758, #35079, #53590, #47277, #72555, #20375, #46027, #71721, #52759, #78467, #8167, #20792, #15318, #72141, #2685, #33832, #46861, #40983, #9002, #42626, #10661, #37139, #29178, #3926, #67908, #68323, #17802, #62398, #62824, #73812, #48114, #67487, #35915, #30410, #3509, #23270, #69133, #74222, #48939, #10244, #29585, #29994, #74641, #16983, #4328, #22455, #81367, #68723, #49763, #61581, #81783, #11064, #22861, #55248, #80955, #36316, #48522, #16149, #41796, #43436, #56078, #16567, #61991, #28761, #55657, #23680, #9823, #43028, #35493, #49354, #54424, #42212, #75051, #75463, #17398, #36722, #4737, #24094, #11485, #54845, #80134, #61158, #80549, #12305, #13145, #70793, #32064, #38796, #39210, #6394, #57725, #24911, #38378, #19438, #69550, #64472, #50988, #51404, #88, #11898, #31231, #50579, #77106, #45089, #32480, #25741, #43847, #5159, #6809, #19020, #37962, #70363, #58143, #44668, #512, #26165, #25324, #5566, #51826, #12718, #77531, #56898, #30823, #37552, #76286, #19866, #45515, #71211, #50174, #18617, #63638, #63226, #13554, #56488, #82592, #82190, #24507, #44260, #5976, #75869, #18212, #69951, #76686, #31647, #64054, #57305, #83003, #46356, #39637, #20281, #53080, #40476, #65328, #1353, #7665, #53914, #34579, #52247, #27004, #21945, #40061, #8903, #28253, #33336, #66154, #58997, #26595, #8081, #77952, #60247, #52666, #78793, #45930, #14407, #64895, #32905, #7232, #40887, #78373, #15647, #2595, #59405, #2176, #20704, #71629, #46777, #27419, #21117, #72468, #79627, #72050, #15228, #65748, #34160, #1762, #14817, #27843, #66569, #13981, #8493, #47604, #33744, #59821, #53504, #79212, #21528, #73298, #47187, #72879, #58572, #937, #23587, #61069, #48021, #36225, #36627, #81271, #74547, #23176, #74960, #17306, #62304, #10154, #61894, #3420, #48431, #29494, #16475, #28672, #55980, #54753, #16060, #80043, #55153, #16892, #41707, #29083, #67399, #30312, #10968, #54333, #80459, #81691, #42122, #68628, #4641, #9734, #42531, #35405, #3005, #67817, #22362, #24002, #22768, #80864, #73721, #74130, #41303, #9321, #66989, #42933, #35820, #75360, #49670, #61485, #4235, #3834, #48846, #68233, #10567, #29899, #55563, #34991, #49258, #60656, #69454, #70265, #37868, #50894, #38278, #77007, #82094, #63543, #64373, #18115, #50482, #76594, #56396, #31967, #70689, #76186, #75774, #17708, #82499, #45012, #37459, #24408, #12620, #13042, #57628, #18924, #82908, #51305, #19340, #38695, #69859, #63955, #63132, #24815, #5876, #18523, #5064, #32379, #31133, #25642, #44990, #44573, #50078, #51724, #6710, #31550, #44166, #25229, #58043, #57207, #6292, #408, #26065, #43748, #43336, #69037, #11387, #11804, #37044, #5471, #56799, #62726, #30733, #12210, #39109, #39535, #52562, #58470, #2074, #14718, #834, #60143, #27739, #32803, #26903, #53404, #47085, #71110, #65650, #13453, #7979, #45829, #79112, #58895, #33643, #64791, #78271, #77426, #45414, #19761, #21430, #52144, #28154, #72775, #71950, #40372, #20179, #7129, #59305, #39963 ) ),
 .UNSPECIFIED., .F., .F., .F. ) 
 B_SPLINE_SURFACE_WITH_KNOTS ( ( 2, 2 ),
 ( 3, 2, 2, 2, 2, 2, 2, 2, 2, 2, 2, 2, 2, 2, 2, 2, 2, 2, 2, 2, 2, 2, 2, 2, 2, 2, 2, 2, 2, 2, 2, 2, 2, 2, 2, 2, 2, 2, 2, 2, 2, 2, 2, 2, 2, 2, 2, 2, 2, 2, 2, 2, 2, 2, 2, 2, 2, 2, 2, 2, 2, 2, 2, 2, 2, 2, 2, 2, 2, 2, 2, 2, 2, 2, 2, 2, 2, 2, 2, 2, 2, 2, 2, 2, 2, 2, 2, 2, 2, 2, 2, 2, 2, 2, 2, 2, 2, 2, 2, 2, 2, 2, 2, 2, 2, 2, 2, 2, 2, 2, 2, 2, 2, 2, 2, 2, 2, 2, 2, 2, 2, 2, 2, 2, 2, 2, 2, 2, 2, 2, 2, 2, 2, 2, 2, 2, 2, 2, 2, 2, 2, 2, 2, 2, 2, 2, 2, 2, 2, 2, 2, 2, 2, 2, 2, 2, 2, 2, 2, 2, 2, 2, 2, 2, 2, 2, 2, 2, 2, 2, 2, 2, 2, 2, 2, 2, 2, 2, 2, 2, 2, 2, 2, 2, 2, 2, 2, 2, 2, 2, 2, 2, 2, 2, 2, 2, 2, 2, 2, 2, 2, 2, 2, 2, 2, 2, 2, 2, 2, 2, 2, 2, 2, 2, 2, 2, 2, 2, 2, 2, 2, 2, 2, 2, 2, 2, 2, 2, 2, 2, 2, 2, 2, 2, 2, 2, 2, 2, 2, 2, 2, 2, 2, 2, 2, 2, 2, 2, 2, 2, 2, 2, 2, 2, 2, 3 ),
 ( 0.000000000000000000, 1.000000000000000000 ),
 ( 0.000000000000000000, 0.003787878787878787984, 0.007575757575757575968, 0.01136363636363636395, 0.01515151515151515194, 0.01893939393939393992, 0.02272727272727272790, 0.02651515151515151589, 0.03030303030303030387, 0.03409090909090908839, 0.03787878787878787984, 0.04166666666666666435, 0.04545454545454545581, 0.04924242424242424032, 0.05303030303030303177, 0.05681818181818181629, 0.06060606060606060774, 0.06439393939393939226, 0.06818181818181817677, 0.07196969696969697516, 0.07575757575757575968, 0.07954545454545454419, 0.08333333333333332871, 0.08712121212121212710, 0.09090909090909091161, 0.09469696969696969613, 0.09848484848484848064, 0.1022727272727272790, 0.1060606060606060635, 0.1098484848484848481, 0.1136363636363636326, 0.1174242424242424310, 0.1212121212121212155, 0.1250000000000000000, 0.1287878787878787845, 0.1325757575757575690, 0.1363636363636363535, 0.1401515151515151381, 0.1439393939393939503, 0.1477272727272727348, 0.1515151515151515194, 0.1553030303030303039, 0.1590909090909090884, 0.1628787878787878729, 0.1666666666666666574, 0.1704545454545454419, 0.1742424242424242542, 0.1780303030303030387, 0.1818181818181818232, 0.1856060606060606077, 0.1893939393939393923, 0.1931818181818181768, 0.1969696969696969613, 0.2007575757575757458, 0.2045454545454545581, 0.2083333333333333426, 0.2121212121212121271, 0.2159090909090909116, 0.2196969696969696961, 0.2234848484848484806, 0.2272727272727272652, 0.2310606060606060497, 0.2348484848484848619, 0.2386363636363636465, 0.2424242424242424310, 0.2462121212121212155, 0.2500000000000000000, 0.2537878787878787845, 0.2575757575757575690, 0.2613636363636363535, 0.2651515151515151381, 0.2689393939393939226, 0.2727272727272727071, 0.2765151515151514916, 0.2803030303030302761, 0.2840909090909091161, 0.2878787878787879007, 0.2916666666666666852, 0.2954545454545454697, 0.2992424242424242542, 0.3030303030303030387, 0.3068181818181818232, 0.3106060606060606077, 0.3143939393939393923, 0.3181818181818181768, 0.3219696969696969613, 0.3257575757575757458, 0.3295454545454545303, 0.3333333333333333148, 0.3371212121212120993, 0.3409090909090908839, 0.3446969696969697239, 0.3484848484848485084, 0.3522727272727272929, 0.3560606060606060774, 0.3598484848484848619, 0.3636363636363636465, 0.3674242424242424310, 0.3712121212121212155, 0.3750000000000000000, 0.3787878787878787845, 0.3825757575757575690, 0.3863636363636363535, 0.3901515151515151381, 0.3939393939393939226, 0.3977272727272727071, 0.4015151515151514916, 0.4053030303030302761, 0.4090909090909091161, 0.4128787878787879007, 0.4166666666666666852, 0.4204545454545454697, 0.4242424242424242542, 0.4280303030303030387, 0.4318181818181818232, 0.4356060606060606077, 0.4393939393939393923, 0.4431818181818181768, 0.4469696969696969613, 0.4507575757575757458, 0.4545454545454545303, 0.4583333333333333148, 0.4621212121212120993, 0.4659090909090908839, 0.4696969696969697239, 0.4734848484848485084, 0.4772727272727272929, 0.4810606060606060774, 0.4848484848484848619, 0.4886363636363636465, 0.4924242424242424310, 0.4962121212121212155, 0.5000000000000000000, 0.5037878787878787845, 0.5075757575757575690, 0.5113636363636363535, 0.5151515151515151381, 0.5189393939393939226, 0.5227272727272727071, 0.5265151515151514916, 0.5303030303030302761, 0.5340909090909090606, 0.5378787878787878451, 0.5416666666666666297, 0.5454545454545454142, 0.5492424242424241987, 0.5530303030303029832, 0.5568181818181817677, 0.5606060606060605522, 0.5643939393939394478, 0.5681818181818182323, 0.5719696969696970168, 0.5757575757575758013, 0.5795454545454545858, 0.5833333333333333703, 0.5871212121212121549, 0.5909090909090909394, 0.5946969696969697239, 0.5984848484848485084, 0.6022727272727272929, 0.6060606060606060774, 0.6098484848484848619, 0.6136363636363636465, 0.6174242424242424310, 0.6212121212121212155, 0.6250000000000000000, 0.6287878787878787845, 0.6325757575757575690, 0.6363636363636363535, 0.6401515151515151381, 0.6439393939393939226, 0.6477272727272727071, 0.6515151515151514916, 0.6553030303030302761, 0.6590909090909090606, 0.6628787878787878451, 0.6666666666666666297, 0.6704545454545454142, 0.6742424242424241987, 0.6780303030303029832, 0.6818181818181817677, 0.6856060606060605522, 0.6893939393939394478, 0.6931818181818182323, 0.6969696969696970168, 0.7007575757575758013, 0.7045454545454545858, 0.7083333333333333703, 0.7121212121212121549, 0.7159090909090909394, 0.7196969696969697239, 0.7234848484848485084, 0.7272727272727272929, 0.7310606060606060774, 0.7348484848484848619, 0.7386363636363636465, 0.7424242424242424310, 0.7462121212121212155, 0.7500000000000000000, 0.7537878787878787845, 0.7575757575757575690, 0.7613636363636363535, 0.7651515151515151381, 0.7689393939393939226, 0.7727272727272727071, 0.7765151515151514916, 0.7803030303030302761, 0.7840909090909090606, 0.7878787878787878451, 0.7916666666666666297, 0.7954545454545454142, 0.7992424242424241987, 0.8030303030303029832, 0.8068181818181817677, 0.8106060606060605522, 0.8143939393939394478, 0.8181818181818182323, 0.8219696969696970168, 0.8257575757575758013, 0.8295454545454545858, 0.8333333333333333703, 0.8371212121212121549, 0.8409090909090909394, 0.8446969696969697239, 0.8484848484848485084, 0.8522727272727272929, 0.8560606060606060774, 0.8598484848484848619, 0.8636363636363636465, 0.8674242424242424310, 0.8712121212121212155, 0.8750000000000000000, 0.8787878787878787845, 0.8825757575757575690, 0.8863636363636363535, 0.8901515151515151381, 0.8939393939393939226, 0.8977272727272727071, 0.9015151515151514916, 0.9053030303030302761, 0.9090909090909090606, 0.9128787878787878451, 0.9166666666666666297, 0.9204545454545454142, 0.9242424242424241987, 0.9280303030303029832, 0.9318181818181817677, 0.9356060606060605522, 0.9393939393939394478, 0.9431818181818182323, 0.9469696969696970168, 0.9507575757575758013, 0.9545454545454545858, 0.9583333333333333703, 0.9621212121212121549, 0.9659090909090909394 ),
 .UNSPECIFIED. ) 
 GEOMETRIC_REPRESENTATION_ITEM ( )  RATIONAL_B_SPLINE_SURFACE ( (
 ( 1.000000000000000000, 0.9659258262890683122, 1.000000000000000000, 0.9659258262890683122, 1.000000000000000000, 0.9659258262890683122, 1.000000000000000000, 0.9659258262890683122, 1.000000000000000000, 0.9659258262890683122, 1.000000000000000000, 0.9659258262890683122, 1.000000000000000000, 0.9659258262890683122, 1.000000000000000000, 0.9659258262890683122, 1.000000000000000000, 0.9659258262890683122, 1.000000000000000000, 0.9659258262890683122, 1.000000000000000000, 0.9659258262890683122, 1.000000000000000000, 0.9659258262890683122, 1.000000000000000000, 0.9659258262890683122, 1.000000000000000000, 0.9659258262890683122, 1.000000000000000000, 0.9659258262890683122, 1.000000000000000000, 0.9659258262890683122, 1.000000000000000000, 0.9659258262890683122, 1.000000000000000000, 0.9659258262890683122, 1.000000000000000000, 0.9659258262890683122, 1.000000000000000000, 0.9659258262890683122, 1.000000000000000000, 0.9659258262890683122, 1.000000000000000000, 0.9659258262890683122, 1.000000000000000000, 0.9659258262890683122, 1.000000000000000000, 0.9659258262890683122, 1.000000000000000000, 0.9659258262890683122, 1.000000000000000000, 0.9659258262890683122, 1.000000000000000000, 0.9659258262890683122, 1.000000000000000000, 0.9659258262890683122, 1.000000000000000000, 0.9659258262890683122, 1.000000000000000000, 0.9659258262890683122, 1.000000000000000000, 0.9659258262890683122, 1.000000000000000000, 0.9659258262890683122, 1.000000000000000000, 0.9659258262890683122, 1.000000000000000000, 0.9659258262890683122, 1.000000000000000000, 0.9659258262890683122, 1.000000000000000000, 0.9659258262890683122, 1.000000000000000000, 0.9659258262890683122, 1.000000000000000000, 0.9659258262890683122, 1.000000000000000000, 0.9659258262890683122, 1.000000000000000000, 0.9659258262890683122, 1.000000000000000000, 0.9659258262890683122, 1.000000000000000000, 0.9659258262890683122, 1.000000000000000000, 0.9659258262890683122, 1.000000000000000000, 0.9659258262890683122, 1.000000000000000000, 0.9659258262890683122, 1.000000000000000000, 0.9659258262890683122, 1.000000000000000000, 0.9659258262890683122, 1.000000000000000000, 0.9659258262890683122, 1.000000000000000000, 0.9659258262890683122, 1.000000000000000000, 0.9659258262890683122, 1.000000000000000000, 0.9659258262890683122, 1.000000000000000000, 0.9659258262890683122, 1.000000000000000000, 0.9659258262890683122, 1.000000000000000000, 0.9659258262890683122, 1.000000000000000000, 0.9659258262890683122, 1.000000000000000000, 0.9659258262890683122, 1.000000000000000000, 0.9659258262890683122, 1.000000000000000000, 0.9659258262890683122, 1.000000000000000000, 0.9659258262890683122, 1.000000000000000000, 0.9659258262890683122, 1.000000000000000000, 0.9659258262890683122, 1.000000000000000000, 0.9659258262890683122, 1.000000000000000000, 0.9659258262890683122, 1.000000000000000000, 0.9659258262890683122, 1.000000000000000000, 0.9659258262890683122, 1.000000000000000000, 0.9659258262890683122, 1.000000000000000000, 0.9659258262890683122, 1.000000000000000000, 0.9659258262890683122, 1.000000000000000000, 0.9659258262890683122, 1.000000000000000000, 0.9659258262890683122, 1.000000000000000000, 0.9659258262890683122, 1.000000000000000000, 0.9659258262890683122, 1.000000000000000000, 0.9659258262890683122, 1.000000000000000000, 0.9659258262890683122, 1.000000000000000000, 0.9659258262890683122, 1.000000000000000000, 0.9659258262890683122, 1.000000000000000000, 0.9659258262890683122, 1.000000000000000000, 0.9659258262890683122, 1.000000000000000000, 0.9659258262890683122, 1.000000000000000000, 0.9659258262890683122, 1.000000000000000000, 0.9659258262890683122, 1.000000000000000000, 0.9659258262890683122, 1.000000000000000000, 0.9659258262890683122, 1.000000000000000000, 0.9659258262890683122, 1.000000000000000000, 0.9659258262890683122, 1.000000000000000000, 0.9659258262890683122, 1.000000000000000000, 0.9659258262890683122, 1.000000000000000000, 0.9659258262890683122, 1.000000000000000000, 0.9659258262890683122, 1.000000000000000000, 0.9659258262890683122, 1.000000000000000000, 0.9659258262890683122, 1.000000000000000000, 0.9659258262890683122, 1.000000000000000000, 0.9659258262890683122, 1.000000000000000000, 0.9659258262890683122, 1.000000000000000000, 0.9659258262890683122, 1.000000000000000000, 0.9659258262890683122, 1.000000000000000000, 0.9659258262890683122, 1.000000000000000000, 0.9659258262890683122, 1.000000000000000000, 0.9659258262890683122, 1.000000000000000000, 0.9659258262890683122, 1.000000000000000000, 0.9659258262890683122, 1.000000000000000000, 0.9659258262890683122, 1.000000000000000000, 0.9659258262890683122, 1.000000000000000000, 0.9659258262890683122, 1.000000000000000000, 0.9659258262890683122, 1.000000000000000000, 0.9659258262890683122, 1.000000000000000000, 0.9659258262890683122, 1.000000000000000000, 0.9659258262890683122, 1.000000000000000000, 0.9659258262890683122, 1.000000000000000000, 0.9659258262890683122, 1.000000000000000000, 0.9659258262890683122, 1.000000000000000000, 0.9659258262890683122, 1.000000000000000000, 0.9659258262890683122, 1.000000000000000000, 0.9659258262890683122, 1.000000000000000000, 0.9659258262890683122, 1.000000000000000000, 0.9659258262890683122, 1.000000000000000000, 0.9659258262890683122, 1.000000000000000000, 0.9659258262890683122, 1.000000000000000000, 0.9659258262890683122, 1.000000000000000000, 0.9659258262890683122, 1.000000000000000000, 0.9659258262890683122, 1.000000000000000000, 0.9659258262890683122, 1.000000000000000000, 0.9659258262890683122, 1.000000000000000000, 0.9659258262890683122, 1.000000000000000000, 0.9659258262890683122, 1.000000000000000000, 0.9659258262890683122, 1.000000000000000000, 0.9659258262890683122, 1.000000000000000000, 0.9659258262890683122, 1.000000000000000000, 0.9659258262890683122, 1.000000000000000000, 0.9659258262890683122, 1.000000000000000000, 0.9659258262890683122, 1.000000000000000000, 0.9659258262890683122, 1.000000000000000000, 0.9659258262890683122, 1.000000000000000000, 0.9659258262890683122, 1.000000000000000000, 0.9659258262890683122, 1.000000000000000000, 0.9659258262890683122, 1.000000000000000000, 0.9659258262890683122, 1.000000000000000000, 0.9659258262890683122, 1.000000000000000000, 0.9659258262890683122, 1.000000000000000000, 0.9659258262890683122, 1.000000000000000000, 0.9659258262890683122, 1.000000000000000000, 0.9659258262890683122, 1.000000000000000000, 0.9659258262890683122, 1.000000000000000000, 0.9659258262890683122, 1.000000000000000000, 0.9659258262890683122, 1.000000000000000000, 0.9659258262890683122, 1.000000000000000000, 0.9659258262890683122, 1.000000000000000000, 0.9659258262890683122, 1.000000000000000000, 0.9659258262890683122, 1.000000000000000000, 0.9659258262890683122, 1.000000000000000000, 0.9659258262890683122, 1.000000000000000000, 0.9659258262890683122, 1.000000000000000000, 0.9659258262890683122, 1.000000000000000000, 0.9659258262890683122, 1.000000000000000000, 0.9659258262890683122, 1.000000000000000000, 0.9659258262890683122, 1.000000000000000000, 0.9659258262890683122, 1.000000000000000000, 0.9659258262890683122, 1.000000000000000000, 0.9659258262890683122, 1.000000000000000000, 0.9659258262890683122, 1.000000000000000000, 0.9659258262890683122, 1.000000000000000000, 0.9659258262890683122, 1.000000000000000000, 0.9659258262890683122, 1.000000000000000000, 0.9659258262890683122, 1.000000000000000000, 0.9659258262890683122, 1.000000000000000000, 0.9659258262890683122, 1.000000000000000000, 0.9659258262890683122, 1.000000000000000000, 0.9659258262890683122, 1.000000000000000000, 0.9659258262890683122, 1.000000000000000000, 0.9659258262890683122, 1.000000000000000000, 0.9659258262890683122, 1.000000000000000000, 0.9659258262890683122, 1.000000000000000000, 0.9659258262890683122, 1.000000000000000000, 0.9659258262890683122, 1.000000000000000000, 0.9659258262890683122, 1.000000000000000000, 0.9659258262890683122, 1.000000000000000000, 0.9659258262890683122, 1.000000000000000000, 0.9659258262890683122, 1.000000000000000000, 0.9659258262890683122, 1.000000000000000000, 0.9659258262890683122, 1.000000000000000000, 0.9659258262890683122, 1.000000000000000000, 0.9659258262890683122, 1.000000000000000000, 0.9659258262890683122, 1.000000000000000000, 0.9659258262890683122, 1.000000000000000000, 0.9659258262890683122, 1.000000000000000000, 0.9659258262890683122, 1.000000000000000000, 0.9659258262890683122, 1.000000000000000000, 0.9659258262890683122, 1.000000000000000000, 0.9659258262890683122, 1.000000000000000000, 0.9659258262890683122, 1.000000000000000000, 0.9659258262890683122, 1.000000000000000000, 0.9659258262890683122, 1.000000000000000000, 0.9659258262890683122, 1.000000000000000000, 0.9659258262890683122, 1.000000000000000000, 0.9659258262890683122, 1.000000000000000000, 0.9659258262890683122, 1.000000000000000000, 0.9659258262890683122, 1.000000000000000000, 0.9659258262890683122, 1.000000000000000000, 0.9659258262890683122, 1.000000000000000000, 0.9659258262890683122, 1.000000000000000000, 0.9659258262890683122, 1.000000000000000000, 0.9659258262890683122, 1.000000000000000000, 0.9659258262890683122, 1.000000000000000000, 0.9659258262890683122, 1.000000000000000000, 0.9659258262890683122, 1.000000000000000000, 0.9659258262890683122, 1.000000000000000000, 0.9659258262890683122, 1.000000000000000000, 0.9659258262890683122, 1.000000000000000000, 0.9659258262890683122, 1.000000000000000000, 0.9659258262890683122, 1.000000000000000000, 0.9659258262890683122, 1.000000000000000000, 0.9659258262890683122, 1.000000000000000000, 0.9659258262890683122, 1.000000000000000000, 0.9659258262890683122, 1.000000000000000000, 0.9659258262890683122, 1.000000000000000000, 0.9659258262890683122, 1.000000000000000000, 0.9659258262890683122, 1.000000000000000000, 0.9659258262890683122, 1.000000000000000000, 0.9659258262890683122, 1.000000000000000000, 0.9659258262890683122, 1.000000000000000000, 0.9659258262890683122, 1.000000000000000000, 0.9659258262890683122, 1.000000000000000000, 0.9659258262890683122, 1.000000000000000000, 0.9659258262890683122, 1.000000000000000000, 0.9659258262890683122, 1.000000000000000000, 0.9659258262890683122, 1.000000000000000000, 0.9659258262890683122, 1.000000000000000000, 0.9659258262890683122, 1.000000000000000000, 0.9659258262890683122, 1.000000000000000000, 0.9659258262890683122, 1.000000000000000000, 0.9659258262890683122, 1.000000000000000000, 0.9659258262890683122, 1.000000000000000000, 0.9659258262890683122, 1.000000000000000000, 0.9659258262890683122, 1.000000000000000000, 0.9659258262890683122, 1.000000000000000000, 0.9659258262890683122, 1.000000000000000000, 0.9659258262890683122, 1.000000000000000000, 0.9659258262890683122, 1.000000000000000000, 0.9659258262890683122, 1.000000000000000000, 0.9659258262890683122, 1.000000000000000000, 0.9659258262890683122, 1.000000000000000000, 0.9659258262890683122, 1.000000000000000000, 0.9659258262890683122, 1.000000000000000000, 0.9659258262890683122, 1.000000000000000000, 0.9659258262890683122, 1.000000000000000000, 0.9659258262890683122, 1.000000000000000000, 0.9659258262890683122, 1.000000000000000000, 0.9659258262890683122, 1.000000000000000000, 0.9659258262890683122, 1.000000000000000000, 0.9659258262890683122, 1.000000000000000000, 0.9659258262890683122, 1.000000000000000000, 0.9659258262890683122, 1.000000000000000000, 0.9659258262890683122, 1.000000000000000000, 0.9659258262890683122, 1.000000000000000000, 0.9659258262890683122, 1.000000000000000000),
 ( 1.000000000000000000, 0.9659258262890683122, 1.000000000000000000, 0.9659258262890683122, 1.000000000000000000, 0.9659258262890683122, 1.000000000000000000, 0.9659258262890683122, 1.000000000000000000, 0.9659258262890683122, 1.000000000000000000, 0.9659258262890683122, 1.000000000000000000, 0.9659258262890683122, 1.000000000000000000, 0.9659258262890683122, 1.000000000000000000, 0.9659258262890683122, 1.000000000000000000, 0.9659258262890683122, 1.000000000000000000, 0.9659258262890683122, 1.000000000000000000, 0.9659258262890683122, 1.000000000000000000, 0.9659258262890683122, 1.000000000000000000, 0.9659258262890683122, 1.000000000000000000, 0.9659258262890683122, 1.000000000000000000, 0.9659258262890683122, 1.000000000000000000, 0.9659258262890683122, 1.000000000000000000, 0.9659258262890683122, 1.000000000000000000, 0.9659258262890683122, 1.000000000000000000, 0.9659258262890683122, 1.000000000000000000, 0.9659258262890683122, 1.000000000000000000, 0.9659258262890683122, 1.000000000000000000, 0.9659258262890683122, 1.000000000000000000, 0.9659258262890683122, 1.000000000000000000, 0.9659258262890683122, 1.000000000000000000, 0.9659258262890683122, 1.000000000000000000, 0.9659258262890683122, 1.000000000000000000, 0.9659258262890683122, 1.000000000000000000, 0.9659258262890683122, 1.000000000000000000, 0.9659258262890683122, 1.000000000000000000, 0.9659258262890683122, 1.000000000000000000, 0.9659258262890683122, 1.000000000000000000, 0.9659258262890683122, 1.000000000000000000, 0.9659258262890683122, 1.000000000000000000, 0.9659258262890683122, 1.000000000000000000, 0.9659258262890683122, 1.000000000000000000, 0.9659258262890683122, 1.000000000000000000, 0.9659258262890683122, 1.000000000000000000, 0.9659258262890683122, 1.000000000000000000, 0.9659258262890683122, 1.000000000000000000, 0.9659258262890683122, 1.000000000000000000, 0.9659258262890683122, 1.000000000000000000, 0.9659258262890683122, 1.000000000000000000, 0.9659258262890683122, 1.000000000000000000, 0.9659258262890683122, 1.000000000000000000, 0.9659258262890683122, 1.000000000000000000, 0.9659258262890683122, 1.000000000000000000, 0.9659258262890683122, 1.000000000000000000, 0.9659258262890683122, 1.000000000000000000, 0.9659258262890683122, 1.000000000000000000, 0.9659258262890683122, 1.000000000000000000, 0.9659258262890683122, 1.000000000000000000, 0.9659258262890683122, 1.000000000000000000, 0.9659258262890683122, 1.000000000000000000, 0.9659258262890683122, 1.000000000000000000, 0.9659258262890683122, 1.000000000000000000, 0.9659258262890683122, 1.000000000000000000, 0.9659258262890683122, 1.000000000000000000, 0.9659258262890683122, 1.000000000000000000, 0.9659258262890683122, 1.000000000000000000, 0.9659258262890683122, 1.000000000000000000, 0.9659258262890683122, 1.000000000000000000, 0.9659258262890683122, 1.000000000000000000, 0.9659258262890683122, 1.000000000000000000, 0.9659258262890683122, 1.000000000000000000, 0.9659258262890683122, 1.000000000000000000, 0.9659258262890683122, 1.000000000000000000, 0.9659258262890683122, 1.000000000000000000, 0.9659258262890683122, 1.000000000000000000, 0.9659258262890683122, 1.000000000000000000, 0.9659258262890683122, 1.000000000000000000, 0.9659258262890683122, 1.000000000000000000, 0.9659258262890683122, 1.000000000000000000, 0.9659258262890683122, 1.000000000000000000, 0.9659258262890683122, 1.000000000000000000, 0.9659258262890683122, 1.000000000000000000, 0.9659258262890683122, 1.000000000000000000, 0.9659258262890683122, 1.000000000000000000, 0.9659258262890683122, 1.000000000000000000, 0.9659258262890683122, 1.000000000000000000, 0.9659258262890683122, 1.000000000000000000, 0.9659258262890683122, 1.000000000000000000, 0.9659258262890683122, 1.000000000000000000, 0.9659258262890683122, 1.000000000000000000, 0.9659258262890683122, 1.000000000000000000, 0.9659258262890683122, 1.000000000000000000, 0.9659258262890683122, 1.000000000000000000, 0.9659258262890683122, 1.000000000000000000, 0.9659258262890683122, 1.000000000000000000, 0.9659258262890683122, 1.000000000000000000, 0.9659258262890683122, 1.000000000000000000, 0.9659258262890683122, 1.000000000000000000, 0.9659258262890683122, 1.000000000000000000, 0.9659258262890683122, 1.000000000000000000, 0.9659258262890683122, 1.000000000000000000, 0.9659258262890683122, 1.000000000000000000, 0.9659258262890683122, 1.000000000000000000, 0.9659258262890683122, 1.000000000000000000, 0.9659258262890683122, 1.000000000000000000, 0.9659258262890683122, 1.000000000000000000, 0.9659258262890683122, 1.000000000000000000, 0.9659258262890683122, 1.000000000000000000, 0.9659258262890683122, 1.000000000000000000, 0.9659258262890683122, 1.000000000000000000, 0.9659258262890683122, 1.000000000000000000, 0.9659258262890683122, 1.000000000000000000, 0.9659258262890683122, 1.000000000000000000, 0.9659258262890683122, 1.000000000000000000, 0.9659258262890683122, 1.000000000000000000, 0.9659258262890683122, 1.000000000000000000, 0.9659258262890683122, 1.000000000000000000, 0.9659258262890683122, 1.000000000000000000, 0.9659258262890683122, 1.000000000000000000, 0.9659258262890683122, 1.000000000000000000, 0.9659258262890683122, 1.000000000000000000, 0.9659258262890683122, 1.000000000000000000, 0.9659258262890683122, 1.000000000000000000, 0.9659258262890683122, 1.000000000000000000, 0.9659258262890683122, 1.000000000000000000, 0.9659258262890683122, 1.000000000000000000, 0.9659258262890683122, 1.000000000000000000, 0.9659258262890683122, 1.000000000000000000, 0.9659258262890683122, 1.000000000000000000, 0.9659258262890683122, 1.000000000000000000, 0.9659258262890683122, 1.000000000000000000, 0.9659258262890683122, 1.000000000000000000, 0.9659258262890683122, 1.000000000000000000, 0.9659258262890683122, 1.000000000000000000, 0.9659258262890683122, 1.000000000000000000, 0.9659258262890683122, 1.000000000000000000, 0.9659258262890683122, 1.000000000000000000, 0.9659258262890683122, 1.000000000000000000, 0.9659258262890683122, 1.000000000000000000, 0.9659258262890683122, 1.000000000000000000, 0.9659258262890683122, 1.000000000000000000, 0.9659258262890683122, 1.000000000000000000, 0.9659258262890683122, 1.000000000000000000, 0.9659258262890683122, 1.000000000000000000, 0.9659258262890683122, 1.000000000000000000, 0.9659258262890683122, 1.000000000000000000, 0.9659258262890683122, 1.000000000000000000, 0.9659258262890683122, 1.000000000000000000, 0.9659258262890683122, 1.000000000000000000, 0.9659258262890683122, 1.000000000000000000, 0.9659258262890683122, 1.000000000000000000, 0.9659258262890683122, 1.000000000000000000, 0.9659258262890683122, 1.000000000000000000, 0.9659258262890683122, 1.000000000000000000, 0.9659258262890683122, 1.000000000000000000, 0.9659258262890683122, 1.000000000000000000, 0.9659258262890683122, 1.000000000000000000, 0.9659258262890683122, 1.000000000000000000, 0.9659258262890683122, 1.000000000000000000, 0.9659258262890683122, 1.000000000000000000, 0.9659258262890683122, 1.000000000000000000, 0.9659258262890683122, 1.000000000000000000, 0.9659258262890683122, 1.000000000000000000, 0.9659258262890683122, 1.000000000000000000, 0.9659258262890683122, 1.000000000000000000, 0.9659258262890683122, 1.000000000000000000, 0.9659258262890683122, 1.000000000000000000, 0.9659258262890683122, 1.000000000000000000, 0.9659258262890683122, 1.000000000000000000, 0.9659258262890683122, 1.000000000000000000, 0.9659258262890683122, 1.000000000000000000, 0.9659258262890683122, 1.000000000000000000, 0.9659258262890683122, 1.000000000000000000, 0.9659258262890683122, 1.000000000000000000, 0.9659258262890683122, 1.000000000000000000, 0.9659258262890683122, 1.000000000000000000, 0.9659258262890683122, 1.000000000000000000, 0.9659258262890683122, 1.000000000000000000, 0.9659258262890683122, 1.000000000000000000, 0.9659258262890683122, 1.000000000000000000, 0.9659258262890683122, 1.000000000000000000, 0.9659258262890683122, 1.000000000000000000, 0.9659258262890683122, 1.000000000000000000, 0.9659258262890683122, 1.000000000000000000, 0.9659258262890683122, 1.000000000000000000, 0.9659258262890683122, 1.000000000000000000, 0.9659258262890683122, 1.000000000000000000, 0.9659258262890683122, 1.000000000000000000, 0.9659258262890683122, 1.000000000000000000, 0.9659258262890683122, 1.000000000000000000, 0.9659258262890683122, 1.000000000000000000, 0.9659258262890683122, 1.000000000000000000, 0.9659258262890683122, 1.000000000000000000, 0.9659258262890683122, 1.000000000000000000, 0.9659258262890683122, 1.000000000000000000, 0.9659258262890683122, 1.000000000000000000, 0.9659258262890683122, 1.000000000000000000, 0.9659258262890683122, 1.000000000000000000, 0.9659258262890683122, 1.000000000000000000, 0.9659258262890683122, 1.000000000000000000, 0.9659258262890683122, 1.000000000000000000, 0.9659258262890683122, 1.000000000000000000, 0.9659258262890683122, 1.000000000000000000, 0.9659258262890683122, 1.000000000000000000, 0.9659258262890683122, 1.000000000000000000, 0.9659258262890683122, 1.000000000000000000, 0.9659258262890683122, 1.000000000000000000, 0.9659258262890683122, 1.000000000000000000, 0.9659258262890683122, 1.000000000000000000, 0.9659258262890683122, 1.000000000000000000, 0.9659258262890683122, 1.000000000000000000, 0.9659258262890683122, 1.000000000000000000, 0.9659258262890683122, 1.000000000000000000, 0.9659258262890683122, 1.000000000000000000, 0.9659258262890683122, 1.000000000000000000, 0.9659258262890683122, 1.000000000000000000, 0.9659258262890683122, 1.000000000000000000, 0.9659258262890683122, 1.000000000000000000, 0.9659258262890683122, 1.000000000000000000, 0.9659258262890683122, 1.000000000000000000, 0.9659258262890683122, 1.000000000000000000, 0.9659258262890683122, 1.000000000000000000, 0.9659258262890683122, 1.000000000000000000, 0.9659258262890683122, 1.000000000000000000, 0.9659258262890683122, 1.000000000000000000, 0.9659258262890683122, 1.000000000000000000, 0.9659258262890683122, 1.000000000000000000, 0.9659258262890683122, 1.000000000000000000, 0.9659258262890683122, 1.000000000000000000, 0.9659258262890683122, 1.000000000000000000, 0.9659258262890683122, 1.000000000000000000, 0.9659258262890683122, 1.000000000000000000, 0.9659258262890683122, 1.000000000000000000, 0.9659258262890683122, 1.000000000000000000, 0.9659258262890683122, 1.000000000000000000, 0.9659258262890683122, 1.000000000000000000, 0.9659258262890683122, 1.000000000000000000, 0.9659258262890683122, 1.000000000000000000, 0.9659258262890683122, 1.000000000000000000, 0.9659258262890683122, 1.000000000000000000, 0.9659258262890683122, 1.000000000000000000, 0.9659258262890683122, 1.000000000000000000, 0.9659258262890683122, 1.000000000000000000, 0.9659258262890683122, 1.000000000000000000, 0.9659258262890683122, 1.000000000000000000, 0.9659258262890683122, 1.000000000000000000, 0.9659258262890683122, 1.000000000000000000, 0.9659258262890683122, 1.000000000000000000, 0.9659258262890683122, 1.000000000000000000, 0.9659258262890683122, 1.000000000000000000, 0.9659258262890683122, 1.000000000000000000, 0.9659258262890683122, 1.000000000000000000, 0.9659258262890683122, 1.000000000000000000, 0.9659258262890683122, 1.000000000000000000, 0.9659258262890683122, 1.000000000000000000, 0.9659258262890683122, 1.000000000000000000, 0.9659258262890683122, 1.000000000000000000, 0.9659258262890683122, 1.000000000000000000, 0.9659258262890683122, 1.000000000000000000, 0.9659258262890683122, 1.000000000000000000, 0.9659258262890683122, 1.000000000000000000) ) ) 
 REPRESENTATION_ITEM ( '' )  SURFACE ( )  );
#14530 = CARTESIAN_POINT ( 'NONE',  ( -1.469816272965878357, 0.2306618581243848609, 0.2411417322834645549 ) ) ;
#14531 = CARTESIAN_POINT ( 'NONE',  ( 0.3937007874015754361, -0.1870078740157479769, 0.4822834645669291653 ) ) ;
#14532 = AXIS2_PLACEMENT_3D ( 'NONE', #58094, #47138, #53031 ) ;
#14533 = ORIENTED_EDGE ( 'NONE', *, *, #23671, .F. ) ;
#14535 = DIRECTION ( 'NONE',  ( 0.000000000000000000, 0.000000000000000000, 1.000000000000000000 ) ) ;
#14534 = CARTESIAN_POINT ( 'NONE',  ( -1.614173228346457378, 0.5038684218300931716, 0.1372047244094476981 ) ) ;
#14536 = CARTESIAN_POINT ( 'NONE',  ( 0.6627296587926517768, -0.6692913385826773087, -0.1292274648535924053 ) ) ;
#14537 = CARTESIAN_POINT ( 'NONE',  ( -1.502624671916009680, -0.05778040916215560624, -0.4822834645669293319 ) ) ;
#14538 = CARTESIAN_POINT ( 'NONE',  ( -0.3392501089628018329, -0.1958661417322836440, -1.234888820701100398 ) ) ;
#14539 = CARTESIAN_POINT ( 'NONE',  ( -0.9120734908136475250, 0.1771653543307087630, 0.09757992244046791164 ) ) ;
#14540 = CARTESIAN_POINT ( 'NONE',  ( 1.620734908136483465, -0.6692913385826771977, 0.1292274648535927661 ) ) ;
#14541 = CARTESIAN_POINT ( 'NONE',  ( -0.4724409448818898682, -8.678599364036362592E-17, -0.8267716535433070613 ) ) ;
#14542 = CARTESIAN_POINT ( 'NONE',  ( 0.3871391076115492380, -0.05778040916215560624, -0.4822834645669293319 ) ) ;
#14543 = CARTESIAN_POINT ( 'NONE',  ( -0.8333333333333323711, 0.1771653543307087630, 0.09757992244046791164 ) ) ;
#14544 = CARTESIAN_POINT ( 'NONE',  ( -0.3215223097112853146, -0.2845877964562159024, 0.3641732283464567677 ) ) ;
#14545 = CARTESIAN_POINT ( 'NONE',  ( -0.1640419947506555343, -0.3162353388693405765, 0.4822834645669290543 ) ) ;
#14546 = CARTESIAN_POINT ( 'NONE',  ( -1.259842519685038686, -0.1870078740157480601, -0.3641732283464567677 ) ) ;
#14547 = CARTESIAN_POINT ( 'NONE',  ( -0.3392501089628017219, -0.1958661417322836995, 0.1082484007535938902 ) ) ;
#14548 = CARTESIAN_POINT ( 'NONE',  ( 0.9251968503937015864, -0.5400638737290844871, 0.3530559997133364547 ) ) ;
#14549 = EDGE_CURVE ( 'NONE', #39843, #58335, #44637, .T. ) ;
#14550 = CARTESIAN_POINT ( 'NONE',  ( 2.530077748780002800, 2.729661042438510155, 0.5314960629921260393 ) ) ;
#14551 = CARTESIAN_POINT ( 'NONE',  ( -0.2362204724409447953, -0.4091458600556404646, -1.717191601049868677 ) ) ;
#14552 = CARTESIAN_POINT ( 'NONE',  ( -0.6627296587926503335, -0.6692913385826771977, 0.1292274648535927661 ) ) ;
#14553 = CARTESIAN_POINT ( 'NONE',  ( -0.006561679790025524116, -0.2845877964562159024, 0.3641732283464567677 ) ) ;
#14554 = CARTESIAN_POINT ( 'NONE',  ( -1.318897637795274802, 0.1660481256975885056, 0.3530559997133364547 ) ) ;
#14555 = CARTESIAN_POINT ( 'NONE',  ( 0.6955380577427828781, -0.3690944881889763329, 0.3153832671262228327 ) ) ;
#14556 = CARTESIAN_POINT ( 'NONE',  ( -0.6299212598425188991, -0.1870078740157479769, 0.3641732283464567677 ) ) ;
#14557 = CARTESIAN_POINT ( 'NONE',  ( -0.8595800524934373854, -0.3162353388693409650, -0.4822834645669289433 ) ) ;
#14558 = CARTESIAN_POINT ( 'NONE',  ( -1.200787401574802349, 0.1660481256975883668, -0.3530559997133364547 ) ) ;
#14559 = CARTESIAN_POINT ( 'NONE',  ( 1.620734908136483465, -0.6692913385826771977, 0.1292274648535927661 ) ) ;
#14560 = DIRECTION ( 'NONE',  ( 0.000000000000000000, 0.4999999999999997224, 0.8660254037844388186 ) ) ;
#14561 = CARTESIAN_POINT ( 'NONE',  ( 1.043307086614173818, 0.07958543189024085140, 0.2665933059059887866 ) ) ;
#14562 = CARTESIAN_POINT ( 'NONE',  ( 0.3608923884514443348, -0.6692913385826771977, 0.1292274648535927661 ) ) ;
#14563 = FACE_OUTER_BOUND ( 'NONE', #79729, .T. ) ;
#14564 = CARTESIAN_POINT ( 'NONE',  ( -1.351706036745406347, 0.05413385826771626580, -0.4176697321401330321 ) ) ;
#14565 = ORIENTED_EDGE ( 'NONE', *, *, #11099, .F. ) ;
#14566 = CARTESIAN_POINT ( 'NONE',  ( 0.3996062992125986035, -0.1070741851644052972, -2.708005249343832688 ) ) ;
#14567 = CARTESIAN_POINT ( 'NONE',  ( -1.312335958005248715, 0.1283753931104748280, 0.1820866141732283561 ) ) ;
#14568 = CARTESIAN_POINT ( 'NONE',  ( -0.6692913385826764205, 0.2952755905511811885, 0.000000000000000000 ) ) ;
#14569 = CARTESIAN_POINT ( 'NONE',  ( 0.7480314960629927956, -0.6692913385826771977, 8.415575281601705876E-17 ) ) ;
#14570 = CARTESIAN_POINT ( 'NONE',  ( -1.437007874015747477, -0.4536011799217367080, 0.2665933059059888421 ) ) ;
#14571 = CARTESIAN_POINT ( 'NONE',  ( -0.1998031496062994405, 0.3460692066303957537, -1.664698162729658870 ) ) ;
#14572 = CARTESIAN_POINT ( 'NONE',  ( -1.607611548556429737, -0.6692913385826771977, 0.1292274648535927661 ) ) ;
#14573 = CARTESIAN_POINT ( 'NONE',  ( 0.6496062992125991586, -0.5400638737290845981, -0.3530559997133363437 ) ) ;
#14574 = CARTESIAN_POINT ( 'NONE',  ( 0.5774278215223104249, 0.2306618581243848609, 0.2411417322834645549 ) ) ;
#14575 = CARTESIAN_POINT ( 'NONE',  ( 1.102362204724410155, -0.1870078740157479769, 0.4822834645669291653 ) ) ;
#14576 = CARTESIAN_POINT ( 'NONE',  ( 0.2755905511811031494, 3.375010863791927619E-17, 6.062992125984251857 ) ) ;
#14577 = CARTESIAN_POINT ( 'NONE',  ( -0.1998031496062994683, 0.3460692066303958092, -1.272965879265091749 ) ) ;
#14578 = CARTESIAN_POINT ( 'NONE',  ( 4.837279021331060870E-17, -0.3949938075777409963, -0.8661417322834645827 ) ) ;
#14579 = CARTESIAN_POINT ( 'NONE',  ( 0.1902887139107617975, 0.1771653543307087630, 0.09757992244046791164 ) ) ;
#14580 = CARTESIAN_POINT ( 'NONE',  ( -0.3608923884514428360, -0.6692913385826773087, -0.1292274648535924053 ) ) ;
#14581 = CARTESIAN_POINT ( 'NONE',  ( 1.377952755905512472, -0.6692913385826771977, 8.415575281601705876E-17 ) ) ;
#14582 = CARTESIAN_POINT ( 'NONE',  ( 4.837279021331061486E-17, -0.3949938075777409963, -1.887795275590550936 ) ) ;
#14583 = CARTESIAN_POINT ( 'NONE',  ( 0.4330708661417329575, 0.1771653543307087630, 0.000000000000000000 ) ) ;
#14584 = CARTESIAN_POINT ( 'NONE',  ( -0.6167979002624665030, -0.4281496062992127816, -0.4176697321401328100 ) ) ;
#14585 = CARTESIAN_POINT ( 'NONE',  ( 1.476377952755906220, 0.1660481256975883668, -0.3530559997133364547 ) ) ;
#14586 = CARTESIAN_POINT ( 'NONE',  ( 0.4265091863517067594, 0.2952755905511811885, 0.1292274648535926551 ) ) ;
#14587 = CARTESIAN_POINT ( 'NONE',  ( -1.157146581871515012E-16, 0.4724409448818898682, -1.889763779527559251 ) ) ;
#14588 = CARTESIAN_POINT ( 'NONE',  ( 0.3436793299028388926, -0.1882840440723189401, -2.755905511811023612 ) ) ;
#14589 = ORIENTED_EDGE ( 'NONE', *, *, #11153, .F. ) ;
#14590 = ORIENTED_EDGE ( 'NONE', *, *, #54812, .T. ) ;
#14591 = CARTESIAN_POINT ( 'NONE',  ( 1.456692913385827515, 0.1771653543307087630, 0.000000000000000000 ) ) ;
#14593 = CARTESIAN_POINT ( 'NONE',  ( -0.9842519685039360366, 0.2952755905511811885, 0.000000000000000000 ) ) ;
#14592 = CARTESIAN_POINT ( 'NONE',  ( -1.213910761154854745, -0.5511811023622046335, 0.09757992244046803654 ) ) ;
#14594 = CARTESIAN_POINT ( 'NONE',  ( 0.1049643490035303689, 0.3917322834645668994, -2.435676222275903857 ) ) ;
#14595 = CARTESIAN_POINT ( 'NONE',  ( 0.3996062992125985480, 2.446882876249141654E-17, -2.872047244094488416 ) ) ;
#14596 = CARTESIAN_POINT ( 'NONE',  ( -1.653543307086613234, -0.1870078740157479769, 0.3641732283464567677 ) ) ;
#14597 = CARTESIAN_POINT ( 'NONE',  ( -1.358267716535432434, 0.1660481256975883668, -0.3530559997133364547 ) ) ;
#14598 = CARTESIAN_POINT ( 'NONE',  ( -0.07874015748031421014, -0.1870078740157480879, -0.4822834645669291653 ) ) ;
#14599 = CARTESIAN_POINT ( 'NONE',  ( -1.371391076115484609, -0.6692913385826771977, 0.1292274648535927661 ) ) ;
#14600 = CARTESIAN_POINT ( 'NONE',  ( 0.2867679344610365999, -0.2867679344610365444, 0.1318897637795274913 ) ) ;
#14601 = CARTESIAN_POINT ( 'NONE',  ( 0.7414698162729663755, -0.6692913385826773087, -0.1292274648535924053 ) ) ;
#14602 = CARTESIAN_POINT ( 'NONE',  ( 4.797336870675656522E-17, -0.3917322834645670104, -1.803149606299212726 ) ) ;
#14603 = CARTESIAN_POINT ( 'NONE',  ( -1.220472440944881054, -0.5511811023622047445, 6.969142054262312111E-17 ) ) ;
#14604 = ORIENTED_EDGE ( 'NONE', *, *, #5896, .F. ) ;
#14605 = CARTESIAN_POINT ( 'NONE',  ( -0.1974969037888706647, 0.3420746716998658843, -2.217847769028871596 ) ) ;
#14606 = ORIENTED_EDGE ( 'NONE', *, *, #37682, .T. ) ;
#14607 = DIRECTION ( 'NONE',  ( -0.000000000000000000, -1.000000000000000000, -0.000000000000000000 ) ) ;
#14608 = CARTESIAN_POINT ( 'NONE',  ( -1.338582677165353729, -0.1870078740157480879, -0.4822834645669291653 ) ) ;
#14609 = CARTESIAN_POINT ( 'NONE',  ( -1.437007874015747477, 0.1660481256975883668, -0.3530559997133364547 ) ) ;
#14610 = CARTESIAN_POINT ( 'NONE',  ( 0.2925321140481932369, 0.2925321140481932369, -0.7677165354330709457 ) ) ;
#14611 = CARTESIAN_POINT ( 'NONE',  ( -1.646981627296586703, -0.3162353388693409650, -0.4822834645669289433 ) ) ;
#14612 = CARTESIAN_POINT ( 'NONE',  ( -1.732283464566928277, -0.1870078740157479769, 0.4822834645669291653 ) ) ;
#14613 = CARTESIAN_POINT ( 'NONE',  ( -1.482939632545930975, 0.05413385826771666132, 0.4176697321401328100 ) ) ;
#14614 = CARTESIAN_POINT ( 'NONE',  ( -0.6199123404867337150, -2.191421614605370878E-15, 0.4445507791589071167 ) ) ;
#14615 = CARTESIAN_POINT ( 'NONE',  ( 3.833048052449394218E-17, 2.145669291338582418, 0.3129921259842520787 ) ) ;
#14616 = CARTESIAN_POINT ( 'NONE',  ( 0.04593175853018440641, -0.5511811023622046335, 0.09757992244046803654 ) ) ;
#14617 = CARTESIAN_POINT ( 'NONE',  ( -0.1958661417322836718, 0.3392501089628017219, -0.2552493438320210806 ) ) ;
#14618 = CARTESIAN_POINT ( 'NONE',  ( -0.5971128608923877978, 0.1771653543307087630, 0.09757992244046791164 ) ) ;
#14619 = CARTESIAN_POINT ( 'NONE',  ( -1.010498687664041384, 0.05413385826771666132, 0.4176697321401328100 ) ) ;
#14620 = CARTESIAN_POINT ( 'NONE',  ( 0.7349081364829402885, -0.6046776061558809534, -0.2411417322834644161 ) ) ;
#14621 = CARTESIAN_POINT ( 'NONE',  ( -0.8923884514435688198, -0.6046776061558807314, 0.2411417322834647770 ) ) ;
#14622 = CARTESIAN_POINT ( 'NONE',  ( -0.3392501089628017219, -0.1958661417322836718, 0.1128608923884514836 ) ) ;
#14623 = EDGE_LOOP ( 'NONE', ( #41172, #35927, #24633, #61887 ) ) ;
#14624 = CARTESIAN_POINT ( 'NONE',  ( -0.8661417322834640276, -0.1870078740157479769, 0.4822834645669291653 ) ) ;
#14625 = CARTESIAN_POINT ( 'NONE',  ( 1.003937007874016185, 0.1660481256975883668, -0.3530559997133364547 ) ) ;
#14626 = CARTESIAN_POINT ( 'NONE',  ( -1.646981627296586703, -0.2845877964562161244, -0.3641732283464567121 ) ) ;
#14627 = CARTESIAN_POINT ( 'NONE',  ( -1.692913385826770645, 0.2952755905511811885, 0.000000000000000000 ) ) ;
#14628 = CARTESIAN_POINT ( 'NONE',  ( 0.1265901696524990294, -0.4724409448818896462, -1.345144356955380704 ) ) ;
#14629 = CARTESIAN_POINT ( 'NONE',  ( 2.159244633716622008, 1.469861850861822639, -0.4698711669589714646 ) ) ;
#14630 = CARTESIAN_POINT ( 'NONE',  ( 0.3917322834645669549, 0.1049643490035304660, -0.1167979002624671414 ) ) ;
#14631 = CARTESIAN_POINT ( 'NONE',  ( 0.1049643490035303689, 0.3917322834645670104, -2.440288713910760521 ) ) ;
#14632 = CARTESIAN_POINT ( 'NONE',  ( -0.2952755905511803003, -0.5400638737290845981, -0.3530559997133363437 ) ) ;
#14633 = CARTESIAN_POINT ( 'NONE',  ( -1.423884514435694859, -0.08942795157528024563, -0.3641732283464568787 ) ) ;
#14634 = CARTESIAN_POINT ( 'NONE',  ( -0.1998031496062991630, -0.3460692066303959202, 0.01509186351706034469 ) ) ;
#14636 = CARTESIAN_POINT ( 'NONE',  ( -0.6758530183727027296, 0.2066929133858267931, 0.1054918080437490802 ) ) ;
#14635 = CARTESIAN_POINT ( 'NONE',  ( -1.141732283464566011, -0.6692913385826771977, 8.415575281601705876E-17 ) ) ;
#14637 = CARTESIAN_POINT ( 'NONE',  ( -1.509186351706035767, 0.05413385826771626580, -0.4176697321401330321 ) ) ;
#14638 = CARTESIAN_POINT ( 'NONE',  ( -0.5511811023622041894, -0.1870078740157480879, -0.4822834645669291653 ) ) ;
#14639 = CARTESIAN_POINT ( 'NONE',  ( -0.3949938075777408852, -0.1058382717557502933, -2.799868766404199683 ) ) ;
#14640 = CARTESIAN_POINT ( 'NONE',  ( 0.4593175853018379162, -0.3690944881889763329, 0.3153832671262228327 ) ) ;
#14641 = CARTESIAN_POINT ( 'NONE',  ( -0.1958661417322836718, 0.3392501089628017219, -0.09776902887139117537 ) ) ;
#14642 = CARTESIAN_POINT ( 'NONE',  ( 0.3083989501312343062, -0.08942795157528024563, -0.3641732283464568787 ) ) ;
#14643 = CARTESIAN_POINT ( 'NONE',  ( 1.450131233595801428, 0.1771653543307087630, 0.09757992244046791164 ) ) ;
#14644 = CARTESIAN_POINT ( 'NONE',  ( 1.069553805774278610, -0.6692913385826771977, 0.1292274648535927661 ) ) ;
#14645 = CARTESIAN_POINT ( 'NONE',  ( -0.02624671916010428221, 0.1283753931104746893, -0.1820866141732285504 ) ) ;
#14646 = CARTESIAN_POINT ( 'NONE',  ( 0.1958661417322836440, -0.3392501089628017219, -1.816272965879265122 ) ) ;
#14647 = CARTESIAN_POINT ( 'NONE',  ( -1.108923884514435132, -0.05778040916215560624, -0.4822834645669293319 ) ) ;
#14648 = CARTESIAN_POINT ( 'NONE',  ( -0.09842519685039295696, 0.07958543189024071263, -0.2665933059059888421 ) ) ;
#14649 = CARTESIAN_POINT ( 'NONE',  ( -1.482939632545930975, -0.004921259842519576551, 0.3153832671262227771 ) ) ;
#14650 = CARTESIAN_POINT ( 'NONE',  ( 0.2362204724409451007, -0.4091458600556402980, -0.3261154855643044748 ) ) ;
#14651 = CARTESIAN_POINT ( 'NONE',  ( -0.6167979002624665030, -0.3690944881889765550, -0.3153832671262227771 ) ) ;
#14652 = EDGE_CURVE ( 'NONE', #72992, #38903, #26195, .T. ) ;
#14653 = CARTESIAN_POINT ( 'NONE',  ( 0.4479262672266381418, 1.381097145630199030, -1.587474637006627276 ) ) ;
#14654 = CARTESIAN_POINT ( 'NONE',  ( -0.1312335958005241554, -0.6046776061558809534, -0.2411417322834644161 ) ) ;
#14655 = LINE ( 'NONE', #33995, #55897 ) ;
#14656 = CARTESIAN_POINT ( 'NONE',  ( 0.4133858267716541968, -0.4536011799217368745, -0.2665933059059886201 ) ) ;
#14657 = CARTESIAN_POINT ( 'NONE',  ( -0.2690288713910754526, 0.1771653543307087075, -0.09757992244046823083 ) ) ;
#14658 = CARTESIAN_POINT ( 'NONE',  ( -0.3018372703412066094, -0.4281496062992127816, -0.4176697321401328100 ) ) ;
#14659 = CARTESIAN_POINT ( 'NONE',  ( -1.732283464566928277, -0.1870078740157479769, 0.4822834645669291653 ) ) ;
#14660 = CARTESIAN_POINT ( 'NONE',  ( -0.9645669291338575535, 0.07958543189024071263, -0.2665933059059888421 ) ) ;
#14661 = CARTESIAN_POINT ( 'NONE',  ( -0.4091458600556405756, 0.2362204724409446288, -1.992782152230971437 ) ) ;
#14662 = CARTESIAN_POINT ( 'NONE',  ( 0.6561679790026253567, -0.6046776061558809534, -0.2411417322834644161 ) ) ;
#14663 = CARTESIAN_POINT ( 'NONE',  ( -0.8727034120734901146, -0.3162353388693405765, 0.4822834645669290543 ) ) ;
#14664 = CARTESIAN_POINT ( 'NONE',  ( -0.3996062992125984925, -0.1070741851644056858, -1.382545931758530022 ) ) ;
#14665 = CARTESIAN_POINT ( 'NONE',  ( -9.594673741351313045E-17, 0.3917322834645670104, -2.761811023622046779 ) ) ;
#14666 = CARTESIAN_POINT ( 'NONE',  ( -0.3608923884514428360, -0.5511811023622048555, -0.09757992244046775898 ) ) ;
#14667 = DIRECTION ( 'NONE',  ( -2.956072690630991733E-16, 1.000000000000000000, 5.002896285981958034E-32 ) ) ;
#14668 = CARTESIAN_POINT ( 'NONE',  ( -1.049868766404198794, -0.5023911411419708095, 0.1820866141732285504 ) ) ;
#14669 = CARTESIAN_POINT ( 'NONE',  ( 1.574803149606299746, -0.1870078740157480879, -0.4822834645669291653 ) ) ;
#14670 = EDGE_CURVE ( 'NONE', #11874, #32456, #72529, .T. ) ;
#14671 = CARTESIAN_POINT ( 'NONE',  ( -0.8464566929133852113, 0.07958543189024085140, 0.2665933059059887866 ) ) ;
#14672 = CARTESIAN_POINT ( 'NONE',  ( -0.5120078740157480990, 0.000000000000000000, 0.000000000000000000 ) ) ;
#14673 = CARTESIAN_POINT ( 'NONE',  ( 0.9514435695538062676, -0.05778040916215522460, 0.4822834645669289988 ) ) ;
#14674 = CARTESIAN_POINT ( 'NONE',  ( 0.1070741851644054915, -0.3996062992125986035, 0.07217847769028869209 ) ) ;
#14675 = CARTESIAN_POINT ( 'NONE',  ( 0.3917322834645670659, 2.398668435337828261E-17, -2.634533751477377450 ) ) ;
#14676 = EDGE_CURVE ( 'NONE', #29189, #27377, #70760, .T. ) ;
#14677 = CARTESIAN_POINT ( 'NONE',  ( -3.821484228344193657, 2.755905511811024056, -0.5314960629921260393 ) ) ;
#14678 = CARTESIAN_POINT ( 'NONE',  ( 1.574803149606299746, -0.1870078740157479769, 0.3641732283464567677 ) ) ;
#14679 = CARTESIAN_POINT ( 'NONE',  ( -1.377952755905511140, 0.2952755905511811885, 0.000000000000000000 ) ) ;
#14680 = CARTESIAN_POINT ( 'NONE',  ( 1.305774278215223960, 0.2952755905511810774, -0.1292274648535930714 ) ) ;
#14681 = CARTESIAN_POINT ( 'NONE',  ( -9.594673741351313045E-17, 0.3917322834645670104, -2.604330708661416693 ) ) ;
#14682 = DIRECTION ( 'NONE',  ( -0.000000000000000000, -1.000000000000000000, 8.673617379884024625E-16 ) ) ;
#14683 = CARTESIAN_POINT ( 'NONE',  ( 0.3215223097112867578, -0.3162353388693409650, -0.4822834645669289433 ) ) ;
#14684 = CARTESIAN_POINT ( 'NONE',  ( -0.5839895013123351797, -0.6692913385826771977, 0.1292274648535927661 ) ) ;
#14685 = CARTESIAN_POINT ( 'NONE',  ( 1.535433070866142558, 0.2952755905511811885, 0.000000000000000000 ) ) ;
#14686 = CARTESIAN_POINT ( 'NONE',  ( 0.3996062992125986035, 2.446882876249141962E-17, -2.007874015748031482 ) ) ;
#14687 = CARTESIAN_POINT ( 'NONE',  ( 0.5774278215223103139, -0.5023911411419708095, -0.1820866141732282451 ) ) ;
#14688 = VECTOR ( 'NONE', #14197, 39.37007874015748854 ) ;
#14689 = CARTESIAN_POINT ( 'NONE',  ( 0.3996062992125986035, 2.446882876249141962E-17, -1.850393700787401619 ) ) ;
#14690 = ORIENTED_EDGE ( 'NONE', *, *, #15825, .F. ) ;
#14691 = CARTESIAN_POINT ( 'NONE',  ( 0.1049643490035303967, 0.3917322834645670659, -0.3051374260180596543 ) ) ;
#14692 = ORIENTED_EDGE ( 'NONE', *, *, #37239, .F. ) ;
#14693 = CARTESIAN_POINT ( 'NONE',  ( -0.4527559055118102749, 0.1660481256975885056, 0.3530559997133364547 ) ) ;
#14694 = CARTESIAN_POINT ( 'NONE',  ( 1.371391076115485719, -0.6692913385826773087, -0.1292274648535924053 ) ) ;
#14695 = CARTESIAN_POINT ( 'NONE',  ( 0.3346456692913393205, -0.5400638737290845981, -0.3530559997133363437 ) ) ;
#14696 = CARTESIAN_POINT ( 'NONE',  ( -0.3871391076115476282, -0.08942795157527998196, 0.3641732283464567121 ) ) ;
#14697 = CARTESIAN_POINT ( 'NONE',  ( 1.410761154855643795, -0.05778040916215560624, -0.4822834645669293319 ) ) ;
#14698 = CARTESIAN_POINT ( 'NONE',  ( -0.6299212598425188991, -0.1870078740157480879, -0.4822834645669291653 ) ) ;
#14699 = CARTESIAN_POINT ( 'NONE',  ( 0.1312335958005255154, -0.6046776061558807314, 0.2411417322834647770 ) ) ;
#14700 = CARTESIAN_POINT ( 'NONE',  ( -1.601049868766403650, 0.2306618581243847221, -0.2411417322834647770 ) ) ;
#14701 = CARTESIAN_POINT ( 'NONE',  ( 0.7086614173228352742, -0.1870078740157480879, -0.4822834645669291653 ) ) ;
#14702 = ADVANCED_FACE ( 'NONE', ( #23204 ), #9349, .F. ) ;
#14703 = CARTESIAN_POINT ( 'NONE',  ( 1.036745406824147731, 0.05413385826771666132, 0.4176697321401328100 ) ) ;
#14704 = CARTESIAN_POINT ( 'NONE',  ( 0.3392501089628018884, -0.1958661417322834220, -0.5695538057742781657 ) ) ;
#14705 = CARTESIAN_POINT ( 'NONE',  ( 8.195543980992789655E-16, -0.1870078740157480601, -0.3641732283464567677 ) ) ;
#14706 = EDGE_LOOP ( 'NONE', ( #45487, #73905, #13746, #44416, #61695, #47509 ) ) ;
#14707 = CARTESIAN_POINT ( 'NONE',  ( 0.1058382717557500713, -0.3949938075777409408, -1.187664041994750619 ) ) ;
#14708 = ORIENTED_EDGE ( 'NONE', *, *, #20551, .F. ) ;
#14709 = CARTESIAN_POINT ( 'NONE',  ( -0.4002624671916004129, -0.08942795157528024563, -0.3641732283464568787 ) ) ;
#14710 = CARTESIAN_POINT ( 'NONE',  ( 0.1115485564304470323, 0.2952755905511811885, 0.1292274648535926551 ) ) ;
#14711 = CARTESIAN_POINT ( 'NONE',  ( 2.619510771202491206, 1.365902157108384696, 0.4425616331406697634 ) ) ;
#14712 = CARTESIAN_POINT ( 'NONE',  ( -0.2690288713910754526, 0.2952755905511810774, -0.1292274648535930714 ) ) ;
#14713 = CARTESIAN_POINT ( 'NONE',  ( -0.3018372703412066094, 0.05413385826771666132, 0.4176697321401328100 ) ) ;
#14714 = CARTESIAN_POINT ( 'NONE',  ( -0.9514435695538050464, -0.05778040916215560624, -0.4822834645669293319 ) ) ;
#14715 = CARTESIAN_POINT ( 'NONE',  ( -0.8727034120734901146, -0.05778040916215560624, -0.4822834645669293319 ) ) ;
#14716 = EDGE_CURVE ( 'NONE', #19641, #33945, #68112, .T. ) ;
#14717 = CARTESIAN_POINT ( 'NONE',  ( 1.318897637795276356, -0.4536011799217367080, 0.2665933059059888421 ) ) ;
#14718 = CARTESIAN_POINT ( 'NONE',  ( -1.456692913385826182, 0.2952755905511811885, 0.000000000000000000 ) ) ;
#14719 = CARTESIAN_POINT ( 'NONE',  ( 0.09404056145105300912, 1.063503333403748474, 0.2573448916946036724 ) ) ;
#14720 = CARTESIAN_POINT ( 'NONE',  ( 0.5446194225721792126, -0.08942795157528024563, -0.3641732283464568787 ) ) ;
#14721 = CARTESIAN_POINT ( 'NONE',  ( 0.4461942257217856311, 0.2306618581243847221, -0.2411417322834647770 ) ) ;
#14722 = CARTESIAN_POINT ( 'NONE',  ( 0.4199475065616805614, 0.2306618581243848609, 0.2411417322834645549 ) ) ;
#14723 = CARTESIAN_POINT ( 'NONE',  ( 0.3996062992125986035, 0.1070741851644054776, -1.069553805774278166 ) ) ;
#14724 = CARTESIAN_POINT ( 'NONE',  ( -0.5611900217179893735, -2.567464376874931580E-15, -0.4445507791589072832 ) ) ;
#14725 = CARTESIAN_POINT ( 'NONE',  ( -0.3996062992125985480, -7.340648628747423112E-17, -0.7460629921259841479 ) ) ;
#14726 = CARTESIAN_POINT ( 'NONE',  ( -0.3460692066303957537, -0.1998031496062994405, -0.6017060367454067915 ) ) ;
#14727 = CARTESIAN_POINT ( 'NONE',  ( -0.4002624671916004129, -0.05778040916215560624, -0.4822834645669293319 ) ) ;
#14728 = CARTESIAN_POINT ( 'NONE',  ( -0.1265901696524986964, -0.4724409448818899238, -0.07217847769028870597 ) ) ;
#14729 = EDGE_CURVE ( 'NONE', #37337, #59692, #26524, .T. ) ;
#14730 = CARTESIAN_POINT ( 'NONE',  ( 0.1958661417322836440, -0.3392501089628017219, -2.066272965879265122 ) ) ;
#14731 = CARTESIAN_POINT ( 'NONE',  ( -1.305774278215222184, 0.1771653543307087630, 0.09757992244046791164 ) ) ;
#14732 = CARTESIAN_POINT ( 'NONE',  ( 0.8595800524934390507, -0.05778040916215560624, -0.4822834645669293319 ) ) ;
#14733 = CARTESIAN_POINT ( 'NONE',  ( 0.8989501312335964611, 0.2952755905511811885, 0.1292274648535926551 ) ) ;
#14734 = CARTESIAN_POINT ( 'NONE',  ( -0.07874015748031421014, -0.1870078740157479769, 0.3641732283464567677 ) ) ;
#14735 = CARTESIAN_POINT ( 'NONE',  ( 0.4855643044619428750, 0.05413385826771666132, 0.4176697321401328100 ) ) ;
#14736 = CARTESIAN_POINT ( 'NONE',  ( 0.3458507752293908943, 0.3458507752293908943, -2.104330708661417138 ) ) ;
#14737 = CARTESIAN_POINT ( 'NONE',  ( 0.05249343832021075018, -0.5023911411419708095, 0.1820866141732285504 ) ) ;
#14738 = CARTESIAN_POINT ( 'NONE',  ( -0.1181102362204717315, 0.2952755905511811885, 0.000000000000000000 ) ) ;
#14739 = CARTESIAN_POINT ( 'NONE',  ( 0.2891555358219910499, -0.2891555358219909944, -1.592519685039370581 ) ) ;
#14740 = CARTESIAN_POINT ( 'NONE',  ( -1.535433070866141225, 0.2952755905511811885, 0.000000000000000000 ) ) ;
#14741 = CARTESIAN_POINT ( 'NONE',  ( 0.4265091863517067039, -0.5511811023622048555, -0.09757992244046775898 ) ) ;
#14742 = FACE_OUTER_BOUND ( 'NONE', #40242, .T. ) ;
#14743 = CARTESIAN_POINT ( 'NONE',  ( -0.6561679790026240244, -0.6046776061558807314, 0.2411417322834647770 ) ) ;
#14744 = CARTESIAN_POINT ( 'NONE',  ( -0.5314960629921250401, 0.07958543189024085140, 0.2665933059059887866 ) ) ;
#14745 = CARTESIAN_POINT ( 'NONE',  ( 1.572991167713778227, 1.535433070866141447, -0.1227090857360983167 ) ) ;
#14746 = CARTESIAN_POINT ( 'NONE',  ( -0.7808398950131225646, -0.05778040916215522460, 0.4822834645669289988 ) ) ;
#14747 = CARTESIAN_POINT ( 'NONE',  ( -0.6627296587926501115, 0.2952755905511810774, -0.1292274648535930714 ) ) ;
#14748 = CARTESIAN_POINT ( 'NONE',  ( 0.03280839895013198948, -0.6692913385826773087, -0.1292274648535924053 ) ) ;
#14749 = CARTESIAN_POINT ( 'NONE',  ( 0.1070741851644054776, -0.3996062992125984925, -2.524278215223096478 ) ) ;
#14750 = CARTESIAN_POINT ( 'NONE',  ( 0.3917322834645668994, 0.1049643490035304522, -2.094468873194538450 ) ) ;
#14751 = CARTESIAN_POINT ( 'NONE',  ( -0.5314960629921127166, 2.755905511811024056, -3.821484228344195433 ) ) ;
#14752 = CARTESIAN_POINT ( 'NONE',  ( 0.6955380577427828781, -0.3690944881889763329, 0.3153832671262228327 ) ) ;
#14753 = CARTESIAN_POINT ( 'NONE',  ( 1.371391076115485719, -0.6692913385826773087, -0.1292274648535924053 ) ) ;
#14754 = CARTESIAN_POINT ( 'NONE',  ( -1.115485564304461219, -0.3690944881889763329, 0.3153832671262228327 ) ) ;
#14755 = CARTESIAN_POINT ( 'NONE',  ( -1.174540682414697335, -0.2845877964562161244, -0.3641732283464567121 ) ) ;
#14756 = CARTESIAN_POINT ( 'NONE',  ( -0.5774278215223089816, 0.2306618581243847221, -0.2411417322834647770 ) ) ;
#14757 = CARTESIAN_POINT ( 'NONE',  ( 0.006561679790026889343, -0.2845877964562161244, -0.3641732283464567121 ) ) ;
#14758 = CARTESIAN_POINT ( 'NONE',  ( -0.2371319115525430399, 0.1759675087575592878, 5.678257627497697690 ) ) ;
#14759 = CARTESIAN_POINT ( 'NONE',  ( 0.9251968503937015864, -0.4536011799217367080, 0.2665933059059888421 ) ) ;
#14760 = CARTESIAN_POINT ( 'NONE',  ( 0.4133858267716541968, 0.1660481256975885056, 0.3530559997133364547 ) ) ;
#14761 = CARTESIAN_POINT ( 'NONE',  ( -0.1998031496062991630, -0.3460692066303959202, 0.1725721784776902690 ) ) ;
#14762 = CARTESIAN_POINT ( 'NONE',  ( -0.6102362204724400829, 0.1660481256975885056, 0.3530559997133364547 ) ) ;
#14763 = CARTESIAN_POINT ( 'NONE',  ( 0.3917322834645670104, 2.398668435337828261E-17, -1.305118110236220375 ) ) ;
#14764 = CARTESIAN_POINT ( 'NONE',  ( -1.719160104986876103, 0.05413385826771666132, 0.4176697321401328100 ) ) ;
#14765 = CARTESIAN_POINT ( 'NONE',  ( 0.5249343832021005074, -0.6046776061558807314, 0.2411417322834647770 ) ) ;
#14766 = CARTESIAN_POINT ( 'NONE',  ( -0.01312335958005186876, 0.05413385826771626580, -0.4176697321401330321 ) ) ;
#14767 = CARTESIAN_POINT ( 'NONE',  ( -0.1246719160104980823, -0.5511811023622048555, -0.09757992244046775898 ) ) ;
#14768 = CARTESIAN_POINT ( 'NONE',  ( 2.795275590551181466, 1.299212598425198095, -1.617488608965169241E-16 ) ) ;
#14769 = CARTESIAN_POINT ( 'NONE',  ( -0.09842519685039295696, -0.4536011799217367080, 0.2665933059059888421 ) ) ;
#14770 = CARTESIAN_POINT ( 'NONE',  ( 0.7480314960629927956, 0.2952755905511811885, 0.000000000000000000 ) ) ;
#14771 = EDGE_CURVE ( 'NONE', #64662, #56613, #34424, .T. ) ;
#14772 = CARTESIAN_POINT ( 'NONE',  ( -0.6824146981627291497, -0.5023911411419708095, -0.1820866141732282451 ) ) ;
#14773 = CARTESIAN_POINT ( 'NONE',  ( -0.2925321140481932369, 0.2925321140481931259, -0.8838582677165351953 ) ) ;
#14774 = CARTESIAN_POINT ( 'NONE',  ( -1.148293963254592542, 0.2952755905511811885, 0.1292274648535926551 ) ) ;
#14775 = CARTESIAN_POINT ( 'NONE',  ( 0.2034120734908141659, 0.2066929133858267098, -0.1054918080437494132 ) ) ;
#14776 = EDGE_LOOP ( 'NONE', ( #71085, #23283, #68737, #39508 ) ) ;
#14777 = CARTESIAN_POINT ( 'NONE',  ( -1.135170603674539924, 0.2952755905511810774, -0.1292274648535930714 ) ) ;
#14778 = CARTESIAN_POINT ( 'NONE',  ( -1.161417322834644716, -0.4536011799217368745, -0.2665933059059886201 ) ) ;
#14779 = CARTESIAN_POINT ( 'NONE',  ( 0.1509186351706042484, -0.3162353388693405765, 0.4822834645669290543 ) ) ;
#14780 = DIRECTION ( 'NONE',  ( 0.000000000000000000, 1.000000000000000000, 0.000000000000000000 ) ) ;
#14781 = CARTESIAN_POINT ( 'NONE',  ( -0.9383202099737524282, -0.3162353388693409650, -0.4822834645669289433 ) ) ;
#14782 = CARTESIAN_POINT ( 'NONE',  ( -1.646051170424378096, 0.000000000000000000, 0.3464511005275205946 ) ) ;
#14784 = CARTESIAN_POINT ( 'NONE',  ( 0.9186351706036751663, -0.6046776061558807314, 0.2411417322834647770 ) ) ;
#14783 = CARTESIAN_POINT ( 'NONE',  ( 1.614173228346457378, -0.6692913385826771977, 8.415575281601705876E-17 ) ) ;
#14785 = CARTESIAN_POINT ( 'NONE',  ( 0.7217847769028878924, 0.05413385826771666132, 0.4176697321401328100 ) ) ;
#14786 = CARTESIAN_POINT ( 'NONE',  ( 0.1049643490035304799, -0.3917322834645669549, -2.282152230971128404 ) ) ;
#14787 = CARTESIAN_POINT ( 'NONE',  ( 1.594488188976378673, 0.1660481256975885056, 0.3530559997133364547 ) ) ;
#14788 = CARTESIAN_POINT ( 'NONE',  ( -1.443569553805773564, -0.6046776061558807314, 0.2411417322834647770 ) ) ;
#14789 = CARTESIAN_POINT ( 'NONE',  ( -0.3460692066303960868, 0.1998031496062990242, -0.6561679790026246906 ) ) ;
#14790 = ORIENTED_EDGE ( 'NONE', *, *, #58775, .F. ) ;
#14791 = CARTESIAN_POINT ( 'NONE',  ( -0.4986876640419939388, 0.1283753931104746893, -0.1820866141732285504 ) ) ;
#14792 = CARTESIAN_POINT ( 'NONE',  ( 0.1958661417322836440, -0.3392501089628017219, -2.288713910761154935 ) ) ;
#14793 = ORIENTED_EDGE ( 'NONE', *, *, #18368, .F. ) ;
#14794 = CARTESIAN_POINT ( 'NONE',  ( 0.4461942257217855201, -0.6046776061558807314, 0.2411417322834647770 ) ) ;
#14795 = CARTESIAN_POINT ( 'NONE',  ( -0.07217847769028813698, -0.3162353388693409650, -0.4822834645669289433 ) ) ;
#14796 = CARTESIAN_POINT ( 'NONE',  ( -0.8202099737532799750, 0.2952755905511810774, -0.1292274648535930714 ) ) ;
#14797 = CARTESIAN_POINT ( 'NONE',  ( 1.345144356955381593, -0.05778040916215522460, 0.4822834645669289988 ) ) ;
#14798 = CARTESIAN_POINT ( 'NONE',  ( -1.036745406824146176, -0.3690944881889763329, 0.3153832671262228327 ) ) ;
#14799 = CARTESIAN_POINT ( 'NONE',  ( 0.05682587177516690985, 1.066401174101865301, -1.556166698229688228 ) ) ;
#14800 = CARTESIAN_POINT ( 'NONE',  ( 0.6955380577427828781, -0.4281496062992124485, 0.4176697321401328655 ) ) ;
#14801 = CARTESIAN_POINT ( 'NONE',  ( 0.4199475065616803948, -0.5023911411419708095, -0.1820866141732282451 ) ) ;
#14802 = CARTESIAN_POINT ( 'NONE',  ( -0.4986876640419939388, 0.2306618581243847221, -0.2411417322834647770 ) ) ;
#14803 = CARTESIAN_POINT ( 'NONE',  ( 0.3917322834645668994, 0.1049643490035304522, -1.149586983430759490 ) ) ;
#14804 = CARTESIAN_POINT ( 'NONE',  ( -1.272965879265091305, 0.05413385826771626580, -0.4176697321401330321 ) ) ;
#14805 = CARTESIAN_POINT ( 'NONE',  ( -1.706036745406823485, 0.1283753931104748280, 0.1820866141732283561 ) ) ;
#14806 = CARTESIAN_POINT ( 'NONE',  ( 1.522309711286089939, 0.2306618581243848609, 0.2411417322834645549 ) ) ;
#14807 = CARTESIAN_POINT ( 'NONE',  ( 1.653543307086614789, -0.1870078740157479769, 0.3641732283464567677 ) ) ;
#14808 = ORIENTED_EDGE ( 'NONE', *, *, #8454, .F. ) ;
#14809 = CARTESIAN_POINT ( 'NONE',  ( 0.1049643490035303967, 0.3917322834645670659, -2.509861835466878244 ) ) ;
#14810 = CARTESIAN_POINT ( 'NONE',  ( -0.09186351706036663400, -0.4281496062992124485, 0.4176697321401328655 ) ) ;
#14811 = ORIENTED_EDGE ( 'NONE', *, *, #76605, .F. ) ;
#14812 = CARTESIAN_POINT ( 'NONE',  ( 0.6627296587926515548, 0.1771653543307087630, 0.09757992244046791164 ) ) ;
#14813 = CARTESIAN_POINT ( 'NONE',  ( -1.154855643044618851, -0.6046776061558809534, -0.2411417322834644161 ) ) ;
#14814 = CARTESIAN_POINT ( 'NONE',  ( 1.056430446194226436, -0.6692913385826773087, -0.1292274648535924053 ) ) ;
#14815 = CARTESIAN_POINT ( 'NONE',  ( 1.154855643044620184, 0.2306618581243847221, -0.2411417322834647770 ) ) ;
#14816 = CARTESIAN_POINT ( 'NONE',  ( 0.4002624671916016896, -0.3162353388693409650, -0.4822834645669289433 ) ) ;
#14817 = CARTESIAN_POINT ( 'NONE',  ( -0.4790026246719152336, -0.05778040916215560624, -0.4822834645669293319 ) ) ;
#14818 = CARTESIAN_POINT ( 'NONE',  ( -0.3917322834645669549, -0.1049643490035306603, -2.020341207349081181 ) ) ;
#14819 = CARTESIAN_POINT ( 'NONE',  ( -1.128608923884513837, -0.6046776061558807314, 0.2411417322834647770 ) ) ;
#14820 = CARTESIAN_POINT ( 'NONE',  ( -0.7349081364829387342, -0.6046776061558807314, 0.2411417322834647770 ) ) ;
#14821 = CARTESIAN_POINT ( 'NONE',  ( -0.5774278215223089816, -0.5023911411419708095, 0.1820866141732285504 ) ) ;
#14822 = CARTESIAN_POINT ( 'NONE',  ( 1.633858267716535639, -0.5400638737290844871, 0.3530559997133364547 ) ) ;
#14823 = CARTESIAN_POINT ( 'NONE',  ( -0.4396325459317579898, 0.2952755905511811885, 0.1292274648535926551 ) ) ;
#14824 = CARTESIAN_POINT ( 'NONE',  ( -1.646051170424378096, 0.000000000000000000, -0.3464511005275205946 ) ) ;
#14825 = CARTESIAN_POINT ( 'NONE',  ( 0.5249343832021003964, 0.2306618581243847221, -0.2411417322834647770 ) ) ;
#14826 = CARTESIAN_POINT ( 'NONE',  ( -9.787531504996567848E-17, 0.3996062992125986035, -1.732283464566929165 ) ) ;
#14827 = CARTESIAN_POINT ( 'NONE',  ( 3.908320185825792770, 1.506432478651347662, -0.4744094488188970171 ) ) ;
#14828 = CARTESIAN_POINT ( 'NONE',  ( -0.1574803149606292529, -0.1870078740157480879, -0.4822834645669291653 ) ) ;
#14830 = CARTESIAN_POINT ( 'NONE',  ( -0.4498537592782897998, 0.000000000000000000, 2.118110236220472675 ) ) ;
#14829 = CARTESIAN_POINT ( 'NONE',  ( 0.8202099737532814183, -0.5511811023622048555, -0.09757992244046775898 ) ) ;
#14831 = CARTESIAN_POINT ( 'NONE',  ( 5.785732909357575061E-17, -0.4724409448818898682, -0.7854330708661416693 ) ) ;
#14832 = CARTESIAN_POINT ( 'NONE',  ( 1.082677165354331228, 0.07958543189024071263, -0.2665933059059888421 ) ) ;
#14833 = CARTESIAN_POINT ( 'NONE',  ( 1.069553805774278610, -0.6692913385826771977, 0.1292274648535927661 ) ) ;
#14834 = CARTESIAN_POINT ( 'NONE',  ( 4.837279021331061486E-17, -0.3949938075777409963, 0.001968503937007861845 ) ) ;
#14835 = CARTESIAN_POINT ( 'NONE',  ( -0.3937007874015740483, -0.1870078740157480879, -0.4822834645669291653 ) ) ;
#14836 = CARTESIAN_POINT ( 'NONE',  ( -0.4037097067573596210, -2.567464376874931580E-15, -0.4445507791589072832 ) ) ;
#14837 = CARTESIAN_POINT ( 'NONE',  ( -1.712598425196849572, 0.1660481256975885056, 0.3530559997133364547 ) ) ;
#14838 = CARTESIAN_POINT ( 'NONE',  ( -0.09186351706036689768, 0.05413385826771626580, -0.4176697321401330321 ) ) ;
#14839 = CARTESIAN_POINT ( 'NONE',  ( 0.3949938075777408852, 0.1058382717557500435, -0.6738845144356955252 ) ) ;
#14840 = CARTESIAN_POINT ( 'NONE',  ( 1.351706036745407680, 0.05413385826771666132, 0.4176697321401328100 ) ) ;
#14841 = CARTESIAN_POINT ( 'NONE',  ( 0.6561679790026253567, 0.2306618581243848609, 0.2411417322834645549 ) ) ;
#14842 = CARTESIAN_POINT ( 'NONE',  ( 0.7874015748031503170, -0.1870078740157480601, -0.3641732283464567677 ) ) ;
#14843 = CARTESIAN_POINT ( 'NONE',  ( 1.374111566022513293E-16, 1.062992125984252745, -1.122047244094488194 ) ) ;
#14844 = CARTESIAN_POINT ( 'NONE',  ( 0.5643044619422579178, -0.004921259842519576551, 0.3153832671262227771 ) ) ;
#14845 = CARTESIAN_POINT ( 'NONE',  ( -1.056430446194224881, 0.2066929133858267098, -0.1054918080437494132 ) ) ;
#14846 = CARTESIAN_POINT ( 'NONE',  ( 0.1070741851644054776, -0.3996062992125984925, -1.421916010498687877 ) ) ;
#14847 = CARTESIAN_POINT ( 'NONE',  ( 0.5971128608923891301, 0.2952755905511810774, -0.1292274648535930714 ) ) ;
#14848 = CARTESIAN_POINT ( 'NONE',  ( 0.1049643490035303689, 0.3917322834645670104, -0.6154855643044617741 ) ) ;
#14850 = CARTESIAN_POINT ( 'NONE',  ( -0.4623158380715545746, 0.02617651024168222984, -2.142213561789874543 ) ) ;
#14849 = CARTESIAN_POINT ( 'NONE',  ( 0.3412073490813655186, -0.6046776061558809534, -0.2411417322834644161 ) ) ;
#14851 = CARTESIAN_POINT ( 'NONE',  ( -0.3674540682414689785, 0.1539470093639523085, 0.1968503937007873850 ) ) ;
#14852 = CARTESIAN_POINT ( 'NONE',  ( 0.1837270341207354329, 0.1283753931104748280, 0.1820866141732283561 ) ) ;
#14853 = CARTESIAN_POINT ( 'NONE',  ( 0.5708661417322842269, 0.1660481256975885056, 0.3530559997133364547 ) ) ;
#14854 = FACE_OUTER_BOUND ( 'NONE', #6781, .T. ) ;
#14855 = CARTESIAN_POINT ( 'NONE',  ( -1.043307086614172707, 0.07958543189024071263, -0.2665933059059888421 ) ) ;
#14856 = CARTESIAN_POINT ( 'NONE',  ( -0.9514435695538050464, -0.3162353388693405765, 0.4822834645669290543 ) ) ;
#14857 = CARTESIAN_POINT ( 'NONE',  ( -1.496062992125983815, -0.1870078740157480879, -0.4822834645669291653 ) ) ;
#14858 = CARTESIAN_POINT ( 'NONE',  ( 0.6102362204724416372, 0.1660481256975883668, -0.3530559997133364547 ) ) ;
#14859 = CARTESIAN_POINT ( 'NONE',  ( -1.594488188976377119, 0.07958543189024071263, -0.2665933059059888421 ) ) ;
#14860 = CARTESIAN_POINT ( 'NONE',  ( -0.3808816823641234528, 0.09156050430092053938, -1.220472440944881942 ) ) ;
#14861 = CARTESIAN_POINT ( 'NONE',  ( 0.4790026246719167324, -0.05778040916215522460, 0.4822834645669289988 ) ) ;
#14862 = CARTESIAN_POINT ( 'NONE',  ( 0.3460692066303959202, -0.1998031496062991630, 0.1332020997375328031 ) ) ;
#14863 = CARTESIAN_POINT ( 'NONE',  ( 1.686351706036745890, 0.2952755905511811885, 0.1292274648535926551 ) ) ;
#14864 = CARTESIAN_POINT ( 'NONE',  ( 1.325459317585302665, -0.4281496062992124485, 0.4176697321401328655 ) ) ;
#14865 = CARTESIAN_POINT ( 'NONE',  ( -1.469816272965878357, -0.5023911411419708095, -0.1820866141732282451 ) ) ;
#14866 = CARTESIAN_POINT ( 'NONE',  ( 1.318897637795276356, -0.4536011799217367080, 0.2665933059059888421 ) ) ;
#14867 = CARTESIAN_POINT ( 'NONE',  ( -1.509186351706035767, -0.3690944881889763329, 0.3153832671262228327 ) ) ;
#14868 = CARTESIAN_POINT ( 'NONE',  ( -0.7283464566929126471, -0.4536011799217367080, 0.2665933059059888421 ) ) ;
#14869 = ADVANCED_FACE ( 'NONE', ( #3447 ), #8933, .T. ) ;
#14870 = CARTESIAN_POINT ( 'NONE',  ( 1.548556430446194954, -0.6046776061558807314, 0.2411417322834647770 ) ) ;
#14871 = CARTESIAN_POINT ( 'NONE',  ( 0.4461942257217855201, -0.5023911411419708095, 0.1820866141732285504 ) ) ;
#14872 = CARTESIAN_POINT ( 'NONE',  ( -0.04593175853018302557, 0.2952755905511811885, 0.1292274648535926551 ) ) ;
#14873 = CARTESIAN_POINT ( 'NONE',  ( 0.9908136482939640111, 0.2952755905511810774, -0.1292274648535930714 ) ) ;
#14874 = CARTESIAN_POINT ( 'NONE',  ( 8.195543980992789655E-16, -0.1870078740157480879, -0.4822834645669291653 ) ) ;
#14875 = CARTESIAN_POINT ( 'NONE',  ( 0.1377952755905518800, -0.4536011799217367080, 0.2665933059059888421 ) ) ;
#14876 = VECTOR ( 'NONE', #5174, 39.37007874015748143 ) ;
#14877 = CARTESIAN_POINT ( 'NONE',  ( 1.181102362204724976, -0.1870078740157480879, -0.4822834645669291653 ) ) ;
#14878 = CARTESIAN_POINT ( 'NONE',  ( -1.653543307086613234, -0.1870078740157479769, 0.4822834645669291653 ) ) ;
#14879 = CARTESIAN_POINT ( 'NONE',  ( -0.9383202099737524282, -0.05778040916215522460, 0.4822834645669289988 ) ) ;
#14880 = CARTESIAN_POINT ( 'NONE',  ( 0.2925321140481932369, -0.2925321140481931814, -0.8858267716535431768 ) ) ;
#14881 = CARTESIAN_POINT ( 'NONE',  ( 0.01968503937007930540, 0.1012011053420777407, 0.2882089793578257453 ) ) ;
#14882 = CARTESIAN_POINT ( 'NONE',  ( -0.8136482939632537770, 0.2306618581243847221, -0.2411417322834647770 ) ) ;
#14883 = CARTESIAN_POINT ( 'NONE',  ( -0.1312335958005241554, 0.2306618581243848609, 0.2411417322834645549 ) ) ;
#14884 = CARTESIAN_POINT ( 'NONE',  ( 0.1998031496062992740, 0.3460692066303959757, -2.664041994750656173 ) ) ;
#14885 = CARTESIAN_POINT ( 'NONE',  ( 0.1974969037888706369, -0.3420746716998659953, -1.981627296587926690 ) ) ;
#14886 = CARTESIAN_POINT ( 'NONE',  ( 0.3392501089628018329, 0.1958661417322835607, -0.5958005249343831800 ) ) ;
#14887 = CARTESIAN_POINT ( 'NONE',  ( 3.892860353355074299, 2.712196231959916659, -0.5314960629921260393 ) ) ;
#14888 = CARTESIAN_POINT ( 'NONE',  ( -1.463254593175852492, -0.5511811023622048555, -0.09757992244046775898 ) ) ;
#14889 = CARTESIAN_POINT ( 'NONE',  ( 0.2867679344610365999, 0.2867679344610365999, -0.9173228346456693272 ) ) ;
#14890 = CARTESIAN_POINT ( 'NONE',  ( -1.686351706036744558, 0.2952755905511810774, -0.1292274648535930714 ) ) ;
#14891 = CARTESIAN_POINT ( 'NONE',  ( -0.1958661417322836440, 0.3392501089628016664, -0.09315653723653360974 ) ) ;
#14892 = CARTESIAN_POINT ( 'NONE',  ( 0.3805774278215230400, -0.4281496062992124485, 0.4176697321401328655 ) ) ;
#14893 = CARTESIAN_POINT ( 'NONE',  ( -0.4330708661417315697, 0.1771653543307087630, 0.000000000000000000 ) ) ;
#14894 = CARTESIAN_POINT ( 'NONE',  ( 0.8923884514435701520, -0.6046776061558809534, -0.2411417322834644161 ) ) ;
#14895 = CARTESIAN_POINT ( 'NONE',  ( 0.1509186351706042484, -0.3162353388693405765, 0.4822834645669290543 ) ) ;
#14896 = CARTESIAN_POINT ( 'NONE',  ( 0.03176189650790594426, 1.062992125984252301, 1.122047244094488194 ) ) ;
#14897 = CARTESIAN_POINT ( 'NONE',  ( 0.1998031496062994405, -0.3460692066303958092, -2.454068241469816058 ) ) ;
#14898 = CARTESIAN_POINT ( 'NONE',  ( -9.594673741351313045E-17, 0.3917322834645670659, -1.256580995571865200 ) ) ;
#14899 = CARTESIAN_POINT ( 'NONE',  ( 1.404199475065617708, 0.05413385826771626580, -0.4176697321401330321 ) ) ;
#14900 = CARTESIAN_POINT ( 'NONE',  ( 0.05905511811023681640, 0.1660481256975883668, -0.3530559997133364547 ) ) ;
#14901 = CARTESIAN_POINT ( 'NONE',  ( 1.574803149606299746, -0.1870078740157479769, 0.4822834645669291653 ) ) ;
#14902 = CARTESIAN_POINT ( 'NONE',  ( 0.9317585301837276734, 0.05413385826771626580, -0.4176697321401330321 ) ) ;
#14903 = CARTESIAN_POINT ( 'NONE',  ( 0.3392501089628018884, -0.1958661417322834220, -0.5045931758530184386 ) ) ;
#14904 = CARTESIAN_POINT ( 'NONE',  ( 0.05905511811023681640, 0.1660481256975883668, -0.3530559997133364547 ) ) ;
#14905 = CARTESIAN_POINT ( 'NONE',  ( 0.5249343832021005074, -0.6046776061558807314, 0.2411417322834647770 ) ) ;
#14906 = CARTESIAN_POINT ( 'NONE',  ( 0.09186351706036827158, 0.05413385826771666132, 0.4176697321401328100 ) ) ;
#14907 = CARTESIAN_POINT ( 'NONE',  ( 0.9186351706036752773, 0.1283753931104746893, -0.1820866141732285504 ) ) ;
#14908 = CARTESIAN_POINT ( 'NONE',  ( -1.338582677165353729, -0.1870078740157480879, -0.4822834645669291653 ) ) ;
#14909 = CARTESIAN_POINT ( 'NONE',  ( -1.253280839895012377, -0.05778040916215522460, 0.4822834645669289988 ) ) ;
#14910 = CARTESIAN_POINT ( 'NONE',  ( 0.6627296587926515548, 0.2952755905511811885, 0.1292274648535926551 ) ) ;
#14911 = CARTESIAN_POINT ( 'NONE',  ( 0.4724409448818898682, 0.000000000000000000, -2.755905511811024056 ) ) ;
#14912 = CARTESIAN_POINT ( 'NONE',  ( -0.3917322834645669549, -0.1049643490035306603, -1.770341207349081181 ) ) ;
#14913 = VERTEX_POINT ( 'NONE', #29111 ) ;
#14914 = CARTESIAN_POINT ( 'NONE',  ( 0.3460692066303959202, 0.1998031496062993295, -0.6036745406824146620 ) ) ;
#14915 = ORIENTED_EDGE ( 'NONE', *, *, #46568, .T. ) ;
#14916 = CARTESIAN_POINT ( 'NONE',  ( 1.240157480314961314, 0.1660481256975883668, -0.3530559997133364547 ) ) ;
#14917 = CARTESIAN_POINT ( 'NONE',  ( 0.3674540682414705883, 0.1283753931104746893, -0.1820866141732285504 ) ) ;
#14918 = CARTESIAN_POINT ( 'NONE',  ( 0.6167979002624679463, 0.05413385826771626580, -0.4176697321401330321 ) ) ;
#14919 = CARTESIAN_POINT ( 'NONE',  ( 0.4531182788721080934, 1.771653543307086354, -0.5309055118110237448 ) ) ;
#14920 = DIRECTION ( 'NONE',  ( -3.491481338843132961E-15, -0.000000000000000000, 1.000000000000000000 ) ) ;
#14921 = CARTESIAN_POINT ( 'NONE',  ( -0.1049643490035302024, -0.3917322834645671215, -1.101706036745407014 ) ) ;
#14922 = CARTESIAN_POINT ( 'NONE',  ( 1.417322834645670104, -0.1870078740157479769, 0.4822834645669291653 ) ) ;
#14923 = CARTESIAN_POINT ( 'NONE',  ( 0.4575346093745696896, 1.663833025909975172, -3.910334573579572037 ) ) ;
#14924 = CARTESIAN_POINT ( 'NONE',  ( -0.2821522309711278487, 0.2952755905511811885, 0.1292274648535926551 ) ) ;
#14925 = CARTESIAN_POINT ( 'NONE',  ( 1.115485564304462551, 0.05413385826771666132, 0.4176697321401328100 ) ) ;
#14926 = ORIENTED_EDGE ( 'NONE', *, *, #60899, .F. ) ;
#14927 = VECTOR ( 'NONE', #46567, 39.37007874015748143 ) ;
#14928 = CARTESIAN_POINT ( 'NONE',  ( -1.587926509186350810, -0.4281496062992124485, 0.4176697321401328655 ) ) ;
#14929 = DIRECTION ( 'NONE',  ( 0.000000000000000000, -1.000000000000000000, 0.000000000000000000 ) ) ;
#14930 = APPLICATION_PROTOCOL_DEFINITION ( 'draft international standard', 'automotive_design', 1998, #6766 ) ;
#14931 = CARTESIAN_POINT ( 'NONE',  ( 1.476377952755906442, -0.4536011799217367080, 0.2665933059059888421 ) ) ;
#14932 = DIRECTION ( 'NONE',  ( 0.000000000000000000, 0.000000000000000000, -1.000000000000000000 ) ) ;
#14933 = CARTESIAN_POINT ( 'NONE',  ( -0.8333333333333323711, 0.1771653543307087630, 0.09757992244046791164 ) ) ;
#14934 = CARTESIAN_POINT ( 'NONE',  ( -1.620734908136482577, 0.2952755905511811885, 0.1292274648535926551 ) ) ;
#14935 = CARTESIAN_POINT ( 'NONE',  ( 0.7349081364829403995, 0.2306618581243848609, 0.2411417322834645549 ) ) ;
#14936 = ORIENTED_EDGE ( 'NONE', *, *, #30614, .F. ) ;
#14938 = CARTESIAN_POINT ( 'NONE',  ( 1.141392835773559211, 0.3937007874015747699, 1.141392835773562764 ) ) ;
#14937 = CARTESIAN_POINT ( 'NONE',  ( 1.646981627296588035, -0.3162353388693405765, 0.4822834645669290543 ) ) ;
#14939 = CARTESIAN_POINT ( 'NONE',  ( -0.5577427821522301654, -0.08942795157528024563, -0.3641732283464568787 ) ) ;
#14940 = CARTESIAN_POINT ( 'NONE',  ( 0.6889763779527566800, -0.5400638737290844871, 0.3530559997133364547 ) ) ;
#14941 = CARTESIAN_POINT ( 'NONE',  ( -1.443569553805773564, -0.6046776061558807314, 0.2411417322834647770 ) ) ;
#14942 = CARTESIAN_POINT ( 'NONE',  ( 0.1958661417322834497, 0.3392501089628018329, -1.326752337761467837 ) ) ;
#14943 = CARTESIAN_POINT ( 'NONE',  ( -0.6167979002624665030, -0.004921259842519576551, 0.3153832671262227771 ) ) ;
#14944 = CARTESIAN_POINT ( 'NONE',  ( -1.417322834645668772, -0.1870078740157480601, -0.3641732283464567677 ) ) ;
#14945 = DIRECTION ( 'NONE',  ( 0.000000000000000000, 0.000000000000000000, -1.000000000000000000 ) ) ;
#14946 = CARTESIAN_POINT ( 'NONE',  ( 0.4527559055118117182, -0.5400638737290844871, 0.3530559997133364547 ) ) ;
#14947 = CARTESIAN_POINT ( 'NONE',  ( -1.023622047244093558, -0.1870078740157479769, 0.3641732283464567677 ) ) ;
#14948 = CARTESIAN_POINT ( 'NONE',  ( -0.1771653543307080136, -0.4536011799217367080, 0.2665933059059888421 ) ) ;
#14949 = VECTOR ( 'NONE', #16026, 39.37007874015748143 ) ;
#14950 = CARTESIAN_POINT ( 'NONE',  ( -0.4265091863517051496, 0.2952755905511810774, -0.1292274648535930714 ) ) ;
#14951 = CARTESIAN_POINT ( 'NONE',  ( 1.614173228346457378, -0.6692913385826771977, 8.415575281601705876E-17 ) ) ;
#14952 = CARTESIAN_POINT ( 'NONE',  ( -0.2867679344610367109, 0.2867679344610365444, -0.01642351525690478181 ) ) ;
#14953 = CARTESIAN_POINT ( 'NONE',  ( 0.8989501312335963501, -0.6692913385826773087, -0.1292274648535924053 ) ) ;
#14954 = ADVANCED_FACE ( 'NONE', ( #48457 ), #42148, .T. ) ;
#14955 = DIRECTION ( 'NONE',  ( -1.000000000000000000, -3.083952846180990774E-16, 0.000000000000000000 ) ) ;
#14956 = CARTESIAN_POINT ( 'NONE',  ( -0.4724409448818899238, 0.1265901696524986686, -1.526902887139107490 ) ) ;
#14957 = CARTESIAN_POINT ( 'NONE',  ( -0.8989501312335946848, 0.2952755905511810774, -0.1292274648535930714 ) ) ;
#14958 = CARTESIAN_POINT ( 'NONE',  ( -0.3280839895013117347, -0.3690944881889763329, 0.3153832671262228327 ) ) ;
#14959 = CARTESIAN_POINT ( 'NONE',  ( -1.423884514435694859, -0.05778040916215560624, -0.4822834645669293319 ) ) ;
#14960 = CARTESIAN_POINT ( 'NONE',  ( 0.5446194225721792126, -0.2845877964562159024, 0.3641732283464567677 ) ) ;
#14961 = CARTESIAN_POINT ( 'NONE',  ( -0.8595800524934373854, -0.2845877964562161244, -0.3641732283464567121 ) ) ;
#14962 = CARTESIAN_POINT ( 'NONE',  ( -1.246719160104986512, 0.05413385826771666132, 0.4176697321401328100 ) ) ;
#14963 = CARTESIAN_POINT ( 'NONE',  ( -1.594488188976377563, -0.5400638737290844871, 0.3530559997133364547 ) ) ;
#14964 = CARTESIAN_POINT ( 'NONE',  ( -1.548556430446193399, -0.6046776061558809534, -0.2411417322834644161 ) ) ;
#14965 = CARTESIAN_POINT ( 'NONE',  ( 1.049868766404200349, 0.1539470093639523085, 0.1968503937007873850 ) ) ;
#14966 = CARTESIAN_POINT ( 'NONE',  ( 0.7939632545931766261, -0.2845877964562161244, -0.3641732283464567121 ) ) ;
#14967 = CARTESIAN_POINT ( 'NONE',  ( 0.2952755905511819101, 0.1660481256975883668, -0.3530559997133364547 ) ) ;
#14968 = CARTESIAN_POINT ( 'NONE',  ( -1.318897637795274802, 0.1660481256975885056, 0.3530559997133364547 ) ) ;
#14969 = CARTESIAN_POINT ( 'NONE',  ( 1.607611548556431069, 0.1771653543307087630, 0.09757992244046791164 ) ) ;
#14970 = ORIENTED_EDGE ( 'NONE', *, *, #8199, .T. ) ;
#14971 = CARTESIAN_POINT ( 'NONE',  ( -0.3420746716998662729, 0.1974969037888702206, 0.2119422572178478181 ) ) ;
#14972 = CARTESIAN_POINT ( 'NONE',  ( -1.279527559055116948, 0.07958543189024071263, -0.2665933059059888421 ) ) ;
#14973 = CARTESIAN_POINT ( 'NONE',  ( -0.4724409448818890911, -0.1870078740157480879, -0.4822834645669291653 ) ) ;
#14974 = CARTESIAN_POINT ( 'NONE',  ( 0.5052493438320215802, 0.2952755905511811885, 0.1292274648535926551 ) ) ;
#14975 = CARTESIAN_POINT ( 'NONE',  ( -1.410761154855642463, -0.08942795157527998196, 0.3641732283464567121 ) ) ;
#14976 = CARTESIAN_POINT ( 'NONE',  ( -0.1070741851644051862, -0.3996062992125986590, -1.723753280839895208 ) ) ;
#14977 = CARTESIAN_POINT ( 'NONE',  ( -1.482939632545930975, -0.4281496062992127816, -0.4176697321401328100 ) ) ;
#14978 = CARTESIAN_POINT ( 'NONE',  ( 0.5708661417322842269, 0.1660481256975885056, 0.3530559997133364547 ) ) ;
#14979 = CARTESIAN_POINT ( 'NONE',  ( 0.07217847769028949700, -0.3162353388693405765, 0.4822834645669290543 ) ) ;
#14980 = CARTESIAN_POINT ( 'NONE',  ( 1.332020997375328974, -0.05778040916215560624, -0.4822834645669293319 ) ) ;
#14981 = CARTESIAN_POINT ( 'NONE',  ( 0.1070741851644053527, 0.3996062992125985480, -1.015091863517060267 ) ) ;
#14982 = CARTESIAN_POINT ( 'NONE',  ( 0.3996062992125986035, 0.1070741851644054776, -1.227034120734908029 ) ) ;
#14983 = CARTESIAN_POINT ( 'NONE',  ( -9.674558042662121740E-17, 0.3949938075777409963, -0.4724409448818898127 ) ) ;
#14984 = CARTESIAN_POINT ( 'NONE',  ( 0.2867679344610366554, -0.2867679344610365444, -0.09055118110236216877 ) ) ;
#14985 = CARTESIAN_POINT ( 'NONE',  ( -0.3083989501312330295, -0.08942795157527998196, 0.3641732283464567121 ) ) ;
#14986 =( GEOMETRIC_REPRESENTATION_CONTEXT ( 3 ) GLOBAL_UNCERTAINTY_ASSIGNED_CONTEXT ( ( #73122 ) ) GLOBAL_UNIT_ASSIGNED_CONTEXT ( ( #36337, #37571, #63245 ) ) REPRESENTATION_CONTEXT ( 'NONE', 'WORKASPACE' ) );
#14987 = CARTESIAN_POINT ( 'NONE',  ( -0.2427821522309703550, -0.05778040916215560624, -0.4822834645669293319 ) ) ;
#14988 = CARTESIAN_POINT ( 'NONE',  ( 0.8727034120734912248, -0.3162353388693409650, -0.4822834645669289433 ) ) ;
#14989 = B_SPLINE_CURVE_WITH_KNOTS ( 'NONE', 3,
 ( #63853, #57110, #57528, #81587 ),
 .UNSPECIFIED., .F., .F.,
 ( 4, 4 ),
 ( 0.1000642744325473399, 0.1014879310549286484 ),
 .UNSPECIFIED. ) ;
#14990 = CARTESIAN_POINT ( 'NONE',  ( 0.3420746716998660508, -0.1974969037888704149, -1.599081364829396223 ) ) ;
#14991 = CARTESIAN_POINT ( 'NONE',  ( -0.03280839895013062252, 0.1771653543307087075, -0.09757992244046823083 ) ) ;
#14992 = CARTESIAN_POINT ( 'NONE',  ( -0.9973753280839886548, 0.2306618581243848609, 0.2411417322834645549 ) ) ;
#14993 = CARTESIAN_POINT ( 'NONE',  ( -1.528871391076114250, -0.6692913385826771977, 0.1292274648535927661 ) ) ;
#14994 = CARTESIAN_POINT ( 'NONE',  ( 0.3458507752293908943, -0.3458507752293908943, -1.830708661417322913 ) ) ;
#14995 = CARTESIAN_POINT ( 'NONE',  ( 0.2749078412854595865, 0.2798680777847445400, -2.755905511811024500 ) ) ;
#14996 = VERTEX_POINT ( 'NONE', #82121 ) ;
#14997 = ORIENTED_EDGE ( 'NONE', *, *, #43522, .T. ) ;
#14998 = CARTESIAN_POINT ( 'NONE',  ( 1.450131233595801428, 0.2952755905511811885, 0.1292274648535926551 ) ) ;
#14999 = CARTESIAN_POINT ( 'NONE',  ( -1.620734908136482577, -0.6692913385826773087, -0.1292274648535924053 ) ) ;
#15001 = CARTESIAN_POINT ( 'NONE',  ( -1.148293963254592542, 0.2952755905511811885, 0.1292274648535926551 ) ) ;
#15000 = CARTESIAN_POINT ( 'NONE',  ( -1.167979002624671470, -0.004921259842519576551, 0.3153832671262227771 ) ) ;
#15002 = CARTESIAN_POINT ( 'NONE',  ( -9.594673741351310580E-17, 0.3917322834645669549, -2.442237902065930388 ) ) ;
#15003 = CARTESIAN_POINT ( 'NONE',  ( -1.010498687664041384, 0.009842519685039467087, 0.3409548833797002021 ) ) ;
#15004 = CARTESIAN_POINT ( 'NONE',  ( 1.148293963254593875, -0.6692913385826771977, 0.1292274648535927661 ) ) ;
#15005 = CARTESIAN_POINT ( 'NONE',  ( -1.646981627296586703, -0.3162353388693409650, -0.4822834645669289433 ) ) ;
#15006 = CARTESIAN_POINT ( 'NONE',  ( -0.2296587926509179312, -0.3162353388693409650, -0.4822834645669289433 ) ) ;
#15007 = CARTESIAN_POINT ( 'NONE',  ( -0.05249343832020938322, -0.6046776061558809534, -0.2411417322834644161 ) ) ;
#15008 = CARTESIAN_POINT ( 'NONE',  ( -1.437007874015747477, 0.1660481256975883668, -0.3530559997133364547 ) ) ;
#15009 = CARTESIAN_POINT ( 'NONE',  ( -0.3392501089628018329, -0.1958661417322836440, -2.809691970307399700 ) ) ;
#15010 = CARTESIAN_POINT ( 'NONE',  ( 0.5052493438320215802, 0.2952755905511811885, 0.1292274648535926551 ) ) ;
#15011 =( BOUNDED_CURVE ( )  B_SPLINE_CURVE ( 2, ( #61297, #48253, #80279, #75187, #43164, #3655, #30135, #74363, #73949, #11209, #4058, #29725, #28901 ),
 .UNSPECIFIED., .F., .F. ) 
 B_SPLINE_CURVE_WITH_KNOTS ( ( 3, 2, 2, 2, 2, 2, 3 ),
 ( 0.6624999999999999778, 0.6666666666666666297, 0.6708333333333332815, 0.6750000000000000444, 0.6791666666666666963, 0.6833333333333333481, 0.6875000000000000000 ),
 .UNSPECIFIED. ) 
 CURVE ( )  GEOMETRIC_REPRESENTATION_ITEM ( )  RATIONAL_B_SPLINE_CURVE ( ( 1.000000000000000000, 0.9659258262890683122, 1.000000000000000000, 0.9659258262890683122, 1.000000000000000000, 0.9659258262890683122, 1.000000000000000000, 0.9659258262890683122, 1.000000000000000000, 0.9659258262890683122, 1.000000000000000000, 0.9659258262890683122, 1.000000000000000000 ) ) 
 REPRESENTATION_ITEM ( '' )  );
#15012 = CARTESIAN_POINT ( 'NONE',  ( -0.3392501089628017219, -0.1958661417322836718, -1.776902887139107490 ) ) ;
#15013 = CARTESIAN_POINT ( 'NONE',  ( -1.318897637795274802, 0.07958543189024085140, 0.2665933059059887866 ) ) ;
#15014 = ORIENTED_EDGE ( 'NONE', *, *, #1342, .F. ) ;
#15015 = CARTESIAN_POINT ( 'NONE',  ( -0.3949938075777411628, 0.1058382717557497937, -2.237532808398950301 ) ) ;
#15016 = ORIENTED_EDGE ( 'NONE', *, *, #42744, .T. ) ;
#15017 = CARTESIAN_POINT ( 'NONE',  ( -1.580526701345955409, 1.383198989551510216, 0.4486511340363580902 ) ) ;
#15018 = CARTESIAN_POINT ( 'NONE',  ( -1.148293963254592542, -0.6692913385826773087, -0.1292274648535924053 ) ) ;
#15019 = CARTESIAN_POINT ( 'NONE',  ( -1.200787401574802349, -0.5400638737290844871, 0.3530559997133364547 ) ) ;
#15020 = CARTESIAN_POINT ( 'NONE',  ( -0.1998031496062994683, 0.3460692066303958092, -0.8005249343832020470 ) ) ;
#15021 = CARTESIAN_POINT ( 'NONE',  ( -1.594488188976377563, -0.5400638737290844871, 0.3530559997133364547 ) ) ;
#15022 = CARTESIAN_POINT ( 'NONE',  ( -0.4724409448818898682, 5.785732909357575061E-17, -2.755905511811024056 ) ) ;
#15023 = CARTESIAN_POINT ( 'NONE',  ( -0.9711286089238838626, 0.2306618581243847221, -0.2411417322834647770 ) ) ;
#15024 = LINE ( 'NONE', #40680, #28369 ) ;
#15025 = CARTESIAN_POINT ( 'NONE',  ( -0.3392501089628019995, 0.1958661417322832277, -0.1108923884514436548 ) ) ;
#15026 = CARTESIAN_POINT ( 'NONE',  ( -0.06561679790026180015, -0.004921259842519576551, 0.3153832671262227771 ) ) ;
#15027 = CARTESIAN_POINT ( 'NONE',  ( -0.7152230971128602510, -0.08942795157528024563, -0.3641732283464568787 ) ) ;
#15028 = CARTESIAN_POINT ( 'NONE',  ( -1.325459317585300889, 0.05413385826771666132, 0.4176697321401328100 ) ) ;
#15029 = CARTESIAN_POINT ( 'NONE',  ( 1.115485564304462551, 0.05413385826771666132, 0.4176697321401328100 ) ) ;
#15030 = CARTESIAN_POINT ( 'NONE',  ( -0.8070866141732276899, 0.1660481256975883668, -0.3530559997133364547 ) ) ;
#15031 = CARTESIAN_POINT ( 'NONE',  ( 0.5314960629921395840, 2.748002881374839834, -3.856579543051779524 ) ) ;
#15032 = ORIENTED_EDGE ( 'NONE', *, *, #25885, .T. ) ;
#15033 = CARTESIAN_POINT ( 'NONE',  ( -1.522309711286088607, -0.6046776061558807314, 0.2411417322834647770 ) ) ;
#15034 = CARTESIAN_POINT ( 'NONE',  ( 0.7742782152230978099, -0.4281496062992124485, 0.4176697321401328655 ) ) ;
#15035 = CARTESIAN_POINT ( 'NONE',  ( -1.666666666666665853, -0.004921259842519870586, -0.3153832671262229437 ) ) ;
#15036 = CARTESIAN_POINT ( 'NONE',  ( -0.06038700950485487162, 1.070773487107445909, 0.2444607762650621019 ) ) ;
#15037 = CARTESIAN_POINT ( 'NONE',  ( -0.1265901696524986964, -0.4724409448818899238, -1.174540682414698001 ) ) ;
#15038 = CARTESIAN_POINT ( 'NONE',  ( 2.104898677616436231, 1.365902157108388248, -0.4425616331406706516 ) ) ;
#15039 = CARTESIAN_POINT ( 'NONE',  ( -0.3392501089628017219, -0.1958661417322836718, -0.8320209973753279753 ) ) ;
#15040 = CARTESIAN_POINT ( 'NONE',  ( 0.2867679344610366554, 0.2867679344610366554, -2.269685039370078705 ) ) ;
#15041 = CARTESIAN_POINT ( 'NONE',  ( -0.4790026246719152336, -0.05778040916215560624, -0.4822834645669293319 ) ) ;
#15042 = CARTESIAN_POINT ( 'NONE',  ( -1.377952755905511140, -0.5511811023622047445, 6.969142054262312111E-17 ) ) ;
#15043 = CARTESIAN_POINT ( 'NONE',  ( -0.3996062992125986590, 0.1070741851644051723, -0.2670603674540683037 ) ) ;
#15045 = CARTESIAN_POINT ( 'NONE',  ( -0.6955380577427815458, 0.009842519685039467087, 0.3409548833797002021 ) ) ;
#15044 = LINE ( 'NONE', #79860, #38237 ) ;
#15046 = CARTESIAN_POINT ( 'NONE',  ( -1.318897637795274802, -0.5400638737290845981, -0.3530559997133363437 ) ) ;
#15047 = CARTESIAN_POINT ( 'NONE',  ( -0.3018372703412066094, 0.05413385826771666132, 0.4176697321401328100 ) ) ;
#15048 = CARTESIAN_POINT ( 'NONE',  ( -0.3392501089628018329, -0.1958661417322836440, 0.1824340139445687625 ) ) ;
#15049 = CARTESIAN_POINT ( 'NONE',  ( 0.3871391076115492380, -0.08942795157528024563, -0.3641732283464568787 ) ) ;
#15050 = CARTESIAN_POINT ( 'NONE',  ( -0.04642319063763892389, -0.3917322834645671215, -0.003003439681892647057 ) ) ;
#15051 = CARTESIAN_POINT ( 'NONE',  ( 0.3805774278215230400, -0.3690944881889763329, 0.3153832671262228327 ) ) ;
#15052 = CARTESIAN_POINT ( 'NONE',  ( 0.8727034120734912248, -0.2845877964562161244, -0.3641732283464567121 ) ) ;
#15053 = CARTESIAN_POINT ( 'NONE',  ( 1.161417322834646271, 0.1660481256975883668, -0.3530559997133364547 ) ) ;
#15054 = CARTESIAN_POINT ( 'NONE',  ( 0.2493438320209980519, -0.004921259842519576551, 0.3153832671262227771 ) ) ;
#15055 = CARTESIAN_POINT ( 'NONE',  ( -0.2867679344610365999, 0.2867679344610364889, -2.059055118110236116 ) ) ;
#15056 = CARTESIAN_POINT ( 'NONE',  ( -1.148293963254592542, 0.2952755905511811885, 0.1292274648535926551 ) ) ;
#15057 = CARTESIAN_POINT ( 'NONE',  ( -0.03280839895013062252, -0.5511811023622046335, 0.09757992244046803654 ) ) ;
#15058 = CARTESIAN_POINT ( 'NONE',  ( -1.437007874015747477, 0.07958543189024071263, -0.2665933059059888421 ) ) ;
#15059 = CARTESIAN_POINT ( 'NONE',  ( -0.3458507752293906723, -0.3458507752293910609, -0.4507874015748031815 ) ) ;
#15060 = CARTESIAN_POINT ( 'NONE',  ( -1.122047244094487306, 0.07958543189024071263, -0.2665933059059888421 ) ) ;
#15061 = CARTESIAN_POINT ( 'NONE',  ( 0.4469741871781334752, 1.378378501333950679, -1.594259055605391939 ) ) ;
#15062 = CARTESIAN_POINT ( 'NONE',  ( 0.006561679790026889343, -0.3162353388693409650, -0.4822834645669289433 ) ) ;
#15063 = DIRECTION ( 'NONE',  ( 1.047444401652940007E-14, -0.000000000000000000, -1.000000000000000000 ) ) ;
#15064 = CARTESIAN_POINT ( 'NONE',  ( 0.4068241469816279987, -0.3690944881889765550, -0.3153832671262227771 ) ) ;
#15065 = CARTESIAN_POINT ( 'NONE',  ( -0.2165354330708654795, -0.4536011799217368745, -0.2665933059059886201 ) ) ;
#15066 = CARTESIAN_POINT ( 'NONE',  ( -0.3871391076115476282, -0.05778040916215522460, 0.4822834645669289988 ) ) ;
#15067 = CARTESIAN_POINT ( 'NONE',  ( -1.204164820379010514, 2.401574803149606474, 0.4915354330708645580 ) ) ;
#15068 = CARTESIAN_POINT ( 'NONE',  ( -1.181102362204723644, -0.1870078740157479769, 0.3641732283464567677 ) ) ;
#15069 = DIRECTION ( 'NONE',  ( 0.000000000000000000, 0.000000000000000000, 1.000000000000000000 ) ) ;
#15070 = CARTESIAN_POINT ( 'NONE',  ( 0.4330708661417329575, 0.2952755905511811885, 0.000000000000000000 ) ) ;
#15071 = ORIENTED_EDGE ( 'NONE', *, *, #3063, .F. ) ;
#15072 = CARTESIAN_POINT ( 'NONE',  ( 0.3996062992125986035, -0.1070741851644052972, -1.448162729658792669 ) ) ;
#15073 = CARTESIAN_POINT ( 'NONE',  ( 2.795275590551181910, 1.771653543307087242, 0.000000000000000000 ) ) ;
#15074 = CARTESIAN_POINT ( 'NONE',  ( -0.1509186351706028884, -0.08942795157527998196, 0.3641732283464567121 ) ) ;
#15075 = CARTESIAN_POINT ( 'NONE',  ( -1.463254593175852492, 0.2952755905511811885, 0.1292274648535926551 ) ) ;
#15076 = CARTESIAN_POINT ( 'NONE',  ( -1.469816272965878357, 0.1283753931104748280, 0.1820866141732283561 ) ) ;
#15077 = CARTESIAN_POINT ( 'NONE',  ( 1.496062992125985147, -0.1870078740157479769, 0.4822834645669291653 ) ) ;
#15078 = CARTESIAN_POINT ( 'NONE',  ( -0.5971128608923877978, 0.1771653543307087630, 0.09757992244046791164 ) ) ;
#15079 = CARTESIAN_POINT ( 'NONE',  ( 0.3460692066303959202, -0.1998031496062991630, -0.02427821522309713681 ) ) ;
#15080 = CARTESIAN_POINT ( 'NONE',  ( 0.8202099737532813073, 0.2952755905511811885, 0.1292274648535926551 ) ) ;
#15081 = CARTESIAN_POINT ( 'NONE',  ( 4.893765752498283924E-17, -0.3996062992125986035, -0.2362204724409449064 ) ) ;
#15082 = CARTESIAN_POINT ( 'NONE',  ( -0.1958661417322833942, -0.3392501089628018884, -2.424559998196537336 ) ) ;
#15083 = PLANE ( 'NONE',  #40519 ) ;
#15084 = ADVANCED_FACE ( 'NONE', ( #82934 ), #73586, .F. ) ;
#15085 = CARTESIAN_POINT ( 'NONE',  ( 1.482939632545932307, -0.004921259842519870586, -0.3153832671262229437 ) ) ;
#15086 = CARTESIAN_POINT ( 'NONE',  ( -1.318897637795274802, -0.5400638737290845981, -0.3530559997133363437 ) ) ;
#15087 = CARTESIAN_POINT ( 'NONE',  ( 1.312335958005249825, 0.2306618581243847221, -0.2411417322834647770 ) ) ;
#15088 = CARTESIAN_POINT ( 'NONE',  ( 0.3917322834645669549, 0.1049643490035304660, -2.571522309711286258 ) ) ;
#15089 = CARTESIAN_POINT ( 'NONE',  ( 1.279527559055118724, -0.4536011799217368745, -0.2665933059059886201 ) ) ;
#15090 = EDGE_CURVE ( 'NONE', #53614, #19971, #15477, .T. ) ;
#15091 = CARTESIAN_POINT ( 'NONE',  ( -0.01312335958005186876, 0.05413385826771626580, -0.4176697321401330321 ) ) ;
#15092 = CARTESIAN_POINT ( 'NONE',  ( -0.3871391076115476282, -0.05778040916215522460, 0.4822834645669289988 ) ) ;
#15093 = CARTESIAN_POINT ( 'NONE',  ( 0.000000000000000000, 2.165354330708661568, 0.000000000000000000 ) ) ;
#15094 = CARTESIAN_POINT ( 'NONE',  ( 1.586052503253845281, 0.7480314960629931287, -0.1653254495020588799 ) ) ;
#15095 = CARTESIAN_POINT ( 'NONE',  ( 0.3346456692913390985, 0.07958543189024085140, 0.2665933059059887866 ) ) ;
#15096 = ORIENTED_EDGE ( 'NONE', *, *, #75806, .T. ) ;
#15097 = CARTESIAN_POINT ( 'NONE',  ( 0.1958661417322834775, 0.3392501089628018884, -0.4560560611886632087 ) ) ;
#15098 = VERTEX_POINT ( 'NONE', #33260 ) ;
#15099 = CARTESIAN_POINT ( 'NONE',  ( -0.4133858267716528645, 0.1660481256975883668, -0.3530559997133364547 ) ) ;
#15100 = PRODUCT_DEFINITION_SHAPE ( 'NONE', 'NONE',  #40864 ) ;
#15101 = CARTESIAN_POINT ( 'NONE',  ( 1.502624671916010790, -0.3162353388693409650, -0.4822834645669289433 ) ) ;
#15102 = CARTESIAN_POINT ( 'NONE',  ( 0.1181102362204730916, 0.2952755905511811885, 0.000000000000000000 ) ) ;
#15103 = CARTESIAN_POINT ( 'NONE',  ( -0.3740157480314953431, 0.07958543189024085140, 0.2665933059059887866 ) ) ;
#15104 = CARTESIAN_POINT ( 'NONE',  ( 1.213910761154856299, 0.2952755905511811885, 0.1292274648535926551 ) ) ;
#15105 = CARTESIAN_POINT ( 'NONE',  ( -1.108923884514435132, -0.05778040916215560624, -0.4822834645669293319 ) ) ;
#15106 = CARTESIAN_POINT ( 'NONE',  ( 0.1968503937007881344, 0.2952755905511811885, 0.000000000000000000 ) ) ;
#15107 = CARTESIAN_POINT ( 'NONE',  ( -0.9973753280839886548, -0.6046776061558809534, -0.2411417322834644161 ) ) ;
#15108 = CARTESIAN_POINT ( 'NONE',  ( 1.128608923884514947, 0.2306618581243848609, 0.2411417322834645549 ) ) ;
#15109 = CONICAL_SURFACE ( 'NONE', #24451, 1.968503937007874072, 0.7853981633974500554 ) ;
#15110 = CARTESIAN_POINT ( 'NONE',  ( 0.9973753280839902091, 0.2306618581243847221, -0.2411417322834647770 ) ) ;
#15111 = CARTESIAN_POINT ( 'NONE',  ( 1.227034120734908917, 0.2952755905511810774, -0.1292274648535930714 ) ) ;
#15112 = ADVANCED_FACE ( 'NONE', ( #18951 ), #66858, .T. ) ;
#15113 = CARTESIAN_POINT ( 'NONE',  ( -0.3392501089628019995, 0.1958661417322832277, -0.8057742782152230721 ) ) ;
#15114 = CARTESIAN_POINT ( 'NONE',  ( 0.06561679790026316017, -0.3690944881889763329, 0.3153832671262228327 ) ) ;
#15115 = ORIENTED_EDGE ( 'NONE', *, *, #58440, .T. ) ;
#15116 = CARTESIAN_POINT ( 'NONE',  ( -0.1058382717557503211, 0.3949938075777409408, -1.108923884514435798 ) ) ;
#15117 = ORIENTED_EDGE ( 'NONE', *, *, #73492, .T. ) ;
#15118 = CARTESIAN_POINT ( 'NONE',  ( -0.9776902887139098386, -0.5511811023622046335, 0.09757992244046803654 ) ) ;
#15119 = CARTESIAN_POINT ( 'NONE',  ( -0.07874015748031421014, -0.1870078740157479769, 0.4822834645669291653 ) ) ;
#15120 = CARTESIAN_POINT ( 'NONE',  ( 1.614173228346457378, 0.5038684218300978346, -0.1372047244094476148 ) ) ;
#15121 = CARTESIAN_POINT ( 'NONE',  ( -0.07874015748031421014, -0.1870078740157480879, -0.4822834645669291653 ) ) ;
#15122 = CARTESIAN_POINT ( 'NONE',  ( -0.4790026246719154557, -0.3162353388693405765, 0.4822834645669290543 ) ) ;
#15123 = CARTESIAN_POINT ( 'NONE',  ( -0.9448818897637790704, -0.1870078740157480879, -0.4822834645669291653 ) ) ;
#15124 = CARTESIAN_POINT ( 'NONE',  ( -1.614173228346456268, -0.6692913385826771977, 8.415575281601705876E-17 ) ) ;
#15125 = CARTESIAN_POINT ( 'NONE',  ( 1.351706036745407680, -0.004921259842519576551, 0.3153832671262227771 ) ) ;
#15126 = CARTESIAN_POINT ( 'NONE',  ( -2.630268417803964809, 1.724409448818898127, -0.4359958488159723089 ) ) ;
#15127 = CARTESIAN_POINT ( 'NONE',  ( 0.3412073490813655186, 0.1283753931104748280, 0.1820866141732283561 ) ) ;
#15128 = CARTESIAN_POINT ( 'NONE',  ( 0.006561679790026889343, -0.3162353388693409650, -0.4822834645669289433 ) ) ;
#15129 = CARTESIAN_POINT ( 'NONE',  ( 0.4068241469816281097, 0.05413385826771666132, 0.4176697321401328100 ) ) ;
#15130 = ORIENTED_EDGE ( 'NONE', *, *, #15427, .T. ) ;
#15131 = CARTESIAN_POINT ( 'NONE',  ( 0.3996062992125986035, 2.446882876249141962E-17, -1.692913385826771533 ) ) ;
#15132 = CARTESIAN_POINT ( 'NONE',  ( -0.6102362204724400829, 0.1012011053420777407, 0.2882089793578257453 ) ) ;
#15133 = CARTESIAN_POINT ( 'NONE',  ( -0.1998031496062994405, 0.3460692066303957537, -1.192257217847769057 ) ) ;
#15134 = CARTESIAN_POINT ( 'NONE',  ( 0.2925321140481932369, 0.2925321140481932369, -0.5295275590551181688 ) ) ;
#15135 = CARTESIAN_POINT ( 'NONE',  ( -0.7414698162729651543, 0.2952755905511810774, -0.1292274648535930714 ) ) ;
#15136 = CARTESIAN_POINT ( 'NONE',  ( 0.1265901696524989462, 0.4724409448818897572, -0.1509186351706036378 ) ) ;
#15137 = CARTESIAN_POINT ( 'NONE',  ( -0.2867679344610365999, 0.2867679344610364889, -2.309055118110235671 ) ) ;
#15138 = CARTESIAN_POINT ( 'NONE',  ( -1.469816272965878357, 0.1283753931104748280, 0.1820866141732283561 ) ) ;
#15139 = CARTESIAN_POINT ( 'NONE',  ( 0.7414698162729663755, -0.6692913385826773087, -0.1292274648535924053 ) ) ;
#15140 = CARTESIAN_POINT ( 'NONE',  ( 1.023622047244095334, -0.1870078740157479769, 0.4822834645669291653 ) ) ;
#15141 = CARTESIAN_POINT ( 'NONE',  ( -0.05249343832020911260, 0.1283753931104748280, 0.1820866141732283561 ) ) ;
#15142 = CARTESIAN_POINT ( 'NONE',  ( -0.1115485564304456306, 0.2952755905511810774, -0.1292274648535930714 ) ) ;
#15143 = CARTESIAN_POINT ( 'NONE',  ( -0.4091458600556402980, -0.2362204724409451284, -2.019028871391076230 ) ) ;
#15144 = CARTESIAN_POINT ( 'NONE',  ( -0.03937007874015669567, 0.1771653543307087630, 0.000000000000000000 ) ) ;
#15145 = CARTESIAN_POINT ( 'NONE',  ( -0.01312335958005186876, -0.4281496062992124485, 0.4176697321401328655 ) ) ;
#15146 = CARTESIAN_POINT ( 'NONE',  ( -0.3949938075777411073, 0.1058382717557497660, -1.999343832020997747 ) ) ;
#15147 = CARTESIAN_POINT ( 'NONE',  ( 1.555118110236221041, -0.4536011799217367080, 0.2665933059059888421 ) ) ;
#15148 = CARTESIAN_POINT ( 'NONE',  ( 0.1115485564304467270, -0.5511811023622048555, -0.09757992244046775898 ) ) ;
#15149 = CARTESIAN_POINT ( 'NONE',  ( 1.397637795275591177, 0.07958543189024071263, -0.2665933059059888421 ) ) ;
#15150 = CARTESIAN_POINT ( 'NONE',  ( -1.358267716535432434, 0.1660481256975883668, -0.3530559997133364547 ) ) ;
#15151 = CARTESIAN_POINT ( 'NONE',  ( -0.5774278215223089816, -0.5023911411419708095, 0.1820866141732285504 ) ) ;
#15152 = CARTESIAN_POINT ( 'NONE',  ( -1.035555078613324964, 4.688555745438257773E-15, -0.3627989612356130045 ) ) ;
#15153 = CARTESIAN_POINT ( 'NONE',  ( -0.5577427821522301654, -0.05778040916215560624, -0.4822834645669293319 ) ) ;
#15154 = CARTESIAN_POINT ( 'NONE',  ( -0.7611548556430438595, -0.6046776061558809534, -0.2411417322834644161 ) ) ;
#15155 = CARTESIAN_POINT ( 'NONE',  ( 0.05249343832021075018, -0.6046776061558807314, 0.2411417322834647770 ) ) ;
#15156 = CARTESIAN_POINT ( 'NONE',  ( -0.1998031496062994405, 0.3460692066303957537, -2.452099737532808188 ) ) ;
#15157 = CARTESIAN_POINT ( 'NONE',  ( -0.3392501089628018329, -0.1958661417322836440, -2.179770710464879802 ) ) ;
#15158 = CARTESIAN_POINT ( 'NONE',  ( -0.5314960629921123836, 2.729333734409945311, -3.881246834694717762 ) ) ;
#15159 = CARTESIAN_POINT ( 'NONE',  ( 0.9317585301837276734, -0.004921259842519870586, -0.3153832671262229437 ) ) ;
#15160 = EDGE_CURVE ( 'NONE', #64866, #59983, #26091, .T. ) ;
#15161 = CARTESIAN_POINT ( 'NONE',  ( 0.9514435695538062676, -0.05778040916215522460, 0.4822834645669289988 ) ) ;
#15162 = CARTESIAN_POINT ( 'NONE',  ( -1.443569553805773564, -0.5023911411419708095, 0.1820866141732285504 ) ) ;
#15163 = CARTESIAN_POINT ( 'NONE',  ( 1.207349081364829990, 0.2306618581243848609, 0.2411417322834645549 ) ) ;
#15164 = CARTESIAN_POINT ( 'NONE',  ( -1.154855643044618851, -0.5023911411419708095, -0.1820866141732282451 ) ) ;
#15165 = VECTOR ( 'NONE', #29234, 39.37007874015748143 ) ;
#15166 = CARTESIAN_POINT ( 'NONE',  ( -0.7020997375328076329, -0.3162353388693409650, -0.4822834645669289433 ) ) ;
#15167 = CARTESIAN_POINT ( 'NONE',  ( -0.06561679790026180015, -0.004921259842519576551, 0.3153832671262227771 ) ) ;
#15168 = CARTESIAN_POINT ( 'NONE',  ( -0.8772393894194419062, 5.410171027439680070E-15, -0.3954985857520040282 ) ) ;
#15169 = CARTESIAN_POINT ( 'NONE',  ( 0.8333333333333340365, 0.1771653543307087075, -0.09757992244046823083 ) ) ;
#15170 = EDGE_CURVE ( 'NONE', #18898, #60349, #399, .T. ) ;
#15171 = CARTESIAN_POINT ( 'NONE',  ( 0.4068241469816281097, 0.05413385826771666132, 0.4176697321401328100 ) ) ;
#15172 = CARTESIAN_POINT ( 'NONE',  ( 0.2925321140481932369, -0.2925321140481931814, -0.1751968503937007537 ) ) ;
#15173 = CARTESIAN_POINT ( 'NONE',  ( -0.8136482939632537770, -0.6046776061558807314, 0.2411417322834647770 ) ) ;
#15174 = CARTESIAN_POINT ( 'NONE',  ( 0.1958661417322834775, 0.3392501089628018884, -1.331364829396325611 ) ) ;
#15175 = CARTESIAN_POINT ( 'NONE',  ( 1.227034120734908917, -0.5511811023622046335, 0.09757992244046803654 ) ) ;
#15176 = CARTESIAN_POINT ( 'NONE',  ( 0.6233595800524942554, -0.05778040916215560624, -0.4822834645669293319 ) ) ;
#15177 = CARTESIAN_POINT ( 'NONE',  ( -0.09842519685039295696, -0.5400638737290844871, 0.3530559997133364547 ) ) ;
#15178 = CARTESIAN_POINT ( 'NONE',  ( -0.1837270341207340729, 0.1283753931104746893, -0.1820866141732285504 ) ) ;
#15179 = LINE ( 'NONE', #27370, #61554 ) ;
#15180 = CARTESIAN_POINT ( 'NONE',  ( 0.08530183727034192087, -0.08942795157527998196, 0.3641732283464567121 ) ) ;
#15181 = CARTESIAN_POINT ( 'NONE',  ( 0.4527559055118117182, 0.1660481256975883668, -0.3530559997133364547 ) ) ;
#15182 = CARTESIAN_POINT ( 'NONE',  ( -0.6496062992125976043, -0.4536011799217367080, 0.2665933059059888421 ) ) ;
#15183 = CARTESIAN_POINT ( 'NONE',  ( 0.3460692066303958092, 0.1998031496062993018, -1.152887139107611425 ) ) ;
#15184 = CARTESIAN_POINT ( 'NONE',  ( -1.220472440944881054, -0.6692913385826771977, 8.415575281601705876E-17 ) ) ;
#15185 = CARTESIAN_POINT ( 'NONE',  ( 0.8554425558739519042, 1.722984403643211298E-16, -0.4118484887281974594 ) ) ;
#15186 = VERTEX_POINT ( 'NONE', #51751 ) ;
#15187 = CARTESIAN_POINT ( 'NONE',  ( -1.082677165354329896, 0.07958543189024085140, 0.2665933059059887866 ) ) ;
#15188 = CARTESIAN_POINT ( 'NONE',  ( -0.2230971128608915943, -0.4281496062992127816, -0.4176697321401328100 ) ) ;
#15189 = CARTESIAN_POINT ( 'NONE',  ( 0.3974711515625343194, 0.004548682155565822449, -1.220472440944882164 ) ) ;
#15190 = CARTESIAN_POINT ( 'NONE',  ( -0.8727034120734901146, -0.3162353388693405765, 0.4822834645669290543 ) ) ;
#15191 = CARTESIAN_POINT ( 'NONE',  ( 0.000000000000000000, 0.000000000000000000, 6.062992125984251857 ) ) ;
#15192 = CARTESIAN_POINT ( 'NONE',  ( 0.4935044252197983150, 1.488513638086841118, -0.5309055118110237448 ) ) ;
#15193 = CARTESIAN_POINT ( 'NONE',  ( 0.6824146981627303710, -0.6046776061558807314, 0.2411417322834647770 ) ) ;
#15194 = CARTESIAN_POINT ( 'NONE',  ( -0.2493438320209966919, 0.009842519685039144428, -0.3409548833797004797 ) ) ;
#15195 = CARTESIAN_POINT ( 'NONE',  ( 1.601049868766404982, 0.2306618581243848609, 0.2411417322834645549 ) ) ;
#15196 = CARTESIAN_POINT ( 'NONE',  ( 0.2362173824511233644, -0.1771694743175191433, 5.690029434716978862 ) ) ;
#15197 = CARTESIAN_POINT ( 'NONE',  ( -1.358267716535432434, 0.1660481256975883668, -0.3530559997133364547 ) ) ;
#15198 = CARTESIAN_POINT ( 'NONE',  ( 0.3460692066303959202, 0.1998031496062993295, -0.2887139107611548794 ) ) ;
#15199 = ORIENTED_EDGE ( 'NONE', *, *, #30053, .T. ) ;
#15200 = CARTESIAN_POINT ( 'NONE',  ( -0.4265091863517051496, -0.5511811023622046335, 0.09757992244046803654 ) ) ;
#15201 = CARTESIAN_POINT ( 'NONE',  ( -0.1958661417322836718, 0.3392501089628017219, -2.052493438320210029 ) ) ;
#15202 = ORIENTED_EDGE ( 'NONE', *, *, #15589, .T. ) ;
#15203 = CARTESIAN_POINT ( 'NONE',  ( 0.9120734908136489683, -0.6692913385826771977, 0.1292274648535927661 ) ) ;
#15204 = CARTESIAN_POINT ( 'NONE',  ( 0.1837270341207354329, 0.2306618581243848609, 0.2411417322834645549 ) ) ;
#15205 = CARTESIAN_POINT ( 'NONE',  ( -0.8661417322834640276, -0.1870078740157479769, 0.4822834645669291653 ) ) ;
#15206 = CARTESIAN_POINT ( 'NONE',  ( 1.653543307086614789, -0.1870078740157479769, 0.4822834645669291653 ) ) ;
#15207 = AXIS2_PLACEMENT_3D ( 'NONE', #7173, #28195, #79566 ) ;
#15208 = CARTESIAN_POINT ( 'NONE',  ( -0.6824146981627288167, 0.1283753931104748280, 0.1820866141732283561 ) ) ;
#15209 = CARTESIAN_POINT ( 'NONE',  ( -0.4724973665168013537, 1.580780302271974636, -2.558933905385162078 ) ) ;
#15210 = CARTESIAN_POINT ( 'NONE',  ( 0.5052493438320218022, -0.6692913385826773087, -0.1292274648535924053 ) ) ;
#15211 = CARTESIAN_POINT ( 'NONE',  ( 0.5052493438320215802, 0.1771653543307087630, 0.09757992244046791164 ) ) ;
#15212 = CARTESIAN_POINT ( 'NONE',  ( -1.017060367454067249, -0.05778040916215522460, 0.4822834645669289988 ) ) ;
#15213 = CARTESIAN_POINT ( 'NONE',  ( -0.1958661417322834497, -0.3392501089628018884, -1.405492495241783102 ) ) ;
#15214 = CARTESIAN_POINT ( 'NONE',  ( -1.404199475065615932, -0.4281496062992127816, -0.4176697321401328100 ) ) ;
#15215 = CARTESIAN_POINT ( 'NONE',  ( -1.686351706036744558, 0.1771653543307087075, -0.09757992244046823083 ) ) ;
#15216 = CARTESIAN_POINT ( 'NONE',  ( 1.489501312335958172, -0.3162353388693405765, 0.4822834645669290543 ) ) ;
#15217 = CARTESIAN_POINT ( 'NONE',  ( 1.220472440944882608, 0.1771653543307087630, 0.000000000000000000 ) ) ;
#15218 = VERTEX_POINT ( 'NONE', #71137 ) ;
#15219 = CARTESIAN_POINT ( 'NONE',  ( -0.1958661417322836995, 0.3392501089628017219, -2.844507504758217120 ) ) ;
#15220 = CARTESIAN_POINT ( 'NONE',  ( -0.4658792650918627265, -0.3162353388693409650, -0.4822834645669289433 ) ) ;
#15221 = VERTEX_POINT ( 'NONE', #65679 ) ;
#15222 = CARTESIAN_POINT ( 'NONE',  ( 0.3937007874015754361, -0.1870078740157480601, -0.3641732283464567677 ) ) ;
#15223 = CARTESIAN_POINT ( 'NONE',  ( -1.305774278215222184, -0.6692913385826773087, -0.1292274648535924053 ) ) ;
#15224 = CARTESIAN_POINT ( 'NONE',  ( 0.8595800524934390507, -0.05778040916215560624, -0.4822834645669293319 ) ) ;
#15225 = CARTESIAN_POINT ( 'NONE',  ( 0.7480314960629927956, -0.6692913385826771977, 8.415575281601705876E-17 ) ) ;
#15226 = CARTESIAN_POINT ( 'NONE',  ( 0.3280839895013130669, 0.05413385826771666132, 0.4176697321401328100 ) ) ;
#15227 = VECTOR ( 'NONE', #45470, 39.37007874015748143 ) ;
#15228 = CARTESIAN_POINT ( 'NONE',  ( -0.4527559055118102749, -0.5400638737290845981, -0.3530559997133363437 ) ) ;
#15229 = CARTESIAN_POINT ( 'NONE',  ( 4.797336870675656522E-17, -0.3917322834645670104, -2.210629921259842590 ) ) ;
#15230 = CARTESIAN_POINT ( 'NONE',  ( 1.535433070866142335, -0.5511811023622047445, 6.969142054262312111E-17 ) ) ;
#15231 = CARTESIAN_POINT ( 'NONE',  ( -0.7414698162729651543, -0.6692913385826771977, 0.1292274648535927661 ) ) ;
#15232 = CARTESIAN_POINT ( 'NONE',  ( -0.3346456692913377662, 0.07958543189024071263, -0.2665933059059888421 ) ) ;
#15233 = CARTESIAN_POINT ( 'NONE',  ( 1.167979002624672580, -0.4281496062992124485, 0.4176697321401328655 ) ) ;
#15234 = CARTESIAN_POINT ( 'NONE',  ( 1.463254593175853824, -0.6692913385826771977, 0.1292274648535927661 ) ) ;
#15235 = CARTESIAN_POINT ( 'NONE',  ( -0.3477690288713905509, -0.6692913385826771977, 0.1292274648535927661 ) ) ;
#15236 = CARTESIAN_POINT ( 'NONE',  ( -0.1070741851644056997, 0.3996062992125984925, -0.08333333333333335646 ) ) ;
#15237 = CARTESIAN_POINT ( 'NONE',  ( 0.7874015748031503170, -0.1870078740157479769, 0.4822834645669291653 ) ) ;
#15238 = CARTESIAN_POINT ( 'NONE',  ( 0.3460692066303959202, 0.1998031496062993295, -1.706036745406824151 ) ) ;
#15239 = DIRECTION ( 'NONE',  ( 1.000000000000000000, 3.096699300667737464E-16, -1.692413147294446216E-16 ) ) ;
#15240 = CARTESIAN_POINT ( 'NONE',  ( -0.1181102362204717315, -0.6692913385826771977, 8.415575281601705876E-17 ) ) ;
#15241 = CARTESIAN_POINT ( 'NONE',  ( -1.279527559055116948, 0.07958543189024071263, -0.2665933059059888421 ) ) ;
#15243 = CARTESIAN_POINT ( 'NONE',  ( 0.4848199769444413998, 1.968301573707852192, -0.4917377963708869926 ) ) ;
#15242 = CARTESIAN_POINT ( 'NONE',  ( 1.017060367454068803, -0.2845877964562159024, 0.3641732283464567677 ) ) ;
#15244 = CARTESIAN_POINT ( 'NONE',  ( -0.3458507752293909498, 0.3458507752293907833, -0.7263779527559056648 ) ) ;
#15245 = CARTESIAN_POINT ( 'NONE',  ( 1.279527559055118724, -0.4536011799217368745, -0.2665933059059886201 ) ) ;
#15246 = EDGE_CURVE ( 'NONE', #47884, #66895, #3648, .T. ) ;
#15247 = CARTESIAN_POINT ( 'NONE',  ( 1.338582677165355062, -0.1870078740157480879, -0.4822834645669291653 ) ) ;
#15248 = CARTESIAN_POINT ( 'NONE',  ( -0.3949938075777408852, -0.1058382717557502933, -0.2801837270341207553 ) ) ;
#15249 = CARTESIAN_POINT ( 'NONE',  ( -0.3280839895013117347, -0.4281496062992124485, 0.4176697321401328655 ) ) ;
#15250 = CARTESIAN_POINT ( 'NONE',  ( 0.5314960629921346991, 2.755905511811024056, -2.503252890251014495 ) ) ;
#15251 = CARTESIAN_POINT ( 'NONE',  ( 1.423884514435696191, -0.08942795157527998196, 0.3641732283464567121 ) ) ;
#15252 = CARTESIAN_POINT ( 'NONE',  ( -0.05905511811023545637, -0.5400638737290845981, -0.3530559997133363437 ) ) ;
#15253 = EDGE_CURVE ( 'NONE', #14101, #28644, #19367, .T. ) ;
#15254 = CARTESIAN_POINT ( 'NONE',  ( -9.674558042662122972E-17, 0.3949938075777409963, -0.3917322834645669549 ) ) ;
#15255 = CARTESIAN_POINT ( 'NONE',  ( 1.135170603674541256, -0.6692913385826773087, -0.1292274648535924053 ) ) ;
#15256 = CARTESIAN_POINT ( 'NONE',  ( 0.3805774278215230400, 0.05413385826771626580, -0.4176697321401330321 ) ) ;
#15257 = CARTESIAN_POINT ( 'NONE',  ( 0.6824146981627303710, -0.5023911411419708095, 0.1820866141732285504 ) ) ;
#15258 = CARTESIAN_POINT ( 'NONE',  ( -0.2898037569319622531, 1.161479134785472045, -1.084046850253320926 ) ) ;
#15259 = CARTESIAN_POINT ( 'NONE',  ( 0.3543307086614181922, -0.5511811023622047445, 6.969142054262312111E-17 ) ) ;
#15260 = CARTESIAN_POINT ( 'NONE',  ( 5.785732909357575061E-17, -0.4724409448818898682, -2.755905511811023612 ) ) ;
#15261 = CARTESIAN_POINT ( 'NONE',  ( -0.2925321140481932369, 0.2925321140481931259, -1.198818897637795367 ) ) ;
#15262 = CARTESIAN_POINT ( 'NONE',  ( 0.6627296587926517768, -0.6692913385826773087, -0.1292274648535924053 ) ) ;
#15263 = CARTESIAN_POINT ( 'NONE',  ( 0.3917322834645670104, -0.1049643490035303411, -0.8910761154855640909 ) ) ;
#15264 = CARTESIAN_POINT ( 'NONE',  ( 0.9332960234133783617, 0.02791078216816427274, -0.4328096321851894190 ) ) ;
#15265 = DIRECTION ( 'NONE',  ( -0.5653208194167064216, 0.6006868920394703437, -0.5653208194167143041 ) ) ;
#15266 = CARTESIAN_POINT ( 'NONE',  ( 0.2296587926509192634, -0.08942795157528024563, -0.3641732283464568787 ) ) ;
#15267 = CARTESIAN_POINT ( 'NONE',  ( -0.08530183727034056085, -0.3162353388693405765, 0.4822834645669290543 ) ) ;
#15268 = CARTESIAN_POINT ( 'NONE',  ( 1.541994750656168645, 0.1771653543307087075, -0.09757992244046823083 ) ) ;
#15269 = CARTESIAN_POINT ( 'NONE',  ( -1.450131233595799651, -0.5511811023622046335, 0.09757992244046803654 ) ) ;
#15270 = CARTESIAN_POINT ( 'NONE',  ( -1.036745406824146176, 0.05413385826771626580, -0.4176697321401330321 ) ) ;
#15271 = AXIS2_PLACEMENT_3D ( 'NONE', #47858, #9992, #53348 ) ;
#15272 = CARTESIAN_POINT ( 'NONE',  ( 0.6824146981627303710, -0.6046776061558807314, 0.2411417322834647770 ) ) ;
#15273 = CARTESIAN_POINT ( 'NONE',  ( 1.509186351706037543, 0.05413385826771666132, 0.4176697321401328100 ) ) ;
#15274 = PLANE ( 'NONE',  #81422 ) ;
#15275 = CARTESIAN_POINT ( 'NONE',  ( 0.6102362204724416372, -0.5400638737290844871, 0.3530559997133364547 ) ) ;
#15276 = CARTESIAN_POINT ( 'NONE',  ( 0.4724409448818898682, 2.892866454678787531E-17, -2.872047244094488416 ) ) ;
#15277 = DIRECTION ( 'NONE',  ( 0.000000000000000000, 0.000000000000000000, -1.000000000000000000 ) ) ;
#15278 = CARTESIAN_POINT ( 'NONE',  ( 1.003937007874016407, -0.5400638737290844871, 0.3530559997133364547 ) ) ;
#15279 = CARTESIAN_POINT ( 'NONE',  ( -1.437007874015747477, -0.4536011799217367080, 0.2665933059059888421 ) ) ;
#15280 = CARTESIAN_POINT ( 'NONE',  ( 1.272965879265092637, -0.3690944881889765550, -0.3153832671262227771 ) ) ;
#15281 = CARTESIAN_POINT ( 'NONE',  ( 1.515748031496063408, 0.1660481256975885056, 0.3530559997133364547 ) ) ;
#15282 = CARTESIAN_POINT ( 'NONE',  ( -0.8267716535433065062, 0.1771653543307087630, 0.000000000000000000 ) ) ;
#15283 = CARTESIAN_POINT ( 'NONE',  ( 1.515748031496063186, -0.5400638737290845981, -0.3530559997133363437 ) ) ;
#15284 = CARTESIAN_POINT ( 'NONE',  ( 0.7020997375328090762, -0.08942795157528024563, -0.3641732283464568787 ) ) ;
#15285 = CIRCLE ( 'NONE', #47523, 3.937007874015748143 ) ;
#15286 = CARTESIAN_POINT ( 'NONE',  ( 0.1968503937007881344, -0.6692913385826771977, 8.415575281601705876E-17 ) ) ;
#15287 = CARTESIAN_POINT ( 'NONE',  ( 1.010498687664042716, 0.05413385826771626580, -0.4176697321401330321 ) ) ;
#15288 = CARTESIAN_POINT ( 'NONE',  ( -0.04593175853018302557, 0.2952755905511811885, 0.1292274648535926551 ) ) ;
#15289 = CARTESIAN_POINT ( 'NONE',  ( -0.05905511811023545637, -0.4536011799217368745, -0.2665933059059886201 ) ) ;
#15290 = CARTESIAN_POINT ( 'NONE',  ( 1.246719160104987623, -0.4281496062992124485, 0.4176697321401328655 ) ) ;
#15291 = CARTESIAN_POINT ( 'NONE',  ( -1.581364829396324945, -0.05778040916215560624, -0.4822834645669293319 ) ) ;
#15292 = CARTESIAN_POINT ( 'NONE',  ( -1.122047244094487306, -0.5400638737290844871, 0.3530559997133364547 ) ) ;
#15293 = CARTESIAN_POINT ( 'NONE',  ( -0.3996062992125985480, -0.1070741851644057135, -0.8333333333333332593 ) ) ;
#15294 = CARTESIAN_POINT ( 'NONE',  ( -1.213910761154854967, 0.2066929133858267098, -0.1054918080437494132 ) ) ;
#15295 = CARTESIAN_POINT ( 'NONE',  ( -0.9251968503937002541, -0.5400638737290845981, -0.3530559997133363437 ) ) ;
#15296 = CARTESIAN_POINT ( 'NONE',  ( -0.03280839895013062252, -0.6692913385826771977, 0.1292274648535927661 ) ) ;
#15297 = CARTESIAN_POINT ( 'NONE',  ( 0.4091458600556403535, 0.2362204724409449896, -0.1312335958005249326 ) ) ;
#15298 = CARTESIAN_POINT ( 'NONE',  ( 0.3949938075777411073, -0.1058382717557499464, -2.316272965879265122 ) ) ;
#15299 = ORIENTED_EDGE ( 'NONE', *, *, #45555, .T. ) ;
#15300 = CARTESIAN_POINT ( 'NONE',  ( -0.3392501089628017219, -0.1958661417322836718, -0.9895013123359579499 ) ) ;
#15301 = CARTESIAN_POINT ( 'NONE',  ( 1.227034120734908917, -0.6692913385826771977, 0.1292274648535927661 ) ) ;
#15302 = LINE ( 'NONE', #42194, #31850 ) ;
#15303 = CARTESIAN_POINT ( 'NONE',  ( -1.509186351706035767, -0.004921259842519870586, -0.3153832671262229437 ) ) ;
#15304 = CARTESIAN_POINT ( 'NONE',  ( 1.614173228346457378, -0.6692913385826771977, 8.415575281601705876E-17 ) ) ;
#15305 = CARTESIAN_POINT ( 'NONE',  ( 1.561679790026247350, -0.3690944881889763329, 0.3153832671262228327 ) ) ;
#15306 = CARTESIAN_POINT ( 'NONE',  ( -0.1049643490035301746, -0.3917322834645670659, -0.4671722852680298410 ) ) ;
#15307 = CARTESIAN_POINT ( 'NONE',  ( 0.2099737532808405305, -0.6046776061558807314, 0.2411417322834647770 ) ) ;
#15308 = CARTESIAN_POINT ( 'NONE',  ( -0.5774278215223089816, 0.1283753931104746893, -0.1820866141732285504 ) ) ;
#15309 = CARTESIAN_POINT ( 'NONE',  ( 0.6692913385826777528, 0.2952755905511811885, 0.000000000000000000 ) ) ;
#15310 = CARTESIAN_POINT ( 'NONE',  ( 0.5183727034120741983, 0.2952755905511810774, -0.1292274648535930714 ) ) ;
#15311 = CARTESIAN_POINT ( 'NONE',  ( 0.1539941091832136288, 1.088406432939548640, 1.111532584200361606 ) ) ;
#15312 = CARTESIAN_POINT ( 'NONE',  ( 0.3458507752293908943, 0.3458507752293908943, -1.082677165354330562 ) ) ;
#15313 = CARTESIAN_POINT ( 'NONE',  ( 0.1958661417322836718, -0.3392501089628017219, -1.663405142553492810 ) ) ;
#15314 = CARTESIAN_POINT ( 'NONE',  ( 1.410761154855643795, -0.05778040916215560624, -0.4822834645669293319 ) ) ;
#15315 = CARTESIAN_POINT ( 'NONE',  ( -0.02624671916010428221, -0.6046776061558807314, 0.2411417322834647770 ) ) ;
#15316 = CARTESIAN_POINT ( 'NONE',  ( -0.8858267716535425107, -0.5400638737290844871, 0.3530559997133364547 ) ) ;
#15317 = CARTESIAN_POINT ( 'NONE',  ( -1.587926509186350810, 0.05413385826771626580, -0.4176697321401330321 ) ) ;
#15318 = CARTESIAN_POINT ( 'NONE',  ( 0.7217847769028878924, 0.05413385826771666132, 0.4176697321401328100 ) ) ;
#15319 = CARTESIAN_POINT ( 'NONE',  ( 0.3917322834645669549, 0.1049643490035304660, -0.6817585301837268963 ) ) ;
#15320 = CARTESIAN_POINT ( 'NONE',  ( -0.3477690288713905509, -0.6692913385826771977, 0.1292274648535927661 ) ) ;
#15321 = CARTESIAN_POINT ( 'NONE',  ( 0.4790026246719168435, -0.3162353388693409650, -0.4822834645669289433 ) ) ;
#15322 = CARTESIAN_POINT ( 'NONE',  ( -0.03280839895013062252, 0.2952755905511810774, -0.1292274648535930714 ) ) ;
#15323 = VECTOR ( 'NONE', #9937, 39.37007874015749564 ) ;
#15324 = CARTESIAN_POINT ( 'NONE',  ( 0.7152230971128616943, -0.08942795157527998196, 0.3641732283464567121 ) ) ;
#15325 = CARTESIAN_POINT ( 'NONE',  ( -1.535433070866141225, 0.2952755905511811885, 0.000000000000000000 ) ) ;
#15326 = CARTESIAN_POINT ( 'NONE',  ( -1.299212598425196097, -0.6692913385826771977, 8.415575281601705876E-17 ) ) ;
#15327 = CARTESIAN_POINT ( 'NONE',  ( 0.8464566929133865436, 0.1660481256975883668, -0.3530559997133364547 ) ) ;
#15328 = CARTESIAN_POINT ( 'NONE',  ( -0.2155943732389342393, -0.3272402980651248905, -1.929133858267717105 ) ) ;
#15329 = CARTESIAN_POINT ( 'NONE',  ( -0.3917322834645669549, -0.1049643490035306603, -2.242782152230970993 ) ) ;
#15330 = ORIENTED_EDGE ( 'NONE', *, *, #8460, .F. ) ;
#15331 = CARTESIAN_POINT ( 'NONE',  ( 0.3996062992125986035, 2.446882876249141962E-17, -0.4330708661417322913 ) ) ;
#15332 = ORIENTED_EDGE ( 'NONE', *, *, #21932, .T. ) ;
#15333 = CARTESIAN_POINT ( 'NONE',  ( 1.233595800524935227, 0.2306618581243847221, -0.2411417322834647770 ) ) ;
#15334 = CARTESIAN_POINT ( 'NONE',  ( 0.5577427821522314977, -0.2845877964562161244, -0.3641732283464567121 ) ) ;
#15335 = DIRECTION ( 'NONE',  ( -0.000000000000000000, -1.000000000000000000, -0.000000000000000000 ) ) ;
#15336 = CARTESIAN_POINT ( 'NONE',  ( 0.000000000000000000, 2.755905511811024056, 0.000000000000000000 ) ) ;
#15337 = FILL_AREA_STYLE_COLOUR ( '', #59365 ) ;
#15338 = CARTESIAN_POINT ( 'NONE',  ( 0.1049643490035303689, 0.3917322834645670104, -1.337926509186352142 ) ) ;
#15339 = EDGE_CURVE ( 'NONE', #15857, #20906, #39989, .T. ) ;
#15340 = AXIS2_PLACEMENT_3D ( 'NONE', #1828, #77602, #27488 ) ;
#15341 = CARTESIAN_POINT ( 'NONE',  ( 0.2925321140481932369, 0.2925321140481932369, -1.946850393700787274 ) ) ;
#15342 = CARTESIAN_POINT ( 'NONE',  ( 0.4479248917284270881, 1.694519753174063892, -3.911447006860421016 ) ) ;
#15343 = CARTESIAN_POINT ( 'NONE',  ( -0.2165354330708654795, -0.5400638737290845981, -0.3530559997133363437 ) ) ;
#15344 = CARTESIAN_POINT ( 'NONE',  ( 1.286089238845145033, 0.2306618581243848609, 0.2411417322834645549 ) ) ;
#15345 = VERTEX_POINT ( 'NONE', #44598 ) ;
#15346 = CARTESIAN_POINT ( 'NONE',  ( -1.706036745406823485, 0.2306618581243848609, 0.2411417322834645549 ) ) ;
#15347 = CARTESIAN_POINT ( 'NONE',  ( 1.679790026246720025, 0.1283753931104748280, 0.1820866141732283561 ) ) ;
#15348 = CARTESIAN_POINT ( 'NONE',  ( 0.000000000000000000, 2.755905511811024056, 0.000000000000000000 ) ) ;
#15349 = FACE_OUTER_BOUND ( 'NONE', #20817, .T. ) ;
#15350 = CARTESIAN_POINT ( 'NONE',  ( -1.443569553805773564, 0.1283753931104746893, -0.1820866141732285504 ) ) ;
#15351 = CARTESIAN_POINT ( 'NONE',  ( 0.3917322834645670104, -0.1049643490035303411, 0.05380577427821527092 ) ) ;
#15352 = CARTESIAN_POINT ( 'NONE',  ( 0.2230971128608932319, -0.4281496062992124485, 0.4176697321401328655 ) ) ;
#15353 = ORIENTED_EDGE ( 'NONE', *, *, #42934, .T. ) ;
#15355 = FACE_OUTER_BOUND ( 'NONE', #71733, .T. ) ;
#15354 = CARTESIAN_POINT ( 'NONE',  ( 1.541994750656168645, 0.2952755905511810774, -0.1292274648535930714 ) ) ;
#15356 = CARTESIAN_POINT ( 'NONE',  ( -0.6824146981627291497, -0.5023911411419708095, -0.1820866141732282451 ) ) ;
#15357 = CARTESIAN_POINT ( 'NONE',  ( 0.7742782152230979209, 0.05413385826771626580, -0.4176697321401330321 ) ) ;
#15358 = CARTESIAN_POINT ( 'NONE',  ( 1.358267716535433323, -0.4536011799217368745, -0.2665933059059886201 ) ) ;
#15359 = CARTESIAN_POINT ( 'NONE',  ( 0.2867679344610365999, 0.2867679344610365999, -1.162710343010812108 ) ) ;
#15360 = CARTESIAN_POINT ( 'NONE',  ( -0.8202099737532801971, -0.5511811023622046335, 0.09757992244046803654 ) ) ;
#15361 = CARTESIAN_POINT ( 'NONE',  ( -1.555118110236219930, -0.4536011799217368745, -0.2665933059059886201 ) ) ;
#15362 = CARTESIAN_POINT ( 'NONE',  ( 0.000000000000000000, 2.755905511811024056, 0.000000000000000000 ) ) ;
#15363 = CARTESIAN_POINT ( 'NONE',  ( 0.4199475065616803948, -0.6046776061558809534, -0.2411417322834644161 ) ) ;
#15364 = CARTESIAN_POINT ( 'NONE',  ( -0.8530183727034112984, -0.004921259842519576551, 0.3153832671262227771 ) ) ;
#15365 = CARTESIAN_POINT ( 'NONE',  ( -0.3805774278215216522, -0.3690944881889765550, -0.3153832671262227771 ) ) ;
#15366 = CARTESIAN_POINT ( 'NONE',  ( -0.3937007874015740483, -0.1870078740157480879, -0.4822834645669291653 ) ) ;
#15367 = CARTESIAN_POINT ( 'NONE',  ( -1.627296587926508442, 0.1283753931104748280, 0.1820866141732283561 ) ) ;
#15368 = CARTESIAN_POINT ( 'NONE',  ( -9.594673741351313045E-17, 0.3917322834645670659, 0.003261524113173961108 ) ) ;
#15369 = CARTESIAN_POINT ( 'NONE',  ( 0.7611548556430451917, -0.6046776061558807314, 0.2411417322834647770 ) ) ;
#15370 = CARTESIAN_POINT ( 'NONE',  ( 0.3458507752293908943, -0.3458507752293908943, -0.2559055118110235560 ) ) ;
#15371 = CARTESIAN_POINT ( 'NONE',  ( 0.3458507752293908943, 0.3458507752293908943, -1.631889763779527325 ) ) ;
#15372 = CARTESIAN_POINT ( 'NONE',  ( -0.8858267716535425107, 0.1660481256975883668, -0.3530559997133364547 ) ) ;
#15373 = CARTESIAN_POINT ( 'NONE',  ( -0.2296587926509179312, -0.2845877964562161244, -0.3641732283464567121 ) ) ;
#15374 = CARTESIAN_POINT ( 'NONE',  ( -1.509186351706035767, -0.4281496062992124485, 0.4176697321401328655 ) ) ;
#15375 = CARTESIAN_POINT ( 'NONE',  ( 0.4790026246719168435, -0.2845877964562161244, -0.3641732283464567121 ) ) ;
#15376 = CARTESIAN_POINT ( 'NONE',  ( -0.6889763779527552368, -0.4536011799217368745, -0.2665933059059886201 ) ) ;
#15377 = CARTESIAN_POINT ( 'NONE',  ( -0.8727034120734901146, -0.05778040916215560624, -0.4822834645669293319 ) ) ;
#15378 = CARTESIAN_POINT ( 'NONE',  ( -1.541994750656167090, 0.2952755905511811885, 0.1292274648535926551 ) ) ;
#15379 = CARTESIAN_POINT ( 'NONE',  ( 1.213910761154856299, 0.2952755905511811885, 0.1292274648535926551 ) ) ;
#15380 = CARTESIAN_POINT ( 'NONE',  ( 0.4177787735907000366, 0.3937007874015748254, -1.382006255033530806 ) ) ;
#15381 = CARTESIAN_POINT ( 'NONE',  ( 0.9251968503937015864, 0.07958543189024071263, -0.2665933059059888421 ) ) ;
#15382 = CARTESIAN_POINT ( 'NONE',  ( 0.5183727034120741983, -0.6692913385826771977, 0.1292274648535927661 ) ) ;
#15383 = DIRECTION ( 'NONE',  ( -0.000000000000000000, 1.000000000000000000, -0.000000000000000000 ) ) ;
#15384 = CARTESIAN_POINT ( 'NONE',  ( 1.601049868766404982, 0.1283753931104748280, 0.1820866141732283561 ) ) ;
#15385 = EDGE_LOOP ( 'NONE', ( #22971, #11276 ) ) ;
#15386 = CARTESIAN_POINT ( 'NONE',  ( -0.3996062992125984925, -0.1070741851644056858, -2.642388451443570041 ) ) ;
#15387 = CARTESIAN_POINT ( 'NONE',  ( -1.292650918635170010, 0.1771653543307087075, -0.09757992244046823083 ) ) ;
#15388 = CARTESIAN_POINT ( 'NONE',  ( -0.2755905511811015396, -0.6692913385826771977, 8.415575281601705876E-17 ) ) ;
#15389 = CARTESIAN_POINT ( 'NONE',  ( 0.4265091863517067039, -0.6692913385826773087, -0.1292274648535924053 ) ) ;
#15390 = CARTESIAN_POINT ( 'NONE',  ( -1.325459317585300889, -0.3690944881889765550, -0.3153832671262227771 ) ) ;
#15391 = CARTESIAN_POINT ( 'NONE',  ( 0.3460692066303958092, 0.1998031496062993018, -1.782808398950131323 ) ) ;
#15392 = CARTESIAN_POINT ( 'NONE',  ( -1.502624671916009680, -0.05778040916215560624, -0.4822834645669293319 ) ) ;
#15393 = CARTESIAN_POINT ( 'NONE',  ( 0.2690288713910767848, 0.2952755905511811885, 0.1292274648535926551 ) ) ;
#15394 = CARTESIAN_POINT ( 'NONE',  ( -0.09842519685039295696, -0.5400638737290844871, 0.3530559997133364547 ) ) ;
#15395 = CARTESIAN_POINT ( 'NONE',  ( 1.325459317585302665, 0.05413385826771626580, -0.4176697321401330321 ) ) ;
#15396 = CARTESIAN_POINT ( 'NONE',  ( 4.893765752498283308E-17, -0.3996062992125985480, -0.9429133858267716439 ) ) ;
#15397 = CARTESIAN_POINT ( 'NONE',  ( 0.3460692066303959202, 0.1998031496062993295, -1.391076115485564424 ) ) ;
#15398 = CIRCLE ( 'NONE', #59717, 0.07874015748031502893 ) ;
#15399 = CARTESIAN_POINT ( 'NONE',  ( 0.3949938075777409963, 2.418639510665530435E-17, -1.062992125984251857 ) ) ;
#15400 = CARTESIAN_POINT ( 'NONE',  ( 0.3996062992125986035, 2.446882876249141962E-17, -2.322834645669291209 ) ) ;
#15401 = LINE ( 'NONE', #60826, #68179 ) ;
#15402 = APPLICATION_CONTEXT ( 'automotive_design' ) ;
#15403 = CARTESIAN_POINT ( 'NONE',  ( -0.1049643490035307020, 0.3917322834645669549, -0.3136482939632545541 ) ) ;
#15404 = CARTESIAN_POINT ( 'NONE',  ( -0.1115485564304456306, 0.1771653543307087075, -0.09757992244046823083 ) ) ;
#15405 = CARTESIAN_POINT ( 'NONE',  ( -0.2493438320209966919, 0.05413385826771626580, -0.4176697321401330321 ) ) ;
#15406 = CARTESIAN_POINT ( 'NONE',  ( 1.010498687664042716, 0.05413385826771626580, -0.4176697321401330321 ) ) ;
#15407 = CARTESIAN_POINT ( 'NONE',  ( 0.2891555358219910499, 0.2891555358219910499, -1.631889763779527991 ) ) ;
#15408 = CARTESIAN_POINT ( 'NONE',  ( -0.1049868766404193215, -0.5023911411419708095, 0.1820866141732285504 ) ) ;
#15409 = CARTESIAN_POINT ( 'NONE',  ( -1.148293963254592542, 0.2952755905511811885, 0.1292274648535926551 ) ) ;
#15410 = CARTESIAN_POINT ( 'NONE',  ( -1.561679790026246017, -0.4281496062992127816, -0.4176697321401328100 ) ) ;
#15411 = CARTESIAN_POINT ( 'NONE',  ( -0.4091458600556405756, 0.2362204724409446288, -1.916010498687664043 ) ) ;
#15412 = CARTESIAN_POINT ( 'NONE',  ( -0.01000891935578489267, 8.471767977567108961E-16, -0.4445507791589058955 ) ) ;
#15413 = ORIENTED_EDGE ( 'NONE', *, *, #61486, .F. ) ;
#15414 = VERTEX_POINT ( 'NONE', #64400 ) ;
#15415 = CARTESIAN_POINT ( 'NONE',  ( 0.9973753280839902091, 0.2306618581243847221, -0.2411417322834647770 ) ) ;
#15416 = CARTESIAN_POINT ( 'NONE',  ( -1.692913385826770645, 0.2952755905511811885, 0.000000000000000000 ) ) ;
#15418 = CARTESIAN_POINT ( 'NONE',  ( -1.154855643044618851, 0.2306618581243848609, 0.2411417322834645549 ) ) ;
#15417 = CARTESIAN_POINT ( 'NONE',  ( -1.299212598425196097, 0.1771653543307087630, 0.000000000000000000 ) ) ;
#15419 = CARTESIAN_POINT ( 'NONE',  ( 0.3392501089628018329, -0.1958661417322834497, -2.389744463745719916 ) ) ;
#15420 = CARTESIAN_POINT ( 'NONE',  ( -1.114781747626346187, -2.609869883881465018E-15, -0.3464511005275220379 ) ) ;
#15421 = CARTESIAN_POINT ( 'NONE',  ( 1.371391076115485941, 0.2952755905511811885, 0.1292274648535926551 ) ) ;
#15422 = CARTESIAN_POINT ( 'NONE',  ( -1.574803149606298636, -0.1870078740157479769, 0.4822834645669291653 ) ) ;
#15423 = CARTESIAN_POINT ( 'NONE',  ( -0.1968503937007867743, -0.6692913385826771977, 8.415575281601705876E-17 ) ) ;
#15424 = CARTESIAN_POINT ( 'NONE',  ( -0.3608923884514428360, -0.6692913385826773087, -0.1292274648535924053 ) ) ;
#15425 = CARTESIAN_POINT ( 'NONE',  ( -1.338582677165353729, -0.1870078740157479769, 0.4822834645669291653 ) ) ;
#15426 = CARTESIAN_POINT ( 'NONE',  ( 0.1049643490035304938, -0.3917322834645669549, 0.1450131233595799429 ) ) ;
#15427 = EDGE_CURVE ( 'NONE', #72166, #6582, #4423, .T. ) ;
#15428 = CARTESIAN_POINT ( 'NONE',  ( 0.5314960629921264834, 0.1660481256975883668, -0.3530559997133364547 ) ) ;
#15429 = CARTESIAN_POINT ( 'NONE',  ( -0.1958661417322836718, 0.3392501089628017219, -1.737532808398950079 ) ) ;
#15430 = CARTESIAN_POINT ( 'NONE',  ( -1.069553805774277722, -0.5511811023622048555, -0.09757992244046775898 ) ) ;
#15431 = ORIENTED_EDGE ( 'NONE', *, *, #3865, .F. ) ;
#15432 = CARTESIAN_POINT ( 'NONE',  ( -9.674558042662121740E-17, 0.3949938075777409963, -2.362204724409449064 ) ) ;
#15433 = ORIENTED_EDGE ( 'NONE', *, *, #17984, .F. ) ;
#15434 = DIRECTION ( 'NONE',  ( 0.000000000000000000, -1.000000000000000000, -0.000000000000000000 ) ) ;
#15435 = CARTESIAN_POINT ( 'NONE',  ( -1.640419947506561060, -0.4281496062992127816, -0.4176697321401328100 ) ) ;
#15436 = CARTESIAN_POINT ( 'NONE',  ( 1.397637795275591177, -0.5400638737290844871, 0.3530559997133364547 ) ) ;
#15437 = CARTESIAN_POINT ( 'NONE',  ( 4.893765752498283924E-17, -0.3996062992125986035, -0.5511811023622047445 ) ) ;
#15438 = CARTESIAN_POINT ( 'NONE',  ( -1.568241469816272105, -0.05778040916215522460, 0.4822834645669289988 ) ) ;
#15439 = CARTESIAN_POINT ( 'NONE',  ( 1.813482582612293559, 2.755905511811024056, -0.5314960629921260393 ) ) ;
#15440 = CARTESIAN_POINT ( 'NONE',  ( 0.4461942257217856311, 0.2306618581243847221, -0.2411417322834647770 ) ) ;
#15441 = CARTESIAN_POINT ( 'NONE',  ( -2.795275590551184575, 0.7480314960629931287, -3.317813449798768424E-16 ) ) ;
#15442 = CARTESIAN_POINT ( 'NONE',  ( 0.1049643490035303689, 0.3917322834645670104, -0.07808398950131241467 ) ) ;
#15443 = EDGE_CURVE ( 'NONE', #51179, #31528, #53604, .T. ) ;
#15444 = CARTESIAN_POINT ( 'NONE',  ( -0.2099737532808391705, 0.1283753931104748280, 0.1820866141732283561 ) ) ;
#15445 = CARTESIAN_POINT ( 'NONE',  ( -0.9186351706036736120, 0.1283753931104748280, 0.1820866141732283561 ) ) ;
#15446 = AXIS2_PLACEMENT_3D ( 'NONE', #45219, #49894, #50302 ) ;
#15447 = CARTESIAN_POINT ( 'NONE',  ( -1.266404199475064773, -0.05778040916215560624, -0.4822834645669293319 ) ) ;
#15448 = CARTESIAN_POINT ( 'NONE',  ( 1.043307086614173818, -0.5400638737290845981, -0.3530559997133363437 ) ) ;
#15449 = CARTESIAN_POINT ( 'NONE',  ( -0.7874015748031489847, -0.1870078740157480879, -0.4822834645669291653 ) ) ;
#15450 = CARTESIAN_POINT ( 'NONE',  ( -0.3917322834645670104, -7.196005306013484475E-17, -0.03149606299212594218 ) ) ;
#15451 = ORIENTED_EDGE ( 'NONE', *, *, #52110, .T. ) ;
#15452 = CARTESIAN_POINT ( 'NONE',  ( -1.266404199475064773, -0.05778040916215560624, -0.4822834645669293319 ) ) ;
#15453 = CARTESIAN_POINT ( 'NONE',  ( -1.608952832271129729, 0.2885925887579551818, -0.09257012520105759035 ) ) ;
#15454 = LENGTH_MEASURE_WITH_UNIT ( LENGTH_MEASURE( 0.02539999999999999897 ), #27231 );
#15455 = CARTESIAN_POINT ( 'NONE',  ( -0.3458507752293909498, 0.3458507752293907833, -1.437007874015747921 ) ) ;
#15456 = DIRECTION ( 'NONE',  ( 1.000000000000000000, -0.000000000000000000, -0.000000000000000000 ) ) ;
#15457 = CARTESIAN_POINT ( 'NONE',  ( 0.2867679344610365999, 0.2867679344610365999, -0.6023622047244093780 ) ) ;
#15458 = CARTESIAN_POINT ( 'NONE',  ( -0.1049643490035307020, 0.3917322834645669549, -2.453412073490813583 ) ) ;
#15459 = CARTESIAN_POINT ( 'NONE',  ( -0.1902887139107604098, 0.2952755905511810774, -0.1292274648535930714 ) ) ;
#15460 = CARTESIAN_POINT ( 'NONE',  ( 1.312335958005250269, -0.6046776061558807314, 0.2411417322834647770 ) ) ;
#15461 = CARTESIAN_POINT ( 'NONE',  ( 0.3460692066303958092, 0.1998031496062993018, 0.1069553805774277888 ) ) ;
#15463 = DIRECTION ( 'NONE',  ( 0.000000000000000000, 0.000000000000000000, -1.000000000000000000 ) ) ;
#15462 = CARTESIAN_POINT ( 'NONE',  ( -1.541994750656167090, 0.2952755905511811885, 0.1292274648535926551 ) ) ;
#15464 = CARTESIAN_POINT ( 'NONE',  ( -1.240157480314959759, 0.1660481256975885056, 0.3530559997133364547 ) ) ;
#15465 = CARTESIAN_POINT ( 'NONE',  ( -0.7283464566929126471, 0.1660481256975883668, -0.3530559997133364547 ) ) ;
#15466 = AXIS2_PLACEMENT_3D ( 'NONE', #75989, #43558, #69668 ) ;
#15467 = CARTESIAN_POINT ( 'NONE',  ( -0.2867679344610364334, -0.2867679344610368219, 0.01839201919391258294 ) ) ;
#15468 = CARTESIAN_POINT ( 'NONE',  ( 0.6496062992125991586, 0.07958543189024085140, 0.2665933059059887866 ) ) ;
#15469 = CARTESIAN_POINT ( 'NONE',  ( -0.1049643490035301885, -0.3917322834645671215, -0.1568241469816273326 ) ) ;
#15470 = CARTESIAN_POINT ( 'NONE',  ( 0.5249343832021005074, -0.5023911411419708095, 0.1820866141732285504 ) ) ;
#15471 = CARTESIAN_POINT ( 'NONE',  ( 1.102362204724410155, -0.1870078740157479769, 0.3641732283464567677 ) ) ;
#15472 = CARTESIAN_POINT ( 'NONE',  ( 1.049868766404200127, -0.6046776061558809534, -0.2411417322834644161 ) ) ;
#15473 = CARTESIAN_POINT ( 'NONE',  ( -0.4593175853018364174, -0.3690944881889765550, -0.3153832671262227771 ) ) ;
#15474 = CARTESIAN_POINT ( 'NONE',  ( -0.1958661417322834220, -0.3392501089628018884, -2.104986876640420057 ) ) ;
#15475 = CARTESIAN_POINT ( 'NONE',  ( -1.135170603674539924, 0.2952755905511810774, -0.1292274648535930714 ) ) ;
#15476 = CARTESIAN_POINT ( 'NONE',  ( -0.02624671916010428221, -0.5023911411419708095, 0.1820866141732285504 ) ) ;
#15477 = B_SPLINE_CURVE_WITH_KNOTS ( 'NONE', 3,
 ( #4667, #16920, #50103, #74575, #24842, #5091, #81717, #68261, #24027, #31160, #43365, #42557, #76213, #74988, #5905, #75800, #69479, #17333, #10597, #81302, #36655, #31577, #30340, #61923, #18142, #55590, #56827, #37894, #44194, #36253, #68657, #30759, #43776, #4264, #42963, #82524, #11832, #10995, #29927, #23616, #56006, #50509, #49285, #62330, #37485, #18549, #69884, #49695, #12238, #75390, #69065, #11415, #37070, #62755, #63159, #63570, #71977, #7158, #32829, #13904 ),
 .UNSPECIFIED., .F., .F.,
 ( 4, 2, 2, 2, 2, 2, 2, 2, 2, 2, 2, 2, 2, 2, 2, 2, 2, 2, 2, 2, 2, 2, 2, 2, 2, 2, 2, 2, 2, 4 ),
 ( 0.01323639539072430336, 0.01388181161316797210, 0.01452722783561164084, 0.01581806028049896964, 0.01710889272538629671, 0.01839972517027362378, 0.02098139006004827098, 0.02356305494982292165, 0.02485388739471023484, 0.02614471983959755497, 0.02743555228448487163, 0.02872638472937218829, 0.03130804961914681467, 0.03259888206403412786, 0.03388971450892144105, 0.03453513073136509071, 0.03518054695380875424, 0.03647137939869606049, 0.03776221184358337368, 0.03905304428847067993, 0.04034387673335799313, 0.04163470917824529938, 0.04421637406801992576, 0.04679803895779455908, 0.04937970384756918546, 0.05067053629245649865, 0.05196136873734381184, 0.05325220118223111809, 0.05389761740467478163, 0.05454303362711843822 ),
 .UNSPECIFIED. ) ;
#15478 = CARTESIAN_POINT ( 'NONE',  ( -1.141732283464566011, 0.1771653543307087630, 0.000000000000000000 ) ) ;
#15479 = CARTESIAN_POINT ( 'NONE',  ( 0.4724409448818897572, -0.1265901696524988906, -0.3458005249343831244 ) ) ;
#15480 = CARTESIAN_POINT ( 'NONE',  ( -0.8333333333333323711, 0.1771653543307087630, 0.09757992244046791164 ) ) ;
#15481 = CARTESIAN_POINT ( 'NONE',  ( -0.2099737532808391705, 0.2306618581243848609, 0.2411417322834645549 ) ) ;
#15482 = CARTESIAN_POINT ( 'NONE',  ( 1.666666666666667185, -0.004921259842519576551, 0.3153832671262227771 ) ) ;
#15483 = CARTESIAN_POINT ( 'NONE',  ( 0.5249343832021003964, 0.1283753931104746893, -0.1820866141732285504 ) ) ;
#15484 = CARTESIAN_POINT ( 'NONE',  ( -0.1706036745406816491, -0.3690944881889763329, 0.3153832671262228327 ) ) ;
#15485 = CARTESIAN_POINT ( 'NONE',  ( -0.8530183727034112984, 0.05413385826771666132, 0.4176697321401328100 ) ) ;
#15486 = CARTESIAN_POINT ( 'NONE',  ( 0.000000000000000000, -1.268531780058464091E-17, 0.000000000000000000 ) ) ;
#15487 = CARTESIAN_POINT ( 'NONE',  ( -0.9711286089238838626, 0.1283753931104746893, -0.1820866141732285504 ) ) ;
#15488 = CARTESIAN_POINT ( 'NONE',  ( -0.4724409448818898682, -8.678599364036362592E-17, -2.005905511811023612 ) ) ;
#15489 = CARTESIAN_POINT ( 'NONE',  ( 0.6692913385826778638, -0.6692913385826771977, 8.415575281601705876E-17 ) ) ;
#15490 = CARTESIAN_POINT ( 'NONE',  ( -0.3996062992125986590, 0.1070741851644051723, -1.684383202099737353 ) ) ;
#15491 = CARTESIAN_POINT ( 'NONE',  ( 1.515748031496063186, -0.5400638737290845981, -0.3530559997133363437 ) ) ;
#15492 = CARTESIAN_POINT ( 'NONE',  ( -0.3280839895013117347, -0.3690944881889763329, 0.3153832671262228327 ) ) ;
#15493 = CARTESIAN_POINT ( 'NONE',  ( -0.02624671916010428221, -0.6046776061558807314, 0.2411417322834647770 ) ) ;
#15494 = CARTESIAN_POINT ( 'NONE',  ( -1.430446194225720724, 0.05413385826771626580, -0.4176697321401330321 ) ) ;
#15495 = CARTESIAN_POINT ( 'NONE',  ( -1.561679790026246017, -0.3690944881889765550, -0.3153832671262227771 ) ) ;
#15496 = CARTESIAN_POINT ( 'NONE',  ( 1.200787401574803681, 0.1660481256975885056, 0.3530559997133364547 ) ) ;
#15497 = CARTESIAN_POINT ( 'NONE',  ( -0.8661417322834640276, -0.1870078740157480601, -0.3641732283464567677 ) ) ;
#15498 = FACE_OUTER_BOUND ( 'NONE', #42007, .T. ) ;
#15499 = CARTESIAN_POINT ( 'NONE',  ( 0.3460692066303959202, 0.1998031496062993295, -0.2887139107611548794 ) ) ;
#15500 = CARTESIAN_POINT ( 'NONE',  ( -9.674558042662121740E-17, 0.3949938075777409963, -5.756223643949423463E-17 ) ) ;
#15501 = CARTESIAN_POINT ( 'NONE',  ( -3.881211926161857395, 2.729373344522950884, -0.5314960629921260393 ) ) ;
#15502 = CARTESIAN_POINT ( 'NONE',  ( 1.043307086614173818, -0.4536011799217368745, -0.2665933059059886201 ) ) ;
#15503 = CARTESIAN_POINT ( 'NONE',  ( -1.528871391076114250, 0.2952755905511810774, -0.1292274648535930714 ) ) ;
#15504 = CARTESIAN_POINT ( 'NONE',  ( 0.8333333333333340365, 0.2952755905511810774, -0.1292274648535930714 ) ) ;
#15505 = CARTESIAN_POINT ( 'NONE',  ( 0.1958661417322834775, 0.3392501089628018884, -2.276246719160105236 ) ) ;
#15506 = CARTESIAN_POINT ( 'NONE',  ( 1.345144356955381593, -0.08942795157527998196, 0.3641732283464567121 ) ) ;
#15507 = CARTESIAN_POINT ( 'NONE',  ( 0.04593175853018440641, -0.6692913385826771977, 0.1292274648535927661 ) ) ;
#15508 = CARTESIAN_POINT ( 'NONE',  ( -0.2690288713910754526, -0.6692913385826771977, 0.1292274648535927661 ) ) ;
#15509 = CARTESIAN_POINT ( 'NONE',  ( 1.509186351706037543, 0.05413385826771666132, 0.4176697321401328100 ) ) ;
#15510 = CARTESIAN_POINT ( 'NONE',  ( -0.2362204724409447953, -0.4091458600556404646, -0.8530183727034120755 ) ) ;
#15511 = CARTESIAN_POINT ( 'NONE',  ( 0.06873123812453012238, 8.471767977567108961E-16, -0.4445507791589058955 ) ) ;
#15512 = VECTOR ( 'NONE', #82304, 39.37007874015748143 ) ;
#15513 = CARTESIAN_POINT ( 'NONE',  ( 0.2559055118110243332, -0.4536011799217368745, -0.2665933059059886201 ) ) ;
#15514 = VERTEX_POINT ( 'NONE', #6736 ) ;
#15516 = CARTESIAN_POINT ( 'NONE',  ( -0.1958661417322833942, -0.3392501089628018884, -0.3773159037083483325 ) ) ;
#15515 = AXIS2_PLACEMENT_3D ( 'NONE', #80238, #73499, #79821 ) ;
#15517 = ORIENTED_EDGE ( 'NONE', *, *, #64730, .T. ) ;
#15518 = CARTESIAN_POINT ( 'NONE',  ( -0.6102362204724400829, 0.1660481256975885056, 0.3530559997133364547 ) ) ;
#15519 = CARTESIAN_POINT ( 'NONE',  ( 1.174540682414699111, -0.05778040916215560624, -0.4822834645669293319 ) ) ;
#15520 = CARTESIAN_POINT ( 'NONE',  ( 0.03937007874015833325, -0.6692913385826771977, 8.415575281601705876E-17 ) ) ;
#15521 = CARTESIAN_POINT ( 'NONE',  ( -0.1574803149606292529, -0.1870078740157480601, -0.3641732283464567677 ) ) ;
#15522 = CARTESIAN_POINT ( 'NONE',  ( 1.003937007874016407, -0.5400638737290844871, 0.3530559997133364547 ) ) ;
#15523 = CARTESIAN_POINT ( 'NONE',  ( -0.8727034120734901146, -0.3162353388693405765, 0.4822834645669290543 ) ) ;
#15524 = CARTESIAN_POINT ( 'NONE',  ( -0.4068241469816267775, 0.05413385826771626580, -0.4176697321401330321 ) ) ;
#15525 = CARTESIAN_POINT ( 'NONE',  ( -0.7677165354330699465, 0.1660481256975885056, 0.3530559997133364547 ) ) ;
#15526 = CARTESIAN_POINT ( 'NONE',  ( 1.056430446194226436, -0.6692913385826773087, -0.1292274648535924053 ) ) ;
#15527 = CARTESIAN_POINT ( 'NONE',  ( 1.076115485564305141, -0.6046776061558807314, 0.2411417322834647770 ) ) ;
#15528 = CARTESIAN_POINT ( 'NONE',  ( 0.7939632545931766261, -0.3162353388693409650, -0.4822834645669289433 ) ) ;
#15529 = CARTESIAN_POINT ( 'NONE',  ( 0.2867679344610365999, 0.2867679344610365999, -0.6023622047244093780 ) ) ;
#15530 = CARTESIAN_POINT ( 'NONE',  ( -0.01312335958005186876, -0.004921259842519870586, -0.3153832671262229437 ) ) ;
#15531 = ORIENTED_EDGE ( 'NONE', *, *, #57864, .F. ) ;
#15532 = CARTESIAN_POINT ( 'NONE',  ( 0.1974969037888706369, -0.3420746716998659953, -1.194225721784776928 ) ) ;
#15533 = ORIENTED_EDGE ( 'NONE', *, *, #36633, .F. ) ;
#15534 = CARTESIAN_POINT ( 'NONE',  ( -0.7874015748031489847, -0.1870078740157479769, 0.3641732283464567677 ) ) ;
#15535 = CARTESIAN_POINT ( 'NONE',  ( 0.1312335958005257930, 0.2306618581243847221, -0.2411417322834647770 ) ) ;
#15536 = CARTESIAN_POINT ( 'NONE',  ( 0.000000000000000000, 2.755905511811024056, 0.000000000000000000 ) ) ;
#15537 = CARTESIAN_POINT ( 'NONE',  ( -0.2099737532808391705, -0.6046776061558809534, -0.2411417322834644161 ) ) ;
#15538 = CARTESIAN_POINT ( 'NONE',  ( -0.3543307086614165824, -0.6692913385826771977, 8.415575281601705876E-17 ) ) ;
#15540 = CARTESIAN_POINT ( 'NONE',  ( -1.154855643044618851, 0.2306618581243848609, 0.2411417322834645549 ) ) ;
#15539 = B_SPLINE_CURVE_WITH_KNOTS ( 'NONE', 3,
 ( #29858, #81229, #55521, #62263, #23546, #74919, #4599 ),
 .UNSPECIFIED., .F., .F.,
 ( 4, 3, 4 ),
 ( 1.734723475976807094E-18, 0.001246230184515548971, 0.002492489877932635954 ),
 .UNSPECIFIED. ) ;
#15541 = CARTESIAN_POINT ( 'NONE',  ( -1.279527559055116948, -0.5400638737290844871, 0.3530559997133364547 ) ) ;
#15542 = CARTESIAN_POINT ( 'NONE',  ( 1.213910761154856299, 0.1771653543307087630, 0.09757992244046791164 ) ) ;
#15543 = CARTESIAN_POINT ( 'NONE',  ( 0.4573980430285805587, 1.664306849931878274, 1.024599542107852423 ) ) ;
#15544 = CARTESIAN_POINT ( 'NONE',  ( 0.2635274766024540694, 0.1334916279589803412, 5.819004606509203370 ) ) ;
#15545 = CARTESIAN_POINT ( 'NONE',  ( 0.4133858267716541968, -0.4536011799217368745, -0.2665933059059886201 ) ) ;
#15546 = CARTESIAN_POINT ( 'NONE',  ( 0.1837270341207357105, -0.6046776061558809534, -0.2411417322834644161 ) ) ;
#15547 = CARTESIAN_POINT ( 'NONE',  ( 0.2362204724409456558, -0.1870078740157479769, 0.4822834645669291653 ) ) ;
#15548 = ORIENTED_EDGE ( 'NONE', *, *, #33485, .T. ) ;
#15549 = CARTESIAN_POINT ( 'NONE',  ( 0.1998031496062994405, -0.3460692066303958092, -1.666666666666666741 ) ) ;
#15550 = FACE_OUTER_BOUND ( 'NONE', #23579, .T. ) ;
#15551 = ORIENTED_EDGE ( 'NONE', *, *, #64058, .T. ) ;
#15552 = CARTESIAN_POINT ( 'NONE',  ( 0.1998031496062992463, 0.3460692066303959202, -1.323490813648294129 ) ) ;
#15553 = CARTESIAN_POINT ( 'NONE',  ( -0.1070741851644051862, -0.3996062992125986590, -0.4639107611548556331 ) ) ;
#15554 = CARTESIAN_POINT ( 'NONE',  ( -0.4986876640419942164, -0.6046776061558807314, 0.2411417322834647770 ) ) ;
#15555 = CARTESIAN_POINT ( 'NONE',  ( -0.4724409448818895907, -0.1265901696524993070, -0.04593175853018372640 ) ) ;
#15556 = CARTESIAN_POINT ( 'NONE',  ( -0.3392501089628017219, -0.1958661417322836718, -2.499343832020997080 ) ) ;
#15557 = CARTESIAN_POINT ( 'NONE',  ( -1.555118110236219930, -0.4536011799217368745, -0.2665933059059886201 ) ) ;
#15558 = CARTESIAN_POINT ( 'NONE',  ( 0.7677165354330716118, -0.5400638737290844871, 0.3530559997133364547 ) ) ;
#15559 = CARTESIAN_POINT ( 'NONE',  ( 0.8202099737532814183, -0.6692913385826773087, -0.1292274648535924053 ) ) ;
#15560 = CARTESIAN_POINT ( 'NONE',  ( -0.4002624671916004129, -0.2845877964562159024, 0.3641732283464567677 ) ) ;
#15561 = CARTESIAN_POINT ( 'NONE',  ( -0.04593175853018302557, -0.6692913385826773087, -0.1292274648535924053 ) ) ;
#15562 = CARTESIAN_POINT ( 'NONE',  ( -0.4724409448818895907, -0.1265901696524993070, -1.854986876640420057 ) ) ;
#15563 = CARTESIAN_POINT ( 'NONE',  ( 0.05905511811023709395, -0.4536011799217367080, 0.2665933059059888421 ) ) ;
#15564 = CARTESIAN_POINT ( 'NONE',  ( -0.4593175853018366950, 0.05413385826771666132, 0.4176697321401328100 ) ) ;
#15565 = CARTESIAN_POINT ( 'NONE',  ( -0.3949938075777408852, -0.1058382717557502933, -1.697506561679790194 ) ) ;
#15566 = CARTESIAN_POINT ( 'NONE',  ( -1.660104986876639543, -0.05778040916215560624, -0.4822834645669293319 ) ) ;
#15567 = CARTESIAN_POINT ( 'NONE',  ( 5.463695987328526437E-16, -0.1870078740157479769, 0.3641732283464567677 ) ) ;
#15568 = CARTESIAN_POINT ( 'NONE',  ( 1.528871391076116026, 0.1771653543307087630, 0.09757992244046791164 ) ) ;
#15570 = EDGE_CURVE ( 'NONE', #32472, #22014, #71555, .T. ) ;
#15569 = CARTESIAN_POINT ( 'NONE',  ( -1.181102362204723644, -0.1870078740157480879, -0.4822834645669291653 ) ) ;
#15571 = CARTESIAN_POINT ( 'NONE',  ( -0.6561679790026240244, 0.1283753931104746893, -0.1820866141732285504 ) ) ;
#15572 = CARTESIAN_POINT ( 'NONE',  ( -1.559171609364246924, 0.3937007874015748254, 0.1028181436694137613 ) ) ;
#15573 = CARTESIAN_POINT ( 'NONE',  ( -1.358267716535432434, 0.1660481256975883668, -0.3530559997133364547 ) ) ;
#15574 = CARTESIAN_POINT ( 'NONE',  ( -0.7217847769028863381, -0.4281496062992124485, 0.4176697321401328655 ) ) ;
#15575 = CARTESIAN_POINT ( 'NONE',  ( 0.1771653543307093182, -0.5400638737290845981, -0.3530559997133363437 ) ) ;
#15576 = CARTESIAN_POINT ( 'NONE',  ( -0.3460692066303960313, 0.1998031496062989965, -2.465223097112860806 ) ) ;
#15577 = CARTESIAN_POINT ( 'NONE',  ( -0.2867679344610364334, -0.2867679344610368219, -2.501293020176166504 ) ) ;
#15578 = CARTESIAN_POINT ( 'NONE',  ( -2.165589143934456118, 1.494558157769223961, -0.4725443725032424380 ) ) ;
#15579 = CARTESIAN_POINT ( 'NONE',  ( 0.4790026246719168435, -0.2845877964562161244, -0.3641732283464567121 ) ) ;
#15580 = CARTESIAN_POINT ( 'NONE',  ( 1.056430446194226436, -0.6692913385826773087, -0.1292274648535924053 ) ) ;
#15581 = CARTESIAN_POINT ( 'NONE',  ( -1.194225721784776262, -0.004921259842519870586, -0.3153832671262229437 ) ) ;
#15582 = CARTESIAN_POINT ( 'NONE',  ( 1.371391076115485941, 0.2952755905511811885, 0.1292274648535926551 ) ) ;
#15583 = CARTESIAN_POINT ( 'NONE',  ( -1.469816272965878357, -0.5023911411419708095, -0.1820866141732282451 ) ) ;
#15584 = CARTESIAN_POINT ( 'NONE',  ( -0.4658792650918627265, -0.05778040916215522460, 0.4822834645669289988 ) ) ;
#15585 = CARTESIAN_POINT ( 'NONE',  ( 0.3215223097112867578, -0.2845877964562161244, -0.3641732283464567121 ) ) ;
#15586 = CARTESIAN_POINT ( 'NONE',  ( 0.2362204724409451007, -0.4091458600556402980, -0.8792650918635170898 ) ) ;
#15587 = CARTESIAN_POINT ( 'NONE',  ( 0.5183727034120741983, 0.1771653543307087075, -0.09757992244046823083 ) ) ;
#15588 = CARTESIAN_POINT ( 'NONE',  ( 0.07217847769028949700, -0.3162353388693405765, 0.4822834645669290543 ) ) ;
#15589 = EDGE_CURVE ( 'NONE', #30707, #8650, #32196, .T. ) ;
#15590 = CARTESIAN_POINT ( 'NONE',  ( -0.3996062992125984925, -0.1070741851644056858, -0.2801837270341207553 ) ) ;
#15591 = CARTESIAN_POINT ( 'NONE',  ( -0.4986876640419942164, -0.6046776061558807314, 0.2411417322834647770 ) ) ;
#15592 = CARTESIAN_POINT ( 'NONE',  ( 0.1958661417322834775, 0.3392501089628018884, -1.803805774278215202 ) ) ;
#15593 = CARTESIAN_POINT ( 'NONE',  ( 0.9973753280839902091, 0.1283753931104746893, -0.1820866141732285504 ) ) ;
#15594 = CARTESIAN_POINT ( 'NONE',  ( 0.07217847769028949700, -0.3162353388693405765, 0.4822834645669290543 ) ) ;
#15595 = CARTESIAN_POINT ( 'NONE',  ( -0.1181102362204717315, -0.6692913385826771977, 8.415575281601705876E-17 ) ) ;
#15596 = CARTESIAN_POINT ( 'NONE',  ( -0.3018372703412066094, -0.3690944881889765550, -0.3153832671262227771 ) ) ;
#15597 = FACE_OUTER_BOUND ( 'NONE', #33436, .T. ) ;
#15598 = CARTESIAN_POINT ( 'NONE',  ( -0.6233595800524928121, -0.2845877964562161244, -0.3641732283464567121 ) ) ;
#15599 = CARTESIAN_POINT ( 'NONE',  ( 0.5183727034120741983, -0.6692913385826771977, 0.1292274648535927661 ) ) ;
#15600 = CARTESIAN_POINT ( 'NONE',  ( -0.8727034120734901146, -0.08942795157528024563, -0.3641732283464568787 ) ) ;
#15601 = CARTESIAN_POINT ( 'NONE',  ( -0.1998031496062991630, -0.3460692066303959202, -0.9297900262467192478 ) ) ;
#15602 = CARTESIAN_POINT ( 'NONE',  ( -1.286089238845143479, 0.2306618581243847221, -0.2411417322834647770 ) ) ;
#15603 = CARTESIAN_POINT ( 'NONE',  ( 0.8550440751474870371, 1.722984403643211298E-16, -0.3954985857520063597 ) ) ;
#15604 = ORIENTED_EDGE ( 'NONE', *, *, #73594, .T. ) ;
#15605 = CARTESIAN_POINT ( 'NONE',  ( -1.102362204724408601, -0.1870078740157479769, 0.3641732283464567677 ) ) ;
#15606 = CARTESIAN_POINT ( 'NONE',  ( -0.4002624671916004129, -0.05778040916215560624, -0.4822834645669293319 ) ) ;
#15607 = EDGE_CURVE ( 'NONE', #77755, #21629, #45017, .T. ) ;
#15608 = CARTESIAN_POINT ( 'NONE',  ( -1.699475065616797398, 0.2952755905511811885, 0.1292274648535926551 ) ) ;
#15609 = CARTESIAN_POINT ( 'NONE',  ( -1.174540682414697335, -0.05778040916215522460, 0.4822834645669289988 ) ) ;
#15610 = FACE_OUTER_BOUND ( 'NONE', #42637, .T. ) ;
#15611 = CARTESIAN_POINT ( 'NONE',  ( 1.332020997375329197, -0.3162353388693405765, 0.4822834645669290543 ) ) ;
#15612 = CARTESIAN_POINT ( 'NONE',  ( 0.7414698162729663755, 0.2952755905511811885, 0.1292274648535926551 ) ) ;
#15613 = CARTESIAN_POINT ( 'NONE',  ( -0.2887139107611542133, 0.1539470093639523085, 0.1968503937007873850 ) ) ;
#15614 = AXIS2_PLACEMENT_3D ( 'NONE', #5411, #31487, #11746 ) ;
#15616 = CIRCLE ( 'NONE', #4834, 0.1968503937007874405 ) ;
#15615 = CARTESIAN_POINT ( 'NONE',  ( 0.2845256677560920044, -0.07972153265861246785, 5.543321648279010638 ) ) ;
#15617 = CARTESIAN_POINT ( 'NONE',  ( 1.574803149606299746, -0.1870078740157479769, 0.3641732283464567677 ) ) ;
#15618 = CARTESIAN_POINT ( 'NONE',  ( 0.1070741851644053527, 0.3996062992125986590, -0.3083989501312335846 ) ) ;
#15619 = ORIENTED_EDGE ( 'NONE', *, *, #36782, .T. ) ;
#15620 = CARTESIAN_POINT ( 'NONE',  ( -0.6430446194225712953, -0.004921259842519870586, -0.3153832671262229437 ) ) ;
#15621 = CARTESIAN_POINT ( 'NONE',  ( 0.3917322834645670104, 2.398668435337828261E-17, -2.314960629921259727 ) ) ;
#15622 = ORIENTED_EDGE ( 'NONE', *, *, #72813, .T. ) ;
#15623 = CARTESIAN_POINT ( 'NONE',  ( 1.010498687664042716, 0.05413385826771626580, -0.4176697321401330321 ) ) ;
#15624 = CARTESIAN_POINT ( 'NONE',  ( 0.1902887139107617975, 0.2952755905511811885, 0.1292274648535926551 ) ) ;
#15625 = CARTESIAN_POINT ( 'NONE',  ( -0.7611548556430438595, -0.6046776061558809534, -0.2411417322834644161 ) ) ;
#15626 = CARTESIAN_POINT ( 'NONE',  ( 1.332020997375329197, -0.3162353388693405765, 0.4822834645669290543 ) ) ;
#15627 = CARTESIAN_POINT ( 'NONE',  ( -1.122047244094487306, 0.07958543189024071263, -0.2665933059059888421 ) ) ;
#15628 = CARTESIAN_POINT ( 'NONE',  ( -0.6299212598425204535, 1.968503937007873628, -0.4915354330708654462 ) ) ;
#15629 = CARTESIAN_POINT ( 'NONE',  ( 0.3477690288713918276, -0.6692913385826773087, -0.1292274648535924053 ) ) ;
#15630 = CARTESIAN_POINT ( 'NONE',  ( 0.6430446194225728496, -0.004921259842519576551, 0.3153832671262227771 ) ) ;
#15631 = CARTESIAN_POINT ( 'NONE',  ( -0.7020997375328074108, -0.05778040916215522460, 0.4822834645669289988 ) ) ;
#15632 = CARTESIAN_POINT ( 'NONE',  ( -0.3392501089628019439, 0.1958661417322832554, -1.523602731462254889 ) ) ;
#15633 = CARTESIAN_POINT ( 'NONE',  ( -1.318897637795274802, 0.1660481256975885056, 0.3530559997133364547 ) ) ;
#15634 = CARTESIAN_POINT ( 'NONE',  ( 0.000000000000000000, 2.165354330708661568, 0.000000000000000000 ) ) ;
#15635 = CARTESIAN_POINT ( 'NONE',  ( 1.082677165354331228, 0.1660481256975883668, -0.3530559997133364547 ) ) ;
#15636 = CARTESIAN_POINT ( 'NONE',  ( 1.154855643044620184, -0.5023911411419708095, 0.1820866141732285504 ) ) ;
#15637 = VERTEX_POINT ( 'NONE', #58922 ) ;
#15638 = CARTESIAN_POINT ( 'NONE',  ( -0.3420746716998659953, -0.1974969037888706647, 0.1049868766404198905 ) ) ;
#15639 = CARTESIAN_POINT ( 'NONE',  ( -0.5708661417322825615, -0.5400638737290844871, 0.3530559997133364547 ) ) ;
#15640 = ORIENTED_EDGE ( 'NONE', *, *, #8676, .T. ) ;
#15642 = CIRCLE ( 'NONE', #30381, 1.122047244094488194 ) ;
#15641 = CARTESIAN_POINT ( 'NONE',  ( 0.2755905511811031494, -0.5511811023622047445, 6.969142054262312111E-17 ) ) ;
#15643 = CARTESIAN_POINT ( 'NONE',  ( -1.161417322834644716, -0.5400638737290845981, -0.3530559997133363437 ) ) ;
#15644 = CARTESIAN_POINT ( 'NONE',  ( 0.8989501312335963501, -0.6692913385826773087, -0.1292274648535924053 ) ) ;
#15645 = CARTESIAN_POINT ( 'NONE',  ( 0.7808398950131240079, -0.3162353388693405765, 0.4822834645669290543 ) ) ;
#15646 = CARTESIAN_POINT ( 'NONE',  ( -0.05905511811023545637, -0.5400638737290845981, -0.3530559997133363437 ) ) ;
#15647 = CARTESIAN_POINT ( 'NONE',  ( -0.3740157480314953431, 0.1660481256975885056, 0.3530559997133364547 ) ) ;
#15648 = CARTESIAN_POINT ( 'NONE',  ( -0.2867679344610365999, 0.2867679344610364889, -2.151574803149605586 ) ) ;
#15649 = CARTESIAN_POINT ( 'NONE',  ( -1.653543307086613234, -0.1870078740157480879, -0.4822834645669291653 ) ) ;
#15650 = CARTESIAN_POINT ( 'NONE',  ( -0.6036745406824141069, -0.6046776061558809534, -0.2411417322834644161 ) ) ;
#15651 = CARTESIAN_POINT ( 'NONE',  ( -0.6299212598425188991, -0.1870078740157480601, -0.3641732283464567677 ) ) ;
#15652 = CARTESIAN_POINT ( 'NONE',  ( 1.489501312335958172, -0.3162353388693405765, 0.4822834645669290543 ) ) ;
#15653 = DIRECTION ( 'NONE',  ( -0.000000000000000000, 1.000000000000000000, -0.000000000000000000 ) ) ;
#15654 = CARTESIAN_POINT ( 'NONE',  ( -1.023622047244094002, -0.1870078740157480879, -0.4822834645669291653 ) ) ;
#15655 = CARTESIAN_POINT ( 'NONE',  ( 0.3460692066303958092, 0.1998031496062993018, 0.1069553805774278027 ) ) ;
#15656 = CARTESIAN_POINT ( 'NONE',  ( 0.5118110236220478892, 0.2952755905511811885, 0.000000000000000000 ) ) ;
#15657 = CARTESIAN_POINT ( 'NONE',  ( 0.3460692066303959202, 0.1998031496062993295, -1.863517060367454015 ) ) ;
#15658 = LINE ( 'NONE', #75269, #30821 ) ;
#15659 = CARTESIAN_POINT ( 'NONE',  ( -0.1837270341207340729, 0.2306618581243847221, -0.2411417322834647770 ) ) ;
#15660 = CARTESIAN_POINT ( 'NONE',  ( -1.364829396325458521, -0.5023911411419708095, 0.1820866141732285504 ) ) ;
#15661 = CARTESIAN_POINT ( 'NONE',  ( 1.102362204724410155, -0.1870078740157480601, -0.3641732283464567677 ) ) ;
#15662 = CARTESIAN_POINT ( 'NONE',  ( -0.4724409448818898682, -8.678599364036362592E-17, -0.7460629921259841479 ) ) ;
#15663 = CARTESIAN_POINT ( 'NONE',  ( 1.272965879265092637, -0.3690944881889765550, -0.3153832671262227771 ) ) ;
#15664 = CARTESIAN_POINT ( 'NONE',  ( 0.7152230971128614723, -0.3162353388693409650, -0.4822834645669289433 ) ) ;
#15665 = CARTESIAN_POINT ( 'NONE',  ( -0.2891555358219909388, -0.2891555358219912164, -0.4507874015748032925 ) ) ;
#15666 = CARTESIAN_POINT ( 'NONE',  ( -0.4855643044619415427, -0.4281496062992124485, 0.4176697321401328655 ) ) ;
#15667 = FACE_OUTER_BOUND ( 'NONE', #60361, .T. ) ;
#15668 = CARTESIAN_POINT ( 'NONE',  ( 1.384514435695538337, -0.5511811023622046335, 0.09757992244046803654 ) ) ;
#15669 = CARTESIAN_POINT ( 'NONE',  ( -0.5249343832020990641, -0.6046776061558809534, -0.2411417322834644161 ) ) ;
#15670 = CARTESIAN_POINT ( 'NONE',  ( 0.2891555358219910499, -0.2891555358219909944, -0.4901574803149606474 ) ) ;
#15671 = EDGE_CURVE ( 'NONE', #25317, #63931, #1005, .T. ) ;
#15672 = CARTESIAN_POINT ( 'NONE',  ( 1.391076115485564868, 0.2306618581243847221, -0.2411417322834647770 ) ) ;
#15673 = CARTESIAN_POINT ( 'NONE',  ( 0.3149606299212603933, -0.1870078740157479769, 0.4822834645669291653 ) ) ;
#15674 = CARTESIAN_POINT ( 'NONE',  ( 0.5905511811023629321, 0.1771653543307087630, 0.000000000000000000 ) ) ;
#15675 = CARTESIAN_POINT ( 'NONE',  ( -0.3136911643361884883, 1.181168853316014955, -1.077377206225114126 ) ) ;
#15676 = CARTESIAN_POINT ( 'NONE',  ( 0.5249343832021005074, -0.5023911411419708095, 0.1820866141732285504 ) ) ;
#15677 = CARTESIAN_POINT ( 'NONE',  ( -0.06632061457837669372, -2.294479370626195693E-15, 0.3464511005275217603 ) ) ;
#15678 = CARTESIAN_POINT ( 'NONE',  ( 0.2925321140481932369, 0.2925321140481932369, -1.474409448818897905 ) ) ;
#15679 = CARTESIAN_POINT ( 'NONE',  ( 0.5708661417322842269, 0.1660481256975885056, 0.3530559997133364547 ) ) ;
#15680 = AXIS2_PLACEMENT_3D ( 'NONE', #72290, #9145, #40292 ) ;
#15681 = CARTESIAN_POINT ( 'NONE',  ( 0.3917322834645669549, 0.1049643490035304660, -0.9041994750656167090 ) ) ;
#15682 = VECTOR ( 'NONE', #81678, 39.37007874015748143 ) ;
#15683 = AXIS2_PLACEMENT_3D ( 'NONE', #66003, #14527, #64190 ) ;
#15684 = CARTESIAN_POINT ( 'NONE',  ( 0.2262115530851599166, 8.471767977567108961E-16, -0.4445507791589058955 ) ) ;
#15685 = CARTESIAN_POINT ( 'NONE',  ( 1.948818897637795367, 2.169649841009080787E-17, 5.524802951929911998 ) ) ;
#15686 = CARTESIAN_POINT ( 'NONE',  ( 0.2230971128608929543, -0.004921259842519870586, -0.3153832671262229437 ) ) ;
#15687 = CARTESIAN_POINT ( 'NONE',  ( 0.09186351706036827158, 0.05413385826771666132, 0.4176697321401328100 ) ) ;
#15688 = CARTESIAN_POINT ( 'NONE',  ( 1.489501312335958172, -0.2845877964562159024, 0.3641732283464567677 ) ) ;
#15689 = CARTESIAN_POINT ( 'NONE',  ( -1.240157480314959759, 0.07958543189024085140, 0.2665933059059887866 ) ) ;
#15690 = CARTESIAN_POINT ( 'NONE',  ( -1.279527559055116948, -0.5400638737290844871, 0.3530559997133364547 ) ) ;
#15691 = CARTESIAN_POINT ( 'NONE',  ( 0.6692913385826778638, -0.6692913385826771977, 8.415575281601705876E-17 ) ) ;
#15692 = CARTESIAN_POINT ( 'NONE',  ( 1.561679790026247350, 0.05413385826771626580, -0.4176697321401330321 ) ) ;
#15693 = CARTESIAN_POINT ( 'NONE',  ( -0.4724409448818899238, 0.1265901696524986964, -0.2670603674540682482 ) ) ;
#15694 = CARTESIAN_POINT ( 'NONE',  ( 0.5249343832021003964, 0.2306618581243847221, -0.2411417322834647770 ) ) ;
#15695 = AXIS2_PLACEMENT_3D ( 'NONE', #7044, #71440, #6204 ) ;
#15696 = CARTESIAN_POINT ( 'NONE',  ( 1.443569553805774897, -0.6046776061558809534, -0.2411417322834644161 ) ) ;
#15697 = CARTESIAN_POINT ( 'NONE',  ( 0.8333333333333340365, -0.6692913385826771977, 0.1292274648535927661 ) ) ;
#15698 = CARTESIAN_POINT ( 'NONE',  ( -1.679790026246718693, 0.1283753931104746893, -0.1820866141732285504 ) ) ;
#15699 = CARTESIAN_POINT ( 'NONE',  ( 1.200787401574803681, 0.07958543189024085140, 0.2665933059059887866 ) ) ;
#15700 = CARTESIAN_POINT ( 'NONE',  ( -1.646981627296586703, -0.08942795157527998196, 0.3641732283464567121 ) ) ;
#15701 = CARTESIAN_POINT ( 'NONE',  ( -0.9448818897637790704, -0.1870078740157480601, -0.3641732283464567677 ) ) ;
#15702 = CARTESIAN_POINT ( 'NONE',  ( 0.6955380577427828781, -0.004921259842519870586, -0.3153832671262229437 ) ) ;
#15703 = CARTESIAN_POINT ( 'NONE',  ( 0.2690288713910767848, 0.2952755905511811885, 0.1292274648535926551 ) ) ;
#15704 = CARTESIAN_POINT ( 'NONE',  ( 0.7545931758530188826, -0.6692913385826771977, 0.1292274648535927661 ) ) ;
#15705 = CARTESIAN_POINT ( 'NONE',  ( -0.2034120734908128059, 0.2952755905511811885, 0.1292274648535926551 ) ) ;
#15706 = CARTESIAN_POINT ( 'NONE',  ( 0.1181102362204730916, -0.5511811023622047445, 6.969142054262312111E-17 ) ) ;
#15707 = CARTESIAN_POINT ( 'NONE',  ( 1.332020997375328974, -0.05778040916215560624, -0.4822834645669293319 ) ) ;
#15708 = DIRECTION ( 'NONE',  ( 0.000000000000000000, 0.000000000000000000, 1.000000000000000000 ) ) ;
#15709 = CARTESIAN_POINT ( 'NONE',  ( -0.8070866141732276899, -0.5400638737290844871, 0.3530559997133364547 ) ) ;
#15711 = CARTESIAN_POINT ( 'NONE',  ( -0.3460692066303960868, 0.1998031496062990242, -0.8136482939632546652 ) ) ;
#15710 = DIRECTION ( 'NONE',  ( -1.000000000000000000, -0.000000000000000000, -0.000000000000000000 ) ) ;
#15712 = FACE_OUTER_BOUND ( 'NONE', #64445, .T. ) ;
#15713 = CARTESIAN_POINT ( 'NONE',  ( -0.6561679790026240244, 0.2306618581243847221, -0.2411417322834647770 ) ) ;
#15714 = CARTESIAN_POINT ( 'NONE',  ( -0.5905511811023615998, 0.2952755905511811885, 0.000000000000000000 ) ) ;
#15715 = EDGE_CURVE ( 'NONE', #55113, #37337, #32407, .T. ) ;
#15716 = CARTESIAN_POINT ( 'NONE',  ( 0.2362204724409451007, -0.4091458600556402980, 0.06561679790026246628 ) ) ;
#15717 = CARTESIAN_POINT ( 'NONE',  ( 0.3949938075777409963, 2.418639510665530435E-17, -2.322834645669291209 ) ) ;
#15718 = ORIENTED_EDGE ( 'NONE', *, *, #78407, .F. ) ;
#15719 = CARTESIAN_POINT ( 'NONE',  ( 0.6102362204724416372, 0.07958543189024071263, -0.2665933059059888421 ) ) ;
#15720 = CARTESIAN_POINT ( 'NONE',  ( -9.594673741351313045E-17, 0.3917322834645670104, -1.094488188976378007 ) ) ;
#15721 = CARTESIAN_POINT ( 'NONE',  ( 1.115485564304462551, 0.05413385826771666132, 0.4176697321401328100 ) ) ;
#15722 = CARTESIAN_POINT ( 'NONE',  ( 1.403614904275686858E-14, 1.537401574803149984, -3.937007874015761910 ) ) ;
#15723 = EDGE_CURVE ( 'NONE', #41461, #76146, #71219, .T. ) ;
#15724 = CARTESIAN_POINT ( 'NONE',  ( -1.181102362204723644, -0.1870078740157480601, -0.3641732283464567677 ) ) ;
#15725 = DIRECTION ( 'NONE',  ( 0.000000000000000000, 1.000000000000000000, 0.000000000000000000 ) ) ;
#15726 = CARTESIAN_POINT ( 'NONE',  ( -1.712598425196849572, 0.1660481256975885056, 0.3530559997133364547 ) ) ;
#15727 = CARTESIAN_POINT ( 'NONE',  ( -0.1958661417322836440, 0.3392501089628016664, -0.4081171671577935034 ) ) ;
#15728 = CARTESIAN_POINT ( 'NONE',  ( 0.1312335958005257930, 0.2306618581243847221, -0.2411417322834647770 ) ) ;
#15729 = CARTESIAN_POINT ( 'NONE',  ( -0.6167979002624665030, -0.004921259842519576551, 0.3153832671262227771 ) ) ;
#15730 = CARTESIAN_POINT ( 'NONE',  ( 0.9055118110236227702, -0.6692913385826771977, 8.415575281601705876E-17 ) ) ;
#15731 = CARTESIAN_POINT ( 'NONE',  ( -0.1902887139107604098, -0.6692913385826771977, 0.1292274648535927661 ) ) ;
#15732 = CARTESIAN_POINT ( 'NONE',  ( 2.795275590551181466, 2.362204724409448620, 0.000000000000000000 ) ) ;
#15733 = VECTOR ( 'NONE', #59443, 39.37007874015748143 ) ;
#15734 = CARTESIAN_POINT ( 'NONE',  ( -9.787531504996567848E-17, 0.3996062992125986035, -2.834645669291338432 ) ) ;
#15735 = CARTESIAN_POINT ( 'NONE',  ( 4.797336870675656522E-17, -0.3917322834645670659, -1.492801468012810329 ) ) ;
#15736 = CARTESIAN_POINT ( 'NONE',  ( 0.9645669291338591078, -0.5400638737290845981, -0.3530559997133363437 ) ) ;
#15737 = CIRCLE ( 'NONE', #21066, 2.559055118110236560 ) ;
#15738 = CARTESIAN_POINT ( 'NONE',  ( 0.2034120734908142214, 0.2952755905511810774, -0.1292274648535930714 ) ) ;
#15739 = CARTESIAN_POINT ( 'NONE',  ( -0.9448818897637790704, -0.1870078740157480879, -0.4822834645669291653 ) ) ;
#15740 = CARTESIAN_POINT ( 'NONE',  ( 1.115485564304462551, 0.05413385826771666132, 0.4176697321401328100 ) ) ;
#15741 = CARTESIAN_POINT ( 'NONE',  ( 0.9711286089238851948, -0.6046776061558809534, -0.2411417322834644161 ) ) ;
#15742 = CARTESIAN_POINT ( 'NONE',  ( -0.3392501089628019995, 0.1958661417322832277, -1.055774278215223294 ) ) ;
#15743 = CARTESIAN_POINT ( 'NONE',  ( -0.3083989501312330295, -0.05778040916215522460, 0.4822834645669289988 ) ) ;
#15744 = CARTESIAN_POINT ( 'NONE',  ( 0.5905511811023629321, 0.2952755905511811885, 0.000000000000000000 ) ) ;
#15745 = CARTESIAN_POINT ( 'NONE',  ( 0.03280839895013198948, -0.6692913385826773087, -0.1292274648535924053 ) ) ;
#15746 = CARTESIAN_POINT ( 'NONE',  ( 0.7808398950131241190, -0.08942795157528024563, -0.3641732283464568787 ) ) ;
#15747 = CARTESIAN_POINT ( 'NONE',  ( -1.397637795275589623, 0.1660481256975885056, 0.3530559997133364547 ) ) ;
#15748 = CARTESIAN_POINT ( 'NONE',  ( -0.3811349131313276350, 1.253490138500164441, -2.704685859045969476 ) ) ;
#15749 = CARTESIAN_POINT ( 'NONE',  ( 0.3215223097112867578, -0.05778040916215522460, 0.4822834645669289988 ) ) ;
#15750 = DIRECTION ( 'NONE',  ( 1.408710688920637755E-15, -1.000000000000000000, 4.918487082195260922E-30 ) ) ;
#15751 = ADVANCED_FACE ( 'NONE', ( #1281 ), #26930, .F. ) ;
#15752 = CARTESIAN_POINT ( 'NONE',  ( -0.3392501089628017219, -0.1958661417322836718, -2.249343832020997525 ) ) ;
#15753 = ORIENTED_EDGE ( 'NONE', *, *, #59403, .F. ) ;
#15754 = ORIENTED_EDGE ( 'NONE', *, *, #79927, .F. ) ;
#15755 = CARTESIAN_POINT ( 'NONE',  ( 0.9842519685039378130, -0.6692913385826771977, 8.415575281601705876E-17 ) ) ;
#15756 = CARTESIAN_POINT ( 'NONE',  ( 0.5249343832021003964, 0.1283753931104746893, -0.1820866141732285504 ) ) ;
#15758 = CARTESIAN_POINT ( 'NONE',  ( 0.6183353934921186346, 0.02791078216816508459, -0.4328096321851889194 ) ) ;
#15757 = CARTESIAN_POINT ( 'NONE',  ( -1.614173228346456712, 2.401574803149606474, 0.1372047244094477536 ) ) ;
#15759 = CARTESIAN_POINT ( 'NONE',  ( 0.4177787735907000366, 0.000000000000000000, -1.874132239285499324 ) ) ;
#15760 = SURFACE_SIDE_STYLE ('',( #41815 ) ) ;
#15761 = CARTESIAN_POINT ( 'NONE',  ( 0.1958661417322836440, -0.3392501089628017219, -1.278871391076115582 ) ) ;
#15762 = EDGE_CURVE ( 'NONE', #25718, #2797, #52089, .T. ) ;
#15763 = CARTESIAN_POINT ( 'NONE',  ( -9.787531504996566615E-17, 0.3996062992125985480, -2.281496062992125928 ) ) ;
#15764 = CARTESIAN_POINT ( 'NONE',  ( -0.9842519685039360366, 0.2952755905511811885, 0.000000000000000000 ) ) ;
#15765 = CARTESIAN_POINT ( 'NONE',  ( -0.6102362204724400829, 0.1660481256975885056, 0.3530559997133364547 ) ) ;
#15766 = CARTESIAN_POINT ( 'NONE',  ( 1.095800524934383846, -0.3162353388693405765, 0.4822834645669290543 ) ) ;
#15767 = ORIENTED_EDGE ( 'NONE', *, *, #25250, .T. ) ;
#15768 = CARTESIAN_POINT ( 'NONE',  ( 1.167979002624672580, 0.05413385826771626580, -0.4176697321401330321 ) ) ;
#15769 = DIRECTION ( 'NONE',  ( 0.000000000000000000, -1.000000000000000000, 0.000000000000000000 ) ) ;
#15770 = ITEM_DEFINED_TRANSFORMATION ( 'NONE', 'NONE', #4661,  #22098 ) ;
#15771 = CARTESIAN_POINT ( 'NONE',  ( 1.633858267716535639, -0.4536011799217367080, 0.2665933059059888421 ) ) ;
#15772 = CARTESIAN_POINT ( 'NONE',  ( -0.3996062992125985480, -7.340648628747423112E-17, -2.005905511811023612 ) ) ;
#15773 = CARTESIAN_POINT ( 'NONE',  ( -1.148293963254592542, 0.1771653543307087630, 0.09757992244046791164 ) ) ;
#15774 = EDGE_CURVE ( 'NONE', #36844, #72992, #36037, .T. ) ;
#15775 = CARTESIAN_POINT ( 'NONE',  ( 1.813482582612293559, 2.755905511811024056, 0.5314960629921260393 ) ) ;
#15776 = CARTESIAN_POINT ( 'NONE',  ( 0.3871391076115493490, -0.3162353388693405765, 0.4822834645669290543 ) ) ;
#15777 = PLANE ( 'NONE',  #25058 ) ;
#15778 = CARTESIAN_POINT ( 'NONE',  ( -1.259842519685038686, -0.1870078740157479769, 0.3641732283464567677 ) ) ;
#15779 = CARTESIAN_POINT ( 'NONE',  ( 0.9711286089238851948, -0.6046776061558809534, -0.2411417322834644161 ) ) ;
#15780 = CARTESIAN_POINT ( 'NONE',  ( 1.286089238845145033, 0.1283753931104748280, 0.1820866141732283561 ) ) ;
#15781 = CARTESIAN_POINT ( 'NONE',  ( 0.1049643490035304522, -0.3917322834645668994, -1.425177534611861585 ) ) ;
#15782 = CARTESIAN_POINT ( 'NONE',  ( -0.8398950131233589023, -0.5023911411419708095, -0.1820866141732282451 ) ) ;
#15783 = CARTESIAN_POINT ( 'NONE',  ( 1.443569553805774897, -0.6046776061558809534, -0.2411417322834644161 ) ) ;
#15784 = CARTESIAN_POINT ( 'NONE',  ( 2.571698080334759329, 1.622209144264170844, -0.4670403427556020226 ) ) ;
#15785 = CARTESIAN_POINT ( 'NONE',  ( -0.04593175853018302557, -0.6692913385826773087, -0.1292274648535924053 ) ) ;
#15786 = CARTESIAN_POINT ( 'NONE',  ( -1.541994750656167090, -0.5511811023622048555, -0.09757992244046775898 ) ) ;
#15787 = CARTESIAN_POINT ( 'NONE',  ( -0.1706036745406816491, -0.3690944881889763329, 0.3153832671262228327 ) ) ;
#15788 = CARTESIAN_POINT ( 'NONE',  ( -0.3543307086614165824, -0.6692913385826771977, 8.415575281601705876E-17 ) ) ;
#15789 = CARTESIAN_POINT ( 'NONE',  ( -1.594488188976377119, 0.07958543189024071263, -0.2665933059059888421 ) ) ;
#15790 = CARTESIAN_POINT ( 'NONE',  ( -0.2867679344610367109, 0.2867679344610365444, -0.3313841451781647240 ) ) ;
#15791 = CARTESIAN_POINT ( 'NONE',  ( 0.3412073490813655186, 0.2306618581243848609, 0.2411417322834645549 ) ) ;
#15792 = CIRCLE ( 'NONE', #43925, 2.362204724409449064 ) ;
#15793 = CARTESIAN_POINT ( 'NONE',  ( 0.4724409448818898127, -0.1265901696524988629, -0.2690288713910760632 ) ) ;
#15794 = CIRCLE ( 'NONE', #10439, 1.289370078740159409 ) ;
#15795 = CARTESIAN_POINT ( 'NONE',  ( -0.4724409448818899238, 0.1265901696524986686, -1.684383202099737353 ) ) ;
#15796 = CARTESIAN_POINT ( 'NONE',  ( -0.8333333333333323711, -0.6692913385826773087, -0.1292274648535924053 ) ) ;
#15797 = CARTESIAN_POINT ( 'NONE',  ( -0.2230971128608915943, -0.3690944881889765550, -0.3153832671262227771 ) ) ;
#15798 = CARTESIAN_POINT ( 'NONE',  ( -1.548556430446193399, -0.6046776061558809534, -0.2411417322834644161 ) ) ;
#15799 = CARTESIAN_POINT ( 'NONE',  ( -0.1181102362204717315, -0.6692913385826771977, 8.415575281601705876E-17 ) ) ;
#15800 = CARTESIAN_POINT ( 'NONE',  ( 0.6102362204724416372, 0.07958543189024071263, -0.2665933059059888421 ) ) ;
#15801 = CARTESIAN_POINT ( 'NONE',  ( -0.8398950131233589023, -0.5023911411419708095, -0.1820866141732282451 ) ) ;
#15802 = CARTESIAN_POINT ( 'NONE',  ( -0.8530183727034112984, -0.4281496062992127816, -0.4176697321401328100 ) ) ;
#15803 = CARTESIAN_POINT ( 'NONE',  ( -1.692913385826770645, 0.2952755905511811885, 0.000000000000000000 ) ) ;
#15804 = CARTESIAN_POINT ( 'NONE',  ( 1.515748031496063408, 0.1660481256975885056, 0.3530559997133364547 ) ) ;
#15805 = CARTESIAN_POINT ( 'NONE',  ( 0.01711285633636193751, 1.063222675620814295, 1.850607425301893372 ) ) ;
#15806 = CARTESIAN_POINT ( 'NONE',  ( 0.6758530183727039509, -0.5511811023622046335, 0.09757992244046803654 ) ) ;
#15807 = PRODUCT_DEFINITION_SHAPE ( 'NONE', 'NONE',  #83328 ) ;
#15808 = CARTESIAN_POINT ( 'NONE',  ( 0.6955380577427828781, -0.4281496062992124485, 0.4176697321401328655 ) ) ;
#15809 = CARTESIAN_POINT ( 'NONE',  ( -2.362204724409448620, 1.724409448818898127, -0.5118110236220719811 ) ) ;
#15810 = CARTESIAN_POINT ( 'NONE',  ( 1.207349081364829990, -0.5023911411419708095, -0.1820866141732282451 ) ) ;
#15811 = ORIENTED_EDGE ( 'NONE', *, *, #67121, .T. ) ;
#15813 = B_SPLINE_CURVE_WITH_KNOTS ( 'NONE', 3,
 ( #81739, #45042, #12258, #57259 ),
 .UNSPECIFIED., .F., .F.,
 ( 4, 4 ),
 ( 0.000000000000000000, 0.001493228121701170282 ),
 .UNSPECIFIED. ) ;
#15812 = CARTESIAN_POINT ( 'NONE',  ( -0.7874015748031489847, -0.1870078740157480879, -0.4822834645669291653 ) ) ;
#15814 = CARTESIAN_POINT ( 'NONE',  ( -0.3949938075777411073, 0.1058382717557497660, 0.2053805774278214813 ) ) ;
#15815 = CARTESIAN_POINT ( 'NONE',  ( -1.102362204724408601, -0.1870078740157480601, -0.3641732283464567677 ) ) ;
#15816 = CARTESIAN_POINT ( 'NONE',  ( -0.4068241469816264999, -0.4281496062992124485, 0.4176697321401328655 ) ) ;
#15817 = CARTESIAN_POINT ( 'NONE',  ( 0.2165354330708668673, 0.1660481256975883668, -0.3530559997133364547 ) ) ;
#15818 = CARTESIAN_POINT ( 'NONE',  ( -1.640419947506561060, -0.3690944881889765550, -0.3153832671262227771 ) ) ;
#15819 = CARTESIAN_POINT ( 'NONE',  ( -0.3996062992125986590, 0.1070741851644051723, -2.314304461942256808 ) ) ;
#15820 = CARTESIAN_POINT ( 'NONE',  ( -1.463254593175852492, -0.6692913385826773087, -0.1292274648535924053 ) ) ;
#15821 = CARTESIAN_POINT ( 'NONE',  ( 0.2952755905511819101, 0.1660481256975883668, -0.3530559997133364547 ) ) ;
#15822 = CARTESIAN_POINT ( 'NONE',  ( 0.1706036745406830368, -0.4281496062992127816, -0.4176697321401328100 ) ) ;
#15823 = CARTESIAN_POINT ( 'NONE',  ( 1.338582677165355062, -0.1870078740157480879, -0.4822834645669291653 ) ) ;
#15825 = EDGE_CURVE ( 'NONE', #8695, #64186, #61408, .T. ) ;
#15824 = CARTESIAN_POINT ( 'NONE',  ( 1.686351706036745890, 0.2952755905511811885, 0.1292274648535926551 ) ) ;
#15826 = CARTESIAN_POINT ( 'NONE',  ( -0.1070741851644056997, 0.3996062992125986035, -1.896325459317584894 ) ) ;
#15827 = CARTESIAN_POINT ( 'NONE',  ( 0.3949938075777411073, -0.1058382717557499464, -1.213910761154855633 ) ) ;
#15828 = CARTESIAN_POINT ( 'NONE',  ( -0.3996062992125987146, 0.1070741851644051862, -2.552493438320210029 ) ) ;
#15829 = DIRECTION ( 'NONE',  ( 0.000000000000000000, 1.000000000000000000, 0.000000000000000000 ) ) ;
#15830 = CARTESIAN_POINT ( 'NONE',  ( -0.2867679344610364334, -0.2867679344610367109, -0.3661417322834645272 ) ) ;
#15831 = CARTESIAN_POINT ( 'NONE',  ( -0.1706036745406816491, -0.3690944881889763329, 0.3153832671262228327 ) ) ;
#15832 = CARTESIAN_POINT ( 'NONE',  ( -0.1443569553805768291, 0.05413385826771666132, 0.4176697321401328100 ) ) ;
#15833 = CARTESIAN_POINT ( 'NONE',  ( 0.7874015748031503170, -0.1870078740157479769, 0.4822834645669291653 ) ) ;
#15834 = CARTESIAN_POINT ( 'NONE',  ( 0.3420746716998660508, -0.1974969037888704149, -2.229002624671915900 ) ) ;
#15835 = CARTESIAN_POINT ( 'NONE',  ( 0.1443569553805781891, -0.004921259842519870586, -0.3153832671262229437 ) ) ;
#15836 = CARTESIAN_POINT ( 'NONE',  ( -1.082677165354329896, -0.5400638737290845981, -0.3530559997133363437 ) ) ;
#15837 = CARTESIAN_POINT ( 'NONE',  ( 1.049868766404200127, -0.6046776061558809534, -0.2411417322834644161 ) ) ;
#15838 = CARTESIAN_POINT ( 'NONE',  ( -0.4724409448818898682, -8.678599364036362592E-17, -2.244094488188976388 ) ) ;
#15839 = DIRECTION ( 'NONE',  ( -0.8050726085550603539, -2.493067783899206833E-16, -0.5931762764594944448 ) ) ;
#15840 = VERTEX_POINT ( 'NONE', #41231 ) ;
#15841 = ORIENTED_EDGE ( 'NONE', *, *, #73907, .T. ) ;
#15842 = CARTESIAN_POINT ( 'NONE',  ( 1.135170603674541256, 0.2952755905511811885, 0.1292274648535926551 ) ) ;
#15843 = CARTESIAN_POINT ( 'NONE',  ( -1.496062992125983815, -0.1870078740157480879, -0.4822834645669291653 ) ) ;
#15845 = CARTESIAN_POINT ( 'NONE',  ( -0.9973753280839886548, 0.2306618581243848609, 0.2411417322834645549 ) ) ;
#15844 = CARTESIAN_POINT ( 'NONE',  ( -1.089238845144356427, -0.3690944881889765550, -0.3153832671262227771 ) ) ;
#15846 = CARTESIAN_POINT ( 'NONE',  ( -0.1049643490035301746, -0.3917322834645670659, -2.829377009677478405 ) ) ;
#15847 = CARTESIAN_POINT ( 'NONE',  ( 1.193521905106662784, 3.421639014772782816E-16, 0.3464511005275203726 ) ) ;
#15848 = CARTESIAN_POINT ( 'NONE',  ( 1.076115485564305141, 0.2306618581243847221, -0.2411417322834647770 ) ) ;
#15849 = CARTESIAN_POINT ( 'NONE',  ( 0.4091458600556404646, -0.2362204724409448231, -2.467191601049868677 ) ) ;
#15850 = CARTESIAN_POINT ( 'NONE',  ( 0.02624671916010564918, 0.2306618581243848609, 0.2411417322834645549 ) ) ;
#15851 = CARTESIAN_POINT ( 'NONE',  ( -0.6430446194225716283, -0.4281496062992124485, 0.4176697321401328655 ) ) ;
#15852 = CARTESIAN_POINT ( 'NONE',  ( -1.450131233595799651, 0.2952755905511810774, -0.1292274648535930714 ) ) ;
#15853 = CARTESIAN_POINT ( 'NONE',  ( 0.2867679344610365999, 0.2867679344610365999, -0.2224409448818898127 ) ) ;
#15854 = CARTESIAN_POINT ( 'NONE',  ( 0.05249343832021075018, 0.2306618581243847221, -0.2411417322834647770 ) ) ;
#15855 = CARTESIAN_POINT ( 'NONE',  ( 0.1049643490035303689, 0.3917322834645670104, -2.347769028871391050 ) ) ;
#15856 = CARTESIAN_POINT ( 'NONE',  ( -1.332020997375327642, -0.08942795157527998196, 0.3641732283464567121 ) ) ;
#15857 = VERTEX_POINT ( 'NONE', #78718 ) ;
#15858 = CARTESIAN_POINT ( 'NONE',  ( -0.3420746716998659953, -0.1974969037888706647, -2.099737532808398921 ) ) ;
#15859 = ORIENTED_EDGE ( 'NONE', *, *, #70225, .F. ) ;
#15860 = DIRECTION ( 'NONE',  ( 0.000000000000000000, 0.000000000000000000, 1.000000000000000000 ) ) ;
#15861 = CONICAL_SURFACE ( 'NONE', #75025, 0.1978346456692914035, 0.8726646259971700959 ) ;
#15862 = CARTESIAN_POINT ( 'NONE',  ( 1.601049868766404982, 0.1283753931104748280, 0.1820866141732283561 ) ) ;
#15863 = CARTESIAN_POINT ( 'NONE',  ( 0.3460692066303959757, -0.1998031496062991907, -0.8923884514435694859 ) ) ;
#15864 = CARTESIAN_POINT ( 'NONE',  ( -1.653543307086613234, -0.1870078740157480879, -0.4822834645669291653 ) ) ;
#15865 = CARTESIAN_POINT ( 'NONE',  ( -1.489501312335957062, -0.3162353388693409650, -0.4822834645669289433 ) ) ;
#15866 = CARTESIAN_POINT ( 'NONE',  ( -0.9908136482939625678, 0.2952755905511811885, 0.1292274648535926551 ) ) ;
#15867 = CARTESIAN_POINT ( 'NONE',  ( -0.3836918680457887532, -2.191421614605370878E-15, 0.4445507791589071167 ) ) ;
#15868 = CARTESIAN_POINT ( 'NONE',  ( 0.3392501089628018329, 0.1958661417322835607, 0.09908136482939623735 ) ) ;
#15869 = CARTESIAN_POINT ( 'NONE',  ( -0.2493438320209966919, -0.3690944881889763329, 0.3153832671262228327 ) ) ;
#15870 = CARTESIAN_POINT ( 'NONE',  ( -0.7217847769028863381, -0.004921259842519870586, -0.3153832671262229437 ) ) ;
#15871 = CARTESIAN_POINT ( 'NONE',  ( -1.167979002624671470, 0.05413385826771666132, 0.4176697321401328100 ) ) ;
#15872 = CARTESIAN_POINT ( 'NONE',  ( 0.4199475065616803948, -0.6046776061558809534, -0.2411417322834644161 ) ) ;
#15873 = CARTESIAN_POINT ( 'NONE',  ( -0.7414698162729651543, -0.6692913385826771977, 0.1292274648535927661 ) ) ;
#15874 = CARTESIAN_POINT ( 'NONE',  ( 0.5314960629921395840, 2.725419031863056674, -3.884512598959603658 ) ) ;
#15875 = ORIENTED_EDGE ( 'NONE', *, *, #58155, .T. ) ;
#15876 = CARTESIAN_POINT ( 'NONE',  ( -1.594488188976377119, 0.1660481256975883668, -0.3530559997133364547 ) ) ;
#15877 = DIRECTION ( 'NONE',  ( 0.000000000000000000, -1.000000000000000000, 0.000000000000000000 ) ) ;
#15878 = CARTESIAN_POINT ( 'NONE',  ( 0.3458507752293908943, -0.3458507752293908943, -1.200787401574803015 ) ) ;
#15879 = PLANE ( 'NONE',  #4915 ) ;
#15880 = CARTESIAN_POINT ( 'NONE',  ( -0.1958661417322834220, -0.3392501089628018884, -0.8451443569553805935 ) ) ;
#15881 = CARTESIAN_POINT ( 'NONE',  ( -0.3917322834645671215, 0.1049643490035301469, -2.479658792650918375 ) ) ;
#15882 = CARTESIAN_POINT ( 'NONE',  ( -0.5774278215223089816, -0.6046776061558807314, 0.2411417322834647770 ) ) ;
#15883 = CARTESIAN_POINT ( 'NONE',  ( 1.443569553805774897, -0.6046776061558809534, -0.2411417322834644161 ) ) ;
#15884 = CARTESIAN_POINT ( 'NONE',  ( -0.1070741851644051862, -0.3996062992125986590, -0.3064304461942257141 ) ) ;
#15885 = CARTESIAN_POINT ( 'NONE',  ( -0.5314960629921373636, 2.755905511811024056, 3.264097702071371288 ) ) ;
#15886 = CARTESIAN_POINT ( 'NONE',  ( -1.325459317585300889, -0.4281496062992127816, -0.4176697321401328100 ) ) ;
#15887 = CARTESIAN_POINT ( 'NONE',  ( -0.6430446194225716283, -0.4281496062992124485, 0.4176697321401328655 ) ) ;
#15888 = CARTESIAN_POINT ( 'NONE',  ( 0.1049643490035304522, -0.3917322834645668994, -0.1653350149268222880 ) ) ;
#15889 = CARTESIAN_POINT ( 'NONE',  ( 0.3215223097112867578, -0.08942795157527998196, 0.3641732283464567121 ) ) ;
#15890 = CARTESIAN_POINT ( 'NONE',  ( 0.1958661417322834775, 0.3392501089628018884, -0.3864829396325459854 ) ) ;
#15891 = CARTESIAN_POINT ( 'NONE',  ( 0.1509186351706045259, -0.08942795157528024563, -0.3641732283464568787 ) ) ;
#15892 = CARTESIAN_POINT ( 'NONE',  ( 1.082677165354331228, -0.4536011799217367080, 0.2665933059059888421 ) ) ;
#15893 = CARTESIAN_POINT ( 'NONE',  ( 0.8005249343832027131, 0.05413385826771666132, 0.4176697321401328100 ) ) ;
#15894 = UNCERTAINTY_MEASURE_WITH_UNIT (LENGTH_MEASURE( 1.000000000000000082E-05 ), #28354, 'distance_accuracy_value', 'NONE');
#15895 = CARTESIAN_POINT ( 'NONE',  ( -0.1837270341207340729, 0.1283753931104746893, -0.1820866141732285504 ) ) ;
#15896 = CARTESIAN_POINT ( 'NONE',  ( -0.1049643490035302024, -0.3917322834645671215, -2.426509186351705427 ) ) ;
#15897 = CARTESIAN_POINT ( 'NONE',  ( 1.397637795275591177, -0.5400638737290844871, 0.3530559997133364547 ) ) ;
#15898 = CARTESIAN_POINT ( 'NONE',  ( -1.351706036745406347, -0.3690944881889763329, 0.3153832671262228327 ) ) ;
#15899 = CARTESIAN_POINT ( 'NONE',  ( -0.2362204724409447953, -0.4091458600556404646, -0.2998687664041995160 ) ) ;
#15900 = CARTESIAN_POINT ( 'NONE',  ( -0.7874015748031489847, -0.1870078740157480601, -0.3641732283464567677 ) ) ;
#15901 = CARTESIAN_POINT ( 'NONE',  ( -0.006561679790025524116, -0.05778040916215560624, -0.4822834645669293319 ) ) ;
#15902 = CARTESIAN_POINT ( 'NONE',  ( -0.3438254193631122835, -0.3704879858182167918, -0.01311675794578955577 ) ) ;
#15903 = CARTESIAN_POINT ( 'NONE',  ( 0.3937007874015754361, -0.1870078740157480601, -0.3641732283464567677 ) ) ;
#15904 = CARTESIAN_POINT ( 'NONE',  ( -0.4658792650918627265, -0.08942795157527998196, 0.3641732283464567121 ) ) ;
#15905 = CARTESIAN_POINT ( 'NONE',  ( -0.9055118110236215490, -0.6692913385826771977, 8.415575281601705876E-17 ) ) ;
#15906 = DIRECTION ( 'NONE',  ( 1.000000000000000000, -1.445602896647338917E-16, 0.000000000000000000 ) ) ;
#15907 = CARTESIAN_POINT ( 'NONE',  ( 1.348312163386739426, 0.2755905511811023723, 0.7386866130305692613 ) ) ;
#15908 = CARTESIAN_POINT ( 'NONE',  ( 0.3018372703412079971, 0.05413385826771626580, -0.4176697321401330321 ) ) ;
#15909 = CARTESIAN_POINT ( 'NONE',  ( 0.2925321140481932369, -0.2925321140481931814, -1.592519685039370358 ) ) ;
#15910 = CARTESIAN_POINT ( 'NONE',  ( 1.377952755905512472, -0.6692913385826771977, 8.415575281601705876E-17 ) ) ;
#15911 = CARTESIAN_POINT ( 'NONE',  ( -0.2755905511811018171, 0.1771653543307087630, 0.000000000000000000 ) ) ;
#15912 = VECTOR ( 'NONE', #1400, 39.37007874015748143 ) ;
#15913 = CARTESIAN_POINT ( 'NONE',  ( -0.1509186351706028884, -0.05778040916215522460, 0.4822834645669289988 ) ) ;
#15914 = CARTESIAN_POINT ( 'NONE',  ( -1.601049868766403650, 0.2306618581243847221, -0.2411417322834647770 ) ) ;
#15915 = CARTESIAN_POINT ( 'NONE',  ( 1.601049868766404982, -0.6046776061558809534, -0.2411417322834644161 ) ) ;
#15916 = CARTESIAN_POINT ( 'NONE',  ( 1.469816272965879911, -0.6046776061558807314, 0.2411417322834647770 ) ) ;
#15917 = CARTESIAN_POINT ( 'NONE',  ( -0.7480314960629914633, 0.1771653543307087630, 0.000000000000000000 ) ) ;
#15919 = EDGE_CURVE ( 'NONE', #50774, #29467, #79972, .T. ) ;
#15918 = CARTESIAN_POINT ( 'NONE',  ( -0.1998031496062994405, 0.3460692066303957537, -0.2473753280839895152 ) ) ;
#15920 = CARTESIAN_POINT ( 'NONE',  ( 0.3996062992125986035, 0.1070741851644054776, -0.4396325459317584339 ) ) ;
#15921 = CARTESIAN_POINT ( 'NONE',  ( 0.3917322834645670659, 2.398668435337828261E-17, -2.792014066438007092 ) ) ;
#15922 = CARTESIAN_POINT ( 'NONE',  ( 1.627296587926509996, -0.5023911411419708095, 0.1820866141732285504 ) ) ;
#15923 = CARTESIAN_POINT ( 'NONE',  ( 1.200787401574803681, -0.4536011799217368745, -0.2665933059059886201 ) ) ;
#15924 = CARTESIAN_POINT ( 'NONE',  ( -1.614173228346456268, -0.6692913385826771977, 8.415575281601705876E-17 ) ) ;
#15925 = CARTESIAN_POINT ( 'NONE',  ( 0.7874015748031503170, -0.1870078740157479769, 0.4822834645669291653 ) ) ;
#15926 = CARTESIAN_POINT ( 'NONE',  ( 0.3949938075777408852, 0.1058382717557500435, -0.8313648293963256108 ) ) ;
#15927 = CARTESIAN_POINT ( 'NONE',  ( 1.154855643044620184, -0.5023911411419708095, 0.1820866141732285504 ) ) ;
#15928 = CARTESIAN_POINT ( 'NONE',  ( -0.08530183727034056085, -0.3162353388693405765, 0.4822834645669290543 ) ) ;
#15929 = CARTESIAN_POINT ( 'NONE',  ( -0.4986876640419939388, 0.2306618581243847221, -0.2411417322834647770 ) ) ;
#15930 = DIRECTION ( 'NONE',  ( -1.000000000000000000, -9.738798461624180871E-16, -8.881784197001252323E-16 ) ) ;
#15931 = CARTESIAN_POINT ( 'NONE',  ( -0.3458507752293906723, -0.3458507752293910609, -0.8464566929133857665 ) ) ;
#15932 = CARTESIAN_POINT ( 'NONE',  ( -0.2925321140481930704, -0.2925321140481933480, -2.263779527559055094 ) ) ;
#15933 = CARTESIAN_POINT ( 'NONE',  ( 0.4461942257217855201, -0.5023911411419708095, 0.1820866141732285504 ) ) ;
#15934 = ORIENTED_EDGE ( 'NONE', *, *, #17054, .F. ) ;
#15935 = CARTESIAN_POINT ( 'NONE',  ( -0.3392501089628017219, -0.1958661417322836995, -0.3641925441282957698 ) ) ;
#15936 = EDGE_LOOP ( 'NONE', ( #78765, #66471, #13569, #11058 ) ) ;
#15937 = CARTESIAN_POINT ( 'NONE',  ( -0.5183727034120726440, -0.6692913385826773087, -0.1292274648535924053 ) ) ;
#15938 = CARTESIAN_POINT ( 'NONE',  ( 0.8333333333333340365, 0.2952755905511810774, -0.1292274648535930714 ) ) ;
#15939 = CARTESIAN_POINT ( 'NONE',  ( 0.1968503937007881344, -0.6692913385826771977, 8.415575281601705876E-17 ) ) ;
#15940 = CARTESIAN_POINT ( 'NONE',  ( -0.3674540682414689785, 0.1283753931104748280, 0.1820866141732283561 ) ) ;
#15941 = CARTESIAN_POINT ( 'NONE',  ( 0.8858267716535438430, 0.1660481256975885056, 0.3530559997133364547 ) ) ;
#15942 = CARTESIAN_POINT ( 'NONE',  ( -0.9973753280839886548, 0.2306618581243848609, 0.2411417322834645549 ) ) ;
#15943 = CARTESIAN_POINT ( 'NONE',  ( -0.4265091863517051496, 0.2952755905511810774, -0.1292274648535930714 ) ) ;
#15944 = CARTESIAN_POINT ( 'NONE',  ( -0.7611548556430438595, 0.2306618581243848609, 0.2411417322834645549 ) ) ;
#15945 = CARTESIAN_POINT ( 'NONE',  ( 1.377952755905512472, -0.6692913385826771977, 8.415575281601705876E-17 ) ) ;
#15946 = CARTESIAN_POINT ( 'NONE',  ( 0.7808398950131240079, -0.3162353388693405765, 0.4822834645669290543 ) ) ;
#15947 = CARTESIAN_POINT ( 'NONE',  ( 0.7152230971128616943, -0.05778040916215522460, 0.4822834645669289988 ) ) ;
#15948 = CARTESIAN_POINT ( 'NONE',  ( -0.2867679344610364334, -0.2867679344610367109, -0.5236220472440944462 ) ) ;
#15949 = CARTESIAN_POINT ( 'NONE',  ( 0.08530183727034192087, -0.08942795157527998196, 0.3641732283464567121 ) ) ;
#15950 = ORIENTED_EDGE ( 'NONE', *, *, #21903, .T. ) ;
#15951 = CARTESIAN_POINT ( 'NONE',  ( -0.3420746716998659953, -0.1974969037888706647, -0.9973753280839895430 ) ) ;
#15952 = ORIENTED_EDGE ( 'NONE', *, *, #38343, .F. ) ;
#15953 = CARTESIAN_POINT ( 'NONE',  ( -0.7283464566929126471, 0.07958543189024071263, -0.2665933059059888421 ) ) ;
#15954 = CARTESIAN_POINT ( 'NONE',  ( -0.5446194225721777693, -0.05778040916215522460, 0.4822834645669289988 ) ) ;
#15955 = CARTESIAN_POINT ( 'NONE',  ( 0.3996062992125986035, 2.446882876249141962E-17, 0.03937007874015747283 ) ) ;
#15956 = CARTESIAN_POINT ( 'NONE',  ( -0.3740157480314953431, -0.5400638737290845981, -0.3530559997133363437 ) ) ;
#15957 = CARTESIAN_POINT ( 'NONE',  ( -0.4265091863517051496, 0.2952755905511810774, -0.1292274648535930714 ) ) ;
#15958 = CARTESIAN_POINT ( 'NONE',  ( -1.082677165354329896, -0.5400638737290845981, -0.3530559997133363437 ) ) ;
#15959 = CARTESIAN_POINT ( 'NONE',  ( -1.213910761154854745, 0.2952755905511810774, -0.1292274648535930714 ) ) ;
#15960 = CARTESIAN_POINT ( 'NONE',  ( 1.115485564304462551, -0.3690944881889765550, -0.3153832671262227771 ) ) ;
#15961 = CARTESIAN_POINT ( 'NONE',  ( 0.4359958488159307310, 1.724409448818897905, 3.937007874015793885 ) ) ;
#15962 = CARTESIAN_POINT ( 'NONE',  ( 0.2710828156362889985, 0.1173918767474883690, 5.835147349599718147 ) ) ;
#15963 = CARTESIAN_POINT ( 'NONE',  ( 0.5314960629921264834, 0.07958543189024071263, -0.2665933059059888421 ) ) ;
#15964 = CARTESIAN_POINT ( 'NONE',  ( -0.1509186351706028884, -0.3162353388693409650, -0.4822834645669289433 ) ) ;
#15965 = CARTESIAN_POINT ( 'NONE',  ( 0.1377952755905518800, 0.1660481256975883668, -0.3530559997133364547 ) ) ;
#15966 = VERTEX_POINT ( 'NONE', #34922 ) ;
#15967 = CARTESIAN_POINT ( 'NONE',  ( 0.1070741851644053527, 0.3996062992125986590, -1.568241469816272993 ) ) ;
#15968 = CARTESIAN_POINT ( 'NONE',  ( -0.6199123404867337150, -2.191421614605370878E-15, 0.4445507791589071167 ) ) ;
#15969 = ORIENTED_EDGE ( 'NONE', *, *, #14729, .T. ) ;
#15970 = CARTESIAN_POINT ( 'NONE',  ( -0.3460692066303960313, 0.1998031496062989965, -1.362860892388451539 ) ) ;
#15971 = CARTESIAN_POINT ( 'NONE',  ( 0.2925321140481932369, 0.2925321140481932369, -0.6870078740157479213 ) ) ;
#15972 = CARTESIAN_POINT ( 'NONE',  ( -0.6233595800524928121, -0.08942795157527998196, 0.3641732283464567121 ) ) ;
#15973 = CARTESIAN_POINT ( 'NONE',  ( -0.8333333333333323711, -0.6692913385826773087, -0.1292274648535924053 ) ) ;
#15974 = CARTESIAN_POINT ( 'NONE',  ( 0.3458507752293908943, -0.3458507752293908943, -0.09842519685039372024 ) ) ;
#15975 = CARTESIAN_POINT ( 'NONE',  ( 0.1958661417322836440, -0.3392501089628017219, -2.538713910761154491 ) ) ;
#15976 = CARTESIAN_POINT ( 'NONE',  ( 1.561679790026247350, 0.05413385826771626580, -0.4176697321401330321 ) ) ;
#15977 = CARTESIAN_POINT ( 'NONE',  ( 0.6758530183727039509, 0.2952755905511810774, -0.1292274648535930714 ) ) ;
#15978 = CARTESIAN_POINT ( 'NONE',  ( 0.3346456692913393205, -0.5400638737290845981, -0.3530559997133363437 ) ) ;
#15979 = CARTESIAN_POINT ( 'NONE',  ( -0.5118110236220466680, 0.1771653543307087630, 0.000000000000000000 ) ) ;
#15980 = CARTESIAN_POINT ( 'NONE',  ( 0.01968503937007930540, 0.1660481256975885056, 0.3530559997133364547 ) ) ;
#15981 = CARTESIAN_POINT ( 'NONE',  ( -0.3458507752293909498, 0.3458507752293907833, -1.986220472440944906 ) ) ;
#15982 = CARTESIAN_POINT ( 'NONE',  ( -0.1640419947506553400, -0.08942795157528024563, -0.3641732283464568787 ) ) ;
#15983 = CARTESIAN_POINT ( 'NONE',  ( -0.4658792650918627265, -0.05778040916215522460, 0.4822834645669289988 ) ) ;
#15984 = CARTESIAN_POINT ( 'NONE',  ( 0.1974969037888706092, -0.3420746716998660508, -1.900918635170603554 ) ) ;
#15985 = CARTESIAN_POINT ( 'NONE',  ( 1.541994750656168645, -0.5511811023622046335, 0.09757992244046803654 ) ) ;
#15986 = CARTESIAN_POINT ( 'NONE',  ( 0.2230971128608929543, -0.004921259842519870586, -0.3153832671262229437 ) ) ;
#15987 = DIRECTION ( 'NONE',  ( 1.000000000000000000, 0.000000000000000000, 0.000000000000000000 ) ) ;
#15988 = CARTESIAN_POINT ( 'NONE',  ( -0.9776902887139098386, -0.6692913385826771977, 0.1292274648535927661 ) ) ;
#15989 = CARTESIAN_POINT ( 'NONE',  ( -0.7414698162729651543, -0.5511811023622046335, 0.09757992244046803654 ) ) ;
#15990 = CARTESIAN_POINT ( 'NONE',  ( -1.034719704380071992, 5.987370802660155681E-15, -0.3954985857520046388 ) ) ;
#15991 = CARTESIAN_POINT ( 'NONE',  ( -1.325459317585300889, -0.4281496062992127816, -0.4176697321401328100 ) ) ;
#15992 = CARTESIAN_POINT ( 'NONE',  ( -0.1246719160104980823, -0.6692913385826773087, -0.1292274648535924053 ) ) ;
#15993 = CARTESIAN_POINT ( 'NONE',  ( 0.2925321140481932369, -0.2925321140481931814, -2.537401574803149984 ) ) ;
#15994 = B_SPLINE_CURVE_WITH_KNOTS ( 'NONE', 3,
 ( #8391, #26493, #78693, #14719, #77427, #52563, #51725, #13043, #409, #14304 ),
 .UNSPECIFIED., .F., .F.,
 ( 4, 2, 2, 2, 4 ),
 ( 0.001464733143057391418, 0.002397049282983275756, 0.003329365422909159877, 0.004261681562835043131, 0.005193997702760927253 ),
 .UNSPECIFIED. ) ;
#15995 = CARTESIAN_POINT ( 'NONE',  ( -0.1049643490035306742, 0.3917322834645668994, -2.606279896816586117 ) ) ;
#15996 = CARTESIAN_POINT ( 'NONE',  ( -2.169555354230969790, 1.520093187801265566, -0.4741711390158128703 ) ) ;
#15997 = CARTESIAN_POINT ( 'NONE',  ( 0.2690288713910767848, 0.1771653543307087630, 0.09757992244046791164 ) ) ;
#15998 = CARTESIAN_POINT ( 'NONE',  ( 0.9842519685039375910, 0.2952755905511811885, 0.000000000000000000 ) ) ;
#15999 = CARTESIAN_POINT ( 'NONE',  ( -1.371391076115484831, 0.1771653543307087075, -0.09757992244046823083 ) ) ;
#16000 = CARTESIAN_POINT ( 'NONE',  ( 1.200787401574803681, 0.1660481256975885056, 0.3530559997133364547 ) ) ;
#16001 = CARTESIAN_POINT ( 'NONE',  ( -1.666666666666665853, -0.004921259842519870586, -0.3153832671262229437 ) ) ;
#16002 = CARTESIAN_POINT ( 'NONE',  ( -0.5314960629921254842, -0.5400638737290845981, -0.3530559997133363437 ) ) ;
#16003 = CARTESIAN_POINT ( 'NONE',  ( 0.1115485564304470323, 0.1771653543307087630, 0.09757992244046791164 ) ) ;
#16004 = DIRECTION ( 'NONE',  ( 0.000000000000000000, 0.000000000000000000, -1.000000000000000000 ) ) ;
#16005 = CARTESIAN_POINT ( 'NONE',  ( 0.7349081364829402885, -0.5023911411419708095, -0.1820866141732282451 ) ) ;
#16006 = CARTESIAN_POINT ( 'NONE',  ( 0.006561679790026889343, -0.3162353388693409650, -0.4822834645669289433 ) ) ;
#16007 = CARTESIAN_POINT ( 'NONE',  ( -0.3460692066303960313, 0.1998031496062989965, -0.1030183727034120617 ) ) ;
#16008 = EDGE_CURVE ( 'NONE', #82474, #67145, #79139, .T. ) ;
#16009 = CARTESIAN_POINT ( 'NONE',  ( -1.266404199475064773, -0.3162353388693405765, 0.4822834645669290543 ) ) ;
#16010 = CARTESIAN_POINT ( 'NONE',  ( 0.1049643490035303689, 0.3917322834645670104, -1.652887139107611425 ) ) ;
#16011 = CARTESIAN_POINT ( 'NONE',  ( 0.9645669291338588858, 0.07958543189024085140, 0.2665933059059887866 ) ) ;
#16012 = CARTESIAN_POINT ( 'NONE',  ( -0.1312335958005241554, -0.6046776061558809534, -0.2411417322834644161 ) ) ;
#16013 = CARTESIAN_POINT ( 'NONE',  ( -0.1246719160104980823, -0.6692913385826773087, -0.1292274648535924053 ) ) ;
#16014 = CARTESIAN_POINT ( 'NONE',  ( -0.4199475065616791736, -0.5023911411419708095, 0.1820866141732285504 ) ) ;
#16015 = CARTESIAN_POINT ( 'NONE',  ( 0.9776902887139113929, 0.2066929133858267931, 0.1054918080437490802 ) ) ;
#16016 = CARTESIAN_POINT ( 'NONE',  ( -0.5643044619422565855, -0.3690944881889763329, 0.3153832671262228327 ) ) ;
#16017 = CARTESIAN_POINT ( 'NONE',  ( 0.1771653543307093182, -0.5400638737290845981, -0.3530559997133363437 ) ) ;
#16018 = CARTESIAN_POINT ( 'NONE',  ( -0.6036745406824141069, 0.1283753931104748280, 0.1820866141732283561 ) ) ;
#16019 = CARTESIAN_POINT ( 'NONE',  ( 0.3460692066303959202, -0.1998031496062991630, -0.8116797900262466836 ) ) ;
#16020 = CARTESIAN_POINT ( 'NONE',  ( -1.272965879265091305, 0.05413385826771626580, -0.4176697321401330321 ) ) ;
#16021 = ORIENTED_EDGE ( 'NONE', *, *, #1687, .F. ) ;
#16022 = CARTESIAN_POINT ( 'NONE',  ( -1.279527559055116948, -0.4536011799217367080, 0.2665933059059888421 ) ) ;
#16023 = CARTESIAN_POINT ( 'NONE',  ( -0.5380577427821514602, -0.4281496062992127816, -0.4176697321401328100 ) ) ;
#16024 = CARTESIAN_POINT ( 'NONE',  ( 0.000000000000000000, 2.755905511811024056, 0.000000000000000000 ) ) ;
#16025 = CARTESIAN_POINT ( 'NONE',  ( -1.227034120734907141, -0.6692913385826773087, -0.1292274648535924053 ) ) ;
#16026 = DIRECTION ( 'NONE',  ( -0.000000000000000000, -1.000000000000000000, -0.000000000000000000 ) ) ;
#16027 = CARTESIAN_POINT ( 'NONE',  ( 1.181102362204725198, -0.1870078740157479769, 0.4822834645669291653 ) ) ;
#16028 = CARTESIAN_POINT ( 'NONE',  ( 0.7480314960629927956, 0.2952755905511811885, 0.000000000000000000 ) ) ;
#16029 = CARTESIAN_POINT ( 'NONE',  ( -0.2486400153428821869, 2.660739321503277841E-15, -0.3464511005275191513 ) ) ;
#16030 = CARTESIAN_POINT ( 'NONE',  ( 0.2952755905511810774, 3.597759587968672259E-17, 5.524802951929911998 ) ) ;
#16031 = CARTESIAN_POINT ( 'NONE',  ( -1.692913385826770645, 0.2952755905511811885, 0.000000000000000000 ) ) ;
#16032 = CARTESIAN_POINT ( 'NONE',  ( 0.2925321140481932369, 0.2925321140481932369, -0.2952755905511811885 ) ) ;
#16033 = ORIENTED_EDGE ( 'NONE', *, *, #56352, .F. ) ;
#16034 = CARTESIAN_POINT ( 'NONE',  ( -0.3477690288713902178, 0.1771653543307087075, -0.09757992244046823083 ) ) ;
#16035 = CARTESIAN_POINT ( 'NONE',  ( -0.3917322834645669549, -0.1049643490035306603, -2.085301837270341352 ) ) ;
#16036 = ORIENTED_EDGE ( 'NONE', *, *, #25941, .T. ) ;
#16037 = CARTESIAN_POINT ( 'NONE',  ( 0.9055118110236227702, -0.6692913385826771977, 8.415575281601705876E-17 ) ) ;
#16038 = CARTESIAN_POINT ( 'NONE',  ( -0.5052493438320203589, -0.6692913385826771977, 0.1292274648535927661 ) ) ;
#16039 = CARTESIAN_POINT ( 'NONE',  ( -0.9186351706036736120, -0.6046776061558809534, -0.2411417322834644161 ) ) ;
#16040 = CARTESIAN_POINT ( 'NONE',  ( 1.620734908136483465, -0.6692913385826771977, 0.1292274648535927661 ) ) ;
#16041 = CARTESIAN_POINT ( 'NONE',  ( -1.240157480314959759, -0.4536011799217368745, -0.2665933059059886201 ) ) ;
#16042 = CARTESIAN_POINT ( 'NONE',  ( -0.4670766846050908305, 1.622013716815570827, -2.571617139894965209 ) ) ;
#16043 = CARTESIAN_POINT ( 'NONE',  ( 0.2230971128608932319, -0.4281496062992124485, 0.4176697321401328655 ) ) ;
#16044 = CARTESIAN_POINT ( 'NONE',  ( -0.8792650918635160906, -0.4281496062992124485, 0.4176697321401328655 ) ) ;
#16045 = CARTESIAN_POINT ( 'NONE',  ( 0.3917322834645668994, 0.1049643490035304522, -1.622027928312648859 ) ) ;
#16046 = CARTESIAN_POINT ( 'NONE',  ( -1.213910761154854745, -0.6692913385826771977, 0.1292274648535927661 ) ) ;
#16047 = PLANE ( 'NONE',  #30427 ) ;
#16048 = CARTESIAN_POINT ( 'NONE',  ( 0.9448818897637802916, -0.1870078740157480879, -0.4822834645669291653 ) ) ;
#16049 = CARTESIAN_POINT ( 'NONE',  ( 1.076115485564305141, 0.1283753931104746893, -0.1820866141732285504 ) ) ;
#16050 = ORIENTED_EDGE ( 'NONE', *, *, #42486, .F. ) ;
#16051 = CARTESIAN_POINT ( 'NONE',  ( -0.3392501089628019995, 0.1958661417322831999, -2.857630864338269738 ) ) ;
#16052 = CARTESIAN_POINT ( 'NONE',  ( -0.2755905511811015396, -0.6692913385826771977, 8.415575281601705876E-17 ) ) ;
#16053 = ORIENTED_EDGE ( 'NONE', *, *, #38721, .T. ) ;
#16054 = CARTESIAN_POINT ( 'NONE',  ( 0.1902887139107617975, 0.1771653543307087630, 0.09757992244046791164 ) ) ;
#16055 = CARTESIAN_POINT ( 'NONE',  ( -1.200787401574802349, 0.1660481256975883668, -0.3530559997133364547 ) ) ;
#16056 = CARTESIAN_POINT ( 'NONE',  ( 0.7874015748031503170, -0.1870078740157479769, 0.4822834645669291653 ) ) ;
#16057 = CARTESIAN_POINT ( 'NONE',  ( 1.043307086614173818, -0.5400638737290845981, -0.3530559997133363437 ) ) ;
#16058 = CARTESIAN_POINT ( 'NONE',  ( -0.3018372703412066094, 0.05413385826771666132, 0.4176697321401328100 ) ) ;
#16059 = CARTESIAN_POINT ( 'NONE',  ( -0.3392501089628017219, -0.1958661417322836995, -1.309074433892075451 ) ) ;
#16060 = CARTESIAN_POINT ( 'NONE',  ( -0.7152230971128602510, -0.3162353388693405765, 0.4822834645669290543 ) ) ;
#16061 = CARTESIAN_POINT ( 'NONE',  ( 0.1958661417322834775, 0.3392501089628018884, -2.118766404199475151 ) ) ;
#16062 = CARTESIAN_POINT ( 'NONE',  ( -1.496062992125983815, -0.1870078740157480879, -0.4822834645669291653 ) ) ;
#16063 = CARTESIAN_POINT ( 'NONE',  ( -0.6364829396325453192, -0.05778040916215560624, -0.4822834645669293319 ) ) ;
#16064 = CARTESIAN_POINT ( 'NONE',  ( -0.3805774278215216522, -0.004921259842519576551, 0.3153832671262227771 ) ) ;
#16065 = CARTESIAN_POINT ( 'NONE',  ( 1.364829396325460076, 0.2306618581243848609, 0.2411417322834645549 ) ) ;
#16066 = CARTESIAN_POINT ( 'NONE',  ( 1.423884514435696413, -0.3162353388693409650, -0.4822834645669289433 ) ) ;
#16067 = CARTESIAN_POINT ( 'NONE',  ( -0.8661417322834640276, -0.1870078740157480879, -0.4822834645669291653 ) ) ;
#16068 = CARTESIAN_POINT ( 'NONE',  ( 0.1070741851644053388, 0.3996062992125986035, -0.07020997375328083545 ) ) ;
#16069 = CARTESIAN_POINT ( 'NONE',  ( 0.7742782152230978099, -0.4281496062992124485, 0.4176697321401328655 ) ) ;
#16070 = CARTESIAN_POINT ( 'NONE',  ( -0.1998031496062994683, 0.3460692066303958092, -1.745406824146981561 ) ) ;
#16071 = CARTESIAN_POINT ( 'NONE',  ( -0.5380577427821514602, 0.05413385826771666132, 0.4176697321401328100 ) ) ;
#16072 = CARTESIAN_POINT ( 'NONE',  ( -1.069553805774277722, -0.5511811023622048555, -0.09757992244046775898 ) ) ;
#16073 = CARTESIAN_POINT ( 'NONE',  ( 0.8005249343832028242, -0.3690944881889765550, -0.3153832671262227771 ) ) ;
#16074 = CARTESIAN_POINT ( 'NONE',  ( 0.4091458600556403535, 0.2362204724409449896, -0.6804461942257218343 ) ) ;
#16075 = CARTESIAN_POINT ( 'NONE',  ( 1.187664041994751285, -0.08942795157527998196, 0.3641732283464567121 ) ) ;
#16076 = VECTOR ( 'NONE', #3016, 39.37007874015748143 ) ;
#16077 = CARTESIAN_POINT ( 'NONE',  ( 0.8858267716535438430, -0.5400638737290845981, -0.3530559997133363437 ) ) ;
#16078 = CARTESIAN_POINT ( 'NONE',  ( -9.674558042662122972E-17, 0.3949938075777409963, -0.7066929133858269596 ) ) ;
#16079 = CARTESIAN_POINT ( 'NONE',  ( -0.4133858267716528645, 0.1660481256975883668, -0.3530559997133364547 ) ) ;
#16080 = CARTESIAN_POINT ( 'NONE',  ( 0.000000000000000000, 0.04488074079120461107, 0.000000000000000000 ) ) ;
#16081 = CARTESIAN_POINT ( 'NONE',  ( 1.174540682414699111, -0.08942795157528024563, -0.3641732283464568787 ) ) ;
#16082 = CARTESIAN_POINT ( 'NONE',  ( -0.5905511811023615998, 0.2952755905511811885, 0.000000000000000000 ) ) ;
#16083 = CARTESIAN_POINT ( 'NONE',  ( 0.3949938075777409963, 2.418639510665530743E-17, -0.3523622047244094335 ) ) ;
#16084 = CARTESIAN_POINT ( 'NONE',  ( 1.469816272965879911, -0.6046776061558807314, 0.2411417322834647770 ) ) ;
#16085 = CARTESIAN_POINT ( 'NONE',  ( -0.03937007874015669567, -0.6692913385826771977, 8.415575281601705876E-17 ) ) ;
#16086 = CARTESIAN_POINT ( 'NONE',  ( 0.6036745406824154392, 0.1283753931104746893, -0.1820866141732285504 ) ) ;
#16087 = CARTESIAN_POINT ( 'NONE',  ( 0.3458507752293908943, -0.3458507752293908943, -0.1751968503937007537 ) ) ;
#16088 = CARTESIAN_POINT ( 'NONE',  ( 0.01968503937007957949, -0.4536011799217368745, -0.2665933059059886201 ) ) ;
#16089 = DIRECTION ( 'NONE',  ( 0.000000000000000000, 0.000000000000000000, -1.000000000000000000 ) ) ;
#16090 = CARTESIAN_POINT ( 'NONE',  ( 0.3460692066303958092, 0.1998031496062993018, -1.310367454068241733 ) ) ;
#16091 = CARTESIAN_POINT ( 'NONE',  ( 0.5643044619422579178, 0.05413385826771666132, 0.4176697321401328100 ) ) ;
#16092 = CARTESIAN_POINT ( 'NONE',  ( 0.3917322834645670104, 2.398668435337828261E-17, -0.8976377952755905110 ) ) ;
#16093 = CARTESIAN_POINT ( 'NONE',  ( 1.555118110236221041, 0.07958543189024071263, -0.2665933059059888421 ) ) ;
#16094 = CARTESIAN_POINT ( 'NONE',  ( -0.3814249188612186536, 0.08989863709126630353, -1.138966262901370454E-17 ) ) ;
#16095 = CARTESIAN_POINT ( 'NONE',  ( -0.04593175853018302557, -0.5511811023622048555, -0.09757992244046775898 ) ) ;
#16096 = CARTESIAN_POINT ( 'NONE',  ( -0.03280839895013062252, 0.2952755905511810774, -0.1292274648535930714 ) ) ;
#16097 = CARTESIAN_POINT ( 'NONE',  ( 1.338582677165355062, -0.1870078740157479769, 0.3641732283464567677 ) ) ;
#16098 = CARTESIAN_POINT ( 'NONE',  ( -1.555118110236219930, 0.07958543189024085140, 0.2665933059059887866 ) ) ;
#16099 = CARTESIAN_POINT ( 'NONE',  ( -1.581364829396324945, -0.3162353388693405765, 0.4822834645669290543 ) ) ;
#16100 = CARTESIAN_POINT ( 'NONE',  ( 0.7217847769028878924, 0.05413385826771666132, 0.4176697321401328100 ) ) ;
#16101 = CARTESIAN_POINT ( 'NONE',  ( 1.082677165354331228, 0.1660481256975883668, -0.3530559997133364547 ) ) ;
#16102 = CARTESIAN_POINT ( 'NONE',  ( -1.157146581871515012E-16, 0.4724409448818898682, -0.2342519685039370358 ) ) ;
#16103 = CARTESIAN_POINT ( 'NONE',  ( 0.3149606299212603933, -0.1870078740157479769, 0.4822834645669291653 ) ) ;
#16104 = CARTESIAN_POINT ( 'NONE',  ( 1.338582677165355062, -0.1870078740157479769, 0.4822834645669291653 ) ) ;
#16105 = CARTESIAN_POINT ( 'NONE',  ( 0.9448818897637802916, -0.1870078740157480879, -0.4822834645669291653 ) ) ;
#16106 = CARTESIAN_POINT ( 'NONE',  ( -0.5120078740157480990, 6.270288040516270789E-17, -0.4921259842519685179 ) ) ;
#16107 = B_SPLINE_CURVE_WITH_KNOTS ( 'NONE', 3,
 ( #66111, #66949, #41263, #2553, #21486, #53038, #1311 ),
 .UNSPECIFIED., .F., .F.,
 ( 4, 3, 4 ),
 ( 1.734723475976806902E-18, 0.001246232571205225376, 0.002492492258783241162 ),
 .UNSPECIFIED. ) ;
#16108 = CARTESIAN_POINT ( 'NONE',  ( 0.9383202099737538715, -0.08942795157528024563, -0.3641732283464568787 ) ) ;
#16109 = CARTESIAN_POINT ( 'NONE',  ( 1.456692913385827515, -0.6692913385826771977, 8.415575281601705876E-17 ) ) ;
#16110 = CARTESIAN_POINT ( 'NONE',  ( -0.8595800524934373854, -0.08942795157527998196, 0.3641732283464567121 ) ) ;
#16111 = CARTESIAN_POINT ( 'NONE',  ( 0.3740157480314966754, 0.07958543189024071263, -0.2665933059059888421 ) ) ;
#16112 = CARTESIAN_POINT ( 'NONE',  ( 0.1377952755905518800, 0.1660481256975883668, -0.3530559997133364547 ) ) ;
#16113 = CARTESIAN_POINT ( 'NONE',  ( 0.7742782152230978099, -0.4281496062992124485, 0.4176697321401328655 ) ) ;
#16114 = CARTESIAN_POINT ( 'NONE',  ( -0.5118110236220466680, 0.2952755905511811885, 0.000000000000000000 ) ) ;
#16115 = CARTESIAN_POINT ( 'NONE',  ( 0.07217847769028949700, -0.08942795157528024563, -0.3641732283464568787 ) ) ;
#16116 = CARTESIAN_POINT ( 'NONE',  ( 0.8267716535433077274, 0.2952755905511811885, 0.000000000000000000 ) ) ;
#16117 = CARTESIAN_POINT ( 'NONE',  ( -1.587201285915124771, 1.129514784140639883, 0.2422955380000797188 ) ) ;
#16118 = CARTESIAN_POINT ( 'NONE',  ( -0.8136482939632537770, -0.6046776061558807314, 0.2411417322834647770 ) ) ;
#16120 = CARTESIAN_POINT ( 'NONE',  ( 0.1070741851644053666, 0.3996062992125986035, -1.095800524934382958 ) ) ;
#16119 = CARTESIAN_POINT ( 'NONE',  ( -0.5314960629921349211, 2.716535433070866645, 2.543486866223387377 ) ) ;
#16121 = DIRECTION ( 'NONE',  ( -0.000000000000000000, -1.000000000000000000, -0.000000000000000000 ) ) ;
#16122 = CARTESIAN_POINT ( 'NONE',  ( -0.9776902887139098386, 0.2952755905511810774, -0.1292274648535930714 ) ) ;
#16123 = CARTESIAN_POINT ( 'NONE',  ( -0.6299212598425188991, -0.1870078740157479769, 0.4822834645669291653 ) ) ;
#16124 = CARTESIAN_POINT ( 'NONE',  ( 0.2362204724409449064, 0.4091458600556404646, 0.01312335958005249326 ) ) ;
#16125 = CARTESIAN_POINT ( 'NONE',  ( 0.2891555358219910499, 0.2891555358219910499, -2.500000000000000444 ) ) ;
#16126 = VERTEX_POINT ( 'NONE', #28599 ) ;
#16127 = CARTESIAN_POINT ( 'NONE',  ( 0.5643044619422579178, -0.004921259842519576551, 0.3153832671262227771 ) ) ;
#16128 = CARTESIAN_POINT ( 'NONE',  ( -9.594673741351313045E-17, 0.3917322834645670104, -0.7795275590551180578 ) ) ;
#16129 = CARTESIAN_POINT ( 'NONE',  ( 0.9251968503937015864, -0.5400638737290844871, 0.3530559997133364547 ) ) ;
#16130 = DIRECTION ( 'NONE',  ( -3.491481338843133355E-15, -0.000000000000000000, 1.000000000000000000 ) ) ;
#16131 = CARTESIAN_POINT ( 'NONE',  ( -1.194225721784776262, -0.004921259842519870586, -0.3153832671262229437 ) ) ;
#16132 = CARTESIAN_POINT ( 'NONE',  ( 1.555118110236221041, 0.1660481256975883668, -0.3530559997133364547 ) ) ;
#16133 = EDGE_CURVE ( 'NONE', #55951, #19971, #66080, .T. ) ;
#16134 = CARTESIAN_POINT ( 'NONE',  ( -1.417322834645668772, -0.1870078740157479769, 0.4822834645669291653 ) ) ;
#16135 = CARTESIAN_POINT ( 'NONE',  ( 0.5118110236220480003, -0.6692913385826771977, 8.415575281601705876E-17 ) ) ;
#16136 = CARTESIAN_POINT ( 'NONE',  ( -0.2867679344610364334, -0.2867679344610368219, -0.2965686107273473038 ) ) ;
#16137 = CARTESIAN_POINT ( 'NONE',  ( 0.07874015748031558404, -0.1870078740157479769, 0.4822834645669291653 ) ) ;
#16138 = CARTESIAN_POINT ( 'NONE',  ( -0.7742782152230965886, -0.004921259842519576551, 0.3153832671262227771 ) ) ;
#16139 = CARTESIAN_POINT ( 'NONE',  ( 0.8267716535433077274, 0.2952755905511811885, 0.000000000000000000 ) ) ;
#16141 = EDGE_CURVE ( 'NONE', #62716, #33549, #8416, .T. ) ;
#16140 = CARTESIAN_POINT ( 'NONE',  ( -0.1968503937007867743, -0.6692913385826771977, 8.415575281601705876E-17 ) ) ;
#16142 = CARTESIAN_POINT ( 'NONE',  ( -1.191111281560509383, -2.567464376874931580E-15, -0.4445507791589072832 ) ) ;
#16143 = CARTESIAN_POINT ( 'NONE',  ( -0.3460692066303960868, 0.1998031496062990242, -2.860892388451443669 ) ) ;
#16144 = CARTESIAN_POINT ( 'NONE',  ( -0.1049643490035307158, 0.3917322834645670104, -1.735583620243781322 ) ) ;
#16145 = CARTESIAN_POINT ( 'NONE',  ( 1.043307086614173818, 0.1660481256975885056, 0.3530559997133364547 ) ) ;
#16146 = CARTESIAN_POINT ( 'NONE',  ( 0.1706036745406830368, 0.05413385826771666132, 0.4176697321401328100 ) ) ;
#16147 = CARTESIAN_POINT ( 'NONE',  ( -0.9580052493438311334, 0.05413385826771626580, -0.4176697321401330321 ) ) ;
#16148 = CARTESIAN_POINT ( 'NONE',  ( 1.154855643044620184, 0.2306618581243847221, -0.2411417322834647770 ) ) ;
#16149 = CARTESIAN_POINT ( 'NONE',  ( 0.4265091863517067594, 0.2952755905511811885, 0.1292274648535926551 ) ) ;
#16150 = CARTESIAN_POINT ( 'NONE',  ( -0.3917322834645670104, -7.196005306013484475E-17, -1.068897637795275690 ) ) ;
#16151 = CARTESIAN_POINT ( 'NONE',  ( -0.4461942257217840213, 0.2306618581243848609, 0.2411417322834645549 ) ) ;
#16152 = CARTESIAN_POINT ( 'NONE',  ( 0.7283464566929143125, 0.1660481256975885056, 0.3530559997133364547 ) ) ;
#16153 = CARTESIAN_POINT ( 'NONE',  ( -0.07217847769028787330, -0.05778040916215522460, 0.4822834645669289988 ) ) ;
#16154 = CARTESIAN_POINT ( 'NONE',  ( 0.7086614173228353852, -0.1870078740157479769, 0.3641732283464567677 ) ) ;
#16155 = CARTESIAN_POINT ( 'NONE',  ( -1.318897637795274802, -0.5400638737290845981, -0.3530559997133363437 ) ) ;
#16156 = CARTESIAN_POINT ( 'NONE',  ( -0.4732434500808642697, 1.503067092966740459, -2.557121834200730248 ) ) ;
#16157 = CARTESIAN_POINT ( 'NONE',  ( 0.5183727034120741983, 0.2952755905511810774, -0.1292274648535930714 ) ) ;
#16158 = DIRECTION ( 'NONE',  ( -0.000000000000000000, 1.000000000000000000, -0.000000000000000000 ) ) ;
#16159 = CARTESIAN_POINT ( 'NONE',  ( 4.797336870675656522E-17, -0.3917322834645670104, -2.275590551181102317 ) ) ;
#16160 = ORIENTED_EDGE ( 'NONE', *, *, #56352, .T. ) ;
#16161 = EDGE_CURVE ( 'NONE', #72462, #23065, #72276, .T. ) ;
#16162 = EDGE_LOOP ( 'NONE', ( #54711, #22758, #25100, #74953 ) ) ;
#16163 = CARTESIAN_POINT ( 'NONE',  ( 1.102362204724410155, -0.1870078740157480879, -0.4822834645669291653 ) ) ;
#16164 = CARTESIAN_POINT ( 'NONE',  ( 0.5839895013123367340, -0.5511811023622048555, -0.09757992244046775898 ) ) ;
#16166 = DIRECTION ( 'NONE',  ( 0.000000000000000000, 0.000000000000000000, 1.000000000000000000 ) ) ;
#16165 = DIRECTION ( 'NONE',  ( -3.491481338843132961E-15, -0.000000000000000000, 1.000000000000000000 ) ) ;
#16167 = CARTESIAN_POINT ( 'NONE',  ( 4.797336870675656522E-17, -0.3917322834645670104, -0.6358267716535433989 ) ) ;
#16168 = EDGE_CURVE ( 'NONE', #13017, #17581, #82941, .T. ) ;
#16169 = CARTESIAN_POINT ( 'NONE',  ( 0.3458507752293908943, -0.3458507752293908943, -0.01771653543307087630 ) ) ;
#16170 = DIRECTION ( 'NONE',  ( 0.000000000000000000, 0.000000000000000000, 1.000000000000000000 ) ) ;
#16171 = CARTESIAN_POINT ( 'NONE',  ( 0.2867679344610365999, -0.2867679344610365444, -1.285433070866141669 ) ) ;
#16172 = CARTESIAN_POINT ( 'NONE',  ( -0.3996062992125984925, -0.1070741851644056858, -2.327427821522309426 ) ) ;
#16173 = CARTESIAN_POINT ( 'NONE',  ( -0.8398950131233585692, 0.2306618581243848609, 0.2411417322834645549 ) ) ;
#16174 = CARTESIAN_POINT ( 'NONE',  ( -0.8267716535433065062, -0.6692913385826771977, 8.415575281601705876E-17 ) ) ;
#16175 = CARTESIAN_POINT ( 'NONE',  ( 0.5774278215223103139, -0.6046776061558809534, -0.2411417322834644161 ) ) ;
#16176 = EDGE_LOOP ( 'NONE', ( #40243, #24254 ) ) ;
#16177 = CARTESIAN_POINT ( 'NONE',  ( 1.286089238845145033, 0.2306618581243848609, 0.2411417322834645549 ) ) ;
#16178 = CARTESIAN_POINT ( 'NONE',  ( -1.077419734549938779, 1.180567382142206467, 0.3141180532221660715 ) ) ;
#16179 = APPLICATION_PROTOCOL_DEFINITION ( 'draft international standard', 'automotive_design', 1998, #74523 ) ;
#16180 = CARTESIAN_POINT ( 'NONE',  ( 1.601049868766404982, -0.5023911411419708095, -0.1820866141732282451 ) ) ;
#16181 = CARTESIAN_POINT ( 'NONE',  ( 0.2925321140481931814, -0.2925321140481931259, -2.064960629921259727 ) ) ;
#16182 = CARTESIAN_POINT ( 'NONE',  ( -1.364829396325458521, -0.5023911411419708095, 0.1820866141732285504 ) ) ;
#16183 = CARTESIAN_POINT ( 'NONE',  ( -0.3917322834645671215, 0.1049643490035301469, 0.1325459317585302166 ) ) ;
#16184 = CARTESIAN_POINT ( 'NONE',  ( 0.1246719160104994284, 0.2952755905511810774, -0.1292274648535930714 ) ) ;
#16186 = DIRECTION ( 'NONE',  ( -0.000000000000000000, 1.000000000000000000, -0.000000000000000000 ) ) ;
#16185 = CARTESIAN_POINT ( 'NONE',  ( 1.653543307086614789, -0.1870078740157479769, 0.4822834645669291653 ) ) ;
#16187 = CARTESIAN_POINT ( 'NONE',  ( -1.141732283464566011, -0.5511811023622047445, 6.969142054262312111E-17 ) ) ;
#16188 = CARTESIAN_POINT ( 'NONE',  ( 0.2296587926509192634, -0.3162353388693405765, 0.4822834645669290543 ) ) ;
#16189 = CARTESIAN_POINT ( 'NONE',  ( 1.246719160104987623, -0.3690944881889763329, 0.3153832671262228327 ) ) ;
#16190 = CARTESIAN_POINT ( 'NONE',  ( -0.1958661417322834497, -0.3392501089628018884, -1.405492495241783102 ) ) ;
#16191 = VECTOR ( 'NONE', #6634, 39.37007874015748854 ) ;
#16192 = CARTESIAN_POINT ( 'NONE',  ( -1.174540682414697335, -0.2845877964562161244, -0.3641732283464567121 ) ) ;
#16193 = CARTESIAN_POINT ( 'NONE',  ( 1.332020997375329197, -0.3162353388693405765, 0.4822834645669290543 ) ) ;
#16194 = DIRECTION ( 'NONE',  ( 0.000000000000000000, -1.000000000000000000, 0.000000000000000000 ) ) ;
#16195 = CARTESIAN_POINT ( 'NONE',  ( -0.3280839895013117347, -0.4281496062992124485, 0.4176697321401328655 ) ) ;
#16196 = CARTESIAN_POINT ( 'NONE',  ( -1.351706036745406347, -0.3690944881889763329, 0.3153832671262228327 ) ) ;
#16197 = CARTESIAN_POINT ( 'NONE',  ( -0.1377952755905504645, 0.07958543189024085140, 0.2665933059059887866 ) ) ;
#16198 = CARTESIAN_POINT ( 'NONE',  ( -0.5511811023622041894, -0.1870078740157480879, -0.4822834645669291653 ) ) ;
#16199 = CARTESIAN_POINT ( 'NONE',  ( -1.489501312335957062, -0.08942795157527998196, 0.3641732283464567121 ) ) ;
#16200 = CARTESIAN_POINT ( 'NONE',  ( 0.3392501089628018884, -0.1958661417322833942, -0.5741662974091357174 ) ) ;
#16201 = CARTESIAN_POINT ( 'NONE',  ( 0.4527559055118117182, -0.5400638737290844871, 0.3530559997133364547 ) ) ;
#16202 = CARTESIAN_POINT ( 'NONE',  ( 0.4043999638110887807, 7.699586553780600482E-16, 0.4118484887281971263 ) ) ;
#16203 = CARTESIAN_POINT ( 'NONE',  ( -0.4724409448818895907, -0.1265901696524993070, -2.012467191601049699 ) ) ;
#16204 = CARTESIAN_POINT ( 'NONE',  ( -1.194225721784776262, 0.05413385826771626580, -0.4176697321401330321 ) ) ;
#16205 = CARTESIAN_POINT ( 'NONE',  ( -0.6627296587926503335, -0.5511811023622046335, 0.09757992244046803654 ) ) ;
#16206 = DIRECTION ( 'NONE',  ( -1.000000000000000000, 0.000000000000000000, 0.000000000000000000 ) ) ;
#16207 = CARTESIAN_POINT ( 'NONE',  ( 0.03937007874015833325, -0.6692913385826771977, 8.415575281601705876E-17 ) ) ;
#16208 = CARTESIAN_POINT ( 'NONE',  ( 0.3346456692913393205, -0.4536011799217368745, -0.2665933059059886201 ) ) ;
#16209 = CARTESIAN_POINT ( 'NONE',  ( -0.9251968503937002541, 0.07958543189024085140, 0.2665933059059887866 ) ) ;
#16210 = CARTESIAN_POINT ( 'NONE',  ( -1.640419947506561060, -0.4281496062992127816, -0.4176697321401328100 ) ) ;
#16211 = CARTESIAN_POINT ( 'NONE',  ( -1.522309711286088607, 0.2306618581243847221, -0.2411417322834647770 ) ) ;
#16212 = CARTESIAN_POINT ( 'NONE',  ( 1.325459317585302665, -0.4281496062992124485, 0.4176697321401328655 ) ) ;
#16213 = CARTESIAN_POINT ( 'NONE',  ( -1.604771003085130765, 0.4934440724007108092, -0.1466069496707737840 ) ) ;
#16214 = CARTESIAN_POINT ( 'NONE',  ( 0.9842519685039378130, -0.5511811023622047445, 6.969142054262312111E-17 ) ) ;
#16215 = CARTESIAN_POINT ( 'NONE',  ( 0.6824146981627303710, -0.6046776061558807314, 0.2411417322834647770 ) ) ;
#16216 = CYLINDRICAL_SURFACE ( 'NONE', #74344, 0.4744094488188972947 ) ;
#16217 = CARTESIAN_POINT ( 'NONE',  ( 1.397637795275591177, -0.4536011799217367080, 0.2665933059059888421 ) ) ;
#16218 = ORIENTED_EDGE ( 'NONE', *, *, #9376, .F. ) ;
#16219 = CARTESIAN_POINT ( 'NONE',  ( -1.332020997375327642, -0.05778040916215522460, 0.4822834645669289988 ) ) ;
#16220 = ADVANCED_FACE ( 'NONE', ( #40809 ), #8828, .F. ) ;
#16221 = CARTESIAN_POINT ( 'NONE',  ( -0.9842519685039360366, 0.2952755905511811885, 0.000000000000000000 ) ) ;
#16222 = CARTESIAN_POINT ( 'NONE',  ( 0.3346456692913390985, 0.1660481256975885056, 0.3530559997133364547 ) ) ;
#16223 = CARTESIAN_POINT ( 'NONE',  ( -1.312335958005248715, -0.5023911411419708095, -0.1820866141732282451 ) ) ;
#16224 = CARTESIAN_POINT ( 'NONE',  ( -0.3460692066303960313, 0.1998031496062989965, -2.150262467191601079 ) ) ;
#16225 = CARTESIAN_POINT ( 'NONE',  ( -1.646981627296586703, -0.3162353388693409650, -0.4822834645669289433 ) ) ;
#16226 = CARTESIAN_POINT ( 'NONE',  ( 0.3674540682414705883, -0.6046776061558807314, 0.2411417322834647770 ) ) ;
#16227 = CARTESIAN_POINT ( 'NONE',  ( 0.7545931758530188826, -0.6692913385826771977, 0.1292274648535927661 ) ) ;
#16228 = CARTESIAN_POINT ( 'NONE',  ( 1.568241469816273659, -0.05778040916215560624, -0.4822834645669293319 ) ) ;
#16229 = CARTESIAN_POINT ( 'NONE',  ( -0.3460692066303960868, 0.1998031496062990242, -1.916010498687664043 ) ) ;
#16230 = CARTESIAN_POINT ( 'NONE',  ( 0.3949938075777409963, 2.418639510665530435E-17, -0.9055118110236219930 ) ) ;
#16231 = CARTESIAN_POINT ( 'NONE',  ( 0.3460692066303959757, -0.1998031496062991907, -2.467191601049868677 ) ) ;
#16232 = CARTESIAN_POINT ( 'NONE',  ( -0.7461015445742957830, 1.969952063615671101, -0.5309055118110235227 ) ) ;
#16233 = CARTESIAN_POINT ( 'NONE',  ( 0.1958661417322836440, -0.3392501089628017219, -0.2414698162729658204 ) ) ;
#16234 = CARTESIAN_POINT ( 'NONE',  ( -0.1049868766404193215, 0.1283753931104746893, -0.1820866141732285504 ) ) ;
#16235 = CARTESIAN_POINT ( 'NONE',  ( -0.4855643044619415427, -0.4281496062992124485, 0.4176697321401328655 ) ) ;
#16236 = CARTESIAN_POINT ( 'NONE',  ( 0.9514435695538062676, -0.05778040916215522460, 0.4822834645669289988 ) ) ;
#16237 = CARTESIAN_POINT ( 'NONE',  ( -0.1974969037888706924, 0.3420746716998658843, -2.294619422572178102 ) ) ;
#16238 = CARTESIAN_POINT ( 'NONE',  ( -0.07217847769028787330, -0.08942795157527998196, 0.3641732283464567121 ) ) ;
#16239 =( BOUNDED_CURVE ( )  B_SPLINE_CURVE ( 3, ( #77222, #58683, #12838, #45629 ),
 .UNSPECIFIED., .F., .F. ) 
 B_SPLINE_CURVE_WITH_KNOTS ( ( 4, 4 ),
 ( 3.539787554096436306, 4.423914789137159076 ),
 .UNSPECIFIED. ) 
 CURVE ( )  GEOMETRIC_REPRESENTATION_ITEM ( )  RATIONAL_B_SPLINE_CURVE ( ( 1.000000000000000000, 0.9359138408343250504, 0.9359138408343250504, 1.000000000000000000 ) ) 
 REPRESENTATION_ITEM ( '' )  );
#16240 = CARTESIAN_POINT ( 'NONE',  ( -1.069553805774277722, -0.6692913385826773087, -0.1292274648535924053 ) ) ;
#16241 = CARTESIAN_POINT ( 'NONE',  ( 1.108923884514436242, -0.05778040916215522460, 0.4822834645669289988 ) ) ;
#16242 = CARTESIAN_POINT ( 'NONE',  ( -0.3458507752293906723, -0.3458507752293910609, -2.421259842519684735 ) ) ;
#16243 = CARTESIAN_POINT ( 'NONE',  ( 0.3996062992125986035, 0.1070741851644054776, -1.856955380577427928 ) ) ;
#16244 = CYLINDRICAL_SURFACE ( 'NONE', #11641, 1.181102362204724310 ) ;
#16245 = ORIENTED_EDGE ( 'NONE', *, *, #24858, .T. ) ;
#16246 = ORIENTED_EDGE ( 'NONE', *, *, #52589, .T. ) ;
#16247 = CARTESIAN_POINT ( 'NONE',  ( 1.102362204724410155, -0.1870078740157479769, 0.4822834645669291653 ) ) ;
#16248 = CARTESIAN_POINT ( 'NONE',  ( -1.522309711286088607, 0.2306618581243847221, -0.2411417322834647770 ) ) ;
#16250 = CARTESIAN_POINT ( 'NONE',  ( -1.607611548556429737, 0.2952755905511810774, -0.1292274648535930714 ) ) ;
#16249 = CARTESIAN_POINT ( 'NONE',  ( -1.456692913385826182, 0.1771653543307087630, 0.000000000000000000 ) ) ;
#16251 = CARTESIAN_POINT ( 'NONE',  ( -0.3392501089628018329, -0.1958661417322836440, -2.809691970307399700 ) ) ;
#16252 = CARTESIAN_POINT ( 'NONE',  ( -0.9973753280839886548, 0.1539470093639523085, 0.1968503937007873850 ) ) ;
#16253 = CARTESIAN_POINT ( 'NONE',  ( 1.345144356955381593, -0.05778040916215522460, 0.4822834645669289988 ) ) ;
#16254 = CARTESIAN_POINT ( 'NONE',  ( 0.2362204724409451007, -0.4091458600556402980, -2.454068241469816058 ) ) ;
#16255 = CARTESIAN_POINT ( 'NONE',  ( 0.1049868766404206816, -0.6046776061558809534, -0.2411417322834644161 ) ) ;
#16256 = CARTESIAN_POINT ( 'NONE',  ( -0.6824146981627291497, -0.6046776061558809534, -0.2411417322834644161 ) ) ;
#16257 = AXIS2_PLACEMENT_3D ( 'NONE', #67503, #69151, #68740 ) ;
#16258 = CARTESIAN_POINT ( 'NONE',  ( 1.601049868766404982, 0.2306618581243848609, 0.2411417322834645549 ) ) ;
#16259 = CARTESIAN_POINT ( 'NONE',  ( -0.3392501089628017219, -0.1958661417322836718, -0.1371391076115486551 ) ) ;
#16260 = CARTESIAN_POINT ( 'NONE',  ( 0.2887139107611556010, -0.6046776061558807314, 0.2411417322834647770 ) ) ;
#16261 = CARTESIAN_POINT ( 'NONE',  ( -0.1049643490035307020, 0.3917322834645669549, -2.203412073490814027 ) ) ;
#16262 = EDGE_CURVE ( 'NONE', #77098, #51714, #73221, .T. ) ;
#16263 = CARTESIAN_POINT ( 'NONE',  ( -1.036745406824146176, -0.3690944881889763329, 0.3153832671262228327 ) ) ;
#16264 = ORIENTED_EDGE ( 'NONE', *, *, #54110, .T. ) ;
#16265 = CARTESIAN_POINT ( 'NONE',  ( 0.1058382717557500713, -0.3949938075777409408, -2.132545931758530244 ) ) ;
#16266 = EDGE_LOOP ( 'NONE', ( #32776, #18914, #6670, #52539 ) ) ;
#16267 = CARTESIAN_POINT ( 'NONE',  ( 6.265965269058076312E-17, 1.062992125984252745, -1.850393700787401619 ) ) ;
#16268 = CARTESIAN_POINT ( 'NONE',  ( -1.528871391076114250, 0.2952755905511810774, -0.1292274648535930714 ) ) ;
#16269 = CARTESIAN_POINT ( 'NONE',  ( 0.2925321140481932369, -0.2925321140481932369, -1.200787401574803015 ) ) ;
#16270 = CARTESIAN_POINT ( 'NONE',  ( 1.686351706036745890, 0.1771653543307087630, 0.09757992244046791164 ) ) ;
#16271 = CARTESIAN_POINT ( 'NONE',  ( -1.640419947506561060, -0.4281496062992127816, -0.4176697321401328100 ) ) ;
#16272 = CARTESIAN_POINT ( 'NONE',  ( 0.4330708661417329575, 0.2952755905511811885, 0.000000000000000000 ) ) ;
#16274 = DIRECTION ( 'NONE',  ( 0.000000000000000000, 0.000000000000000000, -1.000000000000000000 ) ) ;
#16273 = B_SPLINE_CURVE_WITH_KNOTS ( 'NONE', 3,
 ( #77451, #6314, #25253, #50917, #78295, #26515, #58494, #70714, #70290, #33257, #12235, #5902 ),
 .UNSPECIFIED., .F., .F.,
 ( 4, 2, 2, 2, 2, 4 ),
 ( 0.05454303362711843822, 0.05585633982237198786, 0.05651299291999875574, 0.05716964601762552362, 0.05848295221287904549, 0.05979625840813256737 ),
 .UNSPECIFIED. ) ;
#16275 = CARTESIAN_POINT ( 'NONE',  ( -0.3392501089628017219, -0.1958661417322836718, 0.02034120734908127781 ) ) ;
#16276 = CARTESIAN_POINT ( 'NONE',  ( -0.4265091863517051496, -0.5511811023622046335, 0.09757992244046803654 ) ) ;
#16277 = CARTESIAN_POINT ( 'NONE',  ( -0.7677165354330699465, 0.07958543189024085140, 0.2665933059059887866 ) ) ;
#16278 = CARTESIAN_POINT ( 'NONE',  ( -1.279527559055116948, 0.1660481256975883668, -0.3530559997133364547 ) ) ;
#16279 = CARTESIAN_POINT ( 'NONE',  ( 0.3937007874015754361, -0.1870078740157480879, -0.4822834645669291653 ) ) ;
#16280 = CARTESIAN_POINT ( 'NONE',  ( -1.417322834645668772, -0.1870078740157480879, -0.4822834645669291653 ) ) ;
#16281 = CIRCLE ( 'NONE', #75386, 3.858267716535433323 ) ;
#16282 = CARTESIAN_POINT ( 'NONE',  ( 0.1181102362204724532, -0.04921259842519688094, 0.08523872084492505052 ) ) ;
#16283 = ORIENTED_EDGE ( 'NONE', *, *, #45519, .F. ) ;
#16284 = CARTESIAN_POINT ( 'NONE',  ( -1.299212598425196097, 0.2952755905511811885, 0.000000000000000000 ) ) ;
#16285 = DIRECTION ( 'NONE',  ( 0.000000000000000000, 0.000000000000000000, 1.000000000000000000 ) ) ;
#16286 = SHAPE_REPRESENTATION_RELATIONSHIP ( 'NONE' , 'NONE' ,  #76132, #64521 ) ;
#16287 = CARTESIAN_POINT ( 'NONE',  ( 0.4724409448818896462, 0.1265901696524990294, -1.541994750656167978 ) ) ;
#16288 = CYLINDRICAL_SURFACE ( 'NONE', #82842, 0.3937007874015748254 ) ;
#16289 = CARTESIAN_POINT ( 'NONE',  ( -0.2867679344610365999, 0.2867679344610364889, -0.7992125984251968740 ) ) ;
#16290 = CARTESIAN_POINT ( 'NONE',  ( -0.2362204724409451284, 0.4091458600556402425, -0.9580052493438320216 ) ) ;
#16291 = CARTESIAN_POINT ( 'NONE',  ( -0.9055118110236215490, -0.6692913385826771977, 8.415575281601705876E-17 ) ) ;
#16292 = CARTESIAN_POINT ( 'NONE',  ( 1.620734908136483465, -0.6692913385826771977, 0.1292274648535927661 ) ) ;
#16294 = LINE ( 'NONE', #3237, #73466 ) ;
#16293 = CARTESIAN_POINT ( 'NONE',  ( -0.7426113562967729953, 2.199547029020892275, -0.5309055118110235227 ) ) ;
#16295 = ADVANCED_FACE ( 'NONE', ( #35331 ), #60994, .T. ) ;
#16296 = CARTESIAN_POINT ( 'NONE',  ( -1.535433070866141225, 0.2952755905511811885, 0.000000000000000000 ) ) ;
#16297 = CARTESIAN_POINT ( 'NONE',  ( -0.7611548556430438595, 0.2306618581243848609, 0.2411417322834645549 ) ) ;
#16298 = CARTESIAN_POINT ( 'NONE',  ( 0.3917322834645668994, 0.1049643490035304522, -0.04722477870634988334 ) ) ;
#16299 = CARTESIAN_POINT ( 'NONE',  ( -0.1706036745406816491, -0.3690944881889763329, 0.3153832671262228327 ) ) ;
#16300 = CARTESIAN_POINT ( 'NONE',  ( -0.1049643490035307020, 0.3917322834645669549, -0.5636482939632546652 ) ) ;
#16301 = EDGE_CURVE ( 'NONE', #60855, #19993, #80273, .T. ) ;
#16302 = CARTESIAN_POINT ( 'NONE',  ( -0.2755905511811015396, -0.5511811023622047445, 6.969142054262312111E-17 ) ) ;
#16303 = CARTESIAN_POINT ( 'NONE',  ( 0.9645669291338588858, 0.07958543189024085140, 0.2665933059059887866 ) ) ;
#16304 = CARTESIAN_POINT ( 'NONE',  ( 0.4855643044619428750, 0.05413385826771666132, 0.4176697321401328100 ) ) ;
#16305 = CARTESIAN_POINT ( 'NONE',  ( -0.3346456692913377662, 0.07958543189024071263, -0.2665933059059888421 ) ) ;
#16306 = CARTESIAN_POINT ( 'NONE',  ( -0.1958661417322836718, 0.3392501089628017219, -2.367454068241469756 ) ) ;
#16307 = CARTESIAN_POINT ( 'NONE',  ( 1.377952755905512472, -0.6692913385826771977, 8.415575281601705876E-17 ) ) ;
#16308 = CARTESIAN_POINT ( 'NONE',  ( -1.181102362204723644, -0.1870078740157479769, 0.3641732283464567677 ) ) ;
#16309 = CARTESIAN_POINT ( 'NONE',  ( -0.3458507752293906723, -0.3458507752293910609, -0.2933070866141732069 ) ) ;
#16310 = CARTESIAN_POINT ( 'NONE',  ( 0.2099737532808405305, 0.2306618581243847221, -0.2411417322834647770 ) ) ;
#16311 = CARTESIAN_POINT ( 'NONE',  ( -0.6167979002624665030, -0.4281496062992127816, -0.4176697321401328100 ) ) ;
#16312 = DIRECTION ( 'NONE',  ( 0.000000000000000000, 0.000000000000000000, -1.000000000000000000 ) ) ;
#16313 = CARTESIAN_POINT ( 'NONE',  ( 0.5905511811023629321, -0.5511811023622047445, 6.969142054262312111E-17 ) ) ;
#16314 = CARTESIAN_POINT ( 'NONE',  ( -0.2755905511811018171, 0.1771653543307087630, 0.000000000000000000 ) ) ;
#16315 = CARTESIAN_POINT ( 'NONE',  ( -0.6824146981627288167, 0.2306618581243848609, 0.2411417322834645549 ) ) ;
#16316 = DIRECTION ( 'NONE',  ( 0.000000000000000000, 0.000000000000000000, -1.000000000000000000 ) ) ;
#16317 = DIRECTION ( 'NONE',  ( -3.096699300667737957E-16, 1.000000000000000000, -0.000000000000000000 ) ) ;
#16318 = CARTESIAN_POINT ( 'NONE',  ( 0.3280839895013130669, -0.4281496062992127816, -0.4176697321401328100 ) ) ;
#16319 = CIRCLE ( 'NONE', #2850, 3.425196850393701808 ) ;
#16320 = CARTESIAN_POINT ( 'NONE',  ( -9.787531504996566615E-17, 0.3996062992125985480, -1.651574803149606474 ) ) ;
#16321 = CARTESIAN_POINT ( 'NONE',  ( 1.594488188976378673, 0.1660481256975885056, 0.3530559997133364547 ) ) ;
#16322 = CARTESIAN_POINT ( 'NONE',  ( -0.1640419947506555343, -0.2845877964562159024, 0.3641732283464567677 ) ) ;
#16323 = CARTESIAN_POINT ( 'NONE',  ( -0.5314960629921254842, -0.5400638737290845981, -0.3530559997133363437 ) ) ;
#16324 = CARTESIAN_POINT ( 'NONE',  ( 0.4606732211678792877, 2.401574803149606030, 0.5309055118110234117 ) ) ;
#16325 = CARTESIAN_POINT ( 'NONE',  ( 1.633858267716535639, -0.5400638737290844871, 0.3530559997133364547 ) ) ;
#16326 = CARTESIAN_POINT ( 'NONE',  ( 1.318897637795276356, -0.5400638737290844871, 0.3530559997133364547 ) ) ;
#16327 = DIRECTION ( 'NONE',  ( 0.000000000000000000, 0.000000000000000000, 1.000000000000000000 ) ) ;
#16328 = CARTESIAN_POINT ( 'NONE',  ( -0.7414698162729651543, 0.1771653543307087075, -0.09757992244046823083 ) ) ;
#16329 = CARTESIAN_POINT ( 'NONE',  ( -0.1070741851644051862, -0.3996062992125986035, -0.1489501312335957672 ) ) ;
#16330 = CARTESIAN_POINT ( 'NONE',  ( 0.3996062992125986035, 2.446882876249141962E-17, -0.4330708661417322913 ) ) ;
#16331 = CARTESIAN_POINT ( 'NONE',  ( -0.1958661417322833942, -0.3392501089628018884, -2.897000943078426705 ) ) ;
#16332 = CONICAL_SURFACE ( 'NONE', #13621, 0.09842519685039351207, 1.029744258676652091 ) ;
#16333 = CARTESIAN_POINT ( 'NONE',  ( 1.417322834645670104, -0.1870078740157480601, -0.3641732283464567677 ) ) ;
#16334 = CARTESIAN_POINT ( 'NONE',  ( 1.312335958005249825, 0.1283753931104746893, -0.1820866141732285504 ) ) ;
#16335 = CARTESIAN_POINT ( 'NONE',  ( 0.9514435695538062676, -0.05778040916215522460, 0.4822834645669289988 ) ) ;
#16336 = CARTESIAN_POINT ( 'NONE',  ( -1.719160104986876103, 0.05413385826771666132, 0.4176697321401328100 ) ) ;
#16337 = CARTESIAN_POINT ( 'NONE',  ( 1.030183727034121421, -0.3162353388693409650, -0.4822834645669289433 ) ) ;
#16338 = CARTESIAN_POINT ( 'NONE',  ( -0.3949938075777409963, -7.255918531996591613E-17, -0.9035433070866141225 ) ) ;
#16339 = CARTESIAN_POINT ( 'NONE',  ( 1.135170603674541256, -0.5511811023622048555, -0.09757992244046775898 ) ) ;
#16340 = CARTESIAN_POINT ( 'NONE',  ( -0.05905511811023545637, 0.1660481256975885056, 0.3530559997133364547 ) ) ;
#16341 = CARTESIAN_POINT ( 'NONE',  ( -0.6233595800524928121, -0.3162353388693409650, -0.4822834645669289433 ) ) ;
#16342 = CARTESIAN_POINT ( 'NONE',  ( 1.627296587926509996, -0.6046776061558807314, 0.2411417322834647770 ) ) ;
#16343 = CARTESIAN_POINT ( 'NONE',  ( -0.1265901696524986964, -0.4724409448818899238, -1.174540682414698001 ) ) ;
#16344 = CARTESIAN_POINT ( 'NONE',  ( -0.3996062992125986035, -7.340648628747425578E-17, -2.244094488188976388 ) ) ;
#16345 = CARTESIAN_POINT ( 'NONE',  ( 0.4986876640419954376, 0.1283753931104748280, 0.1820866141732283561 ) ) ;
#16346 = ORIENTED_EDGE ( 'NONE', *, *, #10513, .F. ) ;
#16347 = CARTESIAN_POINT ( 'NONE',  ( -0.3392501089628019995, 0.1958661417322831999, -0.1804655100075609198 ) ) ;
#16348 = ORIENTED_EDGE ( 'NONE', *, *, #72224, .F. ) ;
#16349 = CARTESIAN_POINT ( 'NONE',  ( -0.4986876640419942164, -0.6046776061558807314, 0.2411417322834647770 ) ) ;
#16350 = CARTESIAN_POINT ( 'NONE',  ( -0.2821522309711278487, -0.6692913385826773087, -0.1292274648535924053 ) ) ;
#16351 = CARTESIAN_POINT ( 'NONE',  ( -0.3608923884514428360, 0.2952755905511811885, 0.1292274648535926551 ) ) ;
#16352 = CARTESIAN_POINT ( 'NONE',  ( 0.5971128608923891301, 0.2952755905511810774, -0.1292274648535930714 ) ) ;
#16353 = CARTESIAN_POINT ( 'NONE',  ( -1.076115485564303809, -0.6046776061558809534, -0.2411417322834644161 ) ) ;
#16354 = CARTESIAN_POINT ( 'NONE',  ( -0.3280839895013117347, -0.4281496062992124485, 0.4176697321401328655 ) ) ;
#16355 = CARTESIAN_POINT ( 'NONE',  ( 1.272965879265092637, 0.05413385826771666132, 0.4176697321401328100 ) ) ;
#16356 = CARTESIAN_POINT ( 'NONE',  ( 1.017060367454068581, -0.05778040916215560624, -0.4822834645669293319 ) ) ;
#16357 = CARTESIAN_POINT ( 'NONE',  ( 0.6889763779527566800, -0.5400638737290844871, 0.3530559997133364547 ) ) ;
#16358 = CARTESIAN_POINT ( 'NONE',  ( 0.3392501089628018884, -0.1958661417322834220, -0.8845144356955378928 ) ) ;
#16359 = CARTESIAN_POINT ( 'NONE',  ( 0.1640419947506569498, -0.2845877964562161244, -0.3641732283464567121 ) ) ;
#16360 = ORIENTED_EDGE ( 'NONE', *, *, #6655, .T. ) ;
#16361 = CARTESIAN_POINT ( 'NONE',  ( -0.3949938075777409963, -7.255918531996591613E-17, -0.9842519685039369248 ) ) ;
#16362 = ORIENTED_EDGE ( 'NONE', *, *, #13185, .F. ) ;
#16363 = CARTESIAN_POINT ( 'NONE',  ( -1.036745406824146176, -0.004921259842519870586, -0.3153832671262229437 ) ) ;
#16364 = CARTESIAN_POINT ( 'NONE',  ( -0.6561679790026240244, 0.2306618581243847221, -0.2411417322834647770 ) ) ;
#16365 = CARTESIAN_POINT ( 'NONE',  ( -0.6299212598425188991, -0.1870078740157479769, 0.4822834645669291653 ) ) ;
#16366 = CARTESIAN_POINT ( 'NONE',  ( -0.4855643044619415427, -0.4281496062992124485, 0.4176697321401328655 ) ) ;
#16367 = CARTESIAN_POINT ( 'NONE',  ( -1.318897637795274802, 0.1660481256975885056, 0.3530559997133364547 ) ) ;
#16368 = CARTESIAN_POINT ( 'NONE',  ( -1.627296587926508442, -0.6046776061558809534, -0.2411417322834644161 ) ) ;
#16369 = CARTESIAN_POINT ( 'NONE',  ( 0.9842519685039378130, -0.5511811023622047445, 6.969142054262312111E-17 ) ) ;
#16370 = CARTESIAN_POINT ( 'NONE',  ( 0.1265901696524990572, -0.4724409448818897017, -1.030183727034120533 ) ) ;
#16371 = CARTESIAN_POINT ( 'NONE',  ( 0.2813683484248658551, 0.08970734455876072655, 5.854851642268653400 ) ) ;
#16372 = CARTESIAN_POINT ( 'NONE',  ( 0.2821522309711292364, -0.5511811023622046335, 0.09757992244046803654 ) ) ;
#16373 = CARTESIAN_POINT ( 'NONE',  ( 0.2230971128608932319, -0.4281496062992124485, 0.4176697321401328655 ) ) ;
#16374 = CARTESIAN_POINT ( 'NONE',  ( 0.3412073490813655186, -0.6046776061558809534, -0.2411417322834644161 ) ) ;
#16375 = VERTEX_POINT ( 'NONE', #42865 ) ;
#16376 = CIRCLE ( 'NONE', #2911, 0.09842519685039372024 ) ;
#16377 = CARTESIAN_POINT ( 'NONE',  ( -0.3996062992125987146, 0.1070741851644051862, -1.607611548556430403 ) ) ;
#16378 = CARTESIAN_POINT ( 'NONE',  ( -0.5708661417322828946, 0.1660481256975883391, -0.3530559997133364547 ) ) ;
#16379 = VERTEX_POINT ( 'NONE', #36976 ) ;
#16380 = CARTESIAN_POINT ( 'NONE',  ( 0.3996062992125985480, 2.446882876249141654E-17, -1.297244094488188670 ) ) ;
#16381 = CARTESIAN_POINT ( 'NONE',  ( 1.528871391076116026, -0.6692913385826773087, -0.1292274648535924053 ) ) ;
#16382 = CARTESIAN_POINT ( 'NONE',  ( -0.8530183727034112984, -0.3690944881889765550, -0.3153832671262227771 ) ) ;
#16383 = CARTESIAN_POINT ( 'NONE',  ( -0.9908136482939626788, -0.6692913385826773087, -0.1292274648535924053 ) ) ;
#16384 = CARTESIAN_POINT ( 'NONE',  ( -1.157146581871515012E-16, 0.4724409448818898682, -0.6299212598425196763 ) ) ;
#16385 = CARTESIAN_POINT ( 'NONE',  ( -0.1049643490035307020, 0.3917322834645669549, -2.610892388451443225 ) ) ;
#16386 = CARTESIAN_POINT ( 'NONE',  ( 1.673228346456693494, 0.1660481256975885056, 0.3530559997133364547 ) ) ;
#16387 = CARTESIAN_POINT ( 'NONE',  ( 0.4658792650918640033, -0.3162353388693405765, 0.4822834645669290543 ) ) ;
#16388 = CARTESIAN_POINT ( 'NONE',  ( 0.6627296587926517768, -0.6692913385826773087, -0.1292274648535924053 ) ) ;
#16389 = CARTESIAN_POINT ( 'NONE',  ( -0.7020997375328074108, -0.08942795157527998196, 0.3641732283464567121 ) ) ;
#16390 = CARTESIAN_POINT ( 'NONE',  ( 0.05905511811023681640, 0.1660481256975883668, -0.3530559997133364547 ) ) ;
#16391 = CARTESIAN_POINT ( 'NONE',  ( 0.1265901696524989462, 0.4724409448818897572, -2.274934383202099397 ) ) ;
#16392 = CARTESIAN_POINT ( 'NONE',  ( -0.4855643044619415427, -0.004921259842519870586, -0.3153832671262229437 ) ) ;
#16393 = CARTESIAN_POINT ( 'NONE',  ( -0.4855643044619415427, -0.4281496062992124485, 0.4176697321401328655 ) ) ;
#16394 = EDGE_CURVE ( 'NONE', #54726, #60937, #81202, .T. ) ;
#16395 = CARTESIAN_POINT ( 'NONE',  ( -0.3949938075777411073, 0.1058382717557497660, -1.841863517060367661 ) ) ;
#16396 = CARTESIAN_POINT ( 'NONE',  ( -1.502624671916009680, -0.05778040916215560624, -0.4822834645669293319 ) ) ;
#16397 = CARTESIAN_POINT ( 'NONE',  ( 0.1049868766404206816, -0.5023911411419708095, -0.1820866141732282451 ) ) ;
#16398 = CARTESIAN_POINT ( 'NONE',  ( 1.010498687664042716, -0.3690944881889763329, 0.3153832671262228327 ) ) ;
#16399 = CARTESIAN_POINT ( 'NONE',  ( -1.292650918635170010, -0.6692913385826771977, 0.1292274648535927661 ) ) ;
#16400 = CARTESIAN_POINT ( 'NONE',  ( -0.9251968503937002541, -0.4536011799217368745, -0.2665933059059886201 ) ) ;
#16401 = DIRECTION ( 'NONE',  ( -1.692413147294446216E-16, 0.000000000000000000, -1.000000000000000000 ) ) ;
#16402 = CARTESIAN_POINT ( 'NONE',  ( -1.122047244094487306, -0.5400638737290844871, 0.3530559997133364547 ) ) ;
#16403 = CARTESIAN_POINT ( 'NONE',  ( -0.5643044619422565855, -0.4281496062992124485, 0.4176697321401328655 ) ) ;
#16404 = CARTESIAN_POINT ( 'NONE',  ( 0.4790026246719168435, -0.3162353388693409650, -0.4822834645669289433 ) ) ;
#16405 = CARTESIAN_POINT ( 'NONE',  ( -0.1958661417322836440, 0.3392501089628016664, -2.297880946685352033 ) ) ;
#16406 = CARTESIAN_POINT ( 'NONE',  ( -3.908320185825792326, 1.537401574803149984, 0.4744094488188970171 ) ) ;
#16407 = CARTESIAN_POINT ( 'NONE',  ( 0.1837270341207357105, -0.5023911411419708095, -0.1820866141732282451 ) ) ;
#16408 = CARTESIAN_POINT ( 'NONE',  ( 1.154855643044620184, 0.2306618581243847221, -0.2411417322834647770 ) ) ;
#16409 = CARTESIAN_POINT ( 'NONE',  ( -1.095800524934382292, -0.08942795157527998196, 0.3641732283464567121 ) ) ;
#16410 = CARTESIAN_POINT ( 'NONE',  ( 1.161417322834646493, -0.5400638737290844871, 0.3530559997133364547 ) ) ;
#16411 = CARTESIAN_POINT ( 'NONE',  ( -1.732283464566928277, -0.1870078740157479769, 0.3641732283464567677 ) ) ;
#16412 = CARTESIAN_POINT ( 'NONE',  ( 1.607611548556431069, 0.1771653543307087630, 0.09757992244046791164 ) ) ;
#16413 = CARTESIAN_POINT ( 'NONE',  ( -0.9645669291338575535, -0.5400638737290844871, 0.3530559997133364547 ) ) ;
#16414 = CARTESIAN_POINT ( 'NONE',  ( 0.09842519685039434474, 0.07958543189024085140, 0.2665933059059887866 ) ) ;
#16415 = CARTESIAN_POINT ( 'NONE',  ( -0.8780747636526944344, -4.654285808514094606E-15, -0.3627989612356153915 ) ) ;
#16416 = CARTESIAN_POINT ( 'NONE',  ( 0.8595800524934390507, -0.08942795157528024563, -0.3641732283464568787 ) ) ;
#16417 = CARTESIAN_POINT ( 'NONE',  ( -0.04593175853018302557, 0.2952755905511811885, 0.1292274648535926551 ) ) ;
#16418 =( BOUNDED_SURFACE ( )  B_SPLINE_SURFACE ( 1, 2, ( 
 ( #73558, #9986, #3255, #40719, #15482, #21776, #60081, #74797, #9569, #66404, #10408, #2843, #23017, #28507, #79878, #29334, #23428, #34413, #36065, #48269, #61737, #2435, #80703, #35240, #4074, #29741, #22196, #55405, #49093, #80295, #22609, #28917, #54585, #73967, #28092, #53749, #51143, #50738, #30973, #24247, #36886, #12454, #76025, #49920, #69295, #50327, #11644, #6128, #63378, #37302, #5714, #68472, #82341, #75618, #49511, #25064, #56640, #76436, #17144, #62145, #36470, #30154, #62563, #43180, #44408, #38115, #4902, #18370, #17956, #30573, #62976, #56239, #5315, #18765, #63789, #23844, #44010, #75204, #69704, #17548, #57049, #68877, #11226, #12047, #42776, #81936, #43593, #24659, #70102, #37705, #31384, #31803, #82743, #57463, #83157, #25476, #10810, #4486, #55816, #81524, #14133, #1910, #33479, #46502, #7385, #44819, #58724, #6963, #39786, #51555, #51979, #65890, #57876, #77258, #19588, #45250, #25895, #243, #70947, #7813, #1087, #65481, #65048, #70516, #39363, #59141, #33053, #1499, #20433, #13292, #52393, #27151, #52815, #32634, #662, #78526, #58297, #26318, #45665, #77684, #46087, #20014, #71779, #32218, #38944, #59555, #19171, #20849, #13709, #71361, #26739, #72202, #14555, #64627, #78102, #40207, #8225, #33889, #27572, #76837, #12873, #38532, #64213, #6547, #79355, #15800, #61641, #67135, #9464, #54900, #22916, #34310, #47751, #35138, #72612, #14960, #40617, #79775, #29236, #61214, #73868, #28402, #73450, #59972, #66722, #15375, #41451, #21674, #8639, #41036, #60800, #53230, #80193, #3154, #46919, #21264, #2331, #67963, #28817, #35971, #66300, #27987, #53647, #47335, #73025, #9059, #54482, #16208, #80606, #34731, #2742, #22511, #48172, #78946, #60391, #54060, #22091, #3982, #41855, #67547, #48583, #9882, #35551, #3569, #74280, #16624, #10305, #42266, #24967, #37200, #82652, #74698, #5216, #4796, #56955, #37609, #30057, #11954, #30880, #69195, #11544, #4389, #56137, #49823, #81016, #43086, #63697, #63284, #43497, #36785, #49416, #50639, #56547, #62461, #81842, #62881, #24153, #18673, #75929, #75523, #18270, #23329, #82248, #30473, #62051, #5624, #43910, #48999, #31290, #17862, #24566, #50233, #11127, #69608, #17043, #42683, #76343, #44318, #68783, #70008, #68381, #10720, #36377, #12363, #81428, #38021, #29646, #55308, #55718, #23743, #75110, #17456, #146, #51047, #46409, #77164, #20759, #44726, #51885, #51462, #32124, #6454, #45150, #25384, #70423, #83063, #14037, #65385, #39694, #78431, #20337, #25801, #76748, #57368, #19078, #77590, #57782, #7720, #19924, #45574, #70853, #12779, #40113, #71267, #19496, #38436, #72103, #13204, #14461, #64119, #13614, #38851, #64531, #6868, #32537, #58201, #569, #26222, #33388, #59051, #1405, #6036, #45989, #39268, #64950, #7290, #32960, #58627, #994, #26649, #52303, #31708, #78009, #71685, #27061, #52720, #46828, #73774, #53967, #41754, #33799, #53135, #72520, #59464, #1815, #21173, #28305, #73353, #3056, #14868, #79264, #79679, #40943, #65800, #40530, #78846, #27477, #8134, #21996, #66209, #8548, #47241, #34214, #2648, #15282, #67449, #59877, #27896, #2231, #16110, #53556, #66622, #9783, #60707, #21579, #72931, #41358, #8960, #34634, #60298, #47657, #22415, #15701, #67039, #28722, #9371, #35042, #54385, #80095, #48072, #77439, #52991, #33246, #7142, #26504, #7573, #52157, #46688, #20615, #77862, #46267, #25655, #39547, #32815, #6722, #65664, #71962, #51317, #7991, #847, #45842, #20191, #39122, #14316, #77020, #19353, #58907, #71541, #71122, #72381, #65236, #58482, #32392, #33655, #39975, #45002, #59318, #13888, #1267, #26915, #64803, #1674, #70701, #13054, #52575, #78284, #13465, #14731, #38707, #64386, #58055, #27331, #26077, #78704, #21028, #40383, #66066, #421, #8402, #57640, #51737, #19773, #3, #45426, #48758, #72788, #79958, #79538, #60156, #34490, #73207, #53416, #15138, #27752, #42033, #10062, #67727, #23091, #48342, #53824, #47515, #21851, #54241, #2508, #40794, #15557, #22271, #34069, #60979, #73634, #79125, #2087, #66479, #74457, #9647, #16804, #21442, #47099, #8814, #28167, #41216 ),
 ( #68140, #35725, #66904, #16386, #9235, #34907, #28993, #42440, #59733, #29408, #41623, #3744, #60570, #35316, #2921, #61395, #55067, #28585, #80775, #3329, #15976, #67312, #47930, #54659, #80370, #22683, #74039, #44490, #44088, #24327, #17625, #30231, #5795, #69371, #43257, #62640, #43669, #4984, #82821, #56721, #30651, #82418, #61811, #42852, #18446, #24737, #4151, #69782, #36963, #82013, #56315, #75282, #50405, #29816, #55477, #11725, #49997, #23921, #25146, #81187, #23504, #49171, #75694, #62222, #12127, #18035, #37381, #68954, #74876, #10485, #63052, #4560, #17220, #50814, #81605, #76515, #68545, #5390, #55893, #36546, #10886, #49587, #11304, #31052, #76102, #37784, #63461, #31465, #18844, #57127, #36139, #10313, #68790, #22924, #80613, #17463, #61648, #3989, #11135, #36793, #35559, #3576, #48590, #42273, #49006, #62469, #68388, #81435, #67970, #79783, #35978, #41862, #74705, #3161, #29243, #43093, #9471, #28825, #54489, #80200, #60808, #35145, #22518, #42691, #29653, #17050, #16631, #22099, #74287, #10727, #55315, #36384, #81024, #48179, #23336, #62058, #4396, #67554, #61222, #30064, #9889, #54907, #55726, #23750, #49423, #75118, #28409, #67142, #73875, #54068, #47759, #73457, #15808, #41458, #16215, #6460, #25806, #37206, #5223, #12786, #5630, #70015, #25390, #32129, #51467, #18276, #57787, #83069, #30886, #50645, #13209, #38028, #63703, #45155, #38856, #11960, #63290, #82659, #18679, #51053, #4803, #44733, #151, #44324, #56146, #12369, #43917, #76754, #62887, #31297, #77169, #69202, #56553, #82254, #24573, #50240, #11551, #75936, #19085, #6043, #70429, #76349, #81849, #31715, #38442, #57374, #64124, #19501, #69614, #70858, #30480, #24161, #37616, #56961, #49829, #24973, #75529, #17869, #43503, #8139, #45994, #59469, #19929, #7295, #47247, #6873, #46833, #1411, #14042, #39699, #66214, #2236, #13619, #64957, #72525, #65390, #46414, #1822, #8553, #27900, #78015, #34220, #27482, #32965, #27066, #72936, #78437, #20764, #59882, #53561, #45579, #59056, #72108, #574, #26227, #51891, #7725, #40535, #14874, #53140, #33394, #52725, #71272, #14466, #79269, #15288, #77595, #39273, #58632, #1000, #26654, #21584, #64536, #52308, #65806, #40118, #20342, #33804, #71691, #78851, #32542, #58207, #21178, #16532, #73357, #42177, #41362, #80918, #67043, #15705, #10209, #75015, #29141, #9375, #22826, #81329, #35458, #9787, #29954, #48902, #55210, #8965, #74603, #67453, #54807, #61123, #22419, #23231, #60303, #34639, #67871, #3474, #54389, #55619, #2653, #28311, #53972, #80511, #35046, #16946, #48484, #74185, #48076, #79685, #40948, #35877, #60711, #22002, #23643, #28728, #49314, #47662, #61544, #3060, #80100, #73778, #16114, #41758, #3888, #29548, #42588, #68288, #10624, #66627, #36280, #61952, #4292, #18979, #37512, #43396, #56037, #5119, #63187, #17361, #44221, #56856, #11027, #68684, #24055, #32025, #76244, #47, #36683, #30370, #75422, #62359, #4696, #49725, #50540, #37923, #76648, #81745, #50132, #18578, #5526, #42990, #17765, #69096, #11444, #51361, #75832, #37100, #44628, #62785, #82965, #30786, #56449, #12265, #57685, #82151, #12680, #24872, #70324, #24467, #69911, #18173, #38338, #25283, #43806, #50951, #63599, #82554, #5936, #69510, #11859, #31191, #31606, #57267, #64013, #6354, #25700, #896, #13511, #72427, #52626, #26553, #45889, #26962, #71587, #66113, #40022, #13938, #65710, #45049, #58955, #52206, #26123, #6767, #39167, #19823, #21077, #14777, #64852, #78332, #77910, #7189, #39596, #32862, #65285, #78752, #40432, #466, #20662, #51784, #46316, #77488, #33703, #45473, #71170, #72009, #28931, #7623, #58530, #1313, #35255, #33295, #14365, #9586, #8040, #59363, #60919, #3270, #20241, #1722, #27378, #53040, #46735, #77064, #19398, #70750, #13101, #38755, #64432, #32438, #58101, #29349, #29756, #43608, #35666, #55008, #80716, #23031, #3684, #61330, #48697, #68891, #36485, #75218, #42791, #48284, #17158, #36901, #68486, #17563, #81539, #74395, #30168, #43196, #4919, #10422, #61751, #56253, #36080, #4088, #23443, #55419, #23858, #81126, #49525, #10001, #16739 ) ),
 .UNSPECIFIED., .F., .F., .F. ) 
 B_SPLINE_SURFACE_WITH_KNOTS ( ( 2, 2 ),
 ( 3, 2, 2, 2, 2, 2, 2, 2, 2, 2, 2, 2, 2, 2, 2, 2, 2, 2, 2, 2, 2, 2, 2, 2, 2, 2, 2, 2, 2, 2, 2, 2, 2, 2, 2, 2, 2, 2, 2, 2, 2, 2, 2, 2, 2, 2, 2, 2, 2, 2, 2, 2, 2, 2, 2, 2, 2, 2, 2, 2, 2, 2, 2, 2, 2, 2, 2, 2, 2, 2, 2, 2, 2, 2, 2, 2, 2, 2, 2, 2, 2, 2, 2, 2, 2, 2, 2, 2, 2, 2, 2, 2, 2, 2, 2, 2, 2, 2, 2, 2, 2, 2, 2, 2, 2, 2, 2, 2, 2, 2, 2, 2, 2, 2, 2, 2, 2, 2, 2, 2, 2, 2, 2, 2, 2, 2, 2, 2, 2, 2, 2, 2, 2, 2, 2, 2, 2, 2, 2, 2, 2, 2, 2, 2, 2, 2, 2, 2, 2, 2, 2, 2, 2, 2, 2, 2, 2, 2, 2, 2, 2, 2, 2, 2, 2, 2, 2, 2, 2, 2, 2, 2, 2, 2, 2, 2, 2, 2, 2, 2, 2, 2, 2, 2, 2, 2, 2, 2, 2, 2, 2, 2, 2, 2, 2, 2, 2, 2, 2, 2, 2, 2, 2, 2, 2, 2, 2, 2, 2, 2, 2, 2, 2, 2, 2, 2, 2, 2, 2, 2, 2, 2, 2, 2, 2, 2, 2, 2, 2, 2, 2, 2, 2, 2, 2, 2, 2, 2, 2, 2, 2, 2, 2, 2, 2, 2, 2, 2, 2, 2, 2, 2, 2, 2, 2, 3 ),
 ( 0.000000000000000000, 1.000000000000000000 ),
 ( 0.000000000000000000, 0.003787878787878787984, 0.007575757575757575968, 0.01136363636363636395, 0.01515151515151515194, 0.01893939393939393992, 0.02272727272727272790, 0.02651515151515151589, 0.03030303030303030387, 0.03409090909090908839, 0.03787878787878787984, 0.04166666666666666435, 0.04545454545454545581, 0.04924242424242424032, 0.05303030303030303177, 0.05681818181818181629, 0.06060606060606060774, 0.06439393939393939226, 0.06818181818181817677, 0.07196969696969697516, 0.07575757575757575968, 0.07954545454545454419, 0.08333333333333332871, 0.08712121212121212710, 0.09090909090909091161, 0.09469696969696969613, 0.09848484848484848064, 0.1022727272727272790, 0.1060606060606060635, 0.1098484848484848481, 0.1136363636363636326, 0.1174242424242424310, 0.1212121212121212155, 0.1250000000000000000, 0.1287878787878787845, 0.1325757575757575690, 0.1363636363636363535, 0.1401515151515151381, 0.1439393939393939503, 0.1477272727272727348, 0.1515151515151515194, 0.1553030303030303039, 0.1590909090909090884, 0.1628787878787878729, 0.1666666666666666574, 0.1704545454545454419, 0.1742424242424242542, 0.1780303030303030387, 0.1818181818181818232, 0.1856060606060606077, 0.1893939393939393923, 0.1931818181818181768, 0.1969696969696969613, 0.2007575757575757458, 0.2045454545454545581, 0.2083333333333333426, 0.2121212121212121271, 0.2159090909090909116, 0.2196969696969696961, 0.2234848484848484806, 0.2272727272727272652, 0.2310606060606060497, 0.2348484848484848619, 0.2386363636363636465, 0.2424242424242424310, 0.2462121212121212155, 0.2500000000000000000, 0.2537878787878787845, 0.2575757575757575690, 0.2613636363636363535, 0.2651515151515151381, 0.2689393939393939226, 0.2727272727272727071, 0.2765151515151514916, 0.2803030303030302761, 0.2840909090909091161, 0.2878787878787879007, 0.2916666666666666852, 0.2954545454545454697, 0.2992424242424242542, 0.3030303030303030387, 0.3068181818181818232, 0.3106060606060606077, 0.3143939393939393923, 0.3181818181818181768, 0.3219696969696969613, 0.3257575757575757458, 0.3295454545454545303, 0.3333333333333333148, 0.3371212121212120993, 0.3409090909090908839, 0.3446969696969697239, 0.3484848484848485084, 0.3522727272727272929, 0.3560606060606060774, 0.3598484848484848619, 0.3636363636363636465, 0.3674242424242424310, 0.3712121212121212155, 0.3750000000000000000, 0.3787878787878787845, 0.3825757575757575690, 0.3863636363636363535, 0.3901515151515151381, 0.3939393939393939226, 0.3977272727272727071, 0.4015151515151514916, 0.4053030303030302761, 0.4090909090909091161, 0.4128787878787879007, 0.4166666666666666852, 0.4204545454545454697, 0.4242424242424242542, 0.4280303030303030387, 0.4318181818181818232, 0.4356060606060606077, 0.4393939393939393923, 0.4431818181818181768, 0.4469696969696969613, 0.4507575757575757458, 0.4545454545454545303, 0.4583333333333333148, 0.4621212121212120993, 0.4659090909090908839, 0.4696969696969697239, 0.4734848484848485084, 0.4772727272727272929, 0.4810606060606060774, 0.4848484848484848619, 0.4886363636363636465, 0.4924242424242424310, 0.4962121212121212155, 0.5000000000000000000, 0.5037878787878787845, 0.5075757575757575690, 0.5113636363636363535, 0.5151515151515151381, 0.5189393939393939226, 0.5227272727272727071, 0.5265151515151514916, 0.5303030303030302761, 0.5340909090909090606, 0.5378787878787878451, 0.5416666666666666297, 0.5454545454545454142, 0.5492424242424241987, 0.5530303030303029832, 0.5568181818181817677, 0.5606060606060605522, 0.5643939393939394478, 0.5681818181818182323, 0.5719696969696970168, 0.5757575757575758013, 0.5795454545454545858, 0.5833333333333333703, 0.5871212121212121549, 0.5909090909090909394, 0.5946969696969697239, 0.5984848484848485084, 0.6022727272727272929, 0.6060606060606060774, 0.6098484848484848619, 0.6136363636363636465, 0.6174242424242424310, 0.6212121212121212155, 0.6250000000000000000, 0.6287878787878787845, 0.6325757575757575690, 0.6363636363636363535, 0.6401515151515151381, 0.6439393939393939226, 0.6477272727272727071, 0.6515151515151514916, 0.6553030303030302761, 0.6590909090909090606, 0.6628787878787878451, 0.6666666666666666297, 0.6704545454545454142, 0.6742424242424241987, 0.6780303030303029832, 0.6818181818181817677, 0.6856060606060605522, 0.6893939393939394478, 0.6931818181818182323, 0.6969696969696970168, 0.7007575757575758013, 0.7045454545454545858, 0.7083333333333333703, 0.7121212121212121549, 0.7159090909090909394, 0.7196969696969697239, 0.7234848484848485084, 0.7272727272727272929, 0.7310606060606060774, 0.7348484848484848619, 0.7386363636363636465, 0.7424242424242424310, 0.7462121212121212155, 0.7500000000000000000, 0.7537878787878787845, 0.7575757575757575690, 0.7613636363636363535, 0.7651515151515151381, 0.7689393939393939226, 0.7727272727272727071, 0.7765151515151514916, 0.7803030303030302761, 0.7840909090909090606, 0.7878787878787878451, 0.7916666666666666297, 0.7954545454545454142, 0.7992424242424241987, 0.8030303030303029832, 0.8068181818181817677, 0.8106060606060605522, 0.8143939393939394478, 0.8181818181818182323, 0.8219696969696970168, 0.8257575757575758013, 0.8295454545454545858, 0.8333333333333333703, 0.8371212121212121549, 0.8409090909090909394, 0.8446969696969697239, 0.8484848484848485084, 0.8522727272727272929, 0.8560606060606060774, 0.8598484848484848619, 0.8636363636363636465, 0.8674242424242424310, 0.8712121212121212155, 0.8750000000000000000, 0.8787878787878787845, 0.8825757575757575690, 0.8863636363636363535, 0.8901515151515151381, 0.8939393939393939226, 0.8977272727272727071, 0.9015151515151514916, 0.9053030303030302761, 0.9090909090909090606, 0.9128787878787878451, 0.9166666666666666297, 0.9204545454545454142, 0.9242424242424241987, 0.9280303030303029832, 0.9318181818181817677, 0.9356060606060605522, 0.9393939393939394478, 0.9431818181818182323, 0.9469696969696970168, 0.9507575757575758013, 0.9545454545454545858, 0.9583333333333333703, 0.9621212121212121549, 0.9659090909090909394 ),
 .UNSPECIFIED. ) 
 GEOMETRIC_REPRESENTATION_ITEM ( )  RATIONAL_B_SPLINE_SURFACE ( (
 ( 1.000000000000000000, 0.9659258262890683122, 1.000000000000000000, 0.9659258262890683122, 1.000000000000000000, 0.9659258262890683122, 1.000000000000000000, 0.9659258262890683122, 1.000000000000000000, 0.9659258262890683122, 1.000000000000000000, 0.9659258262890683122, 1.000000000000000000, 0.9659258262890683122, 1.000000000000000000, 0.9659258262890683122, 1.000000000000000000, 0.9659258262890683122, 1.000000000000000000, 0.9659258262890683122, 1.000000000000000000, 0.9659258262890683122, 1.000000000000000000, 0.9659258262890683122, 1.000000000000000000, 0.9659258262890683122, 1.000000000000000000, 0.9659258262890683122, 1.000000000000000000, 0.9659258262890683122, 1.000000000000000000, 0.9659258262890683122, 1.000000000000000000, 0.9659258262890683122, 1.000000000000000000, 0.9659258262890683122, 1.000000000000000000, 0.9659258262890683122, 1.000000000000000000, 0.9659258262890683122, 1.000000000000000000, 0.9659258262890683122, 1.000000000000000000, 0.9659258262890683122, 1.000000000000000000, 0.9659258262890683122, 1.000000000000000000, 0.9659258262890683122, 1.000000000000000000, 0.9659258262890683122, 1.000000000000000000, 0.9659258262890683122, 1.000000000000000000, 0.9659258262890683122, 1.000000000000000000, 0.9659258262890683122, 1.000000000000000000, 0.9659258262890683122, 1.000000000000000000, 0.9659258262890683122, 1.000000000000000000, 0.9659258262890683122, 1.000000000000000000, 0.9659258262890683122, 1.000000000000000000, 0.9659258262890683122, 1.000000000000000000, 0.9659258262890683122, 1.000000000000000000, 0.9659258262890683122, 1.000000000000000000, 0.9659258262890683122, 1.000000000000000000, 0.9659258262890683122, 1.000000000000000000, 0.9659258262890683122, 1.000000000000000000, 0.9659258262890683122, 1.000000000000000000, 0.9659258262890683122, 1.000000000000000000, 0.9659258262890683122, 1.000000000000000000, 0.9659258262890683122, 1.000000000000000000, 0.9659258262890683122, 1.000000000000000000, 0.9659258262890683122, 1.000000000000000000, 0.9659258262890683122, 1.000000000000000000, 0.9659258262890683122, 1.000000000000000000, 0.9659258262890683122, 1.000000000000000000, 0.9659258262890683122, 1.000000000000000000, 0.9659258262890683122, 1.000000000000000000, 0.9659258262890683122, 1.000000000000000000, 0.9659258262890683122, 1.000000000000000000, 0.9659258262890683122, 1.000000000000000000, 0.9659258262890683122, 1.000000000000000000, 0.9659258262890683122, 1.000000000000000000, 0.9659258262890683122, 1.000000000000000000, 0.9659258262890683122, 1.000000000000000000, 0.9659258262890683122, 1.000000000000000000, 0.9659258262890683122, 1.000000000000000000, 0.9659258262890683122, 1.000000000000000000, 0.9659258262890683122, 1.000000000000000000, 0.9659258262890683122, 1.000000000000000000, 0.9659258262890683122, 1.000000000000000000, 0.9659258262890683122, 1.000000000000000000, 0.9659258262890683122, 1.000000000000000000, 0.9659258262890683122, 1.000000000000000000, 0.9659258262890683122, 1.000000000000000000, 0.9659258262890683122, 1.000000000000000000, 0.9659258262890683122, 1.000000000000000000, 0.9659258262890683122, 1.000000000000000000, 0.9659258262890683122, 1.000000000000000000, 0.9659258262890683122, 1.000000000000000000, 0.9659258262890683122, 1.000000000000000000, 0.9659258262890683122, 1.000000000000000000, 0.9659258262890683122, 1.000000000000000000, 0.9659258262890683122, 1.000000000000000000, 0.9659258262890683122, 1.000000000000000000, 0.9659258262890683122, 1.000000000000000000, 0.9659258262890683122, 1.000000000000000000, 0.9659258262890683122, 1.000000000000000000, 0.9659258262890683122, 1.000000000000000000, 0.9659258262890683122, 1.000000000000000000, 0.9659258262890683122, 1.000000000000000000, 0.9659258262890683122, 1.000000000000000000, 0.9659258262890683122, 1.000000000000000000, 0.9659258262890683122, 1.000000000000000000, 0.9659258262890683122, 1.000000000000000000, 0.9659258262890683122, 1.000000000000000000, 0.9659258262890683122, 1.000000000000000000, 0.9659258262890683122, 1.000000000000000000, 0.9659258262890683122, 1.000000000000000000, 0.9659258262890683122, 1.000000000000000000, 0.9659258262890683122, 1.000000000000000000, 0.9659258262890683122, 1.000000000000000000, 0.9659258262890683122, 1.000000000000000000, 0.9659258262890683122, 1.000000000000000000, 0.9659258262890683122, 1.000000000000000000, 0.9659258262890683122, 1.000000000000000000, 0.9659258262890683122, 1.000000000000000000, 0.9659258262890683122, 1.000000000000000000, 0.9659258262890683122, 1.000000000000000000, 0.9659258262890683122, 1.000000000000000000, 0.9659258262890683122, 1.000000000000000000, 0.9659258262890683122, 1.000000000000000000, 0.9659258262890683122, 1.000000000000000000, 0.9659258262890683122, 1.000000000000000000, 0.9659258262890683122, 1.000000000000000000, 0.9659258262890683122, 1.000000000000000000, 0.9659258262890683122, 1.000000000000000000, 0.9659258262890683122, 1.000000000000000000, 0.9659258262890683122, 1.000000000000000000, 0.9659258262890683122, 1.000000000000000000, 0.9659258262890683122, 1.000000000000000000, 0.9659258262890683122, 1.000000000000000000, 0.9659258262890683122, 1.000000000000000000, 0.9659258262890683122, 1.000000000000000000, 0.9659258262890683122, 1.000000000000000000, 0.9659258262890683122, 1.000000000000000000, 0.9659258262890683122, 1.000000000000000000, 0.9659258262890683122, 1.000000000000000000, 0.9659258262890683122, 1.000000000000000000, 0.9659258262890683122, 1.000000000000000000, 0.9659258262890683122, 1.000000000000000000, 0.9659258262890683122, 1.000000000000000000, 0.9659258262890683122, 1.000000000000000000, 0.9659258262890683122, 1.000000000000000000, 0.9659258262890683122, 1.000000000000000000, 0.9659258262890683122, 1.000000000000000000, 0.9659258262890683122, 1.000000000000000000, 0.9659258262890683122, 1.000000000000000000, 0.9659258262890683122, 1.000000000000000000, 0.9659258262890683122, 1.000000000000000000, 0.9659258262890683122, 1.000000000000000000, 0.9659258262890683122, 1.000000000000000000, 0.9659258262890683122, 1.000000000000000000, 0.9659258262890683122, 1.000000000000000000, 0.9659258262890683122, 1.000000000000000000, 0.9659258262890683122, 1.000000000000000000, 0.9659258262890683122, 1.000000000000000000, 0.9659258262890683122, 1.000000000000000000, 0.9659258262890683122, 1.000000000000000000, 0.9659258262890683122, 1.000000000000000000, 0.9659258262890683122, 1.000000000000000000, 0.9659258262890683122, 1.000000000000000000, 0.9659258262890683122, 1.000000000000000000, 0.9659258262890683122, 1.000000000000000000, 0.9659258262890683122, 1.000000000000000000, 0.9659258262890683122, 1.000000000000000000, 0.9659258262890683122, 1.000000000000000000, 0.9659258262890683122, 1.000000000000000000, 0.9659258262890683122, 1.000000000000000000, 0.9659258262890683122, 1.000000000000000000, 0.9659258262890683122, 1.000000000000000000, 0.9659258262890683122, 1.000000000000000000, 0.9659258262890683122, 1.000000000000000000, 0.9659258262890683122, 1.000000000000000000, 0.9659258262890683122, 1.000000000000000000, 0.9659258262890683122, 1.000000000000000000, 0.9659258262890683122, 1.000000000000000000, 0.9659258262890683122, 1.000000000000000000, 0.9659258262890683122, 1.000000000000000000, 0.9659258262890683122, 1.000000000000000000, 0.9659258262890683122, 1.000000000000000000, 0.9659258262890683122, 1.000000000000000000, 0.9659258262890683122, 1.000000000000000000, 0.9659258262890683122, 1.000000000000000000, 0.9659258262890683122, 1.000000000000000000, 0.9659258262890683122, 1.000000000000000000, 0.9659258262890683122, 1.000000000000000000, 0.9659258262890683122, 1.000000000000000000, 0.9659258262890683122, 1.000000000000000000, 0.9659258262890683122, 1.000000000000000000, 0.9659258262890683122, 1.000000000000000000, 0.9659258262890683122, 1.000000000000000000, 0.9659258262890683122, 1.000000000000000000, 0.9659258262890683122, 1.000000000000000000, 0.9659258262890683122, 1.000000000000000000, 0.9659258262890683122, 1.000000000000000000, 0.9659258262890683122, 1.000000000000000000, 0.9659258262890683122, 1.000000000000000000, 0.9659258262890683122, 1.000000000000000000, 0.9659258262890683122, 1.000000000000000000, 0.9659258262890683122, 1.000000000000000000, 0.9659258262890683122, 1.000000000000000000, 0.9659258262890683122, 1.000000000000000000, 0.9659258262890683122, 1.000000000000000000, 0.9659258262890683122, 1.000000000000000000, 0.9659258262890683122, 1.000000000000000000, 0.9659258262890683122, 1.000000000000000000, 0.9659258262890683122, 1.000000000000000000, 0.9659258262890683122, 1.000000000000000000, 0.9659258262890683122, 1.000000000000000000, 0.9659258262890683122, 1.000000000000000000, 0.9659258262890683122, 1.000000000000000000, 0.9659258262890683122, 1.000000000000000000, 0.9659258262890683122, 1.000000000000000000, 0.9659258262890683122, 1.000000000000000000, 0.9659258262890683122, 1.000000000000000000, 0.9659258262890683122, 1.000000000000000000, 0.9659258262890683122, 1.000000000000000000, 0.9659258262890683122, 1.000000000000000000, 0.9659258262890683122, 1.000000000000000000, 0.9659258262890683122, 1.000000000000000000, 0.9659258262890683122, 1.000000000000000000, 0.9659258262890683122, 1.000000000000000000, 0.9659258262890683122, 1.000000000000000000, 0.9659258262890683122, 1.000000000000000000, 0.9659258262890683122, 1.000000000000000000, 0.9659258262890683122, 1.000000000000000000, 0.9659258262890683122, 1.000000000000000000, 0.9659258262890683122, 1.000000000000000000, 0.9659258262890683122, 1.000000000000000000, 0.9659258262890683122, 1.000000000000000000, 0.9659258262890683122, 1.000000000000000000, 0.9659258262890683122, 1.000000000000000000, 0.9659258262890683122, 1.000000000000000000, 0.9659258262890683122, 1.000000000000000000, 0.9659258262890683122, 1.000000000000000000, 0.9659258262890683122, 1.000000000000000000, 0.9659258262890683122, 1.000000000000000000, 0.9659258262890683122, 1.000000000000000000, 0.9659258262890683122, 1.000000000000000000, 0.9659258262890683122, 1.000000000000000000, 0.9659258262890683122, 1.000000000000000000, 0.9659258262890683122, 1.000000000000000000, 0.9659258262890683122, 1.000000000000000000, 0.9659258262890683122, 1.000000000000000000, 0.9659258262890683122, 1.000000000000000000, 0.9659258262890683122, 1.000000000000000000, 0.9659258262890683122, 1.000000000000000000, 0.9659258262890683122, 1.000000000000000000, 0.9659258262890683122, 1.000000000000000000, 0.9659258262890683122, 1.000000000000000000, 0.9659258262890683122, 1.000000000000000000, 0.9659258262890683122, 1.000000000000000000, 0.9659258262890683122, 1.000000000000000000, 0.9659258262890683122, 1.000000000000000000, 0.9659258262890683122, 1.000000000000000000, 0.9659258262890683122, 1.000000000000000000, 0.9659258262890683122, 1.000000000000000000, 0.9659258262890683122, 1.000000000000000000, 0.9659258262890683122, 1.000000000000000000, 0.9659258262890683122, 1.000000000000000000, 0.9659258262890683122, 1.000000000000000000, 0.9659258262890683122, 1.000000000000000000, 0.9659258262890683122, 1.000000000000000000, 0.9659258262890683122, 1.000000000000000000, 0.9659258262890683122, 1.000000000000000000, 0.9659258262890683122, 1.000000000000000000, 0.9659258262890683122, 1.000000000000000000, 0.9659258262890683122, 1.000000000000000000, 0.9659258262890683122, 1.000000000000000000, 0.9659258262890683122, 1.000000000000000000, 0.9659258262890683122, 1.000000000000000000, 0.9659258262890683122, 1.000000000000000000, 0.9659258262890683122, 1.000000000000000000),
 ( 1.000000000000000000, 0.9659258262890683122, 1.000000000000000000, 0.9659258262890683122, 1.000000000000000000, 0.9659258262890683122, 1.000000000000000000, 0.9659258262890683122, 1.000000000000000000, 0.9659258262890683122, 1.000000000000000000, 0.9659258262890683122, 1.000000000000000000, 0.9659258262890683122, 1.000000000000000000, 0.9659258262890683122, 1.000000000000000000, 0.9659258262890683122, 1.000000000000000000, 0.9659258262890683122, 1.000000000000000000, 0.9659258262890683122, 1.000000000000000000, 0.9659258262890683122, 1.000000000000000000, 0.9659258262890683122, 1.000000000000000000, 0.9659258262890683122, 1.000000000000000000, 0.9659258262890683122, 1.000000000000000000, 0.9659258262890683122, 1.000000000000000000, 0.9659258262890683122, 1.000000000000000000, 0.9659258262890683122, 1.000000000000000000, 0.9659258262890683122, 1.000000000000000000, 0.9659258262890683122, 1.000000000000000000, 0.9659258262890683122, 1.000000000000000000, 0.9659258262890683122, 1.000000000000000000, 0.9659258262890683122, 1.000000000000000000, 0.9659258262890683122, 1.000000000000000000, 0.9659258262890683122, 1.000000000000000000, 0.9659258262890683122, 1.000000000000000000, 0.9659258262890683122, 1.000000000000000000, 0.9659258262890683122, 1.000000000000000000, 0.9659258262890683122, 1.000000000000000000, 0.9659258262890683122, 1.000000000000000000, 0.9659258262890683122, 1.000000000000000000, 0.9659258262890683122, 1.000000000000000000, 0.9659258262890683122, 1.000000000000000000, 0.9659258262890683122, 1.000000000000000000, 0.9659258262890683122, 1.000000000000000000, 0.9659258262890683122, 1.000000000000000000, 0.9659258262890683122, 1.000000000000000000, 0.9659258262890683122, 1.000000000000000000, 0.9659258262890683122, 1.000000000000000000, 0.9659258262890683122, 1.000000000000000000, 0.9659258262890683122, 1.000000000000000000, 0.9659258262890683122, 1.000000000000000000, 0.9659258262890683122, 1.000000000000000000, 0.9659258262890683122, 1.000000000000000000, 0.9659258262890683122, 1.000000000000000000, 0.9659258262890683122, 1.000000000000000000, 0.9659258262890683122, 1.000000000000000000, 0.9659258262890683122, 1.000000000000000000, 0.9659258262890683122, 1.000000000000000000, 0.9659258262890683122, 1.000000000000000000, 0.9659258262890683122, 1.000000000000000000, 0.9659258262890683122, 1.000000000000000000, 0.9659258262890683122, 1.000000000000000000, 0.9659258262890683122, 1.000000000000000000, 0.9659258262890683122, 1.000000000000000000, 0.9659258262890683122, 1.000000000000000000, 0.9659258262890683122, 1.000000000000000000, 0.9659258262890683122, 1.000000000000000000, 0.9659258262890683122, 1.000000000000000000, 0.9659258262890683122, 1.000000000000000000, 0.9659258262890683122, 1.000000000000000000, 0.9659258262890683122, 1.000000000000000000, 0.9659258262890683122, 1.000000000000000000, 0.9659258262890683122, 1.000000000000000000, 0.9659258262890683122, 1.000000000000000000, 0.9659258262890683122, 1.000000000000000000, 0.9659258262890683122, 1.000000000000000000, 0.9659258262890683122, 1.000000000000000000, 0.9659258262890683122, 1.000000000000000000, 0.9659258262890683122, 1.000000000000000000, 0.9659258262890683122, 1.000000000000000000, 0.9659258262890683122, 1.000000000000000000, 0.9659258262890683122, 1.000000000000000000, 0.9659258262890683122, 1.000000000000000000, 0.9659258262890683122, 1.000000000000000000, 0.9659258262890683122, 1.000000000000000000, 0.9659258262890683122, 1.000000000000000000, 0.9659258262890683122, 1.000000000000000000, 0.9659258262890683122, 1.000000000000000000, 0.9659258262890683122, 1.000000000000000000, 0.9659258262890683122, 1.000000000000000000, 0.9659258262890683122, 1.000000000000000000, 0.9659258262890683122, 1.000000000000000000, 0.9659258262890683122, 1.000000000000000000, 0.9659258262890683122, 1.000000000000000000, 0.9659258262890683122, 1.000000000000000000, 0.9659258262890683122, 1.000000000000000000, 0.9659258262890683122, 1.000000000000000000, 0.9659258262890683122, 1.000000000000000000, 0.9659258262890683122, 1.000000000000000000, 0.9659258262890683122, 1.000000000000000000, 0.9659258262890683122, 1.000000000000000000, 0.9659258262890683122, 1.000000000000000000, 0.9659258262890683122, 1.000000000000000000, 0.9659258262890683122, 1.000000000000000000, 0.9659258262890683122, 1.000000000000000000, 0.9659258262890683122, 1.000000000000000000, 0.9659258262890683122, 1.000000000000000000, 0.9659258262890683122, 1.000000000000000000, 0.9659258262890683122, 1.000000000000000000, 0.9659258262890683122, 1.000000000000000000, 0.9659258262890683122, 1.000000000000000000, 0.9659258262890683122, 1.000000000000000000, 0.9659258262890683122, 1.000000000000000000, 0.9659258262890683122, 1.000000000000000000, 0.9659258262890683122, 1.000000000000000000, 0.9659258262890683122, 1.000000000000000000, 0.9659258262890683122, 1.000000000000000000, 0.9659258262890683122, 1.000000000000000000, 0.9659258262890683122, 1.000000000000000000, 0.9659258262890683122, 1.000000000000000000, 0.9659258262890683122, 1.000000000000000000, 0.9659258262890683122, 1.000000000000000000, 0.9659258262890683122, 1.000000000000000000, 0.9659258262890683122, 1.000000000000000000, 0.9659258262890683122, 1.000000000000000000, 0.9659258262890683122, 1.000000000000000000, 0.9659258262890683122, 1.000000000000000000, 0.9659258262890683122, 1.000000000000000000, 0.9659258262890683122, 1.000000000000000000, 0.9659258262890683122, 1.000000000000000000, 0.9659258262890683122, 1.000000000000000000, 0.9659258262890683122, 1.000000000000000000, 0.9659258262890683122, 1.000000000000000000, 0.9659258262890683122, 1.000000000000000000, 0.9659258262890683122, 1.000000000000000000, 0.9659258262890683122, 1.000000000000000000, 0.9659258262890683122, 1.000000000000000000, 0.9659258262890683122, 1.000000000000000000, 0.9659258262890683122, 1.000000000000000000, 0.9659258262890683122, 1.000000000000000000, 0.9659258262890683122, 1.000000000000000000, 0.9659258262890683122, 1.000000000000000000, 0.9659258262890683122, 1.000000000000000000, 0.9659258262890683122, 1.000000000000000000, 0.9659258262890683122, 1.000000000000000000, 0.9659258262890683122, 1.000000000000000000, 0.9659258262890683122, 1.000000000000000000, 0.9659258262890683122, 1.000000000000000000, 0.9659258262890683122, 1.000000000000000000, 0.9659258262890683122, 1.000000000000000000, 0.9659258262890683122, 1.000000000000000000, 0.9659258262890683122, 1.000000000000000000, 0.9659258262890683122, 1.000000000000000000, 0.9659258262890683122, 1.000000000000000000, 0.9659258262890683122, 1.000000000000000000, 0.9659258262890683122, 1.000000000000000000, 0.9659258262890683122, 1.000000000000000000, 0.9659258262890683122, 1.000000000000000000, 0.9659258262890683122, 1.000000000000000000, 0.9659258262890683122, 1.000000000000000000, 0.9659258262890683122, 1.000000000000000000, 0.9659258262890683122, 1.000000000000000000, 0.9659258262890683122, 1.000000000000000000, 0.9659258262890683122, 1.000000000000000000, 0.9659258262890683122, 1.000000000000000000, 0.9659258262890683122, 1.000000000000000000, 0.9659258262890683122, 1.000000000000000000, 0.9659258262890683122, 1.000000000000000000, 0.9659258262890683122, 1.000000000000000000, 0.9659258262890683122, 1.000000000000000000, 0.9659258262890683122, 1.000000000000000000, 0.9659258262890683122, 1.000000000000000000, 0.9659258262890683122, 1.000000000000000000, 0.9659258262890683122, 1.000000000000000000, 0.9659258262890683122, 1.000000000000000000, 0.9659258262890683122, 1.000000000000000000, 0.9659258262890683122, 1.000000000000000000, 0.9659258262890683122, 1.000000000000000000, 0.9659258262890683122, 1.000000000000000000, 0.9659258262890683122, 1.000000000000000000, 0.9659258262890683122, 1.000000000000000000, 0.9659258262890683122, 1.000000000000000000, 0.9659258262890683122, 1.000000000000000000, 0.9659258262890683122, 1.000000000000000000, 0.9659258262890683122, 1.000000000000000000, 0.9659258262890683122, 1.000000000000000000, 0.9659258262890683122, 1.000000000000000000, 0.9659258262890683122, 1.000000000000000000, 0.9659258262890683122, 1.000000000000000000, 0.9659258262890683122, 1.000000000000000000, 0.9659258262890683122, 1.000000000000000000, 0.9659258262890683122, 1.000000000000000000, 0.9659258262890683122, 1.000000000000000000, 0.9659258262890683122, 1.000000000000000000, 0.9659258262890683122, 1.000000000000000000, 0.9659258262890683122, 1.000000000000000000, 0.9659258262890683122, 1.000000000000000000, 0.9659258262890683122, 1.000000000000000000, 0.9659258262890683122, 1.000000000000000000, 0.9659258262890683122, 1.000000000000000000, 0.9659258262890683122, 1.000000000000000000, 0.9659258262890683122, 1.000000000000000000, 0.9659258262890683122, 1.000000000000000000, 0.9659258262890683122, 1.000000000000000000, 0.9659258262890683122, 1.000000000000000000, 0.9659258262890683122, 1.000000000000000000, 0.9659258262890683122, 1.000000000000000000, 0.9659258262890683122, 1.000000000000000000, 0.9659258262890683122, 1.000000000000000000, 0.9659258262890683122, 1.000000000000000000, 0.9659258262890683122, 1.000000000000000000, 0.9659258262890683122, 1.000000000000000000, 0.9659258262890683122, 1.000000000000000000, 0.9659258262890683122, 1.000000000000000000, 0.9659258262890683122, 1.000000000000000000, 0.9659258262890683122, 1.000000000000000000, 0.9659258262890683122, 1.000000000000000000, 0.9659258262890683122, 1.000000000000000000, 0.9659258262890683122, 1.000000000000000000, 0.9659258262890683122, 1.000000000000000000, 0.9659258262890683122, 1.000000000000000000, 0.9659258262890683122, 1.000000000000000000, 0.9659258262890683122, 1.000000000000000000, 0.9659258262890683122, 1.000000000000000000, 0.9659258262890683122, 1.000000000000000000, 0.9659258262890683122, 1.000000000000000000, 0.9659258262890683122, 1.000000000000000000, 0.9659258262890683122, 1.000000000000000000, 0.9659258262890683122, 1.000000000000000000, 0.9659258262890683122, 1.000000000000000000, 0.9659258262890683122, 1.000000000000000000, 0.9659258262890683122, 1.000000000000000000, 0.9659258262890683122, 1.000000000000000000, 0.9659258262890683122, 1.000000000000000000, 0.9659258262890683122, 1.000000000000000000, 0.9659258262890683122, 1.000000000000000000, 0.9659258262890683122, 1.000000000000000000, 0.9659258262890683122, 1.000000000000000000, 0.9659258262890683122, 1.000000000000000000, 0.9659258262890683122, 1.000000000000000000, 0.9659258262890683122, 1.000000000000000000, 0.9659258262890683122, 1.000000000000000000, 0.9659258262890683122, 1.000000000000000000, 0.9659258262890683122, 1.000000000000000000, 0.9659258262890683122, 1.000000000000000000, 0.9659258262890683122, 1.000000000000000000, 0.9659258262890683122, 1.000000000000000000, 0.9659258262890683122, 1.000000000000000000, 0.9659258262890683122, 1.000000000000000000, 0.9659258262890683122, 1.000000000000000000, 0.9659258262890683122, 1.000000000000000000, 0.9659258262890683122, 1.000000000000000000, 0.9659258262890683122, 1.000000000000000000, 0.9659258262890683122, 1.000000000000000000, 0.9659258262890683122, 1.000000000000000000, 0.9659258262890683122, 1.000000000000000000, 0.9659258262890683122, 1.000000000000000000, 0.9659258262890683122, 1.000000000000000000, 0.9659258262890683122, 1.000000000000000000, 0.9659258262890683122, 1.000000000000000000, 0.9659258262890683122, 1.000000000000000000, 0.9659258262890683122, 1.000000000000000000, 0.9659258262890683122, 1.000000000000000000, 0.9659258262890683122, 1.000000000000000000) ) ) 
 REPRESENTATION_ITEM ( '' )  SURFACE ( )  );
#16419 = CARTESIAN_POINT ( 'NONE',  ( 0.1070741851644053388, 0.3996062992125986035, -0.2276902887139107545 ) ) ;
#16420 = CARTESIAN_POINT ( 'NONE',  ( -1.167979002624671470, -0.4281496062992127816, -0.4176697321401328100 ) ) ;
#16421 = CARTESIAN_POINT ( 'NONE',  ( 0.3917322834645669549, 0.1049643490035304660, -1.626640419947506411 ) ) ;
#16422 = CARTESIAN_POINT ( 'NONE',  ( 1.174540682414699111, -0.08942795157528024563, -0.3641732283464568787 ) ) ;
#16423 = CARTESIAN_POINT ( 'NONE',  ( -0.01312335958005186876, 0.05413385826771626580, -0.4176697321401330321 ) ) ;
#16424 = CARTESIAN_POINT ( 'NONE',  ( -0.4593175853018364174, -0.4281496062992127816, -0.4176697321401328100 ) ) ;
#16425 = CARTESIAN_POINT ( 'NONE',  ( -0.3149606299212590610, -0.1870078740157480601, -0.3641732283464567677 ) ) ;
#16426 = CARTESIAN_POINT ( 'NONE',  ( 1.016821367227983774, 1.537401574803149984, -0.4744094488188970171 ) ) ;
#16427 = CARTESIAN_POINT ( 'NONE',  ( -0.5052493438320203589, 0.1771653543307087075, -0.09757992244046823083 ) ) ;
#16428 = CARTESIAN_POINT ( 'NONE',  ( 0.4593175853018380828, 0.05413385826771626580, -0.4176697321401330321 ) ) ;
#16429 = CARTESIAN_POINT ( 'NONE',  ( -1.227034120734907585, 0.1771653543307087630, 0.09757992244046791164 ) ) ;
#16430 = CARTESIAN_POINT ( 'NONE',  ( 0.1070741851644054776, -0.3996062992125984925, -0.7919947506561679784 ) ) ;
#16431 = CARTESIAN_POINT ( 'NONE',  ( -1.122047244094487306, 0.1660481256975883668, -0.3530559997133364547 ) ) ;
#16432 = CARTESIAN_POINT ( 'NONE',  ( -0.4091458600556405756, 0.2362204724409446288, -2.622703412073490892 ) ) ;
#16433 = VERTEX_POINT ( 'NONE', #55908 ) ;
#16434 = CARTESIAN_POINT ( 'NONE',  ( -1.587926509186350810, -0.3690944881889763329, 0.3153832671262228327 ) ) ;
#16435 = AXIS2_PLACEMENT_3D ( 'NONE', #81031, #36800, #16640 ) ;
#16436 = CARTESIAN_POINT ( 'NONE',  ( -0.6167979002624665030, 0.05413385826771666132, 0.4176697321401328100 ) ) ;
#16437 = CARTESIAN_POINT ( 'NONE',  ( 0.4744094488188886904, 1.528796061338913104, 2.554262525012302554 ) ) ;
#16438 = CARTESIAN_POINT ( 'NONE',  ( -1.200787401574802349, -0.5400638737290844871, 0.3530559997133364547 ) ) ;
#16439 = CARTESIAN_POINT ( 'NONE',  ( 0.1049643490035303689, 0.3917322834645670104, -1.495406824146981117 ) ) ;
#16440 = CARTESIAN_POINT ( 'NONE',  ( 0.000000000000000000, 0.000000000000000000, 0.000000000000000000 ) ) ;
#16441 = CARTESIAN_POINT ( 'NONE',  ( 1.489501312335958172, -0.3162353388693405765, 0.4822834645669290543 ) ) ;
#16442 = CARTESIAN_POINT ( 'NONE',  ( 0.4002624671916016896, -0.05778040916215522460, 0.4822834645669289988 ) ) ;
#16443 = CARTESIAN_POINT ( 'NONE',  ( -1.646051170424378096, 0.8346805926620876059, -0.3149606299212598381 ) ) ;
#16444 = CARTESIAN_POINT ( 'NONE',  ( 0.3460692066303958092, 0.1998031496062993018, -2.570209973753280863 ) ) ;
#16445 = CARTESIAN_POINT ( 'NONE',  ( -1.712598425196849572, 0.1660481256975885056, 0.3530559997133364547 ) ) ;
#16446 = CARTESIAN_POINT ( 'NONE',  ( -0.3996062992125986035, -7.340648628747425578E-17, -0.5118110236220472231 ) ) ;
#16447 = ORIENTED_EDGE ( 'NONE', *, *, #40694, .F. ) ;
#16448 = CARTESIAN_POINT ( 'NONE',  ( -0.8661417322834640276, -0.1870078740157479769, 0.3641732283464567677 ) ) ;
#16449 = CARTESIAN_POINT ( 'NONE',  ( -9.594673741351313045E-17, 0.3917322834645670104, -2.196850393700787496 ) ) ;
#16450 = VERTEX_POINT ( 'NONE', #74471 ) ;
#16451 = CARTESIAN_POINT ( 'NONE',  ( 0.8070866141732288002, 0.1660481256975885056, 0.3530559997133364547 ) ) ;
#16452 = CARTESIAN_POINT ( 'NONE',  ( -0.4986876640419942164, -0.6046776061558807314, 0.2411417322834647770 ) ) ;
#16453 = CARTESIAN_POINT ( 'NONE',  ( -1.049868766404198794, -0.6046776061558807314, 0.2411417322834647770 ) ) ;
#16454 = CARTESIAN_POINT ( 'NONE',  ( 1.181102362204725198, -0.1870078740157479769, 0.4822834645669291653 ) ) ;
#16455 = CARTESIAN_POINT ( 'NONE',  ( -1.384514435695537005, -0.5511811023622048555, -0.09757992244046775898 ) ) ;
#16456 = CARTESIAN_POINT ( 'NONE',  ( 0.6867064689427456736, 2.290696638571109833, -0.1693427315076261597 ) ) ;
#16457 = CARTESIAN_POINT ( 'NONE',  ( 0.3412073490813655186, -0.6046776061558809534, -0.2411417322834644161 ) ) ;
#16458 = CARTESIAN_POINT ( 'NONE',  ( -0.8267716535433065062, 0.2952755905511811885, 0.000000000000000000 ) ) ;
#16459 = CARTESIAN_POINT ( 'NONE',  ( 0.1958661417322834497, 0.3392501089628018329, -1.484232652722097923 ) ) ;
#16460 = CARTESIAN_POINT ( 'NONE',  ( -1.082677165354329896, -0.5400638737290845981, -0.3530559997133363437 ) ) ;
#16461 = DIRECTION ( 'NONE',  ( 0.000000000000000000, 0.000000000000000000, 1.000000000000000000 ) ) ;
#16462 = CARTESIAN_POINT ( 'NONE',  ( 0.7874015748031503170, -0.1870078740157480879, -0.4822834645669291653 ) ) ;
#16463 = CARTESIAN_POINT ( 'NONE',  ( 0.2867679344610365999, -0.2867679344610365444, -2.860236220472440749 ) ) ;
#16464 = CARTESIAN_POINT ( 'NONE',  ( 1.318897637795276356, -0.4536011799217367080, 0.2665933059059888421 ) ) ;
#16465 = ORIENTED_EDGE ( 'NONE', *, *, #63766, .T. ) ;
#16466 = CARTESIAN_POINT ( 'NONE',  ( -0.1974969037888706647, 0.3420746716998658843, 0.1443569553805773842 ) ) ;
#16467 = CARTESIAN_POINT ( 'NONE',  ( -0.3740157480314953431, 0.1660481256975885056, 0.3530559997133364547 ) ) ;
#16468 = VERTEX_POINT ( 'NONE', #43682 ) ;
#16469 = CARTESIAN_POINT ( 'NONE',  ( 0.3412073490813655186, 0.1283753931104748280, 0.1820866141732283561 ) ) ;
#16470 = CARTESIAN_POINT ( 'NONE',  ( -1.535433070866141225, 0.2952755905511811885, 0.000000000000000000 ) ) ;
#16471 = CARTESIAN_POINT ( 'NONE',  ( 0.9842519685039375910, 0.2952755905511811885, 0.000000000000000000 ) ) ;
#16472 = CARTESIAN_POINT ( 'NONE',  ( 0.9186351706036751663, -0.6046776061558807314, 0.2411417322834647770 ) ) ;
#16473 = CARTESIAN_POINT ( 'NONE',  ( 0.01312335958005323398, 0.05413385826771666132, 0.4176697321401328100 ) ) ;
#16474 = CARTESIAN_POINT ( 'NONE',  ( 0.3392501089628018329, 0.1958661417322835607, -1.072853961451130544 ) ) ;
#16475 = CARTESIAN_POINT ( 'NONE',  ( -0.6889763779527552368, 0.1660481256975885056, 0.3530559997133364547 ) ) ;
#16476 = CARTESIAN_POINT ( 'NONE',  ( -0.1958661417322836718, 0.3392501089628017219, -2.145013123359580387 ) ) ;
#16477 = CARTESIAN_POINT ( 'NONE',  ( -1.627296587926508442, -0.6046776061558809534, -0.2411417322834644161 ) ) ;
#16478 = CARTESIAN_POINT ( 'NONE',  ( -1.089238845144356427, -0.4281496062992127816, -0.4176697321401328100 ) ) ;
#16479 = CARTESIAN_POINT ( 'NONE',  ( 1.246719160104987623, 0.05413385826771626580, -0.4176697321401330321 ) ) ;
#16480 = DIRECTION ( 'NONE',  ( 1.047444401652940007E-14, -0.000000000000000000, -1.000000000000000000 ) ) ;
#16481 = CARTESIAN_POINT ( 'NONE',  ( -0.8398950131233589023, -0.6046776061558809534, -0.2411417322834644161 ) ) ;
#16482 = CARTESIAN_POINT ( 'NONE',  ( -0.5314960629921371416, 2.729659898468815182, 3.210901144249700412 ) ) ;
#16483 = CARTESIAN_POINT ( 'NONE',  ( 0.3018372703412079971, -0.4281496062992124485, 0.4176697321401328655 ) ) ;
#16484 = CARTESIAN_POINT ( 'NONE',  ( -0.2925321140481932924, 0.2925321140481931814, -1.909448818897637512 ) ) ;
#16485 = EDGE_CURVE ( 'NONE', #1243, #7519, #53371, .T. ) ;
#16486 = CARTESIAN_POINT ( 'NONE',  ( -0.6496062992125976043, 0.1660481256975883668, -0.3530559997133364547 ) ) ;
#16487 = CARTESIAN_POINT ( 'NONE',  ( -1.502624671916009680, -0.2845877964562159024, 0.3641732283464567677 ) ) ;
#16488 = CARTESIAN_POINT ( 'NONE',  ( 0.6299212598425204535, -0.1870078740157480601, -0.3641732283464567677 ) ) ;
#16489 = CARTESIAN_POINT ( 'NONE',  ( 1.430446194225722500, 0.05413385826771666132, 0.4176697321401328100 ) ) ;
#16490 = CARTESIAN_POINT ( 'NONE',  ( 0.3458507752293908943, -0.3458507752293908943, -1.120078740157480324 ) ) ;
#16491 = CARTESIAN_POINT ( 'NONE',  ( 0.8792650918635177559, -0.004921259842519576551, 0.3153832671262227771 ) ) ;
#16492 = CARTESIAN_POINT ( 'NONE',  ( 0.5971128608923890191, -0.6692913385826771977, 0.1292274648535927661 ) ) ;
#16493 = VECTOR ( 'NONE', #24151, 39.37007874015748143 ) ;
#16494 = EDGE_CURVE ( 'NONE', #21005, #64347, #10386, .T. ) ;
#16495 = CARTESIAN_POINT ( 'NONE',  ( -0.3949938075777411073, 0.1058382717557497660, -0.4245406824146981672 ) ) ;
#16496 = CARTESIAN_POINT ( 'NONE',  ( -0.2296587926509179312, -0.3162353388693409650, -0.4822834645669289433 ) ) ;
#16497 = FACE_OUTER_BOUND ( 'NONE', #70374, .T. ) ;
#16498 = CARTESIAN_POINT ( 'NONE',  ( 1.463254593175853824, 0.1771653543307087075, -0.09757992244046823083 ) ) ;
#16499 = CARTESIAN_POINT ( 'NONE',  ( -0.7152230971128602510, -0.05778040916215560624, -0.4822834645669293319 ) ) ;
#16500 = CARTESIAN_POINT ( 'NONE',  ( -0.3949938075777408852, -0.1058382717557502933, -0.4376640419947507299 ) ) ;
#16501 = CARTESIAN_POINT ( 'NONE',  ( 1.253280839895013710, -0.05778040916215560624, -0.4822834645669293319 ) ) ;
#16502 = CARTESIAN_POINT ( 'NONE',  ( 0.1509186351706042484, -0.3162353388693405765, 0.4822834645669290543 ) ) ;
#16503 = CIRCLE ( 'NONE', #27228, 2.165354330708661568 ) ;
#16504 = CARTESIAN_POINT ( 'NONE',  ( 0.3608923884514443348, -0.5511811023622046335, 0.09757992244046803654 ) ) ;
#16505 = CARTESIAN_POINT ( 'NONE',  ( -0.1241822272904720692, 1.079268584176191093, -1.115255186249766384 ) ) ;
#16506 = CARTESIAN_POINT ( 'NONE',  ( -0.07217847769028787330, -0.08942795157527998196, 0.3641732283464567121 ) ) ;
#16507 = CARTESIAN_POINT ( 'NONE',  ( 0.8070866141732288002, 0.07958543189024085140, 0.2665933059059887866 ) ) ;
#16508 = CARTESIAN_POINT ( 'NONE',  ( -1.633858267716534529, 0.1660481256975885056, 0.3530559997133364547 ) ) ;
#16509 = CARTESIAN_POINT ( 'NONE',  ( 0.3996062992125984925, 0.1070741851644054637, -1.303805774278215202 ) ) ;
#16510 = CARTESIAN_POINT ( 'NONE',  ( 0.9514435695538062676, -0.3162353388693409650, -0.4822834645669289433 ) ) ;
#16511 = CARTESIAN_POINT ( 'NONE',  ( 0.2867679344610365999, 0.2867679344610365999, -0.9173228346456693272 ) ) ;
#16512 = CARTESIAN_POINT ( 'NONE',  ( 1.646981627296588035, -0.2845877964562159024, 0.3641732283464567677 ) ) ;
#16513 = CARTESIAN_POINT ( 'NONE',  ( -0.3486222174624316050, 0.1789624963018554005, -1.599317578742253179E-17 ) ) ;
#16514 = CARTESIAN_POINT ( 'NONE',  ( 0.006561679790026889343, -0.08942795157527998196, 0.3641732283464567121 ) ) ;
#16515 = CARTESIAN_POINT ( 'NONE',  ( 0.04593175853018440641, -0.6692913385826771977, 0.1292274648535927661 ) ) ;
#16516 = CARTESIAN_POINT ( 'NONE',  ( 1.463254593175853824, -0.5511811023622046335, 0.09757992244046803654 ) ) ;
#16517 = CARTESIAN_POINT ( 'NONE',  ( -1.213910761154854745, 0.1771653543307087075, -0.09757992244046823083 ) ) ;
#16518 = CARTESIAN_POINT ( 'NONE',  ( -1.371391076115484831, 0.2952755905511810774, -0.1292274648535930714 ) ) ;
#16519 = CARTESIAN_POINT ( 'NONE',  ( 0.7283464566929143125, 0.1660481256975885056, 0.3530559997133364547 ) ) ;
#16520 = CARTESIAN_POINT ( 'NONE',  ( 1.181102362204725198, -0.1870078740157479769, 0.4822834645669291653 ) ) ;
#16521 = CARTESIAN_POINT ( 'NONE',  ( -0.1265901696524993347, 0.4724409448818896462, -0.2408136482939632061 ) ) ;
#16522 = CARTESIAN_POINT ( 'NONE',  ( -0.02624671916010428221, -0.6046776061558807314, 0.2411417322834647770 ) ) ;
#16523 = CARTESIAN_POINT ( 'NONE',  ( 1.391076115485564868, 0.2306618581243847221, -0.2411417322834647770 ) ) ;
#16524 = CARTESIAN_POINT ( 'NONE',  ( 0.9776902887139113929, -0.6692913385826773087, -0.1292274648535924053 ) ) ;
#16525 = CIRCLE ( 'NONE', #45589, 2.401574803149606474 ) ;
#16526 = CARTESIAN_POINT ( 'NONE',  ( -0.3458507752293906723, -0.3458507752293910609, -0.2933070866141732624 ) ) ;
#16527 = CARTESIAN_POINT ( 'NONE',  ( 0.9448818897637802916, -0.1870078740157480601, -0.3641732283464567677 ) ) ;
#16528 = CARTESIAN_POINT ( 'NONE',  ( 1.666666666666667185, 0.05413385826771666132, 0.4176697321401328100 ) ) ;
#16529 = CARTESIAN_POINT ( 'NONE',  ( 0.03280839895013198948, 0.1771653543307087630, 0.09757992244046791164 ) ) ;
#16530 = CARTESIAN_POINT ( 'NONE',  ( 0.05249343832021075018, -0.6046776061558807314, 0.2411417322834647770 ) ) ;
#16531 = CARTESIAN_POINT ( 'NONE',  ( 0.7414698162729663755, -0.6692913385826773087, -0.1292274648535924053 ) ) ;
#16532 = CARTESIAN_POINT ( 'NONE',  ( -0.1640419947506553400, -0.05778040916215560624, -0.4822834645669293319 ) ) ;
#16533 = CARTESIAN_POINT ( 'NONE',  ( -0.1312335958005241554, 0.1283753931104748280, 0.1820866141732283561 ) ) ;
#16534 = CARTESIAN_POINT ( 'NONE',  ( 0.6627296587926515548, 0.2952755905511811885, 0.1292274648535926551 ) ) ;
#16535 = CARTESIAN_POINT ( 'NONE',  ( 0.7611548556430454138, 0.1283753931104746893, -0.1820866141732285504 ) ) ;
#16536 = DIRECTION ( 'NONE',  ( 1.000000000000000000, 8.462065736472231082E-17, 0.000000000000000000 ) ) ;
#16538 = CARTESIAN_POINT ( 'NONE',  ( -0.1998031496062991907, -0.3460692066303959757, -1.010498687664042050 ) ) ;
#16537 = CARTESIAN_POINT ( 'NONE',  ( -0.4724409448818898682, 5.785732909357575061E-17, -2.755905511811024056 ) ) ;
#16539 = CARTESIAN_POINT ( 'NONE',  ( 2.103512204792505447, 1.710976477253049577, -0.4417575354491481421 ) ) ;
#16540 = CARTESIAN_POINT ( 'NONE',  ( -1.128608923884513837, 0.2306618581243847221, -0.2411417322834647770 ) ) ;
#16541 = CARTESIAN_POINT ( 'NONE',  ( -0.4396325459317579898, 0.2952755905511811885, 0.1292274648535926551 ) ) ;
#16542 = CARTESIAN_POINT ( 'NONE',  ( -0.3458507752293909498, 0.3458507752293907833, 0.1377952755905511861 ) ) ;
#16543 = CARTESIAN_POINT ( 'NONE',  ( 0.1058382717557500713, -0.3949938075777409408, -2.447506561679789971 ) ) ;
#16544 = ORIENTED_EDGE ( 'NONE', *, *, #11244, .F. ) ;
#16545 = CARTESIAN_POINT ( 'NONE',  ( 0.5577427821522316087, -0.08942795157527998196, 0.3641732283464567121 ) ) ;
#16546 = CARTESIAN_POINT ( 'NONE',  ( 0.3917322834645669549, 0.1049643490035304660, -1.061679790026246462 ) ) ;
#16547 = CARTESIAN_POINT ( 'NONE',  ( 1.299212598425197429, 0.2952755905511811885, 0.000000000000000000 ) ) ;
#16548 = EDGE_CURVE ( 'NONE', #68098, #9892, #9953, .T. ) ;
#16549 = CARTESIAN_POINT ( 'NONE',  ( 0.4091458600556403535, 0.2362204724409449896, -2.493438320209973469 ) ) ;
#16550 = DIRECTION ( 'NONE',  ( 0.000000000000000000, 1.000000000000000000, 0.000000000000000000 ) ) ;
#16551 = CARTESIAN_POINT ( 'NONE',  ( -1.213910761154854745, 0.1771653543307087075, -0.09757992244046823083 ) ) ;
#16552 = CARTESIAN_POINT ( 'NONE',  ( -0.03177986912255784807, 1.063795733429741874, 1.121706799229931217 ) ) ;
#16553 = CARTESIAN_POINT ( 'NONE',  ( 1.397637795275591177, -0.4536011799217367080, 0.2665933059059888421 ) ) ;
#16554 = CARTESIAN_POINT ( 'NONE',  ( 0.2493438320209980519, 0.05413385826771666132, 0.4176697321401328100 ) ) ;
#16555 = CARTESIAN_POINT ( 'NONE',  ( -0.3392501089628019439, 0.1958661417322832554, -0.4212405267378459550 ) ) ;
#16556 = CARTESIAN_POINT ( 'NONE',  ( 0.1246719160104994284, 0.2952755905511810774, -0.1292274648535930714 ) ) ;
#16557 = CARTESIAN_POINT ( 'NONE',  ( -0.9645669291338575535, -0.4536011799217367080, 0.2665933059059888421 ) ) ;
#16558 = CARTESIAN_POINT ( 'NONE',  ( 0.3149606299212603933, -0.1870078740157479769, 0.4822834645669291653 ) ) ;
#16559 = CARTESIAN_POINT ( 'NONE',  ( -0.2427821522309703550, -0.05778040916215560624, -0.4822834645669293319 ) ) ;
#16560 = CARTESIAN_POINT ( 'NONE',  ( -0.1341536278048623410, 0.7086614173228346081, 0.2827841492639507903 ) ) ;
#16561 = CARTESIAN_POINT ( 'NONE',  ( -0.3460692066303958092, -0.1998031496062994683, -2.887139107611548461 ) ) ;
#16562 = CARTESIAN_POINT ( 'NONE',  ( 0.1958661417322834775, 0.3392501089628018884, -1.558418265913072309 ) ) ;
#16563 = CARTESIAN_POINT ( 'NONE',  ( 0.9055118110236227702, 0.2952755905511811885, 0.000000000000000000 ) ) ;
#16564 = CARTESIAN_POINT ( 'NONE',  ( -0.4593175853018366950, 0.05413385826771666132, 0.4176697321401328100 ) ) ;
#16565 = CARTESIAN_POINT ( 'NONE',  ( -1.082677165354329896, -0.5400638737290845981, -0.3530559997133363437 ) ) ;
#16566 = CARTESIAN_POINT ( 'NONE',  ( 1.279527559055118724, 0.1660481256975885056, 0.3530559997133364547 ) ) ;
#16567 = CARTESIAN_POINT ( 'NONE',  ( 0.4002624671916016896, -0.05778040916215522460, 0.4822834645669289988 ) ) ;
#16568 = CARTESIAN_POINT ( 'NONE',  ( 0.1049643490035304938, -0.3917322834645669549, -0.7998687664041995715 ) ) ;
#16569 = CARTESIAN_POINT ( 'NONE',  ( -0.5249343832020990641, -0.6046776061558809534, -0.2411417322834644161 ) ) ;
#16570 = CARTESIAN_POINT ( 'NONE',  ( 0.4199475065616805614, 0.2306618581243848609, 0.2411417322834645549 ) ) ;
#16571 = CARTESIAN_POINT ( 'NONE',  ( -0.4593175853018364174, -0.4281496062992127816, -0.4176697321401328100 ) ) ;
#16572 = CARTESIAN_POINT ( 'NONE',  ( 0.7677165354330716118, 0.07958543189024071263, -0.2665933059059888421 ) ) ;
#16573 = CARTESIAN_POINT ( 'NONE',  ( -1.666666666666665853, 0.05413385826771626580, -0.4176697321401330321 ) ) ;
#16574 = CARTESIAN_POINT ( 'NONE',  ( -0.4698482617964682140, 1.469690627553818185, -2.565218379528205528 ) ) ;
#16575 = CARTESIAN_POINT ( 'NONE',  ( 0.2624671916010504757, -0.6046776061558809534, -0.2411417322834644161 ) ) ;
#16576 = CARTESIAN_POINT ( 'NONE',  ( 5.785732909357575061E-17, -0.4724409448818898682, -0.9429133858267716439 ) ) ;
#16577 = CARTESIAN_POINT ( 'NONE',  ( 0.3917322834645670104, 2.398668435337828261E-17, -2.314960629921259727 ) ) ;
#16578 = ORIENTED_EDGE ( 'NONE', *, *, #43922, .F. ) ;
#16579 = ORIENTED_EDGE ( 'NONE', *, *, #66747, .T. ) ;
#16580 = CARTESIAN_POINT ( 'NONE',  ( 0.5380577427821529035, -0.4281496062992124485, 0.4176697321401328655 ) ) ;
#16581 = CARTESIAN_POINT ( 'NONE',  ( 0.3871391076115492380, -0.08942795157528024563, -0.3641732283464568787 ) ) ;
#16583 = DIRECTION ( 'NONE',  ( 0.000000000000000000, -1.000000000000000000, 0.000000000000000000 ) ) ;
#16582 = CARTESIAN_POINT ( 'NONE',  ( 0.9555810825238854056, -8.614921172258640174E-17, 0.4118477457932991359 ) ) ;
#16584 = CARTESIAN_POINT ( 'NONE',  ( -0.3917322834645669549, -0.1049643490035306603, -0.6030183727034120755 ) ) ;
#16585 = CARTESIAN_POINT ( 'NONE',  ( 0.5314960629920917334, 2.755905511811024056, 3.264097702071378393 ) ) ;
#16586 = CARTESIAN_POINT ( 'NONE',  ( -0.2925321140481932369, 0.2925321140481931259, -2.616141732283464805 ) ) ;
#16587 = CARTESIAN_POINT ( 'NONE',  ( 0.8923884514435701520, -0.6046776061558809534, -0.2411417322834644161 ) ) ;
#16588 = CARTESIAN_POINT ( 'NONE',  ( -0.7152230971128602510, -0.3162353388693405765, 0.4822834645669290543 ) ) ;
#16589 = CIRCLE ( 'NONE', #4434, 1.122047244094488194 ) ;
#16590 = CARTESIAN_POINT ( 'NONE',  ( -0.6233595800524928121, -0.05778040916215522460, 0.4822834645669289988 ) ) ;
#16591 = CARTESIAN_POINT ( 'NONE',  ( 0.6496062992125991586, 0.1660481256975885056, 0.3530559997133364547 ) ) ;
#16592 = CARTESIAN_POINT ( 'NONE',  ( 1.351706036745407458, -0.4281496062992127816, -0.4176697321401328100 ) ) ;
#16593 = CARTESIAN_POINT ( 'NONE',  ( -1.109377953303970266, 1.093753137590900648, 0.1687621725689344154 ) ) ;
#16594 = CARTESIAN_POINT ( 'NONE',  ( 1.351706036745407680, -0.004921259842519576551, 0.3153832671262227771 ) ) ;
#16595 = CARTESIAN_POINT ( 'NONE',  ( -0.1998031496062991630, -0.3460692066303959202, -2.032152230971128848 ) ) ;
#16596 = CARTESIAN_POINT ( 'NONE',  ( -1.272965879265091305, -0.004921259842519870586, -0.3153832671262229437 ) ) ;
#16597 = CARTESIAN_POINT ( 'NONE',  ( 0.3392501089628018884, -0.1958661417322834220, 0.06036745406824151755 ) ) ;
#16598 = CARTESIAN_POINT ( 'NONE',  ( -0.01968503937007793844, 0.1660481256975883668, -0.3530559997133364547 ) ) ;
#16600 = LINE ( 'NONE', #67523, #2260 ) ;
#16599 = CARTESIAN_POINT ( 'NONE',  ( -3.937007874015748143, 2.559055118110236560, -0.5314960629921260393 ) ) ;
#16601 = CARTESIAN_POINT ( 'NONE',  ( -1.345144356955379816, -0.08942795157528024563, -0.3641732283464568787 ) ) ;
#16602 =( BOUNDED_CURVE ( )  B_SPLINE_CURVE ( 2, ( #79476, #77807, #27695, #79069, #20138, #71485, #13832, #7935, #20970, #65178, #33596, #27274, #66008 ),
 .UNSPECIFIED., .F., .F. ) 
 B_SPLINE_CURVE_WITH_KNOTS ( ( 3, 2, 2, 2, 2, 2, 3 ),
 ( 0.2763059932978689792, 0.2765151515151514916, 0.2803030303030303871, 0.2840909090909091717, 0.2878787878787879562, 0.2916666666666667407, 0.2918758248839492531 ),
 .UNSPECIFIED. ) 
 CURVE ( )  GEOMETRIC_REPRESENTATION_ITEM ( )  RATIONAL_B_SPLINE_CURVE ( ( 0.9964447847208419695, 0.9981185001348091834, 1.000000000000000000, 0.9659258262890683122, 1.000000000000000000, 0.9659258262890683122, 1.000000000000000000, 0.9659258262890683122, 1.000000000000000000, 0.9659258262890683122, 1.000000000000000000, 0.9981185001348091834, 0.9964447847208420805 ) ) 
 REPRESENTATION_ITEM ( '' )  );
#16603 = CARTESIAN_POINT ( 'NONE',  ( 0.1902887139107617975, -0.6692913385826773087, -0.1292274648535924053 ) ) ;
#16604 = CARTESIAN_POINT ( 'NONE',  ( 1.141732283464567566, 0.1771653543307087630, 0.000000000000000000 ) ) ;
#16605 = CARTESIAN_POINT ( 'NONE',  ( 0.3392501089628018329, 0.1958661417322835052, -1.786069923063305032 ) ) ;
#16606 = AXIS2_PLACEMENT_3D ( 'NONE', #31507, #24774, #76555 ) ;
#16607 = CARTESIAN_POINT ( 'NONE',  ( -1.220472440944881054, 0.1771653543307087630, 0.000000000000000000 ) ) ;
#16608 = CARTESIAN_POINT ( 'NONE',  ( 1.246719160104987623, 0.05413385826771626580, -0.4176697321401330321 ) ) ;
#16609 = CARTESIAN_POINT ( 'NONE',  ( 0.2009426810023753340, 1.919101783098011715, 0.2404105009256824188 ) ) ;
#16610 = CARTESIAN_POINT ( 'NONE',  ( -0.03937007874015669567, -0.6692913385826771977, 8.415575281601705876E-17 ) ) ;
#16611 = CARTESIAN_POINT ( 'NONE',  ( -1.443569553805773564, 0.1283753931104746893, -0.1820866141732285504 ) ) ;
#16612 = EDGE_CURVE ( 'NONE', #79410, #37352, #40814, .T. ) ;
#16613 = CARTESIAN_POINT ( 'NONE',  ( -0.7677165354330699465, 0.1660481256975885056, 0.3530559997133364547 ) ) ;
#16614 = CARTESIAN_POINT ( 'NONE',  ( -1.384514435695537005, -0.5511811023622048555, -0.09757992244046775898 ) ) ;
#16615 = CARTESIAN_POINT ( 'NONE',  ( -0.3917322834645670104, -0.1049643490035307020, -0.5151111792988996019 ) ) ;
#16616 = CARTESIAN_POINT ( 'NONE',  ( 0.3608923884514443348, 0.2952755905511810774, -0.1292274648535930714 ) ) ;
#16617 = PLANE ( 'NONE',  #80323 ) ;
#16618 = CARTESIAN_POINT ( 'NONE',  ( 1.246719160104987623, -0.4281496062992124485, 0.4176697321401328655 ) ) ;
#16619 = CARTESIAN_POINT ( 'NONE',  ( -0.3458507752293909498, 0.3458507752293907833, -2.143700787401574548 ) ) ;
#16620 = CARTESIAN_POINT ( 'NONE',  ( -1.259842519685038686, -0.1870078740157479769, 0.4822834645669291653 ) ) ;
#16621 = CARTESIAN_POINT ( 'NONE',  ( -0.4527559055118102749, 0.07958543189024085140, 0.2665933059059887866 ) ) ;
#16622 = CARTESIAN_POINT ( 'NONE',  ( -0.5183727034120726440, 0.2066929133858267931, 0.1054918080437490802 ) ) ;
#16623 = CARTESIAN_POINT ( 'NONE',  ( 0.09186351706036827158, 0.05413385826771666132, 0.4176697321401328100 ) ) ;
#16624 = CARTESIAN_POINT ( 'NONE',  ( 0.2165354330708668673, -0.4536011799217367080, 0.2665933059059888421 ) ) ;
#16625 = CARTESIAN_POINT ( 'NONE',  ( -1.095800524934382292, -0.08942795157527998196, 0.3641732283464567121 ) ) ;
#16626 = CARTESIAN_POINT ( 'NONE',  ( -1.515748031496062076, 0.1660481256975883668, -0.3530559997133364547 ) ) ;
#16627 = CARTESIAN_POINT ( 'NONE',  ( 1.555118110236221041, -0.4536011799217367080, 0.2665933059059888421 ) ) ;
#16628 = CARTESIAN_POINT ( 'NONE',  ( 1.430446194225722500, -0.4281496062992127816, -0.4176697321401328100 ) ) ;
#16629 = CARTESIAN_POINT ( 'NONE',  ( -0.4091458600556405756, 0.2362204724409446288, -2.150262467191601079 ) ) ;
#16630 = CARTESIAN_POINT ( 'NONE',  ( 0.3280839895013130669, -0.3690944881889765550, -0.3153832671262227771 ) ) ;
#16631 = CARTESIAN_POINT ( 'NONE',  ( 0.8661417322834653598, -0.1870078740157479769, 0.4822834645669291653 ) ) ;
#16632 = DIRECTION ( 'NONE',  ( 0.000000000000000000, 0.000000000000000000, 1.000000000000000000 ) ) ;
#16633 = CARTESIAN_POINT ( 'NONE',  ( 1.023622047244095112, -0.1870078740157480601, -0.3641732283464567677 ) ) ;
#16634 = ORIENTED_EDGE ( 'NONE', *, *, #41785, .F. ) ;
#16635 = EDGE_CURVE ( 'NONE', #23493, #43326, #68968, .T. ) ;
#16636 = CARTESIAN_POINT ( 'NONE',  ( -1.272965879265091305, 0.05413385826771626580, -0.4176697321401330321 ) ) ;
#16637 = EDGE_CURVE ( 'NONE', #8180, #8792, #60187, .T. ) ;
#16638 = CARTESIAN_POINT ( 'NONE',  ( -0.8727034120734901146, -0.3162353388693405765, 0.4822834645669290543 ) ) ;
#16639 = CARTESIAN_POINT ( 'NONE',  ( 0.2493438320209980519, -0.4281496062992127816, -0.4176697321401328100 ) ) ;
#16640 = DIRECTION ( 'NONE',  ( 0.000000000000000000, 0.000000000000000000, -1.000000000000000000 ) ) ;
#16641 = CARTESIAN_POINT ( 'NONE',  ( 0.3460692066303958092, 0.1998031496062993018, -2.255249343832021136 ) ) ;
#16642 = CARTESIAN_POINT ( 'NONE',  ( 0.8005249343832027131, 0.05413385826771666132, 0.4176697321401328100 ) ) ;
#16643 = CARTESIAN_POINT ( 'NONE',  ( 1.502624671916010790, -0.2845877964562161244, -0.3641732283464567121 ) ) ;
#16644 = CARTESIAN_POINT ( 'NONE',  ( 0.02624671916010564918, -0.6046776061558809534, -0.2411417322834644161 ) ) ;
#16645 = CARTESIAN_POINT ( 'NONE',  ( 0.8661417322834652488, -0.1870078740157480879, -0.4822834645669291653 ) ) ;
#16646 = CARTESIAN_POINT ( 'NONE',  ( 0.1070741851644053527, 0.3996062992125986590, -1.883202099737532276 ) ) ;
#16647 = CARTESIAN_POINT ( 'NONE',  ( 0.1058382717557500713, -0.3949938075777409408, -1.030183727034120755 ) ) ;
#16648 = CARTESIAN_POINT ( 'NONE',  ( -0.1998031496062991907, -0.3460692066303959757, -2.427821522309711266 ) ) ;
#16649 = DIRECTION ( 'NONE',  ( 0.000000000000000000, -0.6427876096865352551, -0.7660444431189814551 ) ) ;
#16650 = CIRCLE ( 'NONE', #58244, 0.1978346456692914035 ) ;
#16651 = CARTESIAN_POINT ( 'NONE',  ( -0.1601112597053892528, 0.3598931997258726923, -0.002668403679490424611 ) ) ;
#16652 = CARTESIAN_POINT ( 'NONE',  ( -0.2165354330708654795, -0.4536011799217368745, -0.2665933059059886201 ) ) ;
#16653 = CARTESIAN_POINT ( 'NONE',  ( -0.5380577427821514602, -0.4281496062992127816, -0.4176697321401328100 ) ) ;
#16654 = CARTESIAN_POINT ( 'NONE',  ( 1.003937007874016185, 0.1660481256975883668, -0.3530559997133364547 ) ) ;
#16655 = CARTESIAN_POINT ( 'NONE',  ( -0.1974969037888704149, -0.3420746716998661063, -2.189632545931758489 ) ) ;
#16656 = CARTESIAN_POINT ( 'NONE',  ( 0.06561679790026316017, -0.3690944881889763329, 0.3153832671262228327 ) ) ;
#16657 = CARTESIAN_POINT ( 'NONE',  ( -1.272965879265091305, 0.05413385826771626580, -0.4176697321401330321 ) ) ;
#16658 = CARTESIAN_POINT ( 'NONE',  ( 1.253280839895013710, -0.3162353388693405765, 0.4822834645669290543 ) ) ;
#16659 = CARTESIAN_POINT ( 'NONE',  ( 0.4091458600556404646, -0.2362204724409448231, -2.309711286089239035 ) ) ;
#16660 = CARTESIAN_POINT ( 'NONE',  ( -0.3460692066303958092, -0.1998031496062994683, -1.627296587926509330 ) ) ;
#16661 = LINE ( 'NONE', #35176, #46591 ) ;
#16662 = VERTEX_POINT ( 'NONE', #29422 ) ;
#16663 = CARTESIAN_POINT ( 'NONE',  ( 1.213910761154856299, -0.6692913385826773087, -0.1292274648535924053 ) ) ;
#16664 = AXIS2_PLACEMENT_3D ( 'NONE', #50570, #17793, #25315 ) ;
#16665 = CARTESIAN_POINT ( 'NONE',  ( 1.233595800524935227, -0.5023911411419708095, 0.1820866141732285504 ) ) ;
#16667 = CARTESIAN_POINT ( 'NONE',  ( 1.476377952755906220, 0.1660481256975883668, -0.3530559997133364547 ) ) ;
#16666 = CARTESIAN_POINT ( 'NONE',  ( -1.633858267716534529, 0.07958543189024085140, 0.2665933059059887866 ) ) ;
#16668 = CARTESIAN_POINT ( 'NONE',  ( 0.3917322834645670104, 2.398668435337828261E-17, 0.1122047244094487306 ) ) ;
#16669 = CARTESIAN_POINT ( 'NONE',  ( -0.9573014326657163231, -2.609869883881465018E-15, -0.3464511005275220379 ) ) ;
#16670 = CARTESIAN_POINT ( 'NONE',  ( 1.174540682414699111, -0.3162353388693405765, 0.4822834645669290543 ) ) ;
#16671 = CARTESIAN_POINT ( 'NONE',  ( -1.535433070866141225, 0.2952755905511811885, 0.000000000000000000 ) ) ;
#16672 = CARTESIAN_POINT ( 'NONE',  ( -0.6430446194225716283, -0.4281496062992124485, 0.4176697321401328655 ) ) ;
#16673 = CARTESIAN_POINT ( 'NONE',  ( -0.7611548556430438595, 0.2306618581243848609, 0.2411417322834645549 ) ) ;
#16674 = CARTESIAN_POINT ( 'NONE',  ( 1.489501312335958172, -0.05778040916215560624, -0.4822834645669293319 ) ) ;
#16675 = CARTESIAN_POINT ( 'NONE',  ( -0.3917322834645671215, 0.1049643490035301469, -0.2749343832020998413 ) ) ;
#16676 = CARTESIAN_POINT ( 'NONE',  ( 0.04593175853018440641, 0.2952755905511810774, -0.1292274648535930714 ) ) ;
#16677 = CARTESIAN_POINT ( 'NONE',  ( 0.3917322834645670104, 2.398668435337828261E-17, -2.314960629921259727 ) ) ;
#16678 = CARTESIAN_POINT ( 'NONE',  ( -1.594488188976377119, 0.07958543189024071263, -0.2665933059059888421 ) ) ;
#16679 = ORIENTED_EDGE ( 'NONE', *, *, #2416, .T. ) ;
#16680 = CARTESIAN_POINT ( 'NONE',  ( -0.1974969037888703871, -0.3420746716998661063, -2.742782152230970993 ) ) ;
#16681 = ORIENTED_EDGE ( 'NONE', *, *, #63509, .F. ) ;
#16682 = CARTESIAN_POINT ( 'NONE',  ( 0.3937007874015751585, 1.535433070866141447, 0.000000000000000000 ) ) ;
#16683 = CARTESIAN_POINT ( 'NONE',  ( -1.614173228346456268, -0.6692913385826771977, 8.415575281601705876E-17 ) ) ;
#16684 = CARTESIAN_POINT ( 'NONE',  ( 0.1070741851644053527, 0.3996062992125986590, -0.9383202099737533164 ) ) ;
#16685 = CARTESIAN_POINT ( 'NONE',  ( 1.660104986876641320, -0.08942795157527998196, 0.3641732283464567121 ) ) ;
#16686 = CARTESIAN_POINT ( 'NONE',  ( -0.5314960629921323676, 2.742788276420188520, 1.827151573187007161 ) ) ;
#16687 = CARTESIAN_POINT ( 'NONE',  ( -3.908320185825792326, 1.537401574803149984, -0.4744094488188975722 ) ) ;
#16688 = DIRECTION ( 'NONE',  ( -3.096699300667737957E-16, 1.000000000000000000, -0.000000000000000000 ) ) ;
#16689 = CARTESIAN_POINT ( 'NONE',  ( 0.2867679344610365999, -0.2867679344610365444, -0.02559055118110245899 ) ) ;
#16690 = CARTESIAN_POINT ( 'NONE',  ( -0.5118110236220466680, 0.1771653543307087630, 0.000000000000000000 ) ) ;
#16691 = CARTESIAN_POINT ( 'NONE',  ( -1.095800524934382292, -0.08942795157527998196, 0.3641732283464567121 ) ) ;
#16692 = CARTESIAN_POINT ( 'NONE',  ( 1.476377952755906220, 0.1660481256975883668, -0.3530559997133364547 ) ) ;
#16693 = CARTESIAN_POINT ( 'NONE',  ( 0.3412073490813655186, 0.2306618581243848609, 0.2411417322834645549 ) ) ;
#16694 = CARTESIAN_POINT ( 'NONE',  ( -1.253280839895012377, -0.3162353388693409650, -0.4822834645669289433 ) ) ;
#16695 = CARTESIAN_POINT ( 'NONE',  ( -0.3917322834645671215, 0.1049643490035301469, -0.1824146981627296216 ) ) ;
#16696 = EDGE_LOOP ( 'NONE', ( #13116, #29716, #38808, #56286 ) ) ;
#16697 = CARTESIAN_POINT ( 'NONE',  ( -1.312335958005248715, 0.2306618581243848609, 0.2411417322834645549 ) ) ;
#16698 = DIRECTION ( 'NONE',  ( 1.000000000000000000, 0.000000000000000000, -0.000000000000000000 ) ) ;
#16699 = CARTESIAN_POINT ( 'NONE',  ( 0.1265901696524989462, 0.4724409448818897572, -1.725721784776903078 ) ) ;
#16700 = EDGE_CURVE ( 'NONE', #7865, #25718, #68832, .T. ) ;
#16701 = CARTESIAN_POINT ( 'NONE',  ( 0.1972978822260920695, 0.2198823481317033202, 0.1376690760605704111 ) ) ;
#16702 = DIRECTION ( 'NONE',  ( 1.000000000000000000, -0.000000000000000000, -0.000000000000000000 ) ) ;
#16703 = CARTESIAN_POINT ( 'NONE',  ( -0.6561679790026240244, 0.2306618581243847221, -0.2411417322834647770 ) ) ;
#16704 = CARTESIAN_POINT ( 'NONE',  ( 1.404199475065617708, 0.05413385826771626580, -0.4176697321401330321 ) ) ;
#16706 = FACE_OUTER_BOUND ( 'NONE', #35608, .T. ) ;
#16705 = CARTESIAN_POINT ( 'NONE',  ( -1.640419947506561060, -0.4281496062992127816, -0.4176697321401328100 ) ) ;
#16707 = CARTESIAN_POINT ( 'NONE',  ( 1.633858267716535639, -0.5400638737290844871, 0.3530559997133364547 ) ) ;
#16708 = CARTESIAN_POINT ( 'NONE',  ( -0.6299212598425188991, -0.1870078740157479769, 0.4822834645669291653 ) ) ;
#16709 = CARTESIAN_POINT ( 'NONE',  ( -0.1958661417322836440, 0.3392501089628016664, 0.06432377772409630934 ) ) ;
#16710 = CARTESIAN_POINT ( 'NONE',  ( -0.1181102362204717315, 0.1771653543307087630, 0.000000000000000000 ) ) ;
#16711 = CARTESIAN_POINT ( 'NONE',  ( -0.3917322834645671215, 0.1049643490035301469, -0.4324146981627297603 ) ) ;
#16712 = VECTOR ( 'NONE', #41094, 39.37007874015748854 ) ;
#16713 = CARTESIAN_POINT ( 'NONE',  ( -0.2952755905511803003, -0.4536011799217368745, -0.2665933059059886201 ) ) ;
#16714 = CARTESIAN_POINT ( 'NONE',  ( 0.8792650918635177559, -0.3690944881889765550, -0.3153832671262227771 ) ) ;
#16715 = CARTESIAN_POINT ( 'NONE',  ( 0.5314960629921264834, 0.1660481256975883668, -0.3530559997133364547 ) ) ;
#16716 = CARTESIAN_POINT ( 'NONE',  ( -0.09186351706036663400, -0.3690944881889763329, 0.3153832671262228327 ) ) ;
#16717 = CARTESIAN_POINT ( 'NONE',  ( 0.2867679344610365999, 0.2867679344610365999, -2.492125984251968518 ) ) ;
#16718 = CARTESIAN_POINT ( 'NONE',  ( 1.607611548556431069, 0.2952755905511811885, 0.1292274648535926551 ) ) ;
#16719 = CARTESIAN_POINT ( 'NONE',  ( -0.9908136482939626788, 0.2952755905511811885, 0.1292274648535926551 ) ) ;
#16720 = CARTESIAN_POINT ( 'NONE',  ( -0.1265901696524986964, -0.4724409448818899238, -0.7788713910761155823 ) ) ;
#16721 = CARTESIAN_POINT ( 'NONE',  ( 0.09186351706036799403, -0.4281496062992127816, -0.4176697321401328100 ) ) ;
#16722 = CARTESIAN_POINT ( 'NONE',  ( -0.6496062992125976043, 0.1660481256975883668, -0.3530559997133364547 ) ) ;
#16723 = CARTESIAN_POINT ( 'NONE',  ( -0.3307086614173228023, -0.3647102339900947787, 0.000000000000000000 ) ) ;
#16724 = AXIS2_PLACEMENT_3D ( 'NONE', #3739, #56309, #67721 ) ;
#16725 = CARTESIAN_POINT ( 'NONE',  ( 0.1443569553805781891, -0.3690944881889763329, 0.3153832671262228327 ) ) ;
#16726 = CARTESIAN_POINT ( 'NONE',  ( -0.2230971128608915943, -0.4281496062992127816, -0.4176697321401328100 ) ) ;
#16727 = CARTESIAN_POINT ( 'NONE',  ( -0.7480314960629914633, -0.6692913385826771977, 8.415575281601705876E-17 ) ) ;
#16728 = CARTESIAN_POINT ( 'NONE',  ( -1.646051170424378096, 0.4405861044731112508, -0.3149606299212598381 ) ) ;
#16729 = CARTESIAN_POINT ( 'NONE',  ( 1.614173228346457378, -0.5511811023622047445, 6.969142054262312111E-17 ) ) ;
#16730 = CARTESIAN_POINT ( 'NONE',  ( 0.2821522309711292364, 0.2952755905511810774, -0.1292274648535930714 ) ) ;
#16731 = ORIENTED_EDGE ( 'NONE', *, *, #24704, .F. ) ;
#16732 = CARTESIAN_POINT ( 'NONE',  ( -0.3460692066303960313, 0.1998031496062989965, -2.150262467191601079 ) ) ;
#16733 =( BOUNDED_SURFACE ( )  B_SPLINE_SURFACE ( 1, 2, ( 
 ( #65346, #46372, #19457, #32498, #64491, #7251, #20300, #1369, #63657, #45949, #51845, #12737, #530, #71231, #70813, #58162, #39655, #27021, #13998, #32923, #58589, #25345, #13575, #25760, #52264, #39229, #957, #77970, #20721, #37982, #52682, #5996, #31667, #51422, #51007, #57328, #70382, #76706, #38396, #64076, #6413, #32083, #57744, #106, #77124, #45108, #72895, #53521, #53932, #3436, #48038, #48446, #59422, #33760, #34599, #59840, #3021, #35008, #72483, #2193, #34176, #47620, #79228, #15245, #15663, #60264, #8922, #73316, #8096, #67005, #41324, #2613, #40905, #53098, #66586, #54349, #1778, #16075, #79644, #8510, #27436, #78808, #29098, #28688, #60673, #28270, #14425, #9337, #21961, #21137, #80060, #46792, #22378, #14832, #21544, #73740, #41721, #67414, #9748, #40492, #66170, #35420, #27861, #61085, #54770, #47205, #80474, #22786, #40076, #65763, #80880, #16909, #36241, #37060, #61911, #81289, #18132, #82515, #55579, #42950, #74977, #17726, #56412, #69470, #16491, #82111, #4656, #48863, #36643, #30329, #23605, #49274, #75790, #11823, #50094, #43352, #69054, #35836, #17322, #4253, #62744, #10983, #11403, #62319, #31150, #74146, #37475, #63148, #56816, #29915, #61503, #81707, #55171, #24424, #24017, #74563, #5080, #5489, #30749, #24831, #49685, #75377, #68644, #55995, #43765, #42137, #67832, #10171, #3850, #29510, #23192, #42547, #68250, #10584, #25247, #12637, #70284, #427, #6309, #25661, #51743, #70708, #45008, #26083, #44184, #19779, #77446, #13060, #51323, #5895, #77026, #7148, #69876, #52164, #32398, #44590, #12229, #37886, #39553, #64809, #13471, #19359, #1273, #45433, #38714, #31567, #64392, #63561, #71128, #57225, #58061, #18942, #65242, #39128, #6728, #26510, #32821, #58488, #50911, #853, #7580, #77868, #20197, #45848, #71547, #13894, #76612, #33252, #58914, #82926, #57646, #50500, #76203, #18541, #38296, #63973, #31986, #9, #46694, #60162, #41223, #7997, #9241, #72794, #73213, #53830, #33661, #52997, #72387, #15563, #14737, #34075, #54247, #35322, #8408, #79131, #27758, #79544, #34913, #22277, #52581, #60576, #40800, #1680, #15144, #66485, #59739, #2093, #28591, #47937, #2927, #21857, #47521, #71968, #53422, #40389, #66910, #47105, #79964, #8820, #67318, #26921, #73640, #15982, #9653, #66072, #14323, #34497, #59324, #41629, #2514, #27337, #60985, #78290, #20621, #46273, #28173, #39981, #21448, #65671, #78710, #21034, #38091, #38509, #48348, #22689, #24638, #49897, #76413, #25041, #62538, #75596, #24226, #37681, #43571, #62955, #5691, #50305, #82318, #63357, #80376, #57027, #31361, #76003, #5291, #42039, #30952, #44386, #74045, #6106, #69682, #81914, #16392, #67733, #76815, #18743, #50714, #56619, #3335, #82721, #18345, #10068, #43985, #35731, #70079, #4876, #12025, #56215, #19147, #30549, #12432, #17935, #63765, #54665, #11618, #31779, #69272, #57441, #37279, #44797, #83134, #70493, #25453, #51120, #12850, #28999, #39336, #8198, #27545, #71336, #14528, #20408, #65023, #45223, #59528, #1885, #7358, #78077, #51532, #13683, #64191, #33027, #58696, #1061, #20823, #14933, #53202, #26714, #1473, #6526, #52369, #219, #46059, #6938, #78915, #70924, #71753, #40180, #32610, #33454, #14107, #39759, #27127, #65864, #13270, #65455, #21236, #64603, #7787, #33864, #32195, #59115, #52791, #78500, #38922, #57852, #45641, #46476, #637, #58272, #72172, #46892, #72586, #25870, #77235, #19564, #26292, #51953, #77658, #19990, #48557, #41012, #22889, #15773, #27961, #55279, #54035, #80582, #67936, #41829, #79328, #74672, #74254, #54455, #47725, #22483, #10277, #80167, #67519, #28792, #2713, #66696, #16596, #48145, #35526, #9031, #66274, #47308, #28374, #42241, #35944, #3956, #2301, #79748, #41424, #73842, #16182, #53620, #9856, #60366, #72998, #21648, #61188, #61614, #29618, #34283, #3543, #29210, #15350, #67108, #22065, #54876, #60776, #80989, #3127, #23302, #40592, #48972, #8613, #59945, #73423, #34704, #9439, #35110, #82626, #24540, #75081, #63256, #37994, #43883, #57341, #50205, #18242, #75496, #56109, #56518, #6011, #50611, #51023, #62023, #36348 ),
 ( #63670, #24125, #76318, #82221, #17835, #81399, #12338, #31681, #43469, #30854, #4360, #49794, #17016, #69166, #11517, #37173, #56930, #42656, #83036, #62853, #37583, #68353, #5189, #30028, #75902, #43059, #25360, #23715, #69581, #18648, #68756, #11928, #5597, #31263, #24940, #44292, #49386, #69983, #10693, #17428, #55691, #11098, #36756, #62431, #4769, #30444, #81814, #76722, #58177, #59029, #13179, #121, #71663, #72081, #33366, #26627, #58604, #27037, #52698, #14440, #45549, #20737, #1384, #77140, #78406, #51860, #64093, #8111, #6845, #46388, #40092, #77986, #32098, #27453, #65779, #7267, #546, #973, #33777, #77567, #57759, #59440, #1793, #19901, #32939, #6429, #26199, #19054, #71246, #13590, #39246, #44701, #70398, #12754, #64929, #14014, #38411, #52281, #25776, #20315, #19473, #51437, #45123, #45966, #70831, #38828, #39671, #65361, #7699, #64506, #32515, #34192, #73333, #16510, #53536, #2629, #22804, #53114, #28285, #3038, #53947, #27876, #78823, #34614, #35435, #72910, #59856, #48054, #48462, #9764, #28703, #35024, #3451, #29115, #74162, #21976, #80489, #61100, #79244, #54786, #79660, #40507, #67848, #66603, #42153, #10187, #54365, #8525, #3867, #35852, #67020, #60279, #60688, #61521, #9353, #80077, #41340, #15262, #21559, #21152, #22395, #73755, #47221, #46807, #2208, #40922, #72498, #14847, #66189, #8936, #47638, #15679, #16091, #41736, #67430, #17742, #49290, #36259, #10602, #43370, #5502, #82529, #23209, #69070, #48880, #11420, #81307, #37489, #80896, #36660, #37075, #74580, #24846, #61928, #69888, #55595, #18553, #50513, #16925, #74993, #12242, #4672, #56831, #76218, #62335, #63164, #62761, #5096, #75396, #30345, #68266, #56011, #69484, #42562, #31164, #30764, #23621, #4270, #29932, #44198, #43781, #75805, #81722, #63574, #56426, #24031, #17338, #82126, #42968, #24441, #68663, #50109, #11001, #37898, #18147, #11836, #29526, #49700, #55188, #12650, #45021, #13909, #44602, #77039, #58502, #866, #45446, #13484, #57237, #6323, #45862, #31999, #51756, #7163, #18955, #26523, #6741, #39141, #19795, #70297, #63986, #57659, #64823, #21, #19371, #52178, #7593, #51335, #13074, #70721, #71142, #32834, #20212, #31582, #77881, #58075, #38311, #32412, #441, #38728, #64405, #71560, #39567, #65256, #33265, #5909, #25675, #26096, #77459, #82939, #25260, #50924, #76624, #38159, #81152, #44454, #70145, #63833, #11268, #68510, #5354, #62187, #63421, #31013, #55856, #44052, #18808, #24700, #6170, #56682, #82383, #56278, #36927, #37344, #12497, #31428, #31845, #42816, #17183, #17999, #43220, #69744, #18409, #81566, #68918, #17588, #50369, #62604, #81975, #76067, #43633, #75658, #12090, #74839, #37746, #4945, #30615, #25107, #23468, #24289, #49961, #69336, #5758, #57090, #76481, #49135, #82786, #11686, #23884, #63017, #50780, #10850, #36511, #4524, #30194, #49549, #75244, #83034, #5187, #62429, #43057, #50609, #82219, #11926, #17426, #42655, #23713, #4767, #82623, #24938, #63668, #62022, #30442, #75494, #24538, #56516, #30026, #30852, #36754, #49384, #81397, #50203, #76316, #69981, #10692, #75900, #36347, #18240, #68754, #18646, #68352, #24123, #43881, #4358, #12336, #75079, #57338, #11096, #6009, #37992, #55689, #56107, #25358, #17833, #44290, #31678, #49792, #51021, #69579, #43467, #81812, #17015, #69164, #11515, #37581, #37171, #62851, #63254, #5595, #31261, #56928, #33364, #27451, #72079, #71244, #14012, #76720, #26197, #12752, #64927, #19471, #14438, #57757, #7265, #27034, #45121, #45964, #13588, #26625, #39669, #52696, #119, #39244, #40090, #77138, #51858, #46386, #19052, #77565, #52279, #19899, #51435, #44699, #58175, #59027, #13176, #25774, #71661, #65777, #1382, #77983, #58602, #78403, #70829, #65359, #32937, #20313, #7697, #20735, #38826, #971, #8109, #64504, #45546, #33775, #70396, #59437, #1791, #38409, #6843, #64090, #544, #6427, #32513, #32096, #48052, #48460, #9762, #3036, #35022, #3449, #29113, #74160, #21974, #80487, #61098, #53534, #35433, #28283, #40505, #67846, #66601, #54783, #22802, #54363, #8522, #3864, #16508, #67018, #60277, #41338 ) ),
 .UNSPECIFIED., .F., .F., .F. ) 
 B_SPLINE_SURFACE_WITH_KNOTS ( ( 2, 2 ),
 ( 3, 2, 2, 2, 2, 2, 2, 2, 2, 2, 2, 2, 2, 2, 2, 2, 2, 2, 2, 2, 2, 2, 2, 2, 2, 2, 2, 2, 2, 2, 2, 2, 2, 2, 2, 2, 2, 2, 2, 2, 2, 2, 2, 2, 2, 2, 2, 2, 2, 2, 2, 2, 2, 2, 2, 2, 2, 2, 2, 2, 2, 2, 2, 2, 2, 2, 2, 2, 2, 2, 2, 2, 2, 2, 2, 2, 2, 2, 2, 2, 2, 2, 2, 2, 2, 2, 2, 2, 2, 2, 2, 2, 2, 2, 2, 2, 2, 2, 2, 2, 2, 2, 2, 2, 2, 2, 2, 2, 2, 2, 2, 2, 2, 2, 2, 2, 2, 2, 2, 2, 2, 2, 2, 2, 2, 2, 2, 2, 2, 2, 2, 2, 2, 2, 2, 2, 2, 2, 2, 2, 2, 2, 2, 2, 2, 2, 2, 2, 2, 2, 2, 2, 2, 2, 2, 2, 2, 2, 2, 2, 2, 2, 2, 2, 2, 2, 2, 2, 2, 2, 2, 2, 2, 2, 2, 2, 2, 2, 2, 2, 2, 2, 2, 2, 2, 2, 2, 2, 2, 2, 2, 2, 2, 2, 2, 2, 2, 2, 2, 2, 2, 2, 2, 2, 2, 2, 2, 2, 2, 2, 2, 2, 2, 2, 2, 2, 2, 2, 2, 2, 2, 2, 2, 2, 2, 2, 2, 2, 2, 2, 2, 2, 2, 2, 2, 2, 2, 2, 2, 2, 2, 2, 2, 2, 2, 2, 2, 2, 2, 2, 2, 2, 2, 2, 2, 3 ),
 ( 0.000000000000000000, 1.000000000000000000 ),
 ( 0.000000000000000000, 0.003787878787878787984, 0.007575757575757575968, 0.01136363636363636395, 0.01515151515151515194, 0.01893939393939393992, 0.02272727272727272790, 0.02651515151515151589, 0.03030303030303030387, 0.03409090909090908839, 0.03787878787878787984, 0.04166666666666666435, 0.04545454545454545581, 0.04924242424242424032, 0.05303030303030303177, 0.05681818181818181629, 0.06060606060606060774, 0.06439393939393939226, 0.06818181818181817677, 0.07196969696969697516, 0.07575757575757575968, 0.07954545454545454419, 0.08333333333333332871, 0.08712121212121212710, 0.09090909090909091161, 0.09469696969696969613, 0.09848484848484848064, 0.1022727272727272790, 0.1060606060606060635, 0.1098484848484848481, 0.1136363636363636326, 0.1174242424242424310, 0.1212121212121212155, 0.1250000000000000000, 0.1287878787878787845, 0.1325757575757575690, 0.1363636363636363535, 0.1401515151515151381, 0.1439393939393939503, 0.1477272727272727348, 0.1515151515151515194, 0.1553030303030303039, 0.1590909090909090884, 0.1628787878787878729, 0.1666666666666666574, 0.1704545454545454419, 0.1742424242424242542, 0.1780303030303030387, 0.1818181818181818232, 0.1856060606060606077, 0.1893939393939393923, 0.1931818181818181768, 0.1969696969696969613, 0.2007575757575757458, 0.2045454545454545581, 0.2083333333333333426, 0.2121212121212121271, 0.2159090909090909116, 0.2196969696969696961, 0.2234848484848484806, 0.2272727272727272652, 0.2310606060606060497, 0.2348484848484848619, 0.2386363636363636465, 0.2424242424242424310, 0.2462121212121212155, 0.2500000000000000000, 0.2537878787878787845, 0.2575757575757575690, 0.2613636363636363535, 0.2651515151515151381, 0.2689393939393939226, 0.2727272727272727071, 0.2765151515151514916, 0.2803030303030302761, 0.2840909090909091161, 0.2878787878787879007, 0.2916666666666666852, 0.2954545454545454697, 0.2992424242424242542, 0.3030303030303030387, 0.3068181818181818232, 0.3106060606060606077, 0.3143939393939393923, 0.3181818181818181768, 0.3219696969696969613, 0.3257575757575757458, 0.3295454545454545303, 0.3333333333333333148, 0.3371212121212120993, 0.3409090909090908839, 0.3446969696969697239, 0.3484848484848485084, 0.3522727272727272929, 0.3560606060606060774, 0.3598484848484848619, 0.3636363636363636465, 0.3674242424242424310, 0.3712121212121212155, 0.3750000000000000000, 0.3787878787878787845, 0.3825757575757575690, 0.3863636363636363535, 0.3901515151515151381, 0.3939393939393939226, 0.3977272727272727071, 0.4015151515151514916, 0.4053030303030302761, 0.4090909090909091161, 0.4128787878787879007, 0.4166666666666666852, 0.4204545454545454697, 0.4242424242424242542, 0.4280303030303030387, 0.4318181818181818232, 0.4356060606060606077, 0.4393939393939393923, 0.4431818181818181768, 0.4469696969696969613, 0.4507575757575757458, 0.4545454545454545303, 0.4583333333333333148, 0.4621212121212120993, 0.4659090909090908839, 0.4696969696969697239, 0.4734848484848485084, 0.4772727272727272929, 0.4810606060606060774, 0.4848484848484848619, 0.4886363636363636465, 0.4924242424242424310, 0.4962121212121212155, 0.5000000000000000000, 0.5037878787878787845, 0.5075757575757575690, 0.5113636363636363535, 0.5151515151515151381, 0.5189393939393939226, 0.5227272727272727071, 0.5265151515151514916, 0.5303030303030302761, 0.5340909090909090606, 0.5378787878787878451, 0.5416666666666666297, 0.5454545454545454142, 0.5492424242424241987, 0.5530303030303029832, 0.5568181818181817677, 0.5606060606060605522, 0.5643939393939394478, 0.5681818181818182323, 0.5719696969696970168, 0.5757575757575758013, 0.5795454545454545858, 0.5833333333333333703, 0.5871212121212121549, 0.5909090909090909394, 0.5946969696969697239, 0.5984848484848485084, 0.6022727272727272929, 0.6060606060606060774, 0.6098484848484848619, 0.6136363636363636465, 0.6174242424242424310, 0.6212121212121212155, 0.6250000000000000000, 0.6287878787878787845, 0.6325757575757575690, 0.6363636363636363535, 0.6401515151515151381, 0.6439393939393939226, 0.6477272727272727071, 0.6515151515151514916, 0.6553030303030302761, 0.6590909090909090606, 0.6628787878787878451, 0.6666666666666666297, 0.6704545454545454142, 0.6742424242424241987, 0.6780303030303029832, 0.6818181818181817677, 0.6856060606060605522, 0.6893939393939394478, 0.6931818181818182323, 0.6969696969696970168, 0.7007575757575758013, 0.7045454545454545858, 0.7083333333333333703, 0.7121212121212121549, 0.7159090909090909394, 0.7196969696969697239, 0.7234848484848485084, 0.7272727272727272929, 0.7310606060606060774, 0.7348484848484848619, 0.7386363636363636465, 0.7424242424242424310, 0.7462121212121212155, 0.7500000000000000000, 0.7537878787878787845, 0.7575757575757575690, 0.7613636363636363535, 0.7651515151515151381, 0.7689393939393939226, 0.7727272727272727071, 0.7765151515151514916, 0.7803030303030302761, 0.7840909090909090606, 0.7878787878787878451, 0.7916666666666666297, 0.7954545454545454142, 0.7992424242424241987, 0.8030303030303029832, 0.8068181818181817677, 0.8106060606060605522, 0.8143939393939394478, 0.8181818181818182323, 0.8219696969696970168, 0.8257575757575758013, 0.8295454545454545858, 0.8333333333333333703, 0.8371212121212121549, 0.8409090909090909394, 0.8446969696969697239, 0.8484848484848485084, 0.8522727272727272929, 0.8560606060606060774, 0.8598484848484848619, 0.8636363636363636465, 0.8674242424242424310, 0.8712121212121212155, 0.8750000000000000000, 0.8787878787878787845, 0.8825757575757575690, 0.8863636363636363535, 0.8901515151515151381, 0.8939393939393939226, 0.8977272727272727071, 0.9015151515151514916, 0.9053030303030302761, 0.9090909090909090606, 0.9128787878787878451, 0.9166666666666666297, 0.9204545454545454142, 0.9242424242424241987, 0.9280303030303029832, 0.9318181818181817677, 0.9356060606060605522, 0.9393939393939394478, 0.9431818181818182323, 0.9469696969696970168, 0.9507575757575758013, 0.9545454545454545858, 0.9583333333333333703, 0.9621212121212121549, 0.9659090909090909394 ),
 .UNSPECIFIED. ) 
 GEOMETRIC_REPRESENTATION_ITEM ( )  RATIONAL_B_SPLINE_SURFACE ( (
 ( 1.000000000000000000, 0.9659258262890683122, 1.000000000000000000, 0.9659258262890683122, 1.000000000000000000, 0.9659258262890683122, 1.000000000000000000, 0.9659258262890683122, 1.000000000000000000, 0.9659258262890683122, 1.000000000000000000, 0.9659258262890683122, 1.000000000000000000, 0.9659258262890683122, 1.000000000000000000, 0.9659258262890683122, 1.000000000000000000, 0.9659258262890683122, 1.000000000000000000, 0.9659258262890683122, 1.000000000000000000, 0.9659258262890683122, 1.000000000000000000, 0.9659258262890683122, 1.000000000000000000, 0.9659258262890683122, 1.000000000000000000, 0.9659258262890683122, 1.000000000000000000, 0.9659258262890683122, 1.000000000000000000, 0.9659258262890683122, 1.000000000000000000, 0.9659258262890683122, 1.000000000000000000, 0.9659258262890683122, 1.000000000000000000, 0.9659258262890683122, 1.000000000000000000, 0.9659258262890683122, 1.000000000000000000, 0.9659258262890683122, 1.000000000000000000, 0.9659258262890683122, 1.000000000000000000, 0.9659258262890683122, 1.000000000000000000, 0.9659258262890683122, 1.000000000000000000, 0.9659258262890683122, 1.000000000000000000, 0.9659258262890683122, 1.000000000000000000, 0.9659258262890683122, 1.000000000000000000, 0.9659258262890683122, 1.000000000000000000, 0.9659258262890683122, 1.000000000000000000, 0.9659258262890683122, 1.000000000000000000, 0.9659258262890683122, 1.000000000000000000, 0.9659258262890683122, 1.000000000000000000, 0.9659258262890683122, 1.000000000000000000, 0.9659258262890683122, 1.000000000000000000, 0.9659258262890683122, 1.000000000000000000, 0.9659258262890683122, 1.000000000000000000, 0.9659258262890683122, 1.000000000000000000, 0.9659258262890683122, 1.000000000000000000, 0.9659258262890683122, 1.000000000000000000, 0.9659258262890683122, 1.000000000000000000, 0.9659258262890683122, 1.000000000000000000, 0.9659258262890683122, 1.000000000000000000, 0.9659258262890683122, 1.000000000000000000, 0.9659258262890683122, 1.000000000000000000, 0.9659258262890683122, 1.000000000000000000, 0.9659258262890683122, 1.000000000000000000, 0.9659258262890683122, 1.000000000000000000, 0.9659258262890683122, 1.000000000000000000, 0.9659258262890683122, 1.000000000000000000, 0.9659258262890683122, 1.000000000000000000, 0.9659258262890683122, 1.000000000000000000, 0.9659258262890683122, 1.000000000000000000, 0.9659258262890683122, 1.000000000000000000, 0.9659258262890683122, 1.000000000000000000, 0.9659258262890683122, 1.000000000000000000, 0.9659258262890683122, 1.000000000000000000, 0.9659258262890683122, 1.000000000000000000, 0.9659258262890683122, 1.000000000000000000, 0.9659258262890683122, 1.000000000000000000, 0.9659258262890683122, 1.000000000000000000, 0.9659258262890683122, 1.000000000000000000, 0.9659258262890683122, 1.000000000000000000, 0.9659258262890683122, 1.000000000000000000, 0.9659258262890683122, 1.000000000000000000, 0.9659258262890683122, 1.000000000000000000, 0.9659258262890683122, 1.000000000000000000, 0.9659258262890683122, 1.000000000000000000, 0.9659258262890683122, 1.000000000000000000, 0.9659258262890683122, 1.000000000000000000, 0.9659258262890683122, 1.000000000000000000, 0.9659258262890683122, 1.000000000000000000, 0.9659258262890683122, 1.000000000000000000, 0.9659258262890683122, 1.000000000000000000, 0.9659258262890683122, 1.000000000000000000, 0.9659258262890683122, 1.000000000000000000, 0.9659258262890683122, 1.000000000000000000, 0.9659258262890683122, 1.000000000000000000, 0.9659258262890683122, 1.000000000000000000, 0.9659258262890683122, 1.000000000000000000, 0.9659258262890683122, 1.000000000000000000, 0.9659258262890683122, 1.000000000000000000, 0.9659258262890683122, 1.000000000000000000, 0.9659258262890683122, 1.000000000000000000, 0.9659258262890683122, 1.000000000000000000, 0.9659258262890683122, 1.000000000000000000, 0.9659258262890683122, 1.000000000000000000, 0.9659258262890683122, 1.000000000000000000, 0.9659258262890683122, 1.000000000000000000, 0.9659258262890683122, 1.000000000000000000, 0.9659258262890683122, 1.000000000000000000, 0.9659258262890683122, 1.000000000000000000, 0.9659258262890683122, 1.000000000000000000, 0.9659258262890683122, 1.000000000000000000, 0.9659258262890683122, 1.000000000000000000, 0.9659258262890683122, 1.000000000000000000, 0.9659258262890683122, 1.000000000000000000, 0.9659258262890683122, 1.000000000000000000, 0.9659258262890683122, 1.000000000000000000, 0.9659258262890683122, 1.000000000000000000, 0.9659258262890683122, 1.000000000000000000, 0.9659258262890683122, 1.000000000000000000, 0.9659258262890683122, 1.000000000000000000, 0.9659258262890683122, 1.000000000000000000, 0.9659258262890683122, 1.000000000000000000, 0.9659258262890683122, 1.000000000000000000, 0.9659258262890683122, 1.000000000000000000, 0.9659258262890683122, 1.000000000000000000, 0.9659258262890683122, 1.000000000000000000, 0.9659258262890683122, 1.000000000000000000, 0.9659258262890683122, 1.000000000000000000, 0.9659258262890683122, 1.000000000000000000, 0.9659258262890683122, 1.000000000000000000, 0.9659258262890683122, 1.000000000000000000, 0.9659258262890683122, 1.000000000000000000, 0.9659258262890683122, 1.000000000000000000, 0.9659258262890683122, 1.000000000000000000, 0.9659258262890683122, 1.000000000000000000, 0.9659258262890683122, 1.000000000000000000, 0.9659258262890683122, 1.000000000000000000, 0.9659258262890683122, 1.000000000000000000, 0.9659258262890683122, 1.000000000000000000, 0.9659258262890683122, 1.000000000000000000, 0.9659258262890683122, 1.000000000000000000, 0.9659258262890683122, 1.000000000000000000, 0.9659258262890683122, 1.000000000000000000, 0.9659258262890683122, 1.000000000000000000, 0.9659258262890683122, 1.000000000000000000, 0.9659258262890683122, 1.000000000000000000, 0.9659258262890683122, 1.000000000000000000, 0.9659258262890683122, 1.000000000000000000, 0.9659258262890683122, 1.000000000000000000, 0.9659258262890683122, 1.000000000000000000, 0.9659258262890683122, 1.000000000000000000, 0.9659258262890683122, 1.000000000000000000, 0.9659258262890683122, 1.000000000000000000, 0.9659258262890683122, 1.000000000000000000, 0.9659258262890683122, 1.000000000000000000, 0.9659258262890683122, 1.000000000000000000, 0.9659258262890683122, 1.000000000000000000, 0.9659258262890683122, 1.000000000000000000, 0.9659258262890683122, 1.000000000000000000, 0.9659258262890683122, 1.000000000000000000, 0.9659258262890683122, 1.000000000000000000, 0.9659258262890683122, 1.000000000000000000, 0.9659258262890683122, 1.000000000000000000, 0.9659258262890683122, 1.000000000000000000, 0.9659258262890683122, 1.000000000000000000, 0.9659258262890683122, 1.000000000000000000, 0.9659258262890683122, 1.000000000000000000, 0.9659258262890683122, 1.000000000000000000, 0.9659258262890683122, 1.000000000000000000, 0.9659258262890683122, 1.000000000000000000, 0.9659258262890683122, 1.000000000000000000, 0.9659258262890683122, 1.000000000000000000, 0.9659258262890683122, 1.000000000000000000, 0.9659258262890683122, 1.000000000000000000, 0.9659258262890683122, 1.000000000000000000, 0.9659258262890683122, 1.000000000000000000, 0.9659258262890683122, 1.000000000000000000, 0.9659258262890683122, 1.000000000000000000, 0.9659258262890683122, 1.000000000000000000, 0.9659258262890683122, 1.000000000000000000, 0.9659258262890683122, 1.000000000000000000, 0.9659258262890683122, 1.000000000000000000, 0.9659258262890683122, 1.000000000000000000, 0.9659258262890683122, 1.000000000000000000, 0.9659258262890683122, 1.000000000000000000, 0.9659258262890683122, 1.000000000000000000, 0.9659258262890683122, 1.000000000000000000, 0.9659258262890683122, 1.000000000000000000, 0.9659258262890683122, 1.000000000000000000, 0.9659258262890683122, 1.000000000000000000, 0.9659258262890683122, 1.000000000000000000, 0.9659258262890683122, 1.000000000000000000, 0.9659258262890683122, 1.000000000000000000, 0.9659258262890683122, 1.000000000000000000, 0.9659258262890683122, 1.000000000000000000, 0.9659258262890683122, 1.000000000000000000, 0.9659258262890683122, 1.000000000000000000, 0.9659258262890683122, 1.000000000000000000, 0.9659258262890683122, 1.000000000000000000, 0.9659258262890683122, 1.000000000000000000, 0.9659258262890683122, 1.000000000000000000, 0.9659258262890683122, 1.000000000000000000, 0.9659258262890683122, 1.000000000000000000, 0.9659258262890683122, 1.000000000000000000, 0.9659258262890683122, 1.000000000000000000, 0.9659258262890683122, 1.000000000000000000, 0.9659258262890683122, 1.000000000000000000, 0.9659258262890683122, 1.000000000000000000, 0.9659258262890683122, 1.000000000000000000, 0.9659258262890683122, 1.000000000000000000, 0.9659258262890683122, 1.000000000000000000, 0.9659258262890683122, 1.000000000000000000, 0.9659258262890683122, 1.000000000000000000, 0.9659258262890683122, 1.000000000000000000, 0.9659258262890683122, 1.000000000000000000, 0.9659258262890683122, 1.000000000000000000, 0.9659258262890683122, 1.000000000000000000, 0.9659258262890683122, 1.000000000000000000, 0.9659258262890683122, 1.000000000000000000, 0.9659258262890683122, 1.000000000000000000, 0.9659258262890683122, 1.000000000000000000, 0.9659258262890683122, 1.000000000000000000, 0.9659258262890683122, 1.000000000000000000, 0.9659258262890683122, 1.000000000000000000, 0.9659258262890683122, 1.000000000000000000, 0.9659258262890683122, 1.000000000000000000, 0.9659258262890683122, 1.000000000000000000, 0.9659258262890683122, 1.000000000000000000, 0.9659258262890683122, 1.000000000000000000, 0.9659258262890683122, 1.000000000000000000, 0.9659258262890683122, 1.000000000000000000, 0.9659258262890683122, 1.000000000000000000, 0.9659258262890683122, 1.000000000000000000, 0.9659258262890683122, 1.000000000000000000, 0.9659258262890683122, 1.000000000000000000, 0.9659258262890683122, 1.000000000000000000, 0.9659258262890683122, 1.000000000000000000, 0.9659258262890683122, 1.000000000000000000, 0.9659258262890683122, 1.000000000000000000, 0.9659258262890683122, 1.000000000000000000, 0.9659258262890683122, 1.000000000000000000, 0.9659258262890683122, 1.000000000000000000, 0.9659258262890683122, 1.000000000000000000, 0.9659258262890683122, 1.000000000000000000, 0.9659258262890683122, 1.000000000000000000, 0.9659258262890683122, 1.000000000000000000, 0.9659258262890683122, 1.000000000000000000, 0.9659258262890683122, 1.000000000000000000, 0.9659258262890683122, 1.000000000000000000, 0.9659258262890683122, 1.000000000000000000, 0.9659258262890683122, 1.000000000000000000, 0.9659258262890683122, 1.000000000000000000, 0.9659258262890683122, 1.000000000000000000, 0.9659258262890683122, 1.000000000000000000, 0.9659258262890683122, 1.000000000000000000, 0.9659258262890683122, 1.000000000000000000, 0.9659258262890683122, 1.000000000000000000, 0.9659258262890683122, 1.000000000000000000, 0.9659258262890683122, 1.000000000000000000, 0.9659258262890683122, 1.000000000000000000, 0.9659258262890683122, 1.000000000000000000, 0.9659258262890683122, 1.000000000000000000, 0.9659258262890683122, 1.000000000000000000, 0.9659258262890683122, 1.000000000000000000, 0.9659258262890683122, 1.000000000000000000, 0.9659258262890683122, 1.000000000000000000, 0.9659258262890683122, 1.000000000000000000, 0.9659258262890683122, 1.000000000000000000, 0.9659258262890683122, 1.000000000000000000, 0.9659258262890683122, 1.000000000000000000, 0.9659258262890683122, 1.000000000000000000, 0.9659258262890683122, 1.000000000000000000, 0.9659258262890683122, 1.000000000000000000),
 ( 1.000000000000000000, 0.9659258262890683122, 1.000000000000000000, 0.9659258262890683122, 1.000000000000000000, 0.9659258262890683122, 1.000000000000000000, 0.9659258262890683122, 1.000000000000000000, 0.9659258262890683122, 1.000000000000000000, 0.9659258262890683122, 1.000000000000000000, 0.9659258262890683122, 1.000000000000000000, 0.9659258262890683122, 1.000000000000000000, 0.9659258262890683122, 1.000000000000000000, 0.9659258262890683122, 1.000000000000000000, 0.9659258262890683122, 1.000000000000000000, 0.9659258262890683122, 1.000000000000000000, 0.9659258262890683122, 1.000000000000000000, 0.9659258262890683122, 1.000000000000000000, 0.9659258262890683122, 1.000000000000000000, 0.9659258262890683122, 1.000000000000000000, 0.9659258262890683122, 1.000000000000000000, 0.9659258262890683122, 1.000000000000000000, 0.9659258262890683122, 1.000000000000000000, 0.9659258262890683122, 1.000000000000000000, 0.9659258262890683122, 1.000000000000000000, 0.9659258262890683122, 1.000000000000000000, 0.9659258262890683122, 1.000000000000000000, 0.9659258262890683122, 1.000000000000000000, 0.9659258262890683122, 1.000000000000000000, 0.9659258262890683122, 1.000000000000000000, 0.9659258262890683122, 1.000000000000000000, 0.9659258262890683122, 1.000000000000000000, 0.9659258262890683122, 1.000000000000000000, 0.9659258262890683122, 1.000000000000000000, 0.9659258262890683122, 1.000000000000000000, 0.9659258262890683122, 1.000000000000000000, 0.9659258262890683122, 1.000000000000000000, 0.9659258262890683122, 1.000000000000000000, 0.9659258262890683122, 1.000000000000000000, 0.9659258262890683122, 1.000000000000000000, 0.9659258262890683122, 1.000000000000000000, 0.9659258262890683122, 1.000000000000000000, 0.9659258262890683122, 1.000000000000000000, 0.9659258262890683122, 1.000000000000000000, 0.9659258262890683122, 1.000000000000000000, 0.9659258262890683122, 1.000000000000000000, 0.9659258262890683122, 1.000000000000000000, 0.9659258262890683122, 1.000000000000000000, 0.9659258262890683122, 1.000000000000000000, 0.9659258262890683122, 1.000000000000000000, 0.9659258262890683122, 1.000000000000000000, 0.9659258262890683122, 1.000000000000000000, 0.9659258262890683122, 1.000000000000000000, 0.9659258262890683122, 1.000000000000000000, 0.9659258262890683122, 1.000000000000000000, 0.9659258262890683122, 1.000000000000000000, 0.9659258262890683122, 1.000000000000000000, 0.9659258262890683122, 1.000000000000000000, 0.9659258262890683122, 1.000000000000000000, 0.9659258262890683122, 1.000000000000000000, 0.9659258262890683122, 1.000000000000000000, 0.9659258262890683122, 1.000000000000000000, 0.9659258262890683122, 1.000000000000000000, 0.9659258262890683122, 1.000000000000000000, 0.9659258262890683122, 1.000000000000000000, 0.9659258262890683122, 1.000000000000000000, 0.9659258262890683122, 1.000000000000000000, 0.9659258262890683122, 1.000000000000000000, 0.9659258262890683122, 1.000000000000000000, 0.9659258262890683122, 1.000000000000000000, 0.9659258262890683122, 1.000000000000000000, 0.9659258262890683122, 1.000000000000000000, 0.9659258262890683122, 1.000000000000000000, 0.9659258262890683122, 1.000000000000000000, 0.9659258262890683122, 1.000000000000000000, 0.9659258262890683122, 1.000000000000000000, 0.9659258262890683122, 1.000000000000000000, 0.9659258262890683122, 1.000000000000000000, 0.9659258262890683122, 1.000000000000000000, 0.9659258262890683122, 1.000000000000000000, 0.9659258262890683122, 1.000000000000000000, 0.9659258262890683122, 1.000000000000000000, 0.9659258262890683122, 1.000000000000000000, 0.9659258262890683122, 1.000000000000000000, 0.9659258262890683122, 1.000000000000000000, 0.9659258262890683122, 1.000000000000000000, 0.9659258262890683122, 1.000000000000000000, 0.9659258262890683122, 1.000000000000000000, 0.9659258262890683122, 1.000000000000000000, 0.9659258262890683122, 1.000000000000000000, 0.9659258262890683122, 1.000000000000000000, 0.9659258262890683122, 1.000000000000000000, 0.9659258262890683122, 1.000000000000000000, 0.9659258262890683122, 1.000000000000000000, 0.9659258262890683122, 1.000000000000000000, 0.9659258262890683122, 1.000000000000000000, 0.9659258262890683122, 1.000000000000000000, 0.9659258262890683122, 1.000000000000000000, 0.9659258262890683122, 1.000000000000000000, 0.9659258262890683122, 1.000000000000000000, 0.9659258262890683122, 1.000000000000000000, 0.9659258262890683122, 1.000000000000000000, 0.9659258262890683122, 1.000000000000000000, 0.9659258262890683122, 1.000000000000000000, 0.9659258262890683122, 1.000000000000000000, 0.9659258262890683122, 1.000000000000000000, 0.9659258262890683122, 1.000000000000000000, 0.9659258262890683122, 1.000000000000000000, 0.9659258262890683122, 1.000000000000000000, 0.9659258262890683122, 1.000000000000000000, 0.9659258262890683122, 1.000000000000000000, 0.9659258262890683122, 1.000000000000000000, 0.9659258262890683122, 1.000000000000000000, 0.9659258262890683122, 1.000000000000000000, 0.9659258262890683122, 1.000000000000000000, 0.9659258262890683122, 1.000000000000000000, 0.9659258262890683122, 1.000000000000000000, 0.9659258262890683122, 1.000000000000000000, 0.9659258262890683122, 1.000000000000000000, 0.9659258262890683122, 1.000000000000000000, 0.9659258262890683122, 1.000000000000000000, 0.9659258262890683122, 1.000000000000000000, 0.9659258262890683122, 1.000000000000000000, 0.9659258262890683122, 1.000000000000000000, 0.9659258262890683122, 1.000000000000000000, 0.9659258262890683122, 1.000000000000000000, 0.9659258262890683122, 1.000000000000000000, 0.9659258262890683122, 1.000000000000000000, 0.9659258262890683122, 1.000000000000000000, 0.9659258262890683122, 1.000000000000000000, 0.9659258262890683122, 1.000000000000000000, 0.9659258262890683122, 1.000000000000000000, 0.9659258262890683122, 1.000000000000000000, 0.9659258262890683122, 1.000000000000000000, 0.9659258262890683122, 1.000000000000000000, 0.9659258262890683122, 1.000000000000000000, 0.9659258262890683122, 1.000000000000000000, 0.9659258262890683122, 1.000000000000000000, 0.9659258262890683122, 1.000000000000000000, 0.9659258262890683122, 1.000000000000000000, 0.9659258262890683122, 1.000000000000000000, 0.9659258262890683122, 1.000000000000000000, 0.9659258262890683122, 1.000000000000000000, 0.9659258262890683122, 1.000000000000000000, 0.9659258262890683122, 1.000000000000000000, 0.9659258262890683122, 1.000000000000000000, 0.9659258262890683122, 1.000000000000000000, 0.9659258262890683122, 1.000000000000000000, 0.9659258262890683122, 1.000000000000000000, 0.9659258262890683122, 1.000000000000000000, 0.9659258262890683122, 1.000000000000000000, 0.9659258262890683122, 1.000000000000000000, 0.9659258262890683122, 1.000000000000000000, 0.9659258262890683122, 1.000000000000000000, 0.9659258262890683122, 1.000000000000000000, 0.9659258262890683122, 1.000000000000000000, 0.9659258262890683122, 1.000000000000000000, 0.9659258262890683122, 1.000000000000000000, 0.9659258262890683122, 1.000000000000000000, 0.9659258262890683122, 1.000000000000000000, 0.9659258262890683122, 1.000000000000000000, 0.9659258262890683122, 1.000000000000000000, 0.9659258262890683122, 1.000000000000000000, 0.9659258262890683122, 1.000000000000000000, 0.9659258262890683122, 1.000000000000000000, 0.9659258262890683122, 1.000000000000000000, 0.9659258262890683122, 1.000000000000000000, 0.9659258262890683122, 1.000000000000000000, 0.9659258262890683122, 1.000000000000000000, 0.9659258262890683122, 1.000000000000000000, 0.9659258262890683122, 1.000000000000000000, 0.9659258262890683122, 1.000000000000000000, 0.9659258262890683122, 1.000000000000000000, 0.9659258262890683122, 1.000000000000000000, 0.9659258262890683122, 1.000000000000000000, 0.9659258262890683122, 1.000000000000000000, 0.9659258262890683122, 1.000000000000000000, 0.9659258262890683122, 1.000000000000000000, 0.9659258262890683122, 1.000000000000000000, 0.9659258262890683122, 1.000000000000000000, 0.9659258262890683122, 1.000000000000000000, 0.9659258262890683122, 1.000000000000000000, 0.9659258262890683122, 1.000000000000000000, 0.9659258262890683122, 1.000000000000000000, 0.9659258262890683122, 1.000000000000000000, 0.9659258262890683122, 1.000000000000000000, 0.9659258262890683122, 1.000000000000000000, 0.9659258262890683122, 1.000000000000000000, 0.9659258262890683122, 1.000000000000000000, 0.9659258262890683122, 1.000000000000000000, 0.9659258262890683122, 1.000000000000000000, 0.9659258262890683122, 1.000000000000000000, 0.9659258262890683122, 1.000000000000000000, 0.9659258262890683122, 1.000000000000000000, 0.9659258262890683122, 1.000000000000000000, 0.9659258262890683122, 1.000000000000000000, 0.9659258262890683122, 1.000000000000000000, 0.9659258262890683122, 1.000000000000000000, 0.9659258262890683122, 1.000000000000000000, 0.9659258262890683122, 1.000000000000000000, 0.9659258262890683122, 1.000000000000000000, 0.9659258262890683122, 1.000000000000000000, 0.9659258262890683122, 1.000000000000000000, 0.9659258262890683122, 1.000000000000000000, 0.9659258262890683122, 1.000000000000000000, 0.9659258262890683122, 1.000000000000000000, 0.9659258262890683122, 1.000000000000000000, 0.9659258262890683122, 1.000000000000000000, 0.9659258262890683122, 1.000000000000000000, 0.9659258262890683122, 1.000000000000000000, 0.9659258262890683122, 1.000000000000000000, 0.9659258262890683122, 1.000000000000000000, 0.9659258262890683122, 1.000000000000000000, 0.9659258262890683122, 1.000000000000000000, 0.9659258262890683122, 1.000000000000000000, 0.9659258262890683122, 1.000000000000000000, 0.9659258262890683122, 1.000000000000000000, 0.9659258262890683122, 1.000000000000000000, 0.9659258262890683122, 1.000000000000000000, 0.9659258262890683122, 1.000000000000000000, 0.9659258262890683122, 1.000000000000000000, 0.9659258262890683122, 1.000000000000000000, 0.9659258262890683122, 1.000000000000000000, 0.9659258262890683122, 1.000000000000000000, 0.9659258262890683122, 1.000000000000000000, 0.9659258262890683122, 1.000000000000000000, 0.9659258262890683122, 1.000000000000000000, 0.9659258262890683122, 1.000000000000000000, 0.9659258262890683122, 1.000000000000000000, 0.9659258262890683122, 1.000000000000000000, 0.9659258262890683122, 1.000000000000000000, 0.9659258262890683122, 1.000000000000000000, 0.9659258262890683122, 1.000000000000000000, 0.9659258262890683122, 1.000000000000000000, 0.9659258262890683122, 1.000000000000000000, 0.9659258262890683122, 1.000000000000000000, 0.9659258262890683122, 1.000000000000000000, 0.9659258262890683122, 1.000000000000000000, 0.9659258262890683122, 1.000000000000000000, 0.9659258262890683122, 1.000000000000000000, 0.9659258262890683122, 1.000000000000000000, 0.9659258262890683122, 1.000000000000000000, 0.9659258262890683122, 1.000000000000000000, 0.9659258262890683122, 1.000000000000000000, 0.9659258262890683122, 1.000000000000000000, 0.9659258262890683122, 1.000000000000000000, 0.9659258262890683122, 1.000000000000000000, 0.9659258262890683122, 1.000000000000000000, 0.9659258262890683122, 1.000000000000000000, 0.9659258262890683122, 1.000000000000000000, 0.9659258262890683122, 1.000000000000000000, 0.9659258262890683122, 1.000000000000000000, 0.9659258262890683122, 1.000000000000000000, 0.9659258262890683122, 1.000000000000000000, 0.9659258262890683122, 1.000000000000000000, 0.9659258262890683122, 1.000000000000000000, 0.9659258262890683122, 1.000000000000000000, 0.9659258262890683122, 1.000000000000000000, 0.9659258262890683122, 1.000000000000000000) ) ) 
 REPRESENTATION_ITEM ( '' )  SURFACE ( )  );
#16734 = CARTESIAN_POINT ( 'NONE',  ( 1.450131233595801428, 0.2952755905511811885, 0.1292274648535926551 ) ) ;
#16735 = CARTESIAN_POINT ( 'NONE',  ( -0.7020997375328076329, -0.2845877964562161244, -0.3641732283464567121 ) ) ;
#16736 = CARTESIAN_POINT ( 'NONE',  ( -0.6692913385826764205, -0.6692913385826771977, 8.415575281601705876E-17 ) ) ;
#16737 = CARTESIAN_POINT ( 'NONE',  ( 1.548556430446194954, 0.2306618581243847221, -0.2411417322834647770 ) ) ;
#16738 = CARTESIAN_POINT ( 'NONE',  ( 1.443569553805774897, -0.6046776061558809534, -0.2411417322834644161 ) ) ;
#16739 = CARTESIAN_POINT ( 'NONE',  ( -1.653543307086613234, -0.1870078740157479769, 0.4822834645669291653 ) ) ;
#16740 = CARTESIAN_POINT ( 'NONE',  ( -1.299212598425196097, -0.5511811023622047445, 6.969142054262312111E-17 ) ) ;
#16741 = CARTESIAN_POINT ( 'NONE',  ( 0.2925321140481931814, -0.2925321140481931259, -0.3326771653543306728 ) ) ;
#16742 = CARTESIAN_POINT ( 'NONE',  ( -0.1998031496062994683, 0.3460692066303958092, -0.4855643044619422644 ) ) ;
#16743 = CARTESIAN_POINT ( 'NONE',  ( 0.3392501089628018884, -0.1958661417322833942, -2.778890706857954473 ) ) ;
#16744 = EDGE_CURVE ( 'NONE', #6386, #50169, #34593, .T. ) ;
#16745 = CARTESIAN_POINT ( 'NONE',  ( 0.03087045868620516900, -0.3974833285012868700, -5.548669992249399928E-14 ) ) ;
#16746 = CARTESIAN_POINT ( 'NONE',  ( 1.279527559055118724, 0.07958543189024085140, 0.2665933059059887866 ) ) ;
#16747 = CARTESIAN_POINT ( 'NONE',  ( 0.8792650918635177559, -0.4281496062992127816, -0.4176697321401328100 ) ) ;
#16748 = CARTESIAN_POINT ( 'NONE',  ( 0.01241954290193841674, 0.000000000000000000, 0.3464511005275205946 ) ) ;
#16749 = CARTESIAN_POINT ( 'NONE',  ( 0.7086614173228352742, -0.1870078740157480879, -0.4822834645669291653 ) ) ;
#16750 = CARTESIAN_POINT ( 'NONE',  ( -0.2891555358219909388, -0.2891555358219912164, -0.7657480314960630752 ) ) ;
#16751 = CARTESIAN_POINT ( 'NONE',  ( 1.069553805774278832, 0.1771653543307087075, -0.09757992244046823083 ) ) ;
#16752 = CARTESIAN_POINT ( 'NONE',  ( 0.2821522309711292364, 0.2952755905511810774, -0.1292274648535930714 ) ) ;
#16753 = CARTESIAN_POINT ( 'NONE',  ( -0.8464566929133852113, 0.1660481256975885056, 0.3530559997133364547 ) ) ;
#16754 = CARTESIAN_POINT ( 'NONE',  ( 1.397637795275591177, 0.1660481256975883668, -0.3530559997133364547 ) ) ;
#16755 = CARTESIAN_POINT ( 'NONE',  ( -0.2362204724409447953, -0.4091458600556404646, -1.010498687664042050 ) ) ;
#16756 = CARTESIAN_POINT ( 'NONE',  ( 0.3996062992125986035, -0.1070741851644053111, -2.316272965879265122 ) ) ;
#16757 = CARTESIAN_POINT ( 'NONE',  ( 0.2034120734908142214, 0.1771653543307087075, -0.09757992244046823083 ) ) ;
#16758 = EDGE_CURVE ( 'NONE', #76877, #22642, #53157, .T. ) ;
#16759 = ORIENTED_EDGE ( 'NONE', *, *, #75818, .T. ) ;
#16760 = CARTESIAN_POINT ( 'NONE',  ( 0.3392501089628018329, 0.1958661417322835607, -0.9153736464905005699 ) ) ;
#16761 = VERTEX_POINT ( 'NONE', #23104 ) ;
#16762 = CARTESIAN_POINT ( 'NONE',  ( -0.8989501312335946848, 0.2952755905511810774, -0.1292274648535930714 ) ) ;
#16763 = CARTESIAN_POINT ( 'NONE',  ( -0.1509186351706028884, -0.3162353388693409650, -0.4822834645669289433 ) ) ;
#16764 = CARTESIAN_POINT ( 'NONE',  ( -0.4396325459317577122, -0.6692913385826773087, -0.1292274648535924053 ) ) ;
#16765 = CIRCLE ( 'NONE', #30142, 1.122047244094488194 ) ;
#16766 = CARTESIAN_POINT ( 'NONE',  ( 0.6692913385826778638, -0.6692913385826771977, 8.415575281601705876E-17 ) ) ;
#16767 = EDGE_CURVE ( 'NONE', #17617, #21842, #63066, .T. ) ;
#16768 = CARTESIAN_POINT ( 'NONE',  ( -1.437007874015747477, 0.1660481256975883668, -0.3530559997133364547 ) ) ;
#16769 = CARTESIAN_POINT ( 'NONE',  ( -0.2821522309711278487, 0.2952755905511811885, 0.1292274648535926551 ) ) ;
#16770 = CARTESIAN_POINT ( 'NONE',  ( 1.246719160104987623, -0.4281496062992124485, 0.4176697321401328655 ) ) ;
#16771 = CARTESIAN_POINT ( 'NONE',  ( 0.5905511811023629321, -0.6692913385826771977, 8.415575281601705876E-17 ) ) ;
#16772 = CARTESIAN_POINT ( 'NONE',  ( 0.6233595800524942554, -0.05778040916215560624, -0.4822834645669293319 ) ) ;
#16773 = CARTESIAN_POINT ( 'NONE',  ( 0.1049643490035304938, -0.3917322834645669549, -1.022309711286088829 ) ) ;
#16774 = CARTESIAN_POINT ( 'NONE',  ( -0.5905511811023613777, -0.5511811023622047445, 6.969142054262312111E-17 ) ) ;
#16775 = ORIENTED_EDGE ( 'NONE', *, *, #79045, .F. ) ;
#16776 = CARTESIAN_POINT ( 'NONE',  ( 0.1058382717557499880, 0.3949938075777411073, -1.410761154855643351 ) ) ;
#16777 = ORIENTED_EDGE ( 'NONE', *, *, #11153, .T. ) ;
#16778 = CARTESIAN_POINT ( 'NONE',  ( -0.8989501312335946848, 0.1771653543307087075, -0.09757992244046823083 ) ) ;
#16779 = CARTESIAN_POINT ( 'NONE',  ( -0.2624671916010490880, -0.6046776061558807314, 0.2411417322834647770 ) ) ;
#16780 = CARTESIAN_POINT ( 'NONE',  ( -0.1998031496062994683, 0.3460692066303958092, 0.1443569553805774119 ) ) ;
#16781 = CARTESIAN_POINT ( 'NONE',  ( -0.8530183727034112984, -0.4281496062992127816, -0.4176697321401328100 ) ) ;
#16782 = CARTESIAN_POINT ( 'NONE',  ( -0.9580052493438311334, -0.4281496062992124485, 0.4176697321401328655 ) ) ;
#16783 = CARTESIAN_POINT ( 'NONE',  ( -1.391076115485563314, -0.6046776061558809534, -0.2411417322834644161 ) ) ;
#16784 = CARTESIAN_POINT ( 'NONE',  ( -1.240157480314959759, 0.1660481256975885056, 0.3530559997133364547 ) ) ;
#16785 = VECTOR ( 'NONE', #55692, 39.37007874015748143 ) ;
#16786 = CARTESIAN_POINT ( 'NONE',  ( 0.7480314960629927956, 0.1771653543307087630, 0.000000000000000000 ) ) ;
#16787 = CARTESIAN_POINT ( 'NONE',  ( -0.4724409448818896462, -0.1265901696524993070, -0.9908136482939633449 ) ) ;
#16788 = CARTESIAN_POINT ( 'NONE',  ( 0.1265901696524990572, -0.4724409448818897017, -0.6345144356955381149 ) ) ;
#16789 = CARTESIAN_POINT ( 'NONE',  ( 0.07217847769028949700, -0.08942795157528024563, -0.3641732283464568787 ) ) ;
#16790 = CARTESIAN_POINT ( 'NONE',  ( -0.05905511811023545637, 0.1660481256975885056, 0.3530559997133364547 ) ) ;
#16791 = CARTESIAN_POINT ( 'NONE',  ( 0.07217847769028949700, -0.3162353388693405765, 0.4822834645669290543 ) ) ;
#16792 = ORIENTED_EDGE ( 'NONE', *, *, #56212, .T. ) ;
#16793 = CARTESIAN_POINT ( 'NONE',  ( 0.2925321140481932369, -0.2925321140481932369, -1.515748031496062742 ) ) ;
#16794 = CARTESIAN_POINT ( 'NONE',  ( -0.6299212598425059095, 1.724409448818897905, -3.937007874015764131 ) ) ;
#16795 = ORIENTED_EDGE ( 'NONE', *, *, #80522, .T. ) ;
#16796 = CARTESIAN_POINT ( 'NONE',  ( 0.1070741851644053388, 0.3996062992125986035, -1.172572178477690352 ) ) ;
#16797 = CARTESIAN_POINT ( 'NONE',  ( 1.594488188976378673, 0.1660481256975885056, 0.3530559997133364547 ) ) ;
#16798 = CARTESIAN_POINT ( 'NONE',  ( -0.8136482939632537770, -0.5023911411419708095, 0.1820866141732285504 ) ) ;
#16799 = CARTESIAN_POINT ( 'NONE',  ( -0.7874015748031489847, -0.1870078740157479769, 0.4822834645669291653 ) ) ;
#16800 = CARTESIAN_POINT ( 'NONE',  ( 0.4091458600556403535, 0.2362204724409449896, -0.4461942257217847430 ) ) ;
#16801 = ADVANCED_FACE ( 'NONE', ( #49186 ), #20409, .F. ) ;
#16802 = CARTESIAN_POINT ( 'NONE',  ( -1.646051170424378096, 0.4405861044731112508, 0.5309055118110234117 ) ) ;
#16803 = CARTESIAN_POINT ( 'NONE',  ( -0.1958661417322834220, -0.3392501089628018884, -2.512467191601049699 ) ) ;
#16804 = CARTESIAN_POINT ( 'NONE',  ( -1.620734908136482577, 0.1771653543307087630, 0.09757992244046791164 ) ) ;
#16805 = CARTESIAN_POINT ( 'NONE',  ( 0.3871391076115492380, -0.05778040916215560624, -0.4822834645669293319 ) ) ;
#16806 = CARTESIAN_POINT ( 'NONE',  ( 0.4790026246719168435, -0.3162353388693409650, -0.4822834645669289433 ) ) ;
#16807 = CARTESIAN_POINT ( 'NONE',  ( -0.7545931758530176614, -0.5511811023622048555, -0.09757992244046775898 ) ) ;
#16808 = CARTESIAN_POINT ( 'NONE',  ( 0.03280839895013198948, 0.2952755905511811885, 0.1292274648535926551 ) ) ;
#16809 = CARTESIAN_POINT ( 'NONE',  ( -0.2362204724409451284, 0.4091458600556402425, -2.294619422572178102 ) ) ;
#16810 = CARTESIAN_POINT ( 'NONE',  ( -0.6364829396325453192, -0.3162353388693405765, 0.4822834645669290543 ) ) ;
#16811 = ADVANCED_FACE ( 'NONE', ( #76749 ), #12780, .F. ) ;
#16812 = CARTESIAN_POINT ( 'NONE',  ( 0.1058382717557499880, 0.3949938075777409408, -1.959973753280839670 ) ) ;
#16813 = CARTESIAN_POINT ( 'NONE',  ( 1.496062992125984703, -0.1870078740157480601, -0.3641732283464567677 ) ) ;
#16814 = CARTESIAN_POINT ( 'NONE',  ( 0.1377952755905518800, -0.4536011799217367080, 0.2665933059059888421 ) ) ;
#16815 = CARTESIAN_POINT ( 'NONE',  ( 1.030183727034121421, -0.08942795157527998196, 0.3641732283464567121 ) ) ;
#16816 = CARTESIAN_POINT ( 'NONE',  ( -1.227034120734907585, 0.2952755905511811885, 0.1292274648535926551 ) ) ;
#16817 = CARTESIAN_POINT ( 'NONE',  ( -1.345144356955379816, -0.2845877964562159024, 0.3641732283464567677 ) ) ;
#16818 = CARTESIAN_POINT ( 'NONE',  ( -1.220472440944878834, 2.401574803149606474, -0.4915354330708643360 ) ) ;
#16819 = CARTESIAN_POINT ( 'NONE',  ( -1.115485564304461219, -0.4281496062992124485, 0.4176697321401328655 ) ) ;
#16820 = CARTESIAN_POINT ( 'NONE',  ( -0.3805774278215216522, 0.05413385826771666132, 0.4176697321401328100 ) ) ;
#16821 = CARTESIAN_POINT ( 'NONE',  ( 0.3674540682414705883, -0.6046776061558807314, 0.2411417322834647770 ) ) ;
#16822 = CARTESIAN_POINT ( 'NONE',  ( -9.594673741351310580E-17, 0.3917322834645669549, -2.599718217026559586 ) ) ;
#16823 = CARTESIAN_POINT ( 'NONE',  ( 1.091264520429693574, -3.876714527516387216E-16, -0.3954974714151466841 ) ) ;
#16824 = CARTESIAN_POINT ( 'NONE',  ( 0.1443569553805781891, -0.004921259842519870586, -0.3153832671262229437 ) ) ;
#16825 = CARTESIAN_POINT ( 'NONE',  ( 0.8464566929133865436, 0.1660481256975883668, -0.3530559997133364547 ) ) ;
#16826 = CARTESIAN_POINT ( 'NONE',  ( -1.587926509186350810, -0.3690944881889763329, 0.3153832671262228327 ) ) ;
#16827 = CARTESIAN_POINT ( 'NONE',  ( 0.8267716535433078384, -0.6692913385826771977, 8.415575281601705876E-17 ) ) ;
#16828 = FACE_OUTER_BOUND ( 'NONE', #74750, .T. ) ;
#16829 = CARTESIAN_POINT ( 'NONE',  ( -1.476377952755905110, -0.5400638737290845981, -0.3530559997133363437 ) ) ;
#16830 = CARTESIAN_POINT ( 'NONE',  ( -0.9448818897637790704, -0.1870078740157479769, 0.4822834645669291653 ) ) ;
#16831 = CARTESIAN_POINT ( 'NONE',  ( -0.2034120734908128059, 0.1771653543307087630, 0.09757992244046791164 ) ) ;
#16832 = DIRECTION ( 'NONE',  ( 1.408710688920637755E-15, -1.000000000000000000, 4.918487082195260922E-30 ) ) ;
#16833 = CARTESIAN_POINT ( 'NONE',  ( 0.6167979002624678353, -0.3690944881889763329, 0.3153832671262228327 ) ) ;
#16834 = CARTESIAN_POINT ( 'NONE',  ( -0.3460692066303957537, -0.1998031496062994405, -0.9166666666666666297 ) ) ;
#16835 = CARTESIAN_POINT ( 'NONE',  ( 0.1049868766404206816, 0.2306618581243848609, 0.2411417322834645549 ) ) ;
#16836 = CARTESIAN_POINT ( 'NONE',  ( -0.3996062992125984925, -0.1070741851644056858, -0.4376640419947506744 ) ) ;
#16837 = CARTESIAN_POINT ( 'NONE',  ( -1.082677165354329896, 0.1660481256975885056, 0.3530559997133364547 ) ) ;
#16838 = CARTESIAN_POINT ( 'NONE',  ( 0.2867679344610365999, 0.2867679344610365999, -1.954724409448818978 ) ) ;
#16839 = CARTESIAN_POINT ( 'NONE',  ( 0.8464566929133865436, 0.07958543189024071263, -0.2665933059059888421 ) ) ;
#16840 = CARTESIAN_POINT ( 'NONE',  ( 0.1771653543307093182, -0.5400638737290845981, -0.3530559997133363437 ) ) ;
#16841 = CARTESIAN_POINT ( 'NONE',  ( -0.4724409448818890911, -0.1870078740157480879, -0.4822834645669291653 ) ) ;
#16842 = CARTESIAN_POINT ( 'NONE',  ( -0.2624671916010490880, -0.5023911411419708095, 0.1820866141732285504 ) ) ;
#16843 = CARTESIAN_POINT ( 'NONE',  ( -1.646051170424378096, 0.000000000000000000, -0.3464511005275205946 ) ) ;
#16844 = CARTESIAN_POINT ( 'NONE',  ( -0.3412073490813641308, 0.1283753931104746893, -0.1820866141732285504 ) ) ;
#16845 = CARTESIAN_POINT ( 'NONE',  ( 0.4921259842519691285, -0.5400638737290845981, -0.3530559997133363437 ) ) ;
#16846 = CARTESIAN_POINT ( 'NONE',  ( -1.017060367454067249, -0.2845877964562161244, -0.3641732283464567121 ) ) ;
#16848 = CARTESIAN_POINT ( 'NONE',  ( 0.2925321140481932369, -0.2925321140481931814, -1.435039370078740495 ) ) ;
#16847 = CIRCLE ( 'NONE', #77259, 1.122047244094488194 ) ;
#16849 = CARTESIAN_POINT ( 'NONE',  ( 1.522309711286089939, -0.6046776061558809534, -0.2411417322834644161 ) ) ;
#16850 = DIRECTION ( 'NONE',  ( -1.000000000000000000, -3.050063254464715288E-16, 0.000000000000000000 ) ) ;
#16851 = ORIENTED_EDGE ( 'NONE', *, *, #46574, .F. ) ;
#16852 = CARTESIAN_POINT ( 'NONE',  ( -1.574803149606298636, -0.1870078740157479769, 0.3641732283464567677 ) ) ;
#16853 = CARTESIAN_POINT ( 'NONE',  ( -0.4724409448818890911, -0.1870078740157479769, 0.4822834645669291653 ) ) ;
#16854 = CARTESIAN_POINT ( 'NONE',  ( -1.272965879265091305, 0.05413385826771626580, -0.4176697321401330321 ) ) ;
#16855 = CARTESIAN_POINT ( 'NONE',  ( 4.797336870675656522E-17, -0.3917322834645670104, -1.423228346456693050 ) ) ;
#16856 = CARTESIAN_POINT ( 'NONE',  ( 0.000000000000000000, 2.755905511811024056, 0.000000000000000000 ) ) ;
#16857 = CARTESIAN_POINT ( 'NONE',  ( 1.312335958005250269, -0.6046776061558807314, 0.2411417322834647770 ) ) ;
#16858 = CARTESIAN_POINT ( 'NONE',  ( 0.6299212598425204535, -0.1870078740157480879, -0.4822834645669291653 ) ) ;
#16859 = DIRECTION ( 'NONE',  ( -1.000000000000000000, -0.000000000000000000, -0.000000000000000000 ) ) ;
#16860 = CARTESIAN_POINT ( 'NONE',  ( -9.787531504996566615E-17, 0.3996062992125985480, -2.438976377952756014 ) ) ;
#16861 = CARTESIAN_POINT ( 'NONE',  ( -1.548556430446193399, 0.2306618581243848609, 0.2411417322834645549 ) ) ;
#16862 = EDGE_CURVE ( 'NONE', #10444, #5673, #52304, .T. ) ;
#16863 = CARTESIAN_POINT ( 'NONE',  ( 0.3460692066303959202, 0.1998031496062993295, -0.7611548556430446366 ) ) ;
#16864 = VERTEX_POINT ( 'NONE', #33800 ) ;
#16865 = CARTESIAN_POINT ( 'NONE',  ( -0.8727034120734901146, -0.2845877964562159024, 0.3641732283464567677 ) ) ;
#16866 = CARTESIAN_POINT ( 'NONE',  ( -0.1958661417322836718, 0.3392501089628017219, -2.839895013123359568 ) ) ;
#16867 = ORIENTED_EDGE ( 'NONE', *, *, #3552, .T. ) ;
#16868 = CARTESIAN_POINT ( 'NONE',  ( 0.6824146981627303710, 0.2306618581243847221, -0.2411417322834647770 ) ) ;
#16869 = CARTESIAN_POINT ( 'NONE',  ( -0.1771653543307080136, -0.5400638737290844871, 0.3530559997133364547 ) ) ;
#16870 = CARTESIAN_POINT ( 'NONE',  ( -1.174540682414697335, -0.05778040916215522460, 0.4822834645669289988 ) ) ;
#16871 = CARTESIAN_POINT ( 'NONE',  ( 1.030183727034121421, -0.05778040916215522460, 0.4822834645669289988 ) ) ;
#16872 = CARTESIAN_POINT ( 'NONE',  ( -1.089238845144356427, -0.3690944881889765550, -0.3153832671262227771 ) ) ;
#16873 = DIRECTION ( 'NONE',  ( -0.000000000000000000, -1.000000000000000000, -0.000000000000000000 ) ) ;
#16874 = CARTESIAN_POINT ( 'NONE',  ( 0.4593175853018380828, 0.05413385826771626580, -0.4176697321401330321 ) ) ;
#16875 = CARTESIAN_POINT ( 'NONE',  ( -0.9448818897637790704, -0.1870078740157480879, -0.4822834645669291653 ) ) ;
#16876 = CARTESIAN_POINT ( 'NONE',  ( -0.3392501089628019439, 0.1958661417322832554, -1.681083046422885197 ) ) ;
#16877 = FACE_OUTER_BOUND ( 'NONE', #25206, .T. ) ;
#16878 = CARTESIAN_POINT ( 'NONE',  ( 0.01706770257043118549, 1.062992125984252301, -2.874015748031495399 ) ) ;
#16879 = CARTESIAN_POINT ( 'NONE',  ( 1.056430446194226658, 0.2952755905511811885, 0.1292274648535926551 ) ) ;
#16880 = CARTESIAN_POINT ( 'NONE',  ( -0.1958661417322836718, 0.3392501089628017219, -2.774934383202099841 ) ) ;
#16881 = CARTESIAN_POINT ( 'NONE',  ( 1.358267716535433323, 0.07958543189024085140, 0.2665933059059887866 ) ) ;
#16882 = EDGE_LOOP ( 'NONE', ( #4729, #20294, #8279, #30543, #23475 ) ) ;
#16883 = CARTESIAN_POINT ( 'NONE',  ( -0.1958661417322836995, 0.3392501089628017219, -2.687027189797587035 ) ) ;
#16884 = CARTESIAN_POINT ( 'NONE',  ( -0.2296587926509179312, -0.05778040916215522460, 0.4822834645669289988 ) ) ;
#16885 = VERTEX_POINT ( 'NONE', #21997 ) ;
#16886 = CARTESIAN_POINT ( 'NONE',  ( 0.2427821522309716595, -0.2845877964562161244, -0.3641732283464567121 ) ) ;
#16887 = CARTESIAN_POINT ( 'NONE',  ( -1.692913385826770645, 0.2952755905511811885, 0.000000000000000000 ) ) ;
#16888 = CARTESIAN_POINT ( 'NONE',  ( 0.5708661417322841158, -0.5400638737290845981, -0.3530559997133363437 ) ) ;
#16889 = CARTESIAN_POINT ( 'NONE',  ( 0.9251968503937015864, -0.5400638737290844871, 0.3530559997133364547 ) ) ;
#16890 = CARTESIAN_POINT ( 'NONE',  ( 0.03280839895013198948, 0.2952755905511811885, 0.1292274648535926551 ) ) ;
#16891 = CARTESIAN_POINT ( 'NONE',  ( -0.3917322834645670104, -0.1049643490035307020, -1.145032439141419500 ) ) ;
#16892 = CARTESIAN_POINT ( 'NONE',  ( -0.7349081364829387342, -0.6046776061558807314, 0.2411417322834647770 ) ) ;
#16893 = CARTESIAN_POINT ( 'NONE',  ( -0.1049643490035302024, -0.3917322834645671215, -2.361548556430446144 ) ) ;
#16894 = CARTESIAN_POINT ( 'NONE',  ( 1.587926509186352142, -0.004921259842519576551, 0.3153832671262227771 ) ) ;
#16895 = CARTESIAN_POINT ( 'NONE',  ( -0.8267716535433065062, 0.2952755905511811885, 0.000000000000000000 ) ) ;
#16896 = CARTESIAN_POINT ( 'NONE',  ( 1.476377952755906442, -0.5400638737290844871, 0.3530559997133364547 ) ) ;
#16897 = CARTESIAN_POINT ( 'NONE',  ( 1.305774278215223960, -0.6692913385826771977, 0.1292274648535927661 ) ) ;
#16898 = CARTESIAN_POINT ( 'NONE',  ( -0.1070741851644056997, 0.3996062992125986035, -0.4790026246719158998 ) ) ;
#16899 = CARTESIAN_POINT ( 'NONE',  ( -0.7217847769028863381, 0.05413385826771626580, -0.4176697321401330321 ) ) ;
#16900 = CARTESIAN_POINT ( 'NONE',  ( 0.1998031496062994128, -0.3460692066303957537, 0.1463254593175852825 ) ) ;
#16901 = CARTESIAN_POINT ( 'NONE',  ( 0.1049868766404206816, -0.6046776061558809534, -0.2411417322834644161 ) ) ;
#16902 = CARTESIAN_POINT ( 'NONE',  ( 0.2925321140481932369, -0.2925321140481932369, -2.145669291338581974 ) ) ;
#16903 = CARTESIAN_POINT ( 'NONE',  ( -0.5905511811023613777, -0.6692913385826771977, 8.415575281601705876E-17 ) ) ;
#16904 = CIRCLE ( 'NONE', #6109, 2.362204724409449064 ) ;
#16905 = CARTESIAN_POINT ( 'NONE',  ( 1.620734908136483465, -0.6692913385826771977, 0.1292274648535927661 ) ) ;
#16906 = CARTESIAN_POINT ( 'NONE',  ( 0.7480314960629927956, 0.1771653543307087630, 0.000000000000000000 ) ) ;
#16907 = CARTESIAN_POINT ( 'NONE',  ( 1.220472440944882386, -0.6692913385826771977, 8.415575281601705876E-17 ) ) ;
#16908 = CARTESIAN_POINT ( 'NONE',  ( -0.2362204724409447953, -0.4091458600556404646, -1.087270341207349000 ) ) ;
#16909 = CARTESIAN_POINT ( 'NONE',  ( 0.9645669291338591078, -0.4536011799217368745, -0.2665933059059886201 ) ) ;
#16910 = CARTESIAN_POINT ( 'NONE',  ( 0.6758530183727039509, 0.2952755905511810774, -0.1292274648535930714 ) ) ;
#16911 = CARTESIAN_POINT ( 'NONE',  ( 0.3420746716998660508, -0.1974969037888704149, -0.4967191601049869010 ) ) ;
#16912 = CARTESIAN_POINT ( 'NONE',  ( -1.003937007874015297, -0.5400638737290845981, -0.3530559997133363437 ) ) ;
#16913 = CARTESIAN_POINT ( 'NONE',  ( -1.603475055217291612, 2.157339783260149080, -0.04573490813648262154 ) ) ;
#16914 = CARTESIAN_POINT ( 'NONE',  ( 1.154855643044620184, 0.1283753931104746893, -0.1820866141732285504 ) ) ;
#16915 = CARTESIAN_POINT ( 'NONE',  ( -0.4593175853018366950, 0.05413385826771666132, 0.4176697321401328100 ) ) ;
#16916 = CARTESIAN_POINT ( 'NONE',  ( 0.03937007874015806264, 0.2952755905511811885, 0.000000000000000000 ) ) ;
#16917 = CARTESIAN_POINT ( 'NONE',  ( 0.1689764809739037477, -2.839693391405754848E-15, 0.3791475997938237308 ) ) ;
#16918 = CARTESIAN_POINT ( 'NONE',  ( -0.09842519685039295696, 0.1660481256975883668, -0.3530559997133364547 ) ) ;
#16919 = CARTESIAN_POINT ( 'NONE',  ( 0.01312335958005323398, -0.3690944881889765550, -0.3153832671262227771 ) ) ;
#16920 = CARTESIAN_POINT ( 'NONE',  ( -2.554262525012223062, 1.528804020127598973, 0.4744094488188971281 ) ) ;
#16921 = CARTESIAN_POINT ( 'NONE',  ( 0.1640419947506569498, -0.2845877964562161244, -0.3641732283464567121 ) ) ;
#16922 = CARTESIAN_POINT ( 'NONE',  ( 0.6627296587926515548, 0.1771653543307087630, 0.09757992244046791164 ) ) ;
#16923 = DIRECTION ( 'NONE',  ( 0.000000000000000000, 0.000000000000000000, 1.000000000000000000 ) ) ;
#16924 = CARTESIAN_POINT ( 'NONE',  ( 0.2925321140481932369, 0.2925321140481932369, -1.946850393700787496 ) ) ;
#16925 = CARTESIAN_POINT ( 'NONE',  ( 0.3937007874015754361, -0.1870078740157479769, 0.4822834645669291653 ) ) ;
#16926 = CARTESIAN_POINT ( 'NONE',  ( 0.1958661417322834775, 0.3392501089628018884, -1.238845144356955252 ) ) ;
#16927 = CARTESIAN_POINT ( 'NONE',  ( 1.410761154855643795, -0.08942795157528024563, -0.3641732283464568787 ) ) ;
#16928 = DIRECTION ( 'NONE',  ( 0.000000000000000000, 0.000000000000000000, 1.000000000000000000 ) ) ;
#16929 = CARTESIAN_POINT ( 'NONE',  ( -0.5380577427821514602, -0.3690944881889765550, -0.3153832671262227771 ) ) ;
#16930 = CARTESIAN_POINT ( 'NONE',  ( 0.2690288713910767848, 0.2952755905511811885, 0.1292274648535926551 ) ) ;
#16931 = CARTESIAN_POINT ( 'NONE',  ( 1.233595800524935227, 0.1283753931104746893, -0.1820866141732285504 ) ) ;
#16932 = CARTESIAN_POINT ( 'NONE',  ( -1.437007874015747477, -0.4536011799217367080, 0.2665933059059888421 ) ) ;
#16933 = CARTESIAN_POINT ( 'NONE',  ( -1.574803149606298636, -0.1870078740157479769, 0.4822834645669291653 ) ) ;
#16934 = CARTESIAN_POINT ( 'NONE',  ( 0.2755905511811031494, 0.2952755905511811885, 0.000000000000000000 ) ) ;
#16935 = CARTESIAN_POINT ( 'NONE',  ( 1.377952755905512472, 0.2952755905511811885, 0.000000000000000000 ) ) ;
#16936 = CARTESIAN_POINT ( 'NONE',  ( -0.02273980556643043910, 1.063502421567459111, -1.634061201692638132 ) ) ;
#16937 = CARTESIAN_POINT ( 'NONE',  ( 0.1640419947506569498, -0.05778040916215522460, 0.4822834645669289988 ) ) ;
#16938 = CARTESIAN_POINT ( 'NONE',  ( 1.404199475065617708, 0.05413385826771626580, -0.4176697321401330321 ) ) ;
#16939 = CARTESIAN_POINT ( 'NONE',  ( 0.8595800524934390507, -0.3162353388693405765, 0.4822834645669290543 ) ) ;
#16940 = CARTESIAN_POINT ( 'NONE',  ( 0.4724409448818898127, -0.1265901696524988629, -0.3458005249343831244 ) ) ;
#16941 = CARTESIAN_POINT ( 'NONE',  ( 0.9645669291338591078, -0.4536011799217368745, -0.2665933059059886201 ) ) ;
#16942 = CARTESIAN_POINT ( 'NONE',  ( 1.476377952755906442, -0.5400638737290844871, 0.3530559997133364547 ) ) ;
#16943 = CARTESIAN_POINT ( 'NONE',  ( -0.06561679790026180015, -0.3690944881889765550, -0.3153832671262227771 ) ) ;
#16944 = CARTESIAN_POINT ( 'NONE',  ( -0.09186351706036663400, -0.4281496062992124485, 0.4176697321401328655 ) ) ;
#16945 = CARTESIAN_POINT ( 'NONE',  ( 0.6561679790026253567, 0.2306618581243848609, 0.2411417322834645549 ) ) ;
#16946 = CARTESIAN_POINT ( 'NONE',  ( -0.4002624671916004129, -0.3162353388693405765, 0.4822834645669290543 ) ) ;
#16947 = CARTESIAN_POINT ( 'NONE',  ( -0.1958661417322836995, 0.3392501089628017219, -2.214586244915697222 ) ) ;
#16948 = CARTESIAN_POINT ( 'NONE',  ( -0.2165354330708654795, -0.4536011799217368745, -0.2665933059059886201 ) ) ;
#16949 = CARTESIAN_POINT ( 'NONE',  ( 0.6824146981627303710, 0.2306618581243847221, -0.2411417322834647770 ) ) ;
#16950 = CARTESIAN_POINT ( 'NONE',  ( 0.8595800524934390507, -0.2845877964562159024, 0.3641732283464567677 ) ) ;
#16951 = ADVANCED_FACE ( 'NONE', ( #33390 ), #20338, .F. ) ;
#16952 = CARTESIAN_POINT ( 'NONE',  ( -1.645124945854690601, 1.142361046343763897, 0.2627170963995461572 ) ) ;
#16954 = FACE_OUTER_BOUND ( 'NONE', #65858, .T. ) ;
#16953 = DIRECTION ( 'NONE',  ( 0.000000000000000000, -1.000000000000000000, 0.000000000000000000 ) ) ;
#16955 = CARTESIAN_POINT ( 'NONE',  ( -1.200787401574802349, 0.1012011053420775880, -0.2882089793578257453 ) ) ;
#16957 = AXIS2_PLACEMENT_3D ( 'NONE', #38393, #77121, #56914 ) ;
#16956 = CARTESIAN_POINT ( 'NONE',  ( -1.220472440944881054, -0.6692913385826771977, 8.415575281601705876E-17 ) ) ;
#16958 = CARTESIAN_POINT ( 'NONE',  ( -0.3937007874015740483, -0.1870078740157480879, -0.4822834645669291653 ) ) ;
#16959 = CARTESIAN_POINT ( 'NONE',  ( -0.1265901696524986964, -0.4724409448818899238, -0.07217847769028870597 ) ) ;
#16960 = CARTESIAN_POINT ( 'NONE',  ( 4.837279021331060870E-17, -0.3949938075777409963, -2.755905511811023167 ) ) ;
#16961 = ORIENTED_EDGE ( 'NONE', *, *, #22393, .T. ) ;
#16962 = CARTESIAN_POINT ( 'NONE',  ( 0.3215223097112867578, -0.2845877964562161244, -0.3641732283464567121 ) ) ;
#16963 = CARTESIAN_POINT ( 'NONE',  ( 4.797336870675656522E-17, -0.3917322834645670104, -0.8582677165354329896 ) ) ;
#16964 = CARTESIAN_POINT ( 'NONE',  ( 1.213910761154856299, -0.6692913385826773087, -0.1292274648535924053 ) ) ;
#16965 = CARTESIAN_POINT ( 'NONE',  ( 5.785732909357575061E-17, -0.4724409448818898682, -2.598425196850393970 ) ) ;
#16966 = CARTESIAN_POINT ( 'NONE',  ( -1.220472440944881054, 0.2952755905511811885, 0.000000000000000000 ) ) ;
#16967 = SURFACE_SIDE_STYLE ('',( #43419 ) ) ;
#16968 = CARTESIAN_POINT ( 'NONE',  ( 1.463254593175853824, -0.6692913385826771977, 0.1292274648535927661 ) ) ;
#16969 = CARTESIAN_POINT ( 'NONE',  ( 1.404199475065617264, -0.3690944881889763329, 0.3153832671262228327 ) ) ;
#16970 = CARTESIAN_POINT ( 'NONE',  ( 0.6036745406824154392, 0.2306618581243847221, -0.2411417322834647770 ) ) ;
#16971 = CARTESIAN_POINT ( 'NONE',  ( -0.2867679344610364334, -0.2867679344610368219, -0.4540489256879772784 ) ) ;
#16972 = CARTESIAN_POINT ( 'NONE',  ( -0.07874015748031421014, -0.1870078740157479769, 0.4822834645669291653 ) ) ;
#16973 = CARTESIAN_POINT ( 'NONE',  ( -0.8398950131233589023, -0.5023911411419708095, -0.1820866141732282451 ) ) ;
#16974 = CARTESIAN_POINT ( 'NONE',  ( 0.3871391076115492380, -0.05778040916215560624, -0.4822834645669293319 ) ) ;
#16975 = CARTESIAN_POINT ( 'NONE',  ( 0.09186351706036799403, -0.4281496062992127816, -0.4176697321401328100 ) ) ;
#16976 = CARTESIAN_POINT ( 'NONE',  ( 0.4177787735907000366, 0.3937007874015747699, -1.559171609364239375 ) ) ;
#16977 = CARTESIAN_POINT ( 'NONE',  ( -0.01109768429471590621, 1.490381362800744269E-15, -0.3954974714151453519 ) ) ;
#16978 = CARTESIAN_POINT ( 'NONE',  ( -0.3917322834645671770, 0.1049643490035302024, -1.761830339403886336 ) ) ;
#16979 = CARTESIAN_POINT ( 'NONE',  ( 0.6955380577427828781, -0.4281496062992124485, 0.4176697321401328655 ) ) ;
#16980 = CARTESIAN_POINT ( 'NONE',  ( -0.2296587926509179312, -0.3162353388693409650, -0.4822834645669289433 ) ) ;
#16981 = CARTESIAN_POINT ( 'NONE',  ( -1.541994750656167090, -0.6692913385826773087, -0.1292274648535924053 ) ) ;
#16982 = CARTESIAN_POINT ( 'NONE',  ( 1.010498687664042716, 0.05413385826771626580, -0.4176697321401330321 ) ) ;
#16983 = CARTESIAN_POINT ( 'NONE',  ( 0.5183727034120741983, -0.6692913385826771977, 0.1292274648535927661 ) ) ;
#16984 = CARTESIAN_POINT ( 'NONE',  ( 0.3392501089628018329, 0.1958661417322835607, -1.160761154855643129 ) ) ;
#16985 = CARTESIAN_POINT ( 'NONE',  ( -0.4068241469816267775, 0.05413385826771626580, -0.4176697321401330321 ) ) ;
#16986 = CARTESIAN_POINT ( 'NONE',  ( 0.1312335958005257930, 0.2306618581243847221, -0.2411417322834647770 ) ) ;
#16987 = CARTESIAN_POINT ( 'NONE',  ( -0.5052493438320203589, 0.2952755905511810774, -0.1292274648535930714 ) ) ;
#16988 = CARTESIAN_POINT ( 'NONE',  ( 0.4527559055118117182, 0.07958543189024071263, -0.2665933059059888421 ) ) ;
#16989 = CARTESIAN_POINT ( 'NONE',  ( 1.614173228346457378, -0.5511811023622047445, 6.969142054262312111E-17 ) ) ;
#16990 = CARTESIAN_POINT ( 'NONE',  ( -1.725721784776902190, -0.05778040916215522460, 0.4822834645669289988 ) ) ;
#16991 = CARTESIAN_POINT ( 'NONE',  ( 0.4330708661417329575, -0.6692913385826771977, 8.415575281601705876E-17 ) ) ;
#16992 = CARTESIAN_POINT ( 'NONE',  ( 1.463254593175853824, 0.2952755905511810774, -0.1292274648535930714 ) ) ;
#16993 = CARTESIAN_POINT ( 'NONE',  ( -9.594673741351313045E-17, 0.3917322834645670104, -2.196850393700787496 ) ) ;
#16994 = ORIENTED_EDGE ( 'NONE', *, *, #49705, .T. ) ;
#16995 = ORIENTED_EDGE ( 'NONE', *, *, #79349, .F. ) ;
#16996 = AXIS2_PLACEMENT_3D ( 'NONE', #59951, #53625, #73003 ) ;
#16997 = CARTESIAN_POINT ( 'NONE',  ( 0.7152230971128616943, -0.05778040916215522460, 0.4822834645669289988 ) ) ;
#16998 = CARTESIAN_POINT ( 'NONE',  ( 0.1902887139107617975, 0.1771653543307087630, 0.09757992244046791164 ) ) ;
#16999 = VECTOR ( 'NONE', #15063, 39.37007874015748143 ) ;
#17000 = CIRCLE ( 'NONE', #27731, 3.937007874015748143 ) ;
#17002 = DIRECTION ( 'NONE',  ( -3.096699300667737957E-16, 1.000000000000000000, -0.000000000000000000 ) ) ;
#17001 = CARTESIAN_POINT ( 'NONE',  ( 1.660104986876641320, -0.08942795157527998196, 0.3641732283464567121 ) ) ;
#17003 = CARTESIAN_POINT ( 'NONE',  ( -0.2867679344610365999, 0.2867679344610364889, -0.8917322834645667884 ) ) ;
#17004 = FACE_OUTER_BOUND ( 'NONE', #37860, .T. ) ;
#17005 = CARTESIAN_POINT ( 'NONE',  ( 0.000000000000000000, 0.000000000000000000, 0.1574803149606299191 ) ) ;
#17006 = CARTESIAN_POINT ( 'NONE',  ( -0.3460692066303957537, -0.1998031496062994405, -2.333989501312335957 ) ) ;
#17007 = CARTESIAN_POINT ( 'NONE',  ( 0.7217847769028878924, -0.4281496062992127816, -0.4176697321401328100 ) ) ;
#17008 = CARTESIAN_POINT ( 'NONE',  ( -0.8070866141732276899, 0.1660481256975883668, -0.3530559997133364547 ) ) ;
#17009 = CARTESIAN_POINT ( 'NONE',  ( -0.7939632545931754048, -0.3162353388693405765, 0.4822834645669290543 ) ) ;
#17010 = CARTESIAN_POINT ( 'NONE',  ( 0.7742782152230978099, -0.4281496062992124485, 0.4176697321401328655 ) ) ;
#17011 = CARTESIAN_POINT ( 'NONE',  ( 1.194225721784777594, -0.4281496062992127816, -0.4176697321401328100 ) ) ;
#17012 = CARTESIAN_POINT ( 'NONE',  ( -1.038160555197627399, 1.326112492113292518, 0.4258879071893178492 ) ) ;
#17013 = ITEM_DEFINED_TRANSFORMATION ( 'NONE', 'NONE', #75935,  #22098 ) ;
#17014 = CARTESIAN_POINT ( 'NONE',  ( 1.246719160104987623, -0.004921259842519870586, -0.3153832671262229437 ) ) ;
#17015 = CARTESIAN_POINT ( 'NONE',  ( -1.003937007874014853, 0.1660481256975885056, 0.3530559997133364547 ) ) ;
#17016 = CARTESIAN_POINT ( 'NONE',  ( 1.614173228346457378, -0.6692913385826771977, 8.415575281601705876E-17 ) ) ;
#17017 = CARTESIAN_POINT ( 'NONE',  ( -0.2867679344610364334, -0.2867679344610367109, 0.1062992125984252439 ) ) ;
#17018 = CARTESIAN_POINT ( 'NONE',  ( 0.03937007874015833325, -0.6692913385826771977, 8.415575281601705876E-17 ) ) ;
#17019 = VECTOR ( 'NONE', #33452, 39.37007874015748143 ) ;
#17021 = CARTESIAN_POINT ( 'NONE',  ( 0.4687358108553574265, 1.787282772535975672, -0.5180085934481405419 ) ) ;
#17020 = CARTESIAN_POINT ( 'NONE',  ( 1.049868766404200349, 0.2306618581243848609, 0.2411417322834645549 ) ) ;
#17022 = CARTESIAN_POINT ( 'NONE',  ( -1.305774278215222184, -0.5511811023622048555, -0.09757992244046775898 ) ) ;
#17023 = CARTESIAN_POINT ( 'NONE',  ( 0.3674540682414705883, -0.6046776061558807314, 0.2411417322834647770 ) ) ;
#17024 = CARTESIAN_POINT ( 'NONE',  ( 1.220472440944882386, -0.5511811023622047445, 6.969142054262312111E-17 ) ) ;
#17025 = CARTESIAN_POINT ( 'NONE',  ( -0.1958661417322836440, 0.3392501089628016664, -1.510479371882202937 ) ) ;
#17026 = CARTESIAN_POINT ( 'NONE',  ( -1.141732283464566011, -0.5511811023622047445, 6.969142054262312111E-17 ) ) ;
#17027 = CARTESIAN_POINT ( 'NONE',  ( 1.469816272965879911, -0.6046776061558807314, 0.2411417322834647770 ) ) ;
#17028 = CARTESIAN_POINT ( 'NONE',  ( 0.2320225394537987207, 1.899862155193571711, 0.2105147107788077343 ) ) ;
#17029 = CARTESIAN_POINT ( 'NONE',  ( -0.06561679790026180015, -0.3690944881889765550, -0.3153832671262227771 ) ) ;
#17030 = CARTESIAN_POINT ( 'NONE',  ( -0.1902887139107604098, -0.6692913385826771977, 0.1292274648535927661 ) ) ;
#17031 = CARTESIAN_POINT ( 'NONE',  ( -1.286089238845143479, 0.1283753931104746893, -0.1820866141732285504 ) ) ;
#17032 = CARTESIAN_POINT ( 'NONE',  ( -0.9186351706036736120, 0.2306618581243848609, 0.2411417322834645549 ) ) ;
#17033 = CARTESIAN_POINT ( 'NONE',  ( 1.509186351706037543, 0.05413385826771666132, 0.4176697321401328100 ) ) ;
#17034 = CARTESIAN_POINT ( 'NONE',  ( 0.3917322834645670104, 0.1049643490035304660, -0.5938513367792144226 ) ) ;
#17035 = CARTESIAN_POINT ( 'NONE',  ( 0.4256376116915605023, 1.327230063460893783, -1.689708071488565500 ) ) ;
#17036 = CARTESIAN_POINT ( 'NONE',  ( 1.207349081364829990, -0.6046776061558809534, -0.2411417322834644161 ) ) ;
#17037 = CARTESIAN_POINT ( 'NONE',  ( -0.3458507752293906723, -0.3458507752293910609, -2.183070866141731958 ) ) ;
#17038 = CARTESIAN_POINT ( 'NONE',  ( -1.299212598425196097, -0.6692913385826771977, 8.415575281601705876E-17 ) ) ;
#17039 = CARTESIAN_POINT ( 'NONE',  ( -1.062992125984250968, -0.5511811023622047445, 6.969142054262312111E-17 ) ) ;
#17040 = CARTESIAN_POINT ( 'NONE',  ( -0.7677165354330699465, 0.07958543189024085140, 0.2665933059059887866 ) ) ;
#17041 = LINE ( 'NONE', #55306, #12441 ) ;
#17042 = CARTESIAN_POINT ( 'NONE',  ( -0.1443569553805765515, -0.4281496062992127816, -0.4176697321401328100 ) ) ;
#17043 = CARTESIAN_POINT ( 'NONE',  ( -0.1049868766404193215, -0.5023911411419708095, 0.1820866141732285504 ) ) ;
#17044 = CARTESIAN_POINT ( 'NONE',  ( -0.9514435695538050464, -0.2845877964562159024, 0.3641732283464567677 ) ) ;
#17045 = CARTESIAN_POINT ( 'NONE',  ( -1.660104986876639543, -0.05778040916215560624, -0.4822834645669293319 ) ) ;
#17046 = CARTESIAN_POINT ( 'NONE',  ( 1.509186351706037543, -0.3690944881889765550, -0.3153832671262227771 ) ) ;
#17047 = CARTESIAN_POINT ( 'NONE',  ( 1.332020997375329197, -0.3162353388693405765, 0.4822834645669290543 ) ) ;
#17048 = CARTESIAN_POINT ( 'NONE',  ( 0.1656158939409557440, 1.092528437896314486, 1.877649196272271226 ) ) ;
#17049 = CARTESIAN_POINT ( 'NONE',  ( 0.4068241469816281097, -0.004921259842519576551, 0.3153832671262227771 ) ) ;
#17050 = CARTESIAN_POINT ( 'NONE',  ( 0.8727034120734913358, -0.05778040916215522460, 0.4822834645669289988 ) ) ;
#17051 = CARTESIAN_POINT ( 'NONE',  ( 1.082677165354331228, -0.4536011799217367080, 0.2665933059059888421 ) ) ;
#17052 = ORIENTED_EDGE ( 'NONE', *, *, #672, .T. ) ;
#17053 = CARTESIAN_POINT ( 'NONE',  ( -1.043307086614172041, -0.5400638737290844871, 0.3530559997133364547 ) ) ;
#17054 = EDGE_CURVE ( 'NONE', #5751, #65743, #75230, .T. ) ;
#17055 = CARTESIAN_POINT ( 'NONE',  ( -1.049868766404198794, -0.6046776061558807314, 0.2411417322834647770 ) ) ;
#17056 = CARTESIAN_POINT ( 'NONE',  ( 0.006561679790026889343, -0.05778040916215522460, 0.4822834645669289988 ) ) ;
#17057 = AXIS2_PLACEMENT_3D ( 'NONE', #60684, #21555, #3034 ) ;
#17058 = CARTESIAN_POINT ( 'NONE',  ( -2.129998074986464207, 1.668416680336017421, -0.4562095852119731343 ) ) ;
#17059 = CARTESIAN_POINT ( 'NONE',  ( -0.3996062992125986590, 0.1070741851644051723, -2.156824146981627166 ) ) ;
#17060 = CARTESIAN_POINT ( 'NONE',  ( 1.030183727034121421, -0.3162353388693409650, -0.4822834645669289433 ) ) ;
#17061 = CARTESIAN_POINT ( 'NONE',  ( 1.410761154855643795, -0.2845877964562159024, 0.3641732283464567677 ) ) ;
#17062 = AXIS2_PLACEMENT_3D ( 'NONE', #12458, #26322, #18374 ) ;
#17063 = VECTOR ( 'NONE', #41062, 39.37007874015748143 ) ;
#17064 = CARTESIAN_POINT ( 'NONE',  ( -0.03937007874015669567, 0.2952755905511811885, 0.000000000000000000 ) ) ;
#17065 = CARTESIAN_POINT ( 'NONE',  ( 0.8005249343832027131, 0.05413385826771666132, 0.4176697321401328100 ) ) ;
#17066 = CARTESIAN_POINT ( 'NONE',  ( -0.1998031496062994683, 0.3460692066303958092, -1.745406824146981561 ) ) ;
#17067 = CARTESIAN_POINT ( 'NONE',  ( -0.1974969037888703871, -0.3420746716998661063, -1.010498687664042050 ) ) ;
#17068 = CARTESIAN_POINT ( 'NONE',  ( 0.1070741851644054915, -0.3996062992125986035, -2.290026246719159442 ) ) ;
#17069 = CARTESIAN_POINT ( 'NONE',  ( 0.4177787735907000366, 0.3937007874015748254, -1.559171609364239375 ) ) ;
#17070 = CARTESIAN_POINT ( 'NONE',  ( 0.1958661417322834775, 0.3392501089628018884, -0.6089238845144356871 ) ) ;
#17071 = CARTESIAN_POINT ( 'NONE',  ( -0.5971128608923877978, 0.1771653543307087630, 0.09757992244046791164 ) ) ;
#17072 = CARTESIAN_POINT ( 'NONE',  ( -0.6889763779527552368, -0.5400638737290845981, -0.3530559997133363437 ) ) ;
#17073 = CARTESIAN_POINT ( 'NONE',  ( 0.4199475065616803948, -0.6046776061558809534, -0.2411417322834644161 ) ) ;
#17074 = CARTESIAN_POINT ( 'NONE',  ( -0.2891555358219909388, -0.2891555358219912164, -2.340551181102362488 ) ) ;
#17075 = CARTESIAN_POINT ( 'NONE',  ( 1.594488188976378673, 0.1660481256975885056, 0.3530559997133364547 ) ) ;
#17076 = CARTESIAN_POINT ( 'NONE',  ( 1.318897637795276356, 0.1660481256975883668, -0.3530559997133364547 ) ) ;
#17077 = CARTESIAN_POINT ( 'NONE',  ( 0.2362204724409451007, -0.4091458600556402980, -2.454068241469816058 ) ) ;
#17078 = CARTESIAN_POINT ( 'NONE',  ( 4.893765752498283924E-17, -0.3996062992125986035, -1.653543307086614123 ) ) ;
#17079 = DIRECTION ( 'NONE',  ( -0.000000000000000000, -1.000000000000000000, -0.000000000000000000 ) ) ;
#17080 = CARTESIAN_POINT ( 'NONE',  ( 1.128608923884514947, 0.2306618581243848609, 0.2411417322834645549 ) ) ;
#17081 = CARTESIAN_POINT ( 'NONE',  ( 1.227034120734908917, -0.5511811023622046335, 0.09757992244046803654 ) ) ;
#17083 = CARTESIAN_POINT ( 'NONE',  ( -1.541994750656167090, -0.6692913385826773087, -0.1292274648535924053 ) ) ;
#17082 = CARTESIAN_POINT ( 'NONE',  ( 1.574803149606299746, -0.1870078740157480879, -0.4822834645669291653 ) ) ;
#17084 = CARTESIAN_POINT ( 'NONE',  ( 0.2867679344610365999, 0.2867679344610365999, -2.737513492617110522 ) ) ;
#17085 = FILL_AREA_STYLE ('',( #74737 ) ) ;
#17086 = CARTESIAN_POINT ( 'NONE',  ( 0.9711286089238851948, -0.6046776061558809534, -0.2411417322834644161 ) ) ;
#17087 = CARTESIAN_POINT ( 'NONE',  ( 1.607611548556431069, -0.5511811023622048555, -0.09757992244046775898 ) ) ;
#17088 = CARTESIAN_POINT ( 'NONE',  ( -0.6692913385826764205, -0.6692913385826771977, 8.415575281601705876E-17 ) ) ;
#17089 = CARTESIAN_POINT ( 'NONE',  ( -0.5905511811023615998, 0.2952755905511811885, 0.000000000000000000 ) ) ;
#17090 = EDGE_CURVE ( 'NONE', #70570, #16375, #21174, .T. ) ;
#17091 = CARTESIAN_POINT ( 'NONE',  ( -1.607611548556429737, 0.2952755905511810774, -0.1292274648535930714 ) ) ;
#17092 = B_SPLINE_CURVE_WITH_KNOTS ( 'NONE', 3,
 ( #78498, #14526, #66272, #60774 ),
 .UNSPECIFIED., .F., .F.,
 ( 4, 4 ),
 ( 3.593986969197074577E-07, 0.001287825409103162408 ),
 .UNSPECIFIED. ) ;
#17093 = CARTESIAN_POINT ( 'NONE',  ( 0.2867679344610365999, -0.2867679344610365444, -0.1830708661417323746 ) ) ;
#17094 = CARTESIAN_POINT ( 'NONE',  ( 0.03280839895013198948, 0.2952755905511811885, 0.1292274648535926551 ) ) ;
#17095 = CARTESIAN_POINT ( 'NONE',  ( 0.1049643490035304938, -0.3917322834645669549, -2.282152230971128404 ) ) ;
#17096 = CARTESIAN_POINT ( 'NONE',  ( 1.594488188976378673, -0.5400638737290845981, -0.3530559997133363437 ) ) ;
#17097 = VERTEX_POINT ( 'NONE', #59052 ) ;
#17098 = CARTESIAN_POINT ( 'NONE',  ( -0.2891555358219911054, 0.2891555358219909388, -2.696850393700787496 ) ) ;
#17099 = EDGE_LOOP ( 'NONE', ( #61475, #11680, #31244, #67774 ) ) ;
#17100 = CARTESIAN_POINT ( 'NONE',  ( -0.06596743314205839870, 0.004960608223778821026, 0.3437734562760189072 ) ) ;
#17101 = CARTESIAN_POINT ( 'NONE',  ( -1.351706036745406347, 0.05413385826771626580, -0.4176697321401330321 ) ) ;
#17102 = CARTESIAN_POINT ( 'NONE',  ( -0.3996062992125987146, 0.1070741851644051862, -0.8202099737532806412 ) ) ;
#17103 = FACE_OUTER_BOUND ( 'NONE', #28662, .T. ) ;
#17104 = CARTESIAN_POINT ( 'NONE',  ( -0.7137454485294959516, 2.001539355558159983, 0.4917280318828578523 ) ) ;
#17105 = DIRECTION ( 'NONE',  ( 0.000000000000000000, 0.000000000000000000, 1.000000000000000000 ) ) ;
#17106 = CARTESIAN_POINT ( 'NONE',  ( -0.2867050620510094849, 1.825346416092846091, 0.1260848743807634342 ) ) ;
#17107 = CARTESIAN_POINT ( 'NONE',  ( -0.1958661417322836718, 0.3392501089628017219, -0.5702099737532808632 ) ) ;
#17108 =( BOUNDED_SURFACE ( )  B_SPLINE_SURFACE ( 1, 2, ( 
 ( #49782, #23702, #49373, #36742, #50598, #75069, #17417, #68743, #11085, #4756, #30432, #56097, #75889, #69154, #5177, #50192, #81802, #24113, #69568, #75482, #24526, #82208, #17823, #11505, #37161, #18230, #11916, #37570, #63244, #5584, #82612, #24929, #76306, #18635, #44279, #69969, #61600, #3946, #55266, #23289, #48959, #74660, #70812, #13162, #39654, #59013, #70381, #38395, #45948, #38813, #12736, #32922, #105, #45107, #19038, #58588, #33350, #26611, #52681, #956, #78389, #46371, #32082, #529, #64490, #63656, #77551, #57327, #83021, #25344, #71646, #64075, #7250, #64913, #6828, #77123, #19883, #27020, #13997, #72065, #51006, #76705, #26182, #51421, #52263, #37981, #45532, #19456, #77969, #32497, #6412, #20720, #5995, #20299, #65345, #57743, #44685, #25759, #58161, #31666, #51844, #71230, #13574, #39228, #7682, #1368, #54348, #65762, #61084, #28687, #34598, #73739, #67413, #8095, #2612, #33759, #28269, #66169, #22377, #80473, #21136, #21543, #22785, #34175, #79227, #41323, #47204, #3435, #35007, #46791, #53097, #60672, #40075, #3020, #9747, #59421, #29097, #67004, #1777, #48037, #16074, #41720, #54769, #59839, #9336, #35419, #40491, #15244, #48445, #14424, #15662, #80059, #8509, #27435, #78807, #72482, #14831, #2192, #27860, #73315, #53520, #72894, #40904, #66585, #8921, #60263, #53931, #47619, #79643, #21960, #55170, #23604, #49684, #10982, #74145, #48862, #29509, #10170, #24830, #23191, #50093, #3849, #36240, #56411, #10583, #80879, #69053, #69469, #30748, #24016, #55994, #63147, #62743, #36642, #43764, #18131, #82110, #74562, #24423, #75376, #30328, #81706, #16908, #55578, #42546, #68249, #61910, #16490, #75789, #4655, #81288, #4252, #11822, #17725, #49273, #43351, #37474, #5488, #35835, #61502, #31149, #56815, #82514, #42136, #37059, #29914, #74976, #17321, #11402, #42949, #68643, #62318, #5079, #67831, #38295, #33251, #76611, #82925, #19778, #1272, #57224, #58487, #44183, #6727, #39552, #45432, #426, #13893, #71127, #51322, #70707, #71546, #25660, #45007, #64391, #13470, #58913, #7147, #20196, #32397, #50499, #18941, #38713, #5894, #25246, #77025, #65241, #31566, #50910, #44589, #70283, #12636, #63972, #6308, #64808, #58060, #51742, #39127, #31985, #57645, #32820, #13059, #852, #77445, #8, #19358, #26082, #26509, #52163, #77867, #45847, #7579, #76202, #18540, #69875, #12228, #37885, #63560, #65670, #52996, #79963, #28172, #28590, #20620, #59738, #2092, #54246, #47936, #59323, #27336, #34912, #27757, #1679, #21856, #72386, #34074, #7996, #47520, #22276, #15562, #41628, #73212, #67317, #35321, #21033, #72793, #53421, #52580, #66484, #46272, #71967, #14322, #60575, #78709, #79543, #53829, #79130, #66071, #8819, #15981, #2926, #60984, #39980, #33660, #15143, #40388, #41222, #26920, #34496, #8407, #66909, #21447, #46693, #9652, #78289, #9240, #47104, #14736, #73639, #40799, #60161, #2513, #49592, #43674, #11730, #80780, #49177, #61816, #28998, #42857, #22688, #48347, #74044, #36968, #29413, #55900, #30236, #4156, #42446, #68550, #75699, #62647, #37386, #16391, #42038, #74881, #16809, #81611, #3334, #10891, #68145, #43262, #10490, #61400, #69377, #54664, #23926, #75287, #23096, #67732, #48763, #29821, #80375, #74462, #10067, #55072, #35730, #17630, #3749, #36144, #11309, #55483, #36551, #18040, #68959, #62227, #50002, #4989, #81192, #23509, #24332, #17225, #4565, #30656, #56320, #82018, #19675, #32719, #76925, #63057, #5800, #51227, #18451, #37789, #38198, #52062, #44093, #63466, #31470, #57132, #12132, #69787, #82829, #77344, #44905, #64293, #51639, #25151, #50819, #45334, #25560, #25981, #6627, #76520, #18849, #44495, #71029, #19253, #70603, #70186, #39026, #12539, #31888, #63873, #32299, #6212, #57959, #57548, #83239, #58386, #327, #64710, #56726, #12958, #38615 ),
 ( #13373, #7050, #747, #26408, #77768, #20100, #45751, #71446, #13794, #5395, #31057, #82423, #24742, #50410, #76110, #1583, #2413, #79030, #1992, #65565, #15461, #20933, #8308, #40290, #66384, #46592, #34392, #78189, #7899, #9143, #40699, #41119, #33146, #72288, #14634, #66810, #60473, #71868, #39878, #47419, #65971, #14218, #60060, #27238, #33975, #20520, #28071, #34814, #53729, #54145, #79437, #79859, #47834, #33560, #27655, #59636, #65139, #21349, #58815, #1172, #26823, #73110, #59222, #8721, #21756, #53320, #78610, #47002, #28485, #2824, #73540, #52481, #46172, #72696, #52897, #22176, #39451, #15043, #7475, #56929, #81813, #75080, #57340, #15884, #43882, #69580, #36755, #4359, #62430, #75495, #25359, #4768, #83035, #43058, #49385, #11927, #51022, #23714, #24939, #9551, #56517, #6010, #37582, #50204, #63669, #63255, #17834, #37172, #37993, #43468, #11516, #30853, #5596, #41532, #82625, #69982, #82220, #67218, #68755, #5188, #55690, #17427, #69165, #31680, #11097, #62852, #35221, #81398, #30443, #56108, #24124, #49793, #24539, #75901, #31262, #18241, #50610, #76317, #18647, #44291, #12337, #60885, #30027, #20314, #120, #19472, #38827, #39670, #32938, #39245, #45122, #52697, #58176, #45548, #77566, #45965, #545, #71662, #32097, #70830, #46387, #77985, #78405, #70397, #26198, #51859, #20736, #14439, #25775, #77139, #1383, #19900, #51436, #14013, #64505, #71245, #57758, #65360, #72080, #7698, #8110, #33365, #33776, #1792, #13178, #64928, #13589, #19053, #58603, #12753, #38410, #64092, #27036, #6844, #59028, #40091, #7266, #32514, #972, #65778, #59439, #27452, #6428, #26626, #52280, #76721, #44700, #61520, #9352, #34613, #9763, #60278, #27875, #10186, #53113, #80076, #22394, #72909, #40506, #15261, #28284, #3866, #40921, #35851, #79243, #2207, #48053, #78822, #59855, #61099, #46806, #35023, #42152, #73754, #3037, #16509, #16090, #53946, #73332, #74161, #79659, #47637, #67019, #41735, #21151, #35434, #22803, #60687, #72497, #21558, #41339, #8524, #3450, #14846, #28702, #67847, #67429, #54364, #66188, #29114, #21975, #15678, #34191, #54785, #80488, #48461, #53535, #47220, #66602, #8935, #2628, #29525, #55594, #17741, #68265, #4269, #4671, #18552, #10601, #29931, #81306, #23620, #61927, #36258, #49289, #43780, #11419, #30763, #18146, #74992, #17337, #11835, #75395, #75804, #56425, #42967, #68662, #11000, #69483, #69069, #43369, #36659, #5501, #62334, #81721, #30344, #82125, #56010, #24440, #24030, #49699, #82528, #50108, #31163, #23208, #37074, #62760, #56830, #50512, #5095, #37488, #63163, #24845, #76217, #44197, #69887, #12241, #37897, #63573, #55187, #80895, #48879, #74579, #16924, #42561, #20, #51755, #64404, #31581, #45445, #25259, #50923, #76623, #39566, #31998, #58501, #32833, #6740, #45020, #71141, #78302, #65255, #39993, #18954, #44601, #77458, #19370, #865, #14335, #13483, #70720, #45861, #13073, #63985, #46285, #5908, #26522, #52177, #25674, #70296, #51334, #32411, #57236, #77038, #71981, #57658, #38310, #77880, #82938, #12649, #38727, #6322, #58074, #440, #20211, #71559, #26095, #19794, #39140, #64822, #7162, #13908, #7592, #33264, #58926, #1285, #26934, #52595, #20634, #33674, #34509, #73651, #73225, #28185, #47949, #47534, #21460, #40813, #22288, #47118, #15156, #60172, #15576, #67331, #9253, #54259, #2527, #65683, #66084, #53843, #21047, #14749, #72807, #15993, #46706, #40403, #8420, #34088, #72400, #59751, #2105, #34925, #79556, #21869, #41234, #27770, #53435, #60588, #8832, #66921, #2938, #79143, #66498, #28602, #79975, #41640, #9664, #8010, #59336, #1693, #27351, #53009, #78722, #38986, #52436, #12917, #285, #27195, #58767, #59183, #51185, #7008, #32676, #1540, #78569, #6589, #57921, #65523, #58342, #32260, #78146, #19632, #76883, #20895, #14595 ) ),
 .UNSPECIFIED., .F., .F., .F. ) 
 B_SPLINE_SURFACE_WITH_KNOTS ( ( 2, 2 ),
 ( 3, 2, 2, 2, 2, 2, 2, 2, 2, 2, 2, 2, 2, 2, 2, 2, 2, 2, 2, 2, 2, 2, 2, 2, 2, 2, 2, 2, 2, 2, 2, 2, 2, 2, 2, 2, 2, 2, 2, 2, 2, 2, 2, 2, 2, 2, 2, 2, 2, 2, 2, 2, 2, 2, 2, 2, 2, 2, 2, 2, 2, 2, 2, 2, 2, 2, 2, 2, 2, 2, 2, 2, 2, 2, 2, 2, 2, 2, 2, 2, 2, 2, 2, 2, 2, 2, 2, 2, 2, 2, 2, 2, 2, 2, 2, 2, 2, 2, 2, 2, 2, 2, 2, 2, 2, 2, 2, 2, 2, 2, 2, 2, 2, 2, 2, 2, 2, 2, 2, 2, 2, 2, 2, 2, 2, 2, 2, 2, 2, 2, 2, 2, 2, 2, 2, 2, 2, 2, 2, 2, 2, 2, 2, 2, 2, 2, 2, 2, 2, 2, 2, 2, 2, 2, 2, 2, 2, 2, 2, 2, 2, 2, 2, 2, 2, 2, 2, 2, 2, 2, 2, 2, 2, 2, 2, 2, 2, 2, 2, 2, 2, 2, 2, 2, 2, 2, 2, 2, 2, 2, 2, 2, 2, 2, 2, 2, 2, 2, 2, 2, 2, 2, 2, 2, 2, 2, 2, 2, 2, 2, 2, 2, 2, 2, 2, 2, 2, 2, 2, 2, 2, 2, 2, 2, 2, 2, 2, 2, 2, 2, 2, 2, 2, 2, 2, 2, 2, 3 ),
 ( 0.000000000000000000, 1.000000000000000000 ),
 ( 0.000000000000000000, 0.004166666666666666609, 0.008333333333333333218, 0.01250000000000000069, 0.01666666666666666644, 0.02083333333333333218, 0.02500000000000000139, 0.02916666666666666713, 0.03333333333333333287, 0.03749999999999999861, 0.04166666666666666435, 0.04583333333333333010, 0.05000000000000000278, 0.05416666666666666852, 0.05833333333333333426, 0.06250000000000000000, 0.06666666666666666574, 0.07083333333333333148, 0.07499999999999999722, 0.07916666666666666297, 0.08333333333333332871, 0.08749999999999999445, 0.09166666666666666019, 0.09583333333333333981, 0.1000000000000000056, 0.1041666666666666713, 0.1083333333333333370, 0.1125000000000000028, 0.1166666666666666685, 0.1208333333333333343, 0.1250000000000000000, 0.1291666666666666796, 0.1333333333333333315, 0.1375000000000000111, 0.1416666666666666630, 0.1458333333333333426, 0.1499999999999999944, 0.1541666666666666741, 0.1583333333333333259, 0.1625000000000000056, 0.1666666666666666574, 0.1708333333333333370, 0.1749999999999999889, 0.1791666666666666685, 0.1833333333333333204, 0.1875000000000000000, 0.1916666666666666796, 0.1958333333333333315, 0.2000000000000000111, 0.2041666666666666630, 0.2083333333333333426, 0.2124999999999999944, 0.2166666666666666741, 0.2208333333333333259, 0.2250000000000000056, 0.2291666666666666574, 0.2333333333333333370, 0.2374999999999999889, 0.2416666666666666685, 0.2458333333333333204, 0.2500000000000000000, 0.2541666666666666519, 0.2583333333333333592, 0.2625000000000000111, 0.2666666666666666630, 0.2708333333333333148, 0.2750000000000000222, 0.2791666666666666741, 0.2833333333333333259, 0.2874999999999999778, 0.2916666666666666852, 0.2958333333333333370, 0.2999999999999999889, 0.3041666666666666408, 0.3083333333333333481, 0.3125000000000000000, 0.3166666666666666519, 0.3208333333333333592, 0.3250000000000000111, 0.3291666666666666630, 0.3333333333333333148, 0.3375000000000000222, 0.3416666666666666741, 0.3458333333333333259, 0.3499999999999999778, 0.3541666666666666852, 0.3583333333333333370, 0.3624999999999999889, 0.3666666666666666408, 0.3708333333333333481, 0.3750000000000000000, 0.3791666666666666519, 0.3833333333333333592, 0.3875000000000000111, 0.3916666666666666630, 0.3958333333333333148, 0.4000000000000000222, 0.4041666666666666741, 0.4083333333333333259, 0.4124999999999999778, 0.4166666666666666852, 0.4208333333333333370, 0.4249999999999999889, 0.4291666666666666408, 0.4333333333333333481, 0.4375000000000000000, 0.4416666666666666519, 0.4458333333333333592, 0.4500000000000000111, 0.4541666666666666630, 0.4583333333333333148, 0.4625000000000000222, 0.4666666666666666741, 0.4708333333333333259, 0.4749999999999999778, 0.4791666666666666852, 0.4833333333333333370, 0.4874999999999999889, 0.4916666666666666408, 0.4958333333333333481, 0.5000000000000000000, 0.5041666666666666519, 0.5083333333333333037, 0.5124999999999999556, 0.5166666666666667185, 0.5208333333333333703, 0.5250000000000000222, 0.5291666666666666741, 0.5333333333333333259, 0.5374999999999999778, 0.5416666666666666297, 0.5458333333333332815, 0.5500000000000000444, 0.5541666666666666963, 0.5583333333333333481, 0.5625000000000000000, 0.5666666666666666519, 0.5708333333333333037, 0.5749999999999999556, 0.5791666666666667185, 0.5833333333333333703, 0.5875000000000000222, 0.5916666666666666741, 0.5958333333333333259, 0.5999999999999999778, 0.6041666666666666297, 0.6083333333333332815, 0.6125000000000000444, 0.6166666666666666963, 0.6208333333333333481, 0.6250000000000000000, 0.6291666666666666519, 0.6333333333333333037, 0.6374999999999999556, 0.6416666666666667185, 0.6458333333333333703, 0.6500000000000000222, 0.6541666666666666741, 0.6583333333333333259, 0.6624999999999999778, 0.6666666666666666297, 0.6708333333333332815, 0.6750000000000000444, 0.6791666666666666963, 0.6833333333333333481, 0.6875000000000000000, 0.6916666666666666519, 0.6958333333333333037, 0.6999999999999999556, 0.7041666666666667185, 0.7083333333333333703, 0.7125000000000000222, 0.7166666666666666741, 0.7208333333333333259, 0.7249999999999999778, 0.7291666666666666297, 0.7333333333333332815, 0.7375000000000000444, 0.7416666666666666963, 0.7458333333333333481, 0.7500000000000000000, 0.7541666666666666519, 0.7583333333333333037, 0.7624999999999999556, 0.7666666666666667185, 0.7708333333333333703, 0.7750000000000000222, 0.7791666666666666741, 0.7833333333333333259, 0.7874999999999999778, 0.7916666666666666297, 0.7958333333333332815, 0.8000000000000000444, 0.8041666666666666963, 0.8083333333333333481, 0.8125000000000000000, 0.8166666666666666519, 0.8208333333333333037, 0.8249999999999999556, 0.8291666666666667185, 0.8333333333333333703, 0.8375000000000000222, 0.8416666666666666741, 0.8458333333333333259, 0.8499999999999999778, 0.8541666666666666297, 0.8583333333333332815, 0.8625000000000000444, 0.8666666666666666963, 0.8708333333333333481, 0.8750000000000000000, 0.8791666666666666519, 0.8833333333333333037, 0.8874999999999999556, 0.8916666666666667185, 0.8958333333333333703, 0.9000000000000000222, 0.9041666666666666741, 0.9083333333333333259, 0.9124999999999999778, 0.9166666666666666297, 0.9208333333333332815, 0.9250000000000000444, 0.9291666666666666963, 0.9333333333333333481, 0.9375000000000000000, 0.9416666666666666519, 0.9458333333333333037, 0.9499999999999999556, 0.9541666666666667185, 0.9583333333333333703, 0.9625000000000000222, 0.9666666666666666741, 0.9708333333333333259, 0.9749999999999999778, 0.9791666666666666297, 0.9833333333333332815, 0.9875000000000000444 ),
 .UNSPECIFIED. ) 
 GEOMETRIC_REPRESENTATION_ITEM ( )  RATIONAL_B_SPLINE_SURFACE ( (
 ( 1.000000000000000000, 0.9659258262890683122, 1.000000000000000000, 0.9659258262890683122, 1.000000000000000000, 0.9659258262890683122, 1.000000000000000000, 0.9659258262890683122, 1.000000000000000000, 0.9659258262890683122, 1.000000000000000000, 0.9659258262890683122, 1.000000000000000000, 0.9659258262890683122, 1.000000000000000000, 0.9659258262890683122, 1.000000000000000000, 0.9659258262890683122, 1.000000000000000000, 0.9659258262890683122, 1.000000000000000000, 0.9659258262890683122, 1.000000000000000000, 0.9659258262890683122, 1.000000000000000000, 0.9659258262890683122, 1.000000000000000000, 0.9659258262890683122, 1.000000000000000000, 0.9659258262890683122, 1.000000000000000000, 0.9659258262890683122, 1.000000000000000000, 0.9659258262890683122, 1.000000000000000000, 0.9659258262890683122, 1.000000000000000000, 0.9659258262890683122, 1.000000000000000000, 0.9659258262890683122, 1.000000000000000000, 0.9659258262890683122, 1.000000000000000000, 0.9659258262890683122, 1.000000000000000000, 0.9659258262890683122, 1.000000000000000000, 0.9659258262890683122, 1.000000000000000000, 0.9659258262890683122, 1.000000000000000000, 0.9659258262890683122, 1.000000000000000000, 0.9659258262890683122, 1.000000000000000000, 0.9659258262890683122, 1.000000000000000000, 0.9659258262890683122, 1.000000000000000000, 0.9659258262890683122, 1.000000000000000000, 0.9659258262890683122, 1.000000000000000000, 0.9659258262890683122, 1.000000000000000000, 0.9659258262890683122, 1.000000000000000000, 0.9659258262890683122, 1.000000000000000000, 0.9659258262890683122, 1.000000000000000000, 0.9659258262890683122, 1.000000000000000000, 0.9659258262890683122, 1.000000000000000000, 0.9659258262890683122, 1.000000000000000000, 0.9659258262890683122, 1.000000000000000000, 0.9659258262890683122, 1.000000000000000000, 0.9659258262890683122, 1.000000000000000000, 0.9659258262890683122, 1.000000000000000000, 0.9659258262890683122, 1.000000000000000000, 0.9659258262890683122, 1.000000000000000000, 0.9659258262890683122, 1.000000000000000000, 0.9659258262890683122, 1.000000000000000000, 0.9659258262890683122, 1.000000000000000000, 0.9659258262890683122, 1.000000000000000000, 0.9659258262890683122, 1.000000000000000000, 0.9659258262890683122, 1.000000000000000000, 0.9659258262890683122, 1.000000000000000000, 0.9659258262890683122, 1.000000000000000000, 0.9659258262890683122, 1.000000000000000000, 0.9659258262890683122, 1.000000000000000000, 0.9659258262890683122, 1.000000000000000000, 0.9659258262890683122, 1.000000000000000000, 0.9659258262890683122, 1.000000000000000000, 0.9659258262890683122, 1.000000000000000000, 0.9659258262890683122, 1.000000000000000000, 0.9659258262890683122, 1.000000000000000000, 0.9659258262890683122, 1.000000000000000000, 0.9659258262890683122, 1.000000000000000000, 0.9659258262890683122, 1.000000000000000000, 0.9659258262890683122, 1.000000000000000000, 0.9659258262890683122, 1.000000000000000000, 0.9659258262890683122, 1.000000000000000000, 0.9659258262890683122, 1.000000000000000000, 0.9659258262890683122, 1.000000000000000000, 0.9659258262890683122, 1.000000000000000000, 0.9659258262890683122, 1.000000000000000000, 0.9659258262890683122, 1.000000000000000000, 0.9659258262890683122, 1.000000000000000000, 0.9659258262890683122, 1.000000000000000000, 0.9659258262890683122, 1.000000000000000000, 0.9659258262890683122, 1.000000000000000000, 0.9659258262890683122, 1.000000000000000000, 0.9659258262890683122, 1.000000000000000000, 0.9659258262890683122, 1.000000000000000000, 0.9659258262890683122, 1.000000000000000000, 0.9659258262890683122, 1.000000000000000000, 0.9659258262890683122, 1.000000000000000000, 0.9659258262890683122, 1.000000000000000000, 0.9659258262890683122, 1.000000000000000000, 0.9659258262890683122, 1.000000000000000000, 0.9659258262890683122, 1.000000000000000000, 0.9659258262890683122, 1.000000000000000000, 0.9659258262890683122, 1.000000000000000000, 0.9659258262890683122, 1.000000000000000000, 0.9659258262890683122, 1.000000000000000000, 0.9659258262890683122, 1.000000000000000000, 0.9659258262890683122, 1.000000000000000000, 0.9659258262890683122, 1.000000000000000000, 0.9659258262890683122, 1.000000000000000000, 0.9659258262890683122, 1.000000000000000000, 0.9659258262890683122, 1.000000000000000000, 0.9659258262890683122, 1.000000000000000000, 0.9659258262890683122, 1.000000000000000000, 0.9659258262890683122, 1.000000000000000000, 0.9659258262890683122, 1.000000000000000000, 0.9659258262890683122, 1.000000000000000000, 0.9659258262890683122, 1.000000000000000000, 0.9659258262890683122, 1.000000000000000000, 0.9659258262890683122, 1.000000000000000000, 0.9659258262890683122, 1.000000000000000000, 0.9659258262890683122, 1.000000000000000000, 0.9659258262890683122, 1.000000000000000000, 0.9659258262890683122, 1.000000000000000000, 0.9659258262890683122, 1.000000000000000000, 0.9659258262890683122, 1.000000000000000000, 0.9659258262890683122, 1.000000000000000000, 0.9659258262890683122, 1.000000000000000000, 0.9659258262890683122, 1.000000000000000000, 0.9659258262890683122, 1.000000000000000000, 0.9659258262890683122, 1.000000000000000000, 0.9659258262890683122, 1.000000000000000000, 0.9659258262890683122, 1.000000000000000000, 0.9659258262890683122, 1.000000000000000000, 0.9659258262890683122, 1.000000000000000000, 0.9659258262890683122, 1.000000000000000000, 0.9659258262890683122, 1.000000000000000000, 0.9659258262890683122, 1.000000000000000000, 0.9659258262890683122, 1.000000000000000000, 0.9659258262890683122, 1.000000000000000000, 0.9659258262890683122, 1.000000000000000000, 0.9659258262890683122, 1.000000000000000000, 0.9659258262890683122, 1.000000000000000000, 0.9659258262890683122, 1.000000000000000000, 0.9659258262890683122, 1.000000000000000000, 0.9659258262890683122, 1.000000000000000000, 0.9659258262890683122, 1.000000000000000000, 0.9659258262890683122, 1.000000000000000000, 0.9659258262890683122, 1.000000000000000000, 0.9659258262890683122, 1.000000000000000000, 0.9659258262890683122, 1.000000000000000000, 0.9659258262890683122, 1.000000000000000000, 0.9659258262890683122, 1.000000000000000000, 0.9659258262890683122, 1.000000000000000000, 0.9659258262890683122, 1.000000000000000000, 0.9659258262890683122, 1.000000000000000000, 0.9659258262890683122, 1.000000000000000000, 0.9659258262890683122, 1.000000000000000000, 0.9659258262890683122, 1.000000000000000000, 0.9659258262890683122, 1.000000000000000000, 0.9659258262890683122, 1.000000000000000000, 0.9659258262890683122, 1.000000000000000000, 0.9659258262890683122, 1.000000000000000000, 0.9659258262890683122, 1.000000000000000000, 0.9659258262890683122, 1.000000000000000000, 0.9659258262890683122, 1.000000000000000000, 0.9659258262890683122, 1.000000000000000000, 0.9659258262890683122, 1.000000000000000000, 0.9659258262890683122, 1.000000000000000000, 0.9659258262890683122, 1.000000000000000000, 0.9659258262890683122, 1.000000000000000000, 0.9659258262890683122, 1.000000000000000000, 0.9659258262890683122, 1.000000000000000000, 0.9659258262890683122, 1.000000000000000000, 0.9659258262890683122, 1.000000000000000000, 0.9659258262890683122, 1.000000000000000000, 0.9659258262890683122, 1.000000000000000000, 0.9659258262890683122, 1.000000000000000000, 0.9659258262890683122, 1.000000000000000000, 0.9659258262890683122, 1.000000000000000000, 0.9659258262890683122, 1.000000000000000000, 0.9659258262890683122, 1.000000000000000000, 0.9659258262890683122, 1.000000000000000000, 0.9659258262890683122, 1.000000000000000000, 0.9659258262890683122, 1.000000000000000000, 0.9659258262890683122, 1.000000000000000000, 0.9659258262890683122, 1.000000000000000000, 0.9659258262890683122, 1.000000000000000000, 0.9659258262890683122, 1.000000000000000000, 0.9659258262890683122, 1.000000000000000000, 0.9659258262890683122, 1.000000000000000000, 0.9659258262890683122, 1.000000000000000000, 0.9659258262890683122, 1.000000000000000000, 0.9659258262890683122, 1.000000000000000000, 0.9659258262890683122, 1.000000000000000000, 0.9659258262890683122, 1.000000000000000000, 0.9659258262890683122, 1.000000000000000000, 0.9659258262890683122, 1.000000000000000000, 0.9659258262890683122, 1.000000000000000000, 0.9659258262890683122, 1.000000000000000000, 0.9659258262890683122, 1.000000000000000000, 0.9659258262890683122, 1.000000000000000000, 0.9659258262890683122, 1.000000000000000000, 0.9659258262890683122, 1.000000000000000000, 0.9659258262890683122, 1.000000000000000000, 0.9659258262890683122, 1.000000000000000000, 0.9659258262890683122, 1.000000000000000000, 0.9659258262890683122, 1.000000000000000000, 0.9659258262890683122, 1.000000000000000000, 0.9659258262890683122, 1.000000000000000000, 0.9659258262890683122, 1.000000000000000000, 0.9659258262890683122, 1.000000000000000000, 0.9659258262890683122, 1.000000000000000000, 0.9659258262890683122, 1.000000000000000000, 0.9659258262890683122, 1.000000000000000000, 0.9659258262890683122, 1.000000000000000000, 0.9659258262890683122, 1.000000000000000000, 0.9659258262890683122, 1.000000000000000000, 0.9659258262890683122, 1.000000000000000000, 0.9659258262890683122, 1.000000000000000000, 0.9659258262890683122, 1.000000000000000000, 0.9659258262890683122, 1.000000000000000000, 0.9659258262890683122, 1.000000000000000000, 0.9659258262890683122, 1.000000000000000000, 0.9659258262890683122, 1.000000000000000000, 0.9659258262890683122, 1.000000000000000000, 0.9659258262890683122, 1.000000000000000000, 0.9659258262890683122, 1.000000000000000000, 0.9659258262890683122, 1.000000000000000000, 0.9659258262890683122, 1.000000000000000000, 0.9659258262890683122, 1.000000000000000000, 0.9659258262890683122, 1.000000000000000000, 0.9659258262890683122, 1.000000000000000000, 0.9659258262890683122, 1.000000000000000000, 0.9659258262890683122, 1.000000000000000000, 0.9659258262890683122, 1.000000000000000000, 0.9659258262890683122, 1.000000000000000000, 0.9659258262890683122, 1.000000000000000000, 0.9659258262890683122, 1.000000000000000000, 0.9659258262890683122, 1.000000000000000000, 0.9659258262890683122, 1.000000000000000000, 0.9659258262890683122, 1.000000000000000000, 0.9659258262890683122, 1.000000000000000000, 0.9659258262890683122, 1.000000000000000000, 0.9659258262890683122, 1.000000000000000000, 0.9659258262890683122, 1.000000000000000000, 0.9659258262890683122, 1.000000000000000000, 0.9659258262890683122, 1.000000000000000000, 0.9659258262890683122, 1.000000000000000000, 0.9659258262890683122, 1.000000000000000000, 0.9659258262890683122, 1.000000000000000000, 0.9659258262890683122, 1.000000000000000000, 0.9659258262890683122, 1.000000000000000000, 0.9659258262890683122, 1.000000000000000000),
 ( 1.000000000000000000, 0.9659258262890683122, 1.000000000000000000, 0.9659258262890683122, 1.000000000000000000, 0.9659258262890683122, 1.000000000000000000, 0.9659258262890683122, 1.000000000000000000, 0.9659258262890683122, 1.000000000000000000, 0.9659258262890683122, 1.000000000000000000, 0.9659258262890683122, 1.000000000000000000, 0.9659258262890683122, 1.000000000000000000, 0.9659258262890683122, 1.000000000000000000, 0.9659258262890683122, 1.000000000000000000, 0.9659258262890683122, 1.000000000000000000, 0.9659258262890683122, 1.000000000000000000, 0.9659258262890683122, 1.000000000000000000, 0.9659258262890683122, 1.000000000000000000, 0.9659258262890683122, 1.000000000000000000, 0.9659258262890683122, 1.000000000000000000, 0.9659258262890683122, 1.000000000000000000, 0.9659258262890683122, 1.000000000000000000, 0.9659258262890683122, 1.000000000000000000, 0.9659258262890683122, 1.000000000000000000, 0.9659258262890683122, 1.000000000000000000, 0.9659258262890683122, 1.000000000000000000, 0.9659258262890683122, 1.000000000000000000, 0.9659258262890683122, 1.000000000000000000, 0.9659258262890683122, 1.000000000000000000, 0.9659258262890683122, 1.000000000000000000, 0.9659258262890683122, 1.000000000000000000, 0.9659258262890683122, 1.000000000000000000, 0.9659258262890683122, 1.000000000000000000, 0.9659258262890683122, 1.000000000000000000, 0.9659258262890683122, 1.000000000000000000, 0.9659258262890683122, 1.000000000000000000, 0.9659258262890683122, 1.000000000000000000, 0.9659258262890683122, 1.000000000000000000, 0.9659258262890683122, 1.000000000000000000, 0.9659258262890683122, 1.000000000000000000, 0.9659258262890683122, 1.000000000000000000, 0.9659258262890683122, 1.000000000000000000, 0.9659258262890683122, 1.000000000000000000, 0.9659258262890683122, 1.000000000000000000, 0.9659258262890683122, 1.000000000000000000, 0.9659258262890683122, 1.000000000000000000, 0.9659258262890683122, 1.000000000000000000, 0.9659258262890683122, 1.000000000000000000, 0.9659258262890683122, 1.000000000000000000, 0.9659258262890683122, 1.000000000000000000, 0.9659258262890683122, 1.000000000000000000, 0.9659258262890683122, 1.000000000000000000, 0.9659258262890683122, 1.000000000000000000, 0.9659258262890683122, 1.000000000000000000, 0.9659258262890683122, 1.000000000000000000, 0.9659258262890683122, 1.000000000000000000, 0.9659258262890683122, 1.000000000000000000, 0.9659258262890683122, 1.000000000000000000, 0.9659258262890683122, 1.000000000000000000, 0.9659258262890683122, 1.000000000000000000, 0.9659258262890683122, 1.000000000000000000, 0.9659258262890683122, 1.000000000000000000, 0.9659258262890683122, 1.000000000000000000, 0.9659258262890683122, 1.000000000000000000, 0.9659258262890683122, 1.000000000000000000, 0.9659258262890683122, 1.000000000000000000, 0.9659258262890683122, 1.000000000000000000, 0.9659258262890683122, 1.000000000000000000, 0.9659258262890683122, 1.000000000000000000, 0.9659258262890683122, 1.000000000000000000, 0.9659258262890683122, 1.000000000000000000, 0.9659258262890683122, 1.000000000000000000, 0.9659258262890683122, 1.000000000000000000, 0.9659258262890683122, 1.000000000000000000, 0.9659258262890683122, 1.000000000000000000, 0.9659258262890683122, 1.000000000000000000, 0.9659258262890683122, 1.000000000000000000, 0.9659258262890683122, 1.000000000000000000, 0.9659258262890683122, 1.000000000000000000, 0.9659258262890683122, 1.000000000000000000, 0.9659258262890683122, 1.000000000000000000, 0.9659258262890683122, 1.000000000000000000, 0.9659258262890683122, 1.000000000000000000, 0.9659258262890683122, 1.000000000000000000, 0.9659258262890683122, 1.000000000000000000, 0.9659258262890683122, 1.000000000000000000, 0.9659258262890683122, 1.000000000000000000, 0.9659258262890683122, 1.000000000000000000, 0.9659258262890683122, 1.000000000000000000, 0.9659258262890683122, 1.000000000000000000, 0.9659258262890683122, 1.000000000000000000, 0.9659258262890683122, 1.000000000000000000, 0.9659258262890683122, 1.000000000000000000, 0.9659258262890683122, 1.000000000000000000, 0.9659258262890683122, 1.000000000000000000, 0.9659258262890683122, 1.000000000000000000, 0.9659258262890683122, 1.000000000000000000, 0.9659258262890683122, 1.000000000000000000, 0.9659258262890683122, 1.000000000000000000, 0.9659258262890683122, 1.000000000000000000, 0.9659258262890683122, 1.000000000000000000, 0.9659258262890683122, 1.000000000000000000, 0.9659258262890683122, 1.000000000000000000, 0.9659258262890683122, 1.000000000000000000, 0.9659258262890683122, 1.000000000000000000, 0.9659258262890683122, 1.000000000000000000, 0.9659258262890683122, 1.000000000000000000, 0.9659258262890683122, 1.000000000000000000, 0.9659258262890683122, 1.000000000000000000, 0.9659258262890683122, 1.000000000000000000, 0.9659258262890683122, 1.000000000000000000, 0.9659258262890683122, 1.000000000000000000, 0.9659258262890683122, 1.000000000000000000, 0.9659258262890683122, 1.000000000000000000, 0.9659258262890683122, 1.000000000000000000, 0.9659258262890683122, 1.000000000000000000, 0.9659258262890683122, 1.000000000000000000, 0.9659258262890683122, 1.000000000000000000, 0.9659258262890683122, 1.000000000000000000, 0.9659258262890683122, 1.000000000000000000, 0.9659258262890683122, 1.000000000000000000, 0.9659258262890683122, 1.000000000000000000, 0.9659258262890683122, 1.000000000000000000, 0.9659258262890683122, 1.000000000000000000, 0.9659258262890683122, 1.000000000000000000, 0.9659258262890683122, 1.000000000000000000, 0.9659258262890683122, 1.000000000000000000, 0.9659258262890683122, 1.000000000000000000, 0.9659258262890683122, 1.000000000000000000, 0.9659258262890683122, 1.000000000000000000, 0.9659258262890683122, 1.000000000000000000, 0.9659258262890683122, 1.000000000000000000, 0.9659258262890683122, 1.000000000000000000, 0.9659258262890683122, 1.000000000000000000, 0.9659258262890683122, 1.000000000000000000, 0.9659258262890683122, 1.000000000000000000, 0.9659258262890683122, 1.000000000000000000, 0.9659258262890683122, 1.000000000000000000, 0.9659258262890683122, 1.000000000000000000, 0.9659258262890683122, 1.000000000000000000, 0.9659258262890683122, 1.000000000000000000, 0.9659258262890683122, 1.000000000000000000, 0.9659258262890683122, 1.000000000000000000, 0.9659258262890683122, 1.000000000000000000, 0.9659258262890683122, 1.000000000000000000, 0.9659258262890683122, 1.000000000000000000, 0.9659258262890683122, 1.000000000000000000, 0.9659258262890683122, 1.000000000000000000, 0.9659258262890683122, 1.000000000000000000, 0.9659258262890683122, 1.000000000000000000, 0.9659258262890683122, 1.000000000000000000, 0.9659258262890683122, 1.000000000000000000, 0.9659258262890683122, 1.000000000000000000, 0.9659258262890683122, 1.000000000000000000, 0.9659258262890683122, 1.000000000000000000, 0.9659258262890683122, 1.000000000000000000, 0.9659258262890683122, 1.000000000000000000, 0.9659258262890683122, 1.000000000000000000, 0.9659258262890683122, 1.000000000000000000, 0.9659258262890683122, 1.000000000000000000, 0.9659258262890683122, 1.000000000000000000, 0.9659258262890683122, 1.000000000000000000, 0.9659258262890683122, 1.000000000000000000, 0.9659258262890683122, 1.000000000000000000, 0.9659258262890683122, 1.000000000000000000, 0.9659258262890683122, 1.000000000000000000, 0.9659258262890683122, 1.000000000000000000, 0.9659258262890683122, 1.000000000000000000, 0.9659258262890683122, 1.000000000000000000, 0.9659258262890683122, 1.000000000000000000, 0.9659258262890683122, 1.000000000000000000, 0.9659258262890683122, 1.000000000000000000, 0.9659258262890683122, 1.000000000000000000, 0.9659258262890683122, 1.000000000000000000, 0.9659258262890683122, 1.000000000000000000, 0.9659258262890683122, 1.000000000000000000, 0.9659258262890683122, 1.000000000000000000, 0.9659258262890683122, 1.000000000000000000, 0.9659258262890683122, 1.000000000000000000, 0.9659258262890683122, 1.000000000000000000, 0.9659258262890683122, 1.000000000000000000, 0.9659258262890683122, 1.000000000000000000, 0.9659258262890683122, 1.000000000000000000, 0.9659258262890683122, 1.000000000000000000, 0.9659258262890683122, 1.000000000000000000, 0.9659258262890683122, 1.000000000000000000, 0.9659258262890683122, 1.000000000000000000, 0.9659258262890683122, 1.000000000000000000, 0.9659258262890683122, 1.000000000000000000, 0.9659258262890683122, 1.000000000000000000, 0.9659258262890683122, 1.000000000000000000, 0.9659258262890683122, 1.000000000000000000, 0.9659258262890683122, 1.000000000000000000, 0.9659258262890683122, 1.000000000000000000, 0.9659258262890683122, 1.000000000000000000, 0.9659258262890683122, 1.000000000000000000, 0.9659258262890683122, 1.000000000000000000, 0.9659258262890683122, 1.000000000000000000, 0.9659258262890683122, 1.000000000000000000, 0.9659258262890683122, 1.000000000000000000, 0.9659258262890683122, 1.000000000000000000, 0.9659258262890683122, 1.000000000000000000, 0.9659258262890683122, 1.000000000000000000, 0.9659258262890683122, 1.000000000000000000, 0.9659258262890683122, 1.000000000000000000, 0.9659258262890683122, 1.000000000000000000, 0.9659258262890683122, 1.000000000000000000, 0.9659258262890683122, 1.000000000000000000, 0.9659258262890683122, 1.000000000000000000, 0.9659258262890683122, 1.000000000000000000, 0.9659258262890683122, 1.000000000000000000, 0.9659258262890683122, 1.000000000000000000, 0.9659258262890683122, 1.000000000000000000, 0.9659258262890683122, 1.000000000000000000, 0.9659258262890683122, 1.000000000000000000, 0.9659258262890683122, 1.000000000000000000, 0.9659258262890683122, 1.000000000000000000, 0.9659258262890683122, 1.000000000000000000, 0.9659258262890683122, 1.000000000000000000, 0.9659258262890683122, 1.000000000000000000, 0.9659258262890683122, 1.000000000000000000, 0.9659258262890683122, 1.000000000000000000, 0.9659258262890683122, 1.000000000000000000, 0.9659258262890683122, 1.000000000000000000, 0.9659258262890683122, 1.000000000000000000, 0.9659258262890683122, 1.000000000000000000, 0.9659258262890683122, 1.000000000000000000, 0.9659258262890683122, 1.000000000000000000, 0.9659258262890683122, 1.000000000000000000, 0.9659258262890683122, 1.000000000000000000, 0.9659258262890683122, 1.000000000000000000, 0.9659258262890683122, 1.000000000000000000, 0.9659258262890683122, 1.000000000000000000, 0.9659258262890683122, 1.000000000000000000, 0.9659258262890683122, 1.000000000000000000, 0.9659258262890683122, 1.000000000000000000, 0.9659258262890683122, 1.000000000000000000, 0.9659258262890683122, 1.000000000000000000, 0.9659258262890683122, 1.000000000000000000, 0.9659258262890683122, 1.000000000000000000, 0.9659258262890683122, 1.000000000000000000) ) ) 
 REPRESENTATION_ITEM ( '' )  SURFACE ( )  );
#17109 = CARTESIAN_POINT ( 'NONE',  ( -0.2821522309711278487, -0.5511811023622048555, -0.09757992244046775898 ) ) ;
#17110 = CARTESIAN_POINT ( 'NONE',  ( -1.312335958005248715, -0.5023911411419708095, -0.1820866141732282451 ) ) ;
#17111 = CARTESIAN_POINT ( 'NONE',  ( 1.581364829396326277, -0.05778040916215522460, 0.4822834645669289988 ) ) ;
#17112 = CARTESIAN_POINT ( 'NONE',  ( 0.3543307086614179147, 0.2952755905511811885, 0.000000000000000000 ) ) ;
#17113 = CARTESIAN_POINT ( 'NONE',  ( -1.220472440944881054, -0.6692913385826771977, 8.415575281601705876E-17 ) ) ;
#17114 = CARTESIAN_POINT ( 'NONE',  ( 0.2867679344610365999, 0.2867679344610365999, -0.2874015748031494843 ) ) ;
#17115 = VERTEX_POINT ( 'NONE', #59878 ) ;
#17116 = CARTESIAN_POINT ( 'NONE',  ( 1.555118110236221041, -0.5400638737290844871, 0.3530559997133364547 ) ) ;
#17117 = LINE ( 'NONE', #68447, #9801 ) ;
#17118 = CARTESIAN_POINT ( 'NONE',  ( -0.3458507752293906723, -0.3458507752293910609, -1.791338582677165059 ) ) ;
#17119 = CARTESIAN_POINT ( 'NONE',  ( 0.000000000000000000, 0.4201155382560080032, 0.000000000000000000 ) ) ;
#17120 = EDGE_CURVE ( 'NONE', #76587, #40450, #58068, .T. ) ;
#17121 = AXIS2_PLACEMENT_3D ( 'NONE', #33164, #50834, #83255 ) ;
#17122 = DIRECTION ( 'NONE',  ( 1.000000000000000000, 0.000000000000000000, -1.692413147294446216E-16 ) ) ;
#17123 = CARTESIAN_POINT ( 'NONE',  ( -0.9514435695538050464, -0.05778040916215560624, -0.4822834645669293319 ) ) ;
#17124 = CARTESIAN_POINT ( 'NONE',  ( 1.627296587926509996, -0.6046776061558807314, 0.2411417322834647770 ) ) ;
#17125 = AXIS2_PLACEMENT_3D ( 'NONE', #95, #25332, #51411 ) ;
#17126 = CIRCLE ( 'NONE', #31859, 3.858267716535433323 ) ;
#17128 = CARTESIAN_POINT ( 'NONE',  ( 0.6430446194225728496, 0.009842519685039463617, 0.3409548833797002576 ) ) ;
#17127 = CARTESIAN_POINT ( 'NONE',  ( 0.7202472836732369821, 0.02791078216816263863, 0.4328096321851903627 ) ) ;
#17129 = CARTESIAN_POINT ( 'NONE',  ( 1.535433070866142558, 0.2952755905511811885, 0.000000000000000000 ) ) ;
#17130 = CARTESIAN_POINT ( 'NONE',  ( -0.9186351706036736120, 0.2306618581243848609, 0.2411417322834645549 ) ) ;
#17131 = CARTESIAN_POINT ( 'NONE',  ( 0.3917322834645669549, 2.398668435337827645E-17, -0.1981434138769535558 ) ) ;
#17132 = CARTESIAN_POINT ( 'NONE',  ( -0.06561679790026180015, -0.3690944881889765550, -0.3153832671262227771 ) ) ;
#17133 = CARTESIAN_POINT ( 'NONE',  ( -0.1958661417322836718, 0.3392501089628017219, -0.2552493438320210806 ) ) ;
#17134 = CARTESIAN_POINT ( 'NONE',  ( 0.01312335958005323398, -0.3690944881889765550, -0.3153832671262227771 ) ) ;
#17135 = CARTESIAN_POINT ( 'NONE',  ( 0.7152230971128614723, -0.2845877964562161244, -0.3641732283464567121 ) ) ;
#17136 = CARTESIAN_POINT ( 'NONE',  ( 0.4527559055118117182, -0.5400638737290844871, 0.3530559997133364547 ) ) ;
#17137 = CARTESIAN_POINT ( 'NONE',  ( -0.8530183727034112984, -0.004921259842519576551, 0.3153832671262227771 ) ) ;
#17138 = CARTESIAN_POINT ( 'NONE',  ( -0.2867679344610365999, 0.2867679344610364889, -2.531496062992125484 ) ) ;
#17139 = CARTESIAN_POINT ( 'NONE',  ( -1.528871391076114250, -0.6692913385826771977, 0.1292274648535927661 ) ) ;
#17140 = CARTESIAN_POINT ( 'NONE',  ( -1.220472440944881054, -0.6692913385826771977, 8.415575281601705876E-17 ) ) ;
#17141 = CARTESIAN_POINT ( 'NONE',  ( -0.3458507752293906723, -0.3458507752293910609, -0.6082677165354329896 ) ) ;
#17142 = CARTESIAN_POINT ( 'NONE',  ( 0.09842519685039434474, -0.5400638737290845981, -0.3530559997133363437 ) ) ;
#17143 = CARTESIAN_POINT ( 'NONE',  ( -0.4790026246719152336, -0.05778040916215560624, -0.4822834645669293319 ) ) ;
#17144 = CARTESIAN_POINT ( 'NONE',  ( 1.312335958005250269, -0.5023911411419708095, 0.1820866141732285504 ) ) ;
#17145 = CARTESIAN_POINT ( 'NONE',  ( 0.3083989501312343062, -0.2845877964562159024, 0.3641732283464567677 ) ) ;
#17146 = CARTESIAN_POINT ( 'NONE',  ( -0.3871391076115479057, -0.3162353388693409650, -0.4822834645669289433 ) ) ;
#17147 = CARTESIAN_POINT ( 'NONE',  ( -0.7086614173228339419, -0.1870078740157479769, 0.4822834645669291653 ) ) ;
#17148 = DIRECTION ( 'NONE',  ( 1.000000000000000000, -0.000000000000000000, -0.000000000000000000 ) ) ;
#17149 = LINE ( 'NONE', #49925, #8646 ) ;
#17150 = CARTESIAN_POINT ( 'NONE',  ( 0.2165354330708668673, -0.5400638737290844871, 0.3530559997133364547 ) ) ;
#17151 = VERTEX_POINT ( 'NONE', #14462 ) ;
#17152 = CARTESIAN_POINT ( 'NONE',  ( 0.1998031496062992463, 0.3460692066303959202, -1.953412073490813805 ) ) ;
#17153 = CARTESIAN_POINT ( 'NONE',  ( 1.141732283464567566, 0.2952755905511811885, 0.000000000000000000 ) ) ;
#17154 = CARTESIAN_POINT ( 'NONE',  ( -0.4396325459317579898, 0.1771653543307087630, 0.09757992244046791164 ) ) ;
#17155 = CARTESIAN_POINT ( 'NONE',  ( -0.6561679790026240244, -0.6046776061558807314, 0.2411417322834647770 ) ) ;
#17156 = CARTESIAN_POINT ( 'NONE',  ( 1.456692913385827515, -0.6692913385826771977, 8.415575281601705876E-17 ) ) ;
#17157 = CARTESIAN_POINT ( 'NONE',  ( 0.8727034120734913358, -0.05778040916215522460, 0.4822834645669289988 ) ) ;
#17158 = CARTESIAN_POINT ( 'NONE',  ( -1.522309711286088607, -0.6046776061558807314, 0.2411417322834647770 ) ) ;
#17159 = CARTESIAN_POINT ( 'NONE',  ( -1.017060367454067249, -0.2845877964562161244, -0.3641732283464567121 ) ) ;
#17160 = CARTESIAN_POINT ( 'NONE',  ( 0.3460692066303959202, -0.1998031496062991630, -0.1817585301837270351 ) ) ;
#17161 = CARTESIAN_POINT ( 'NONE',  ( -0.3460692066303960868, 0.1998031496062990242, -0.6561679790026246906 ) ) ;
#17162 = CARTESIAN_POINT ( 'NONE',  ( -0.3420746716998661618, 0.1974969037888702206, 0.1312335958005248771 ) ) ;
#17163 = CARTESIAN_POINT ( 'NONE',  ( 1.594488188976378673, -0.4536011799217368745, -0.2665933059059886201 ) ) ;
#17164 = CARTESIAN_POINT ( 'NONE',  ( 1.017060367454068581, -0.08942795157528024563, -0.3641732283464568787 ) ) ;
#17165 = CARTESIAN_POINT ( 'NONE',  ( 0.3674540682414705883, 0.2306618581243847221, -0.2411417322834647770 ) ) ;
#17166 = CARTESIAN_POINT ( 'NONE',  ( -1.660104986876639543, -0.05778040916215560624, -0.4822834645669293319 ) ) ;
#17167 = CARTESIAN_POINT ( 'NONE',  ( -0.3420746716998662729, 0.1974969037888702206, -0.8904199475065616154 ) ) ;
#17168 = CARTESIAN_POINT ( 'NONE',  ( 0.7742782152230979209, -0.004921259842519870586, -0.3153832671262229437 ) ) ;
#17169 = CARTESIAN_POINT ( 'NONE',  ( -0.3083989501312330295, -0.3162353388693409650, -0.4822834645669289433 ) ) ;
#17170 = CARTESIAN_POINT ( 'NONE',  ( -0.7152230971128602510, -0.3162353388693405765, 0.4822834645669290543 ) ) ;
#17171 = CARTESIAN_POINT ( 'NONE',  ( 1.286089238845145033, -0.6046776061558809534, -0.2411417322834644161 ) ) ;
#17172 = CARTESIAN_POINT ( 'NONE',  ( -0.4724409448818895907, -0.1265901696524993070, -1.305774278215223072 ) ) ;
#17173 = AXIS2_PLACEMENT_3D ( 'NONE', #37442, #37027, #10950 ) ;
#17174 = CARTESIAN_POINT ( 'NONE',  ( -0.1070741851644051862, -0.3996062992125986590, -2.434383202099737353 ) ) ;
#17175 = CARTESIAN_POINT ( 'NONE',  ( 0.1115485564304467270, -0.5511811023622048555, -0.09757992244046775898 ) ) ;
#17176 = ORIENTED_EDGE ( 'NONE', *, *, #57314, .F. ) ;
#17177 = CARTESIAN_POINT ( 'NONE',  ( 4.797336870675656522E-17, -0.3917322834645670659, -0.8628802081702905413 ) ) ;
#17178 = VERTEX_POINT ( 'NONE', #72104 ) ;
#17179 = CARTESIAN_POINT ( 'NONE',  ( -0.7283464566929126471, 0.1660481256975883668, -0.3530559997133364547 ) ) ;
#17180 = CARTESIAN_POINT ( 'NONE',  ( -0.1049868766404193215, -0.6046776061558807314, 0.2411417322834647770 ) ) ;
#17181 = CARTESIAN_POINT ( 'NONE',  ( -0.3280839895013117347, 0.05413385826771626580, -0.4176697321401330321 ) ) ;
#17182 = CARTESIAN_POINT ( 'NONE',  ( 0.9580052493438327987, -0.4281496062992127816, -0.4176697321401328100 ) ) ;
#17183 = CARTESIAN_POINT ( 'NONE',  ( -0.3937007874015740483, -0.1870078740157479769, 0.4822834645669291653 ) ) ;
#17184 = CARTESIAN_POINT ( 'NONE',  ( -1.318897637795274802, 0.1660481256975885056, 0.3530559997133364547 ) ) ;
#17185 = CARTESIAN_POINT ( 'NONE',  ( -0.4921259842519677963, -0.5400638737290844871, 0.3530559997133364547 ) ) ;
#17186 = CARTESIAN_POINT ( 'NONE',  ( 0.7152230971128614723, -0.3162353388693409650, -0.4822834645669289433 ) ) ;
#17187 = ADVANCED_FACE ( 'NONE', ( #34215 ), #49406, .F. ) ;
#17188 = CARTESIAN_POINT ( 'NONE',  ( 0.4527559055118117182, -0.5400638737290844871, 0.3530559997133364547 ) ) ;
#17189 = CARTESIAN_POINT ( 'NONE',  ( -0.3917322834645671215, 0.1049643490035301469, -0.9698162729658791337 ) ) ;
#17190 = CARTESIAN_POINT ( 'NONE',  ( -0.5183727034120726440, 0.1771653543307087630, 0.09757992244046791164 ) ) ;
#17191 = ORIENTED_EDGE ( 'NONE', *, *, #48857, .F. ) ;
#17192 = CARTESIAN_POINT ( 'NONE',  ( 0.1058382717557499880, 0.3949938075777411073, -1.568241469816272993 ) ) ;
#17193 = ORIENTED_EDGE ( 'NONE', *, *, #53241, .F. ) ;
#17194 = CARTESIAN_POINT ( 'NONE',  ( -1.476377952755905110, -0.4536011799217368745, -0.2665933059059886201 ) ) ;
#17195 = CARTESIAN_POINT ( 'NONE',  ( -0.3674540682414689785, 0.2306618581243848609, 0.2411417322834645549 ) ) ;
#17196 = CARTESIAN_POINT ( 'NONE',  ( -0.1070741851644056997, 0.3996062992125986035, 0.1509186351706036100 ) ) ;
#17197 = CARTESIAN_POINT ( 'NONE',  ( -0.8070866141732276899, -0.5400638737290844871, 0.3530559997133364547 ) ) ;
#17198 = CARTESIAN_POINT ( 'NONE',  ( -0.7611548556430438595, 0.2306618581243848609, 0.2411417322834645549 ) ) ;
#17199 = CARTESIAN_POINT ( 'NONE',  ( -1.450131233595799651, 0.2952755905511810774, -0.1292274648535930714 ) ) ;
#17200 = CYLINDRICAL_SURFACE ( 'NONE', #61721, 0.3937007874015748254 ) ;
#17201 = CARTESIAN_POINT ( 'NONE',  ( 0.9055118110236227702, 0.1771653543307087630, 0.000000000000000000 ) ) ;
#17202 = CARTESIAN_POINT ( 'NONE',  ( 0.4478583149154592435, 1.694693813591205300, 1.028805191090655935 ) ) ;
#17203 = CARTESIAN_POINT ( 'NONE',  ( 0.2867679344610365999, 0.2867679344610365999, 0.09251968503937001154 ) ) ;
#17204 = CARTESIAN_POINT ( 'NONE',  ( 0.1115485564304467270, -0.5511811023622048555, -0.09757992244046775898 ) ) ;
#17205 = CARTESIAN_POINT ( 'NONE',  ( -0.4724409448818890911, -0.1870078740157480879, -0.4822834645669291653 ) ) ;
#17206 = CARTESIAN_POINT ( 'NONE',  ( -0.3307086614173228023, 0.3242060844882008741, 0.000000000000000000 ) ) ;
#17207 = CARTESIAN_POINT ( 'NONE',  ( 0.02624671916010564918, -0.6046776061558809534, -0.2411417322834644161 ) ) ;
#17208 = ORIENTED_EDGE ( 'NONE', *, *, #71135, .T. ) ;
#17209 = CARTESIAN_POINT ( 'NONE',  ( 0.3996062992125986035, 2.446882876249141962E-17, -2.007874015748031482 ) ) ;
#17210 = PLANE ( 'NONE',  #57386 ) ;
#17211 = ORIENTED_EDGE ( 'NONE', *, *, #28505, .F. ) ;
#17212 = CARTESIAN_POINT ( 'NONE',  ( 0.3996062992125985480, 2.446882876249141654E-17, -1.454724409448818756 ) ) ;
#17213 = CARTESIAN_POINT ( 'NONE',  ( -0.2061694042878472743, 0.2114133405073579941, 0.1284558427095351396 ) ) ;
#17214 = CARTESIAN_POINT ( 'NONE',  ( -0.6364829396325453192, -0.2845877964562159024, 0.3641732283464567677 ) ) ;
#17215 = CARTESIAN_POINT ( 'NONE',  ( -0.9973753280839886548, -0.6046776061558809534, -0.2411417322834644161 ) ) ;
#17216 = CARTESIAN_POINT ( 'NONE',  ( 0.4724409448818897572, -0.1265901696524988906, -0.2690288713910760632 ) ) ;
#17217 = CARTESIAN_POINT ( 'NONE',  ( -0.3307086614173228023, 0.3051181102362204856, 0.000000000000000000 ) ) ;
#17218 = ADVANCED_FACE ( 'NONE', ( #55914 ), #81627, .T. ) ;
#17219 = CARTESIAN_POINT ( 'NONE',  ( 4.797336870675656522E-17, -0.3917322834645670104, -2.368110236220472675 ) ) ;
#17220 = CARTESIAN_POINT ( 'NONE',  ( 1.220472440944882608, 0.2952755905511811885, 0.000000000000000000 ) ) ;
#17221 = CARTESIAN_POINT ( 'NONE',  ( 0.3280839895013130669, 0.05413385826771666132, 0.4176697321401328100 ) ) ;
#17222 = CARTESIAN_POINT ( 'NONE',  ( 0.5052493438320218022, -0.6692913385826773087, -0.1292274648535924053 ) ) ;
#17223 = CARTESIAN_POINT ( 'NONE',  ( -0.4593175853018364174, -0.3690944881889765550, -0.3153832671262227771 ) ) ;
#17224 = CARTESIAN_POINT ( 'NONE',  ( -0.4461942257217840213, 0.2306618581243848609, 0.2411417322834645549 ) ) ;
#17225 = CARTESIAN_POINT ( 'NONE',  ( 0.1265901696524990294, -0.4724409448818896462, -2.524278215223096478 ) ) ;
#17226 = EDGE_CURVE ( 'NONE', #18415, #17964, #30672, .T. ) ;
#17227 = CARTESIAN_POINT ( 'NONE',  ( -0.8398950131233589023, -0.6046776061558809534, -0.2411417322834644161 ) ) ;
#17228 = CARTESIAN_POINT ( 'NONE',  ( 0.1974969037888704704, 0.3420746716998660508, -2.425853018372703396 ) ) ;
#17229 = PRODUCT_RELATED_PRODUCT_CATEGORY ( 'part', '', ( #72209 ) ) ;
#17230 = CARTESIAN_POINT ( 'NONE',  ( 1.417322834645670104, -0.1870078740157479769, 0.3641732283464567677 ) ) ;
#17231 = CARTESIAN_POINT ( 'NONE',  ( -0.1574803149606292529, -0.1870078740157479769, 0.3641732283464567677 ) ) ;
#17232 = CARTESIAN_POINT ( 'NONE',  ( 1.187664041994751285, -0.08942795157527998196, 0.3641732283464567121 ) ) ;
#17233 = CARTESIAN_POINT ( 'NONE',  ( 1.614173228346457378, 0.1771653543307087630, 0.000000000000000000 ) ) ;
#17234 = CARTESIAN_POINT ( 'NONE',  ( -1.181102362204723644, -0.1870078740157479769, 0.3641732283464567677 ) ) ;
#17235 = DIRECTION ( 'NONE',  ( 0.000000000000000000, 0.000000000000000000, 1.000000000000000000 ) ) ;
#17236 = CARTESIAN_POINT ( 'NONE',  ( -1.049868766404198794, 0.2306618581243847221, -0.2411417322834647770 ) ) ;
#17237 = CARTESIAN_POINT ( 'NONE',  ( -0.4068241469816264999, -0.4281496062992124485, 0.4176697321401328655 ) ) ;
#17238 =( BOUNDED_CURVE ( )  B_SPLINE_CURVE ( 2, ( #323, #71025, #71442, #32715, #57128, #70182, #19669, #7046, #13790, #50406, #58382, #24738, #76516, #63462, #51223, #57544, #25556, #52058, #39447, #64289, #32295, #76921, #33140, #65135, #25147, #76104, #51635, #45330, #50815, #44089, #31466, #12535, #69783, #12128, #5796, #82823, #38194, #19249, #18845, #63869, #13369, #6207, #39022, #64706, #31884, #70599, #9140, #21753, #78607, #71864, #7895, #67215, #65561, #15040, #34389, #52894, #60055, #22173, #79027, #41529, #46587, #73536, #54142, #14214, #20930, #47416, #34811, #40696, #53726, #27235, #2410, #73107, #72285, #39872, #33556, #9548, #59219, #66381, #28068, #14631, #79434, #15458, #1580, #40287, #65968, #15881, #79856, #8305, #33972, #41116, #60470, #8718, #66806, #59633, #2821, #1989, #46168, #78185, #28482, #47831, #27652, #53315, #20516, #21346, #35218, #46999, #72693, #1168, #26819, #52477, #10790, #29721, #41934, #55383, #76717, #48661, #30131, #68451, #43160, #35632, #81089, #60882, #12749, #22588, #36450, #81501, #36864, #67630, #54975 ),
 .UNSPECIFIED., .F., .F. ) 
 B_SPLINE_CURVE_WITH_KNOTS ( ( 3, 2, 2, 2, 2, 2, 2, 2, 2, 2, 2, 2, 2, 2, 2, 2, 2, 2, 2, 2, 2, 2, 2, 2, 2, 2, 2, 2, 2, 2, 2, 2, 2, 2, 2, 2, 2, 2, 2, 2, 2, 2, 2, 2, 2, 2, 2, 2, 2, 2, 2, 2, 2, 2, 2, 2, 2, 2, 2, 2, 2, 2, 2, 2, 3 ),
 ( 0.6856214849132036271, 0.6875000000000000000, 0.6916666666666666519, 0.6958333333333333037, 0.6999999999999999556, 0.7041666666666667185, 0.7083333333333333703, 0.7125000000000000222, 0.7166666666666666741, 0.7208333333333333259, 0.7249999999999999778, 0.7291666666666666297, 0.7333333333333332815, 0.7375000000000000444, 0.7416666666666666963, 0.7458333333333333481, 0.7500000000000000000, 0.7541666666666666519, 0.7583333333333333037, 0.7624999999999999556, 0.7666666666666667185, 0.7708333333333333703, 0.7750000000000000222, 0.7791666666666666741, 0.7833333333333333259, 0.7874999999999999778, 0.7916666666666666297, 0.7958333333333332815, 0.8000000000000000444, 0.8041666666666666963, 0.8083333333333333481, 0.8125000000000000000, 0.8166666666666666519, 0.8208333333333333037, 0.8249999999999999556, 0.8291666666666667185, 0.8333333333333333703, 0.8375000000000000222, 0.8416666666666666741, 0.8458333333333333259, 0.8499999999999999778, 0.8541666666666666297, 0.8583333333333332815, 0.8625000000000000444, 0.8666666666666666963, 0.8708333333333333481, 0.8750000000000000000, 0.8791666666666666519, 0.8833333333333333037, 0.8874999999999999556, 0.8916666666666667185, 0.8958333333333333703, 0.9000000000000000222, 0.9041666666666666741, 0.9083333333333333259, 0.9124999999999999778, 0.9166666666666666297, 0.9208333333333332815, 0.9250000000000000444, 0.9291666666666666963, 0.9333333333333333481, 0.9375000000000000000, 0.9416666666666666519, 0.9458333333333333037, 0.9481214849132038047 ),
 .UNSPECIFIED. ) 
 CURVE ( )  GEOMETRIC_REPRESENTATION_ITEM ( )  RATIONAL_B_SPLINE_CURVE ( ( 0.9831275833774530959, 0.9846378761473346675, 1.000000000000000000, 0.9659258262890683122, 1.000000000000000000, 0.9659258262890683122, 1.000000000000000000, 0.9659258262890683122, 1.000000000000000000, 0.9659258262890683122, 1.000000000000000000, 0.9659258262890683122, 1.000000000000000000, 0.9659258262890683122, 1.000000000000000000, 0.9659258262890683122, 1.000000000000000000, 0.9659258262890683122, 1.000000000000000000, 0.9659258262890683122, 1.000000000000000000, 0.9659258262890683122, 1.000000000000000000, 0.9659258262890683122, 1.000000000000000000, 0.9659258262890683122, 1.000000000000000000, 0.9659258262890683122, 1.000000000000000000, 0.9659258262890683122, 1.000000000000000000, 0.9659258262890683122, 1.000000000000000000, 0.9659258262890683122, 1.000000000000000000, 0.9659258262890683122, 1.000000000000000000, 0.9659258262890683122, 1.000000000000000000, 0.9659258262890683122, 1.000000000000000000, 0.9659258262890683122, 1.000000000000000000, 0.9659258262890683122, 1.000000000000000000, 0.9659258262890683122, 1.000000000000000000, 0.9659258262890683122, 1.000000000000000000, 0.9659258262890683122, 1.000000000000000000, 0.9659258262890683122, 1.000000000000000000, 0.9659258262890683122, 1.000000000000000000, 0.9659258262890683122, 1.000000000000000000, 0.9659258262890683122, 1.000000000000000000, 0.9659258262890683122, 1.000000000000000000, 0.9659258262890683122, 1.000000000000000000, 0.9659258262890683122, 1.000000000000000000, 0.9659258262890683122, 1.000000000000000000, 0.9659258262890683122, 1.000000000000000000, 0.9659258262890683122, 1.000000000000000000, 0.9659258262890683122, 1.000000000000000000, 0.9659258262890683122, 1.000000000000000000, 0.9659258262890683122, 1.000000000000000000, 0.9659258262890683122, 1.000000000000000000, 0.9659258262890683122, 1.000000000000000000, 0.9659258262890683122, 1.000000000000000000, 0.9659258262890683122, 1.000000000000000000, 0.9659258262890683122, 1.000000000000000000, 0.9659258262890683122, 1.000000000000000000, 0.9659258262890683122, 1.000000000000000000, 0.9659258262890683122, 1.000000000000000000, 0.9659258262890683122, 1.000000000000000000, 0.9659258262890683122, 1.000000000000000000, 0.9659258262890683122, 1.000000000000000000, 0.9659258262890683122, 1.000000000000000000, 0.9659258262890683122, 1.000000000000000000, 0.9659258262890683122, 1.000000000000000000, 0.9659258262890683122, 1.000000000000000000, 0.9659258262890683122, 1.000000000000000000, 0.9659258262890683122, 1.000000000000000000, 0.9659258262890683122, 1.000000000000000000, 0.9659258262890683122, 1.000000000000000000, 0.9659258262890683122, 1.000000000000000000, 0.9659258262890683122, 1.000000000000000000, 0.9659258262890683122, 1.000000000000000000, 0.9659258262890683122, 1.000000000000000000, 0.9659258262890683122, 1.000000000000000000, 0.9659258262890683122, 1.000000000000000000, 0.9812879501417318684, 0.9831275833774535400 ) ) 
 REPRESENTATION_ITEM ( '' )  );
#17239 = AXIS2_PLACEMENT_3D ( 'NONE', #44939, #43293, #70216 ) ;
#17240 = CARTESIAN_POINT ( 'NONE',  ( -2.077234194078065865, 1.326002914239481356, 0.4256865378621424445 ) ) ;
#17241 = CARTESIAN_POINT ( 'NONE',  ( -0.1115485564304453947, -0.5511811023622046335, 0.09757992244046803654 ) ) ;
#17242 = CARTESIAN_POINT ( 'NONE',  ( -1.666666666666665853, -0.004921259842519870586, -0.3153832671262229437 ) ) ;
#17243 = CARTESIAN_POINT ( 'NONE',  ( 0.6102362204724416372, 0.1660481256975883668, -0.3530559997133364547 ) ) ;
#17244 = DIRECTION ( 'NONE',  ( 0.000000000000000000, 0.000000000000000000, 1.000000000000000000 ) ) ;
#17245 = CARTESIAN_POINT ( 'NONE',  ( 1.574803149606299746, -0.1870078740157479769, 0.3641732283464567677 ) ) ;
#17246 = CARTESIAN_POINT ( 'NONE',  ( -1.089238845144356427, 0.05413385826771666132, 0.4176697321401328100 ) ) ;
#17247 = CARTESIAN_POINT ( 'NONE',  ( -0.2493438320209966919, -0.3690944881889763329, 0.3153832671262228327 ) ) ;
#17248 = DIRECTION ( 'NONE',  ( -1.000000000000000000, 1.445602896647338917E-16, -0.000000000000000000 ) ) ;
#17249 = CARTESIAN_POINT ( 'NONE',  ( 0.1443569553805781891, -0.3690944881889763329, 0.3153832671262228327 ) ) ;
#17250 = EDGE_CURVE ( 'NONE', #14101, #59522, #62930, .T. ) ;
#17251 = CARTESIAN_POINT ( 'NONE',  ( -0.2690288713910754526, -0.6692913385826771977, 0.1292274648535927661 ) ) ;
#17252 = CARTESIAN_POINT ( 'NONE',  ( -0.1998031496062994405, 0.3460692066303957537, -0.5623359580052492701 ) ) ;
#17253 = CARTESIAN_POINT ( 'NONE',  ( -0.3392501089628017219, -0.1958661417322836718, -2.026902887139107712 ) ) ;
#17254 = CARTESIAN_POINT ( 'NONE',  ( 0.7545931758530188826, -0.5511811023622046335, 0.09757992244046803654 ) ) ;
#17255 = CARTESIAN_POINT ( 'NONE',  ( 0.09186351706036827158, 0.05413385826771666132, 0.4176697321401328100 ) ) ;
#17256 = CARTESIAN_POINT ( 'NONE',  ( -0.5774278215223089816, -0.6046776061558807314, 0.2411417322834647770 ) ) ;
#17257 = CARTESIAN_POINT ( 'NONE',  ( -0.8267716535433065062, 0.1771653543307087630, 0.000000000000000000 ) ) ;
#17258 = CARTESIAN_POINT ( 'NONE',  ( 0.9645669291338589968, 0.1012011053420777407, 0.2882089793578257453 ) ) ;
#17259 = CARTESIAN_POINT ( 'NONE',  ( -0.3674540682414689785, 0.1283753931104748280, 0.1820866141732283561 ) ) ;
#17260 = CARTESIAN_POINT ( 'NONE',  ( -0.1771653543307080136, 0.1660481256975883668, -0.3530559997133364547 ) ) ;
#17261 = CARTESIAN_POINT ( 'NONE',  ( -1.207349081364828880, 0.1283753931104746893, -0.1820866141732285504 ) ) ;
#17262 = CARTESIAN_POINT ( 'NONE',  ( -0.1070741851644051862, -0.3996062992125986590, -1.566272965879265344 ) ) ;
#17263 = CARTESIAN_POINT ( 'NONE',  ( -1.450131233595799651, 0.2952755905511810774, -0.1292274648535930714 ) ) ;
#17264 = CARTESIAN_POINT ( 'NONE',  ( 0.4091458600556403535, 0.2362204724409449896, -2.570209973753280863 ) ) ;
#17265 = ORIENTED_EDGE ( 'NONE', *, *, #82913, .F. ) ;
#17266 = CARTESIAN_POINT ( 'NONE',  ( -1.358267716535432434, 0.07958543189024071263, -0.2665933059059888421 ) ) ;
#17267 = CARTESIAN_POINT ( 'NONE',  ( -0.3477690288713905509, -0.6692913385826771977, 0.1292274648535927661 ) ) ;
#17268 = EDGE_CURVE ( 'NONE', #2483, #65017, #46189, .T. ) ;
#17269 = CARTESIAN_POINT ( 'NONE',  ( -1.030183727034119867, -0.3162353388693405765, 0.4822834645669290543 ) ) ;
#17270 = CARTESIAN_POINT ( 'NONE',  ( -0.3917322834645670104, -7.196005306013484475E-17, -1.698818897637795367 ) ) ;
#17271 = DIRECTION ( 'NONE',  ( 0.000000000000000000, -1.000000000000000000, 0.000000000000000000 ) ) ;
#17272 = CARTESIAN_POINT ( 'NONE',  ( 1.555118110236221041, 0.1660481256975883668, -0.3530559997133364547 ) ) ;
#17273 = CARTESIAN_POINT ( 'NONE',  ( 0.3149606299212606708, -0.1870078740157480879, -0.4822834645669291653 ) ) ;
#17274 = DIRECTION ( 'NONE',  ( -0.000000000000000000, -1.000000000000000000, -0.000000000000000000 ) ) ;
#17275 = CARTESIAN_POINT ( 'NONE',  ( 4.893765752498283308E-17, -0.3996062992125985480, -2.202755905511811108 ) ) ;
#17276 = CARTESIAN_POINT ( 'NONE',  ( 1.535433070866142335, -0.5511811023622047445, 6.969142054262312111E-17 ) ) ;
#17277 = CARTESIAN_POINT ( 'NONE',  ( -9.787531504996567848E-17, 0.3996062992125986035, -0.7874015748031496509 ) ) ;
#17278 = ORIENTED_EDGE ( 'NONE', *, *, #53641, .F. ) ;
#17279 = CARTESIAN_POINT ( 'NONE',  ( -0.7808398950131222316, -0.2845877964562161244, -0.3641732283464567121 ) ) ;
#17280 = CARTESIAN_POINT ( 'NONE',  ( 0.1958661417322836440, -0.3392501089628017219, -2.603674540682414218 ) ) ;
#17281 = ORIENTED_EDGE ( 'NONE', *, *, #11019, .T. ) ;
#17282 = CARTESIAN_POINT ( 'NONE',  ( 0.2887139107611556010, -0.6046776061558807314, 0.2411417322834647770 ) ) ;
#17283 = CARTESIAN_POINT ( 'NONE',  ( -0.5774278215223089816, 0.2306618581243847221, -0.2411417322834647770 ) ) ;
#17284 = CARTESIAN_POINT ( 'NONE',  ( -1.213910761154854745, -0.6692913385826771977, 0.1292274648535927661 ) ) ;
#17285 = CARTESIAN_POINT ( 'NONE',  ( 1.246719160104987623, 0.05413385826771626580, -0.4176697321401330321 ) ) ;
#17286 = CARTESIAN_POINT ( 'NONE',  ( -1.345144356955379816, -0.2845877964562159024, 0.3641732283464567677 ) ) ;
#17287 = LINE ( 'NONE', #55960, #2388 ) ;
#17288 = CARTESIAN_POINT ( 'NONE',  ( -0.05249343832020911260, 0.2306618581243848609, 0.2411417322834645549 ) ) ;
#17289 = CARTESIAN_POINT ( 'NONE',  ( -1.128608923884513837, 0.2306618581243847221, -0.2411417322834647770 ) ) ;
#17290 = CARTESIAN_POINT ( 'NONE',  ( -0.1049643490035301746, -0.3917322834645670659, -1.884495119913699002 ) ) ;
#17291 = CARTESIAN_POINT ( 'NONE',  ( -1.646051170424378096, -0.1870078740157480046, 1.254653134982923898E-17 ) ) ;
#17292 = CYLINDRICAL_SURFACE ( 'NONE', #34528, 1.181102362204724310 ) ;
#17293 = EDGE_CURVE ( 'NONE', #10560, #71339, #72038, .T. ) ;
#17294 = CARTESIAN_POINT ( 'NONE',  ( 4.797336870675656522E-17, -0.3917322834645670104, 0.08661417322834651100 ) ) ;
#17295 = CARTESIAN_POINT ( 'NONE',  ( 0.8858267716535438430, 0.07958543189024085140, 0.2665933059059887866 ) ) ;
#17296 = ORIENTED_EDGE ( 'NONE', *, *, #6402, .T. ) ;
#17297 = CARTESIAN_POINT ( 'NONE',  ( -0.1058382717557497937, -0.3949938075777411628, -0.2296587926509187083 ) ) ;
#17298 = CARTESIAN_POINT ( 'NONE',  ( -1.003937007874014853, 0.1660481256975885056, 0.3530559997133364547 ) ) ;
#17299 = VERTEX_POINT ( 'NONE', #38632 ) ;
#17300 = CARTESIAN_POINT ( 'NONE',  ( -0.1574803149606292529, -0.1870078740157479769, 0.3641732283464567677 ) ) ;
#17301 = CARTESIAN_POINT ( 'NONE',  ( -1.725721784776902190, -0.05778040916215522460, 0.4822834645669289988 ) ) ;
#17302 = CARTESIAN_POINT ( 'NONE',  ( 0.4527559055118117182, -0.5400638737290844871, 0.3530559997133364547 ) ) ;
#17303 = CARTESIAN_POINT ( 'NONE',  ( 0.6167979002624678353, -0.4281496062992124485, 0.4176697321401328655 ) ) ;
#17304 = CARTESIAN_POINT ( 'NONE',  ( -0.1640419947506555343, -0.3162353388693405765, 0.4822834645669290543 ) ) ;
#17305 = CARTESIAN_POINT ( 'NONE',  ( -0.3917322834645671770, 0.1049643490035302024, -1.446869709482626831 ) ) ;
#17306 = CARTESIAN_POINT ( 'NONE',  ( -0.6430446194225712953, 0.05413385826771626580, -0.4176697321401330321 ) ) ;
#17307 = CARTESIAN_POINT ( 'NONE',  ( 0.1049643490035303689, 0.3917322834645670104, -2.597769028871390606 ) ) ;
#17308 = CARTESIAN_POINT ( 'NONE',  ( 1.122047244094488860, 0.07958543189024085140, 0.2665933059059887866 ) ) ;
#17309 = CARTESIAN_POINT ( 'NONE',  ( -0.9383202099737524282, -0.3162353388693409650, -0.4822834645669289433 ) ) ;
#17310 = CARTESIAN_POINT ( 'NONE',  ( 0.8464566929133866546, -0.5400638737290844871, 0.3530559997133364547 ) ) ;
#17311 = CARTESIAN_POINT ( 'NONE',  ( 1.089238845144357759, 0.05413385826771626580, -0.4176697321401330321 ) ) ;
#17312 = CARTESIAN_POINT ( 'NONE',  ( 0.1998031496062994405, -0.3460692066303958092, -0.7217847769028871152 ) ) ;
#17313 = CARTESIAN_POINT ( 'NONE',  ( -0.9383202099737524282, -0.05778040916215522460, 0.4822834645669289988 ) ) ;
#17314 = CARTESIAN_POINT ( 'NONE',  ( 0.3996062992125985480, 2.446882876249141654E-17, -0.1948818897637795422 ) ) ;
#17315 = CARTESIAN_POINT ( 'NONE',  ( 0.3740157480314966754, 0.1660481256975883668, -0.3530559997133364547 ) ) ;
#17316 = CARTESIAN_POINT ( 'NONE',  ( 4.893765752498283924E-17, -0.3996062992125986035, -2.125984251968504157 ) ) ;
#17317 = CARTESIAN_POINT ( 'NONE',  ( -0.5971128608923877978, -0.6692913385826773087, -0.1292274648535924053 ) ) ;
#17318 = CARTESIAN_POINT ( 'NONE',  ( -1.568241469816272105, -0.2845877964562161244, -0.3641732283464567121 ) ) ;
#17319 = CARTESIAN_POINT ( 'NONE',  ( 0.4855643044619430415, -0.3690944881889765550, -0.3153832671262227771 ) ) ;
#17320 = CARTESIAN_POINT ( 'NONE',  ( 0.8267716535433077274, 0.2952755905511811885, 0.000000000000000000 ) ) ;
#17321 = CARTESIAN_POINT ( 'NONE',  ( -0.1265901696524986964, -0.4724409448818899238, -1.251312335958005173 ) ) ;
#17322 = CARTESIAN_POINT ( 'NONE',  ( 0.7874015748031503170, -0.1870078740157480601, -0.3641732283464567677 ) ) ;
#17323 = CARTESIAN_POINT ( 'NONE',  ( 0.7808398950131240079, -0.3162353388693405765, 0.4822834645669290543 ) ) ;
#17324 = CARTESIAN_POINT ( 'NONE',  ( 0.3949938075777408852, 0.1058382717557500435, -0.5164041994750657727 ) ) ;
#17325 = CARTESIAN_POINT ( 'NONE',  ( -0.5971128608923877978, 0.2952755905511811885, 0.1292274648535926551 ) ) ;
#17326 = CARTESIAN_POINT ( 'NONE',  ( -0.1706036745406816491, 0.05413385826771626580, -0.4176697321401330321 ) ) ;
#17327 = CARTESIAN_POINT ( 'NONE',  ( 0.8202099737532813073, 0.1771653543307087630, 0.09757992244046791164 ) ) ;
#17328 = CARTESIAN_POINT ( 'NONE',  ( -0.6430446194225716283, -0.4281496062992124485, 0.4176697321401328655 ) ) ;
#17329 = CARTESIAN_POINT ( 'NONE',  ( -0.09186351706036689768, 0.05413385826771626580, -0.4176697321401330321 ) ) ;
#17330 = CYLINDRICAL_SURFACE ( 'NONE', #78942, 0.4724409448818898682 ) ;
#17331 = CARTESIAN_POINT ( 'NONE',  ( -0.006561679790025524116, -0.3162353388693405765, 0.4822834645669290543 ) ) ;
#17332 = CARTESIAN_POINT ( 'NONE',  ( 0.1771653543307093182, -0.4536011799217368745, -0.2665933059059886201 ) ) ;
#17333 = CARTESIAN_POINT ( 'NONE',  ( -2.776658174029175363, 1.170105060311657619, 0.3006284332565994366 ) ) ;
#17334 = CARTESIAN_POINT ( 'NONE',  ( 0.1706036745406830368, -0.3690944881889765550, -0.3153832671262227771 ) ) ;
#17335 = CARTESIAN_POINT ( 'NONE',  ( 0.7414698162729663755, -0.5511811023622048555, -0.09757992244046775898 ) ) ;
#17336 = DIRECTION ( 'NONE',  ( 0.000000000000000000, 0.000000000000000000, 1.000000000000000000 ) ) ;
#17337 = CARTESIAN_POINT ( 'NONE',  ( -0.1998031496062994405, 0.3460692066303957537, -1.664698162729658870 ) ) ;
#17338 = CARTESIAN_POINT ( 'NONE',  ( 0.2099737532808405305, -0.6046776061558807314, 0.2411417322834647770 ) ) ;
#17339 = CARTESIAN_POINT ( 'NONE',  ( -0.1049643490035307020, 0.3917322834645669549, -1.573490813648293907 ) ) ;
#17340 = FACE_OUTER_BOUND ( 'NONE', #68334, .T. ) ;
#17341 = CARTESIAN_POINT ( 'NONE',  ( -0.3913445824879501211, 0.02733964191758146006, 1.458593243026434070E-17 ) ) ;
#17342 = CARTESIAN_POINT ( 'NONE',  ( -0.3937007874015740483, -0.1870078740157480601, -0.3641732283464567677 ) ) ;
#17343 = EDGE_CURVE ( 'NONE', #20923, #9917, #71539, .T. ) ;
#17344 = CARTESIAN_POINT ( 'NONE',  ( -0.2493438320209966919, -0.4281496062992124485, 0.4176697321401328655 ) ) ;
#17345 = CARTESIAN_POINT ( 'NONE',  ( 1.102362204724410155, -0.1870078740157480601, -0.3641732283464567677 ) ) ;
#17346 = CARTESIAN_POINT ( 'NONE',  ( 0.1085784267831624711, 1.075318549932396728, -1.116887896051823814 ) ) ;
#17347 = CARTESIAN_POINT ( 'NONE',  ( -1.325459317585300889, -0.4281496062992127816, -0.4176697321401328100 ) ) ;
#17348 = EDGE_CURVE ( 'NONE', #77755, #58154, #69486, .T. ) ;
#17349 = CARTESIAN_POINT ( 'NONE',  ( 0.1706036745406830368, -0.4281496062992127816, -0.4176697321401328100 ) ) ;
#17350 = CARTESIAN_POINT ( 'NONE',  ( 1.286089238845145033, -0.6046776061558809534, -0.2411417322834644161 ) ) ;
#17351 = CARTESIAN_POINT ( 'NONE',  ( 0.4122598602536549084, 1.300945800302083288, -2.057903956725271488 ) ) ;
#17352 = CARTESIAN_POINT ( 'NONE',  ( 0.09186351706036799403, -0.4281496062992127816, -0.4176697321401328100 ) ) ;
#17353 = CARTESIAN_POINT ( 'NONE',  ( 1.266404199475066328, -0.3162353388693409650, -0.4822834645669289433 ) ) ;
#17354 = CARTESIAN_POINT ( 'NONE',  ( 0.4461942257217856311, 0.2306618581243847221, -0.2411417322834647770 ) ) ;
#17355 = CARTESIAN_POINT ( 'NONE',  ( -1.603475055217291612, 1.330568129716839909, -0.04573490813648262154 ) ) ;
#17356 = CARTESIAN_POINT ( 'NONE',  ( 0.8202099737532814183, -0.5511811023622048555, -0.09757992244046775898 ) ) ;
#17357 = CARTESIAN_POINT ( 'NONE',  ( 1.115485564304462551, -0.4281496062992127816, -0.4176697321401328100 ) ) ;
#17358 = CARTESIAN_POINT ( 'NONE',  ( 0.2296587926509192634, -0.08942795157528024563, -0.3641732283464568787 ) ) ;
#17359 = CARTESIAN_POINT ( 'NONE',  ( -0.3346456692913377662, 0.1660481256975883668, -0.3530559997133364547 ) ) ;
#17360 = CARTESIAN_POINT ( 'NONE',  ( 0.7677165354330716118, -0.5400638737290844871, 0.3530559997133364547 ) ) ;
#17361 = CARTESIAN_POINT ( 'NONE',  ( -0.6233595800524928121, -0.3162353388693409650, -0.4822834645669289433 ) ) ;
#17362 = CARTESIAN_POINT ( 'NONE',  ( 4.797336870675656522E-17, -0.3917322834645670659, -2.122722727855329783 ) ) ;
#17363 = CARTESIAN_POINT ( 'NONE',  ( -0.08530183727034056085, -0.08942795157528024563, -0.3641732283464568787 ) ) ;
#17364 = CARTESIAN_POINT ( 'NONE',  ( 0.6955380577427828781, 0.05413385826771626580, -0.4176697321401330321 ) ) ;
#17365 = CARTESIAN_POINT ( 'NONE',  ( 1.003937007874016407, -0.4536011799217367080, 0.2665933059059888421 ) ) ;
#17366 = CARTESIAN_POINT ( 'NONE',  ( 0.02624671916010564918, -0.6046776061558809534, -0.2411417322834644161 ) ) ;
#17367 = DIRECTION ( 'NONE',  ( -0.000000000000000000, 1.000000000000000000, -0.000000000000000000 ) ) ;
#17369 = CARTESIAN_POINT ( 'NONE',  ( 1.574803149606299746, -0.1870078740157479769, 0.4822834645669291653 ) ) ;
#17368 = LINE ( 'NONE', #74609, #19103 ) ;
#17370 = CARTESIAN_POINT ( 'NONE',  ( 0.2867679344610366554, -0.2867679344610365444, -2.137795275590550936 ) ) ;
#17371 = CARTESIAN_POINT ( 'NONE',  ( -1.430446194225720724, 0.05413385826771626580, -0.4176697321401330321 ) ) ;
#17372 = CARTESIAN_POINT ( 'NONE',  ( -0.3412073490813641308, -0.6046776061558807314, 0.2411417322834647770 ) ) ;
#17373 = CARTESIAN_POINT ( 'NONE',  ( 0.2362204724409449064, 0.4091458600556404646, -0.4593175853018372501 ) ) ;
#17374 = CARTESIAN_POINT ( 'NONE',  ( -0.2891555358219911054, 0.2891555358219909388, -2.854330708661418026 ) ) ;
#17375 = EDGE_LOOP ( 'NONE', ( #46472, #55670, #58351, #17281 ) ) ;
#17376 = CARTESIAN_POINT ( 'NONE',  ( 0.2296587926509192634, -0.2845877964562159024, 0.3641732283464567677 ) ) ;
#17377 = CARTESIAN_POINT ( 'NONE',  ( 0.3392501089628018329, 0.1958661417322835607, -1.540682414698162805 ) ) ;
#17378 = CARTESIAN_POINT ( 'NONE',  ( 0.8923884514435701520, -0.6046776061558809534, -0.2411417322834644161 ) ) ;
#17379 = CARTESIAN_POINT ( 'NONE',  ( 0.3458507752293908943, -0.3458507752293908943, -2.618110236220472675 ) ) ;
#17380 = CARTESIAN_POINT ( 'NONE',  ( 0.9580052493438326877, 0.05413385826771666132, 0.4176697321401328100 ) ) ;
#17381 = CARTESIAN_POINT ( 'NONE',  ( -1.653543307086613234, -0.1870078740157480601, -0.3641732283464567677 ) ) ;
#17382 = CARTESIAN_POINT ( 'NONE',  ( 1.167979002624672580, -0.4281496062992124485, 0.4176697321401328655 ) ) ;
#17383 = CARTESIAN_POINT ( 'NONE',  ( 1.515748031496063186, -0.4536011799217368745, -0.2665933059059886201 ) ) ;
#17384 = CARTESIAN_POINT ( 'NONE',  ( 0.3871391076115493490, -0.3162353388693405765, 0.4822834645669290543 ) ) ;
#17385 = CARTESIAN_POINT ( 'NONE',  ( 0.2867679344610365999, 0.2867679344610365999, -0.5327890831682923212 ) ) ;
#17386 = CARTESIAN_POINT ( 'NONE',  ( -0.3018372703412066094, -0.4281496062992127816, -0.4176697321401328100 ) ) ;
#17387 = CARTESIAN_POINT ( 'NONE',  ( -1.036745406824146176, -0.004921259842519870586, -0.3153832671262229437 ) ) ;
#17388 = CARTESIAN_POINT ( 'NONE',  ( 0.2559055118110243332, -0.5400638737290845981, -0.3530559997133363437 ) ) ;
#17389 = CARTESIAN_POINT ( 'NONE',  ( 0.07874015748031558404, -0.1870078740157480879, -0.4822834645669291653 ) ) ;
#17390 = CARTESIAN_POINT ( 'NONE',  ( 0.4614150585118587666, 1.648843903847227566, 3.909876957777870476 ) ) ;
#17391 = CARTESIAN_POINT ( 'NONE',  ( 0.6418543022643073970, 2.377811541467197069E-16, 0.3627985898453514602 ) ) ;
#17392 = CARTESIAN_POINT ( 'NONE',  ( 0.3917322834645670104, 0.1049643490035304660, -2.168654486385513724 ) ) ;
#17393 = CARTESIAN_POINT ( 'NONE',  ( 0.5905511811023629321, 0.2952755905511811885, 0.000000000000000000 ) ) ;
#17394 = CARTESIAN_POINT ( 'NONE',  ( -0.4002624671916004129, -0.05778040916215560624, -0.4822834645669293319 ) ) ;
#17395 = CARTESIAN_POINT ( 'NONE',  ( -1.410761154855641575, -0.3162353388693409650, -0.4822834645669289433 ) ) ;
#17396 = VECTOR ( 'NONE', #66165, 39.37007874015748143 ) ;
#17397 = CARTESIAN_POINT ( 'NONE',  ( 1.246719160104987623, -0.4281496062992124485, 0.4176697321401328655 ) ) ;
#17398 = CARTESIAN_POINT ( 'NONE',  ( 0.3149606299212606708, -0.1870078740157480879, -0.4822834645669291653 ) ) ;
#17399 = CARTESIAN_POINT ( 'NONE',  ( 0.2867679344610365999, 0.2867679344610365999, -1.009842519685039353 ) ) ;
#17400 = CARTESIAN_POINT ( 'NONE',  ( -0.9186351706036736120, 0.2306618581243848609, 0.2411417322834645549 ) ) ;
#17401 = CARTESIAN_POINT ( 'NONE',  ( 0.03280839895013198948, -0.6692913385826773087, -0.1292274648535924053 ) ) ;
#17402 = CARTESIAN_POINT ( 'NONE',  ( -0.3937007874015740483, -0.1870078740157479769, 0.4822834645669291653 ) ) ;
#17403 = CARTESIAN_POINT ( 'NONE',  ( 0.1837270341207357105, -0.5023911411419708095, -0.1820866141732282451 ) ) ;
#17404 = CARTESIAN_POINT ( 'NONE',  ( 1.581364829396326277, -0.2845877964562161244, -0.3641732283464567121 ) ) ;
#17405 = CARTESIAN_POINT ( 'NONE',  ( -0.4606671848300740169, 1.422950954677616897, -2.585357360710740515 ) ) ;
#17406 = CARTESIAN_POINT ( 'NONE',  ( 0.1968503937007881344, 0.2952755905511811885, 0.000000000000000000 ) ) ;
#17407 = CYLINDRICAL_SURFACE ( 'NONE', #50658, 0.2952755905511810774 ) ;
#17408 = CARTESIAN_POINT ( 'NONE',  ( -1.581364829396324945, -0.05778040916215560624, -0.4822834645669293319 ) ) ;
#17409 = CARTESIAN_POINT ( 'NONE',  ( -0.1958661417322836718, 0.3392501089628017219, -2.839895013123359568 ) ) ;
#17410 = EDGE_LOOP ( 'NONE', ( #8296, #46770, #252, #19312 ) ) ;
#17411 = ORIENTED_EDGE ( 'NONE', *, *, #7637, .F. ) ;
#17412 = CARTESIAN_POINT ( 'NONE',  ( 0.8530183727034128527, -0.4281496062992124485, 0.4176697321401328655 ) ) ;
#17413 = CARTESIAN_POINT ( 'NONE',  ( 0.006561679790026889343, -0.08942795157527998196, 0.3641732283464567121 ) ) ;
#17415 = CARTESIAN_POINT ( 'NONE',  ( -3.264097702071373064, 2.755905511811024056, -0.5314960629921260393 ) ) ;
#17414 = CARTESIAN_POINT ( 'NONE',  ( -1.028793376639876023, 1.694622884024324261, 0.4478856567166526470 ) ) ;
#17416 = CARTESIAN_POINT ( 'NONE',  ( 0.3392501089628018329, 0.1958661417322835607, -0.8458005249343831800 ) ) ;
#17417 = CARTESIAN_POINT ( 'NONE',  ( -0.4724409448818898682, -8.678599364036362592E-17, 0.1988188976377952832 ) ) ;
#17418 = CARTESIAN_POINT ( 'NONE',  ( 0.3460692066303959202, -0.1998031496062991630, -2.229002624671915900 ) ) ;
#17419 = CARTESIAN_POINT ( 'NONE',  ( 0.5708661417322841158, -0.5400638737290845981, -0.3530559997133363437 ) ) ;
#17420 = CARTESIAN_POINT ( 'NONE',  ( -0.7283464566929126471, -0.5400638737290844871, 0.3530559997133364547 ) ) ;
#17421 = CARTESIAN_POINT ( 'NONE',  ( -0.8070866141732276899, -0.5400638737290844871, 0.3530559997133364547 ) ) ;
#17422 = CARTESIAN_POINT ( 'NONE',  ( 0.6233595800524939223, -0.3162353388693405765, 0.4822834645669290543 ) ) ;
#17423 = CARTESIAN_POINT ( 'NONE',  ( 1.476377952755906220, 0.1660481256975883668, -0.3530559997133364547 ) ) ;
#17424 = CARTESIAN_POINT ( 'NONE',  ( 1.437007874015748810, -0.4536011799217368745, -0.2665933059059886201 ) ) ;
#17425 = CARTESIAN_POINT ( 'NONE',  ( 1.430446194225722500, -0.3690944881889765550, -0.3153832671262227771 ) ) ;
#17426 = CARTESIAN_POINT ( 'NONE',  ( -0.6955380577427815458, 0.05413385826771666132, 0.4176697321401328100 ) ) ;
#17427 = CARTESIAN_POINT ( 'NONE',  ( -0.1070741851644056997, 0.3996062992125984925, -0.5557742782152230721 ) ) ;
#17428 = CARTESIAN_POINT ( 'NONE',  ( 1.437007874015748810, -0.5400638737290845981, -0.3530559997133363437 ) ) ;
#17429 = CARTESIAN_POINT ( 'NONE',  ( 4.797336870675656522E-17, -0.3917322834645670104, -0.07086614173228342195 ) ) ;
#17430 = CARTESIAN_POINT ( 'NONE',  ( -0.04593175853018302557, 0.2952755905511811885, 0.1292274648535926551 ) ) ;
#17432 = LINE ( 'NONE', #10282, #45243 ) ;
#17431 = CARTESIAN_POINT ( 'NONE',  ( 0.9842519685039378130, -0.6692913385826771977, 8.415575281601705876E-17 ) ) ;
#17433 = CARTESIAN_POINT ( 'NONE',  ( -1.312335958005248715, -0.5023911411419708095, -0.1820866141732282451 ) ) ;
#17434 = CARTESIAN_POINT ( 'NONE',  ( 0.4133858267716541968, 0.1660481256975885056, 0.3530559997133364547 ) ) ;
#17435 = CARTESIAN_POINT ( 'NONE',  ( 0.9842519685039375910, 0.1771653543307087630, 0.000000000000000000 ) ) ;
#17436 = EDGE_CURVE ( 'NONE', #59949, #49068, #45766, .T. ) ;
#17437 = CARTESIAN_POINT ( 'NONE',  ( 0.2867679344610365999, -0.2867679344610365999, -1.753261524113173708 ) ) ;
#17438 = CARTESIAN_POINT ( 'NONE',  ( -1.259842519685038686, -0.1870078740157479769, 0.3641732283464567677 ) ) ;
#17439 = CARTESIAN_POINT ( 'NONE',  ( 1.233595800524935227, 0.2306618581243847221, -0.2411417322834647770 ) ) ;
#17440 = LINE ( 'NONE', #76327, #27672 ) ;
#17441 = CARTESIAN_POINT ( 'NONE',  ( -0.6758530183727028406, -0.5511811023622048555, -0.09757992244046775898 ) ) ;
#17442 = CARTESIAN_POINT ( 'NONE',  ( -0.1771653543307080136, -0.5400638737290844871, 0.3530559997133364547 ) ) ;
#17443 = CARTESIAN_POINT ( 'NONE',  ( -1.207349081364828436, -0.5023911411419708095, 0.1820866141732285504 ) ) ;
#17444 = CARTESIAN_POINT ( 'NONE',  ( -0.6692913385826764205, -0.6692913385826771977, 8.415575281601705876E-17 ) ) ;
#17445 = CARTESIAN_POINT ( 'NONE',  ( 1.246719160104987623, 0.05413385826771626580, -0.4176697321401330321 ) ) ;
#17446 = CARTESIAN_POINT ( 'NONE',  ( 0.3917322834645670659, 2.398668435337828261E-17, -0.5872896569891882246 ) ) ;
#17447 = CARTESIAN_POINT ( 'NONE',  ( -0.9580052493438311334, -0.004921259842519870586, -0.3153832671262229437 ) ) ;
#17448 = CARTESIAN_POINT ( 'NONE',  ( 1.084092808546051057, 1.161348697294517951, 0.2896277429123272351 ) ) ;
#17449 = CARTESIAN_POINT ( 'NONE',  ( 1.555118110236221041, -0.5400638737290844871, 0.3530559997133364547 ) ) ;
#17450 = CARTESIAN_POINT ( 'NONE',  ( 0.2362204724409451007, -0.4091458600556402980, -2.215879265091863726 ) ) ;
#17451 = CARTESIAN_POINT ( 'NONE',  ( -1.076115485564303809, 0.2306618581243848609, 0.2411417322834645549 ) ) ;
#17452 = CARTESIAN_POINT ( 'NONE',  ( -1.266404199475064773, -0.08942795157528024563, -0.3641732283464568787 ) ) ;
#17453 = CARTESIAN_POINT ( 'NONE',  ( -0.4265091863517051496, 0.1771653543307087075, -0.09757992244046823083 ) ) ;
#17454 = LINE ( 'NONE', #61212, #44667 ) ;
#17455 = CARTESIAN_POINT ( 'NONE',  ( 0.006561679790026889343, -0.3162353388693409650, -0.4822834645669289433 ) ) ;
#17456 = CARTESIAN_POINT ( 'NONE',  ( -0.2165354330708654795, 0.07958543189024085140, 0.2665933059059887866 ) ) ;
#17457 = CARTESIAN_POINT ( 'NONE',  ( -1.174540682414697335, -0.2845877964562161244, -0.3641732283464567121 ) ) ;
#17458 = CARTESIAN_POINT ( 'NONE',  ( -1.614173228346456268, -0.6692913385826771977, 8.415575281601705876E-17 ) ) ;
#17459 = CARTESIAN_POINT ( 'NONE',  ( 1.345144356955381593, -0.2845877964562161244, -0.3641732283464567121 ) ) ;
#17460 = CARTESIAN_POINT ( 'NONE',  ( 1.049868766404200349, 0.2306618581243848609, 0.2411417322834645549 ) ) ;
#17461 = DIRECTION ( 'NONE',  ( 0.000000000000000000, -1.000000000000000000, 0.000000000000000000 ) ) ;
#17462 = CARTESIAN_POINT ( 'NONE',  ( 0.5052493438320218022, -0.5511811023622048555, -0.09757992244046775898 ) ) ;
#17463 = CARTESIAN_POINT ( 'NONE',  ( 1.069553805774278832, 0.2952755905511810774, -0.1292274648535930714 ) ) ;
#17464 = CARTESIAN_POINT ( 'NONE',  ( 0.9580052493438326877, -0.004921259842519576551, 0.3153832671262227771 ) ) ;
#17465 = ORIENTED_EDGE ( 'NONE', *, *, #58706, .T. ) ;
#17466 = CARTESIAN_POINT ( 'NONE',  ( -1.345144356955379816, -0.3162353388693405765, 0.4822834645669290543 ) ) ;
#17467 = CARTESIAN_POINT ( 'NONE',  ( -1.010498687664041384, 0.05413385826771666132, 0.4176697321401328100 ) ) ;
#17468 = CARTESIAN_POINT ( 'NONE',  ( -0.1181102362204717315, 0.2952755905511811885, 0.000000000000000000 ) ) ;
#17469 = CARTESIAN_POINT ( 'NONE',  ( -1.706036745406823485, 0.1283753931104748280, 0.1820866141732283561 ) ) ;
#17470 = CARTESIAN_POINT ( 'NONE',  ( 4.893765752498283308E-17, -0.3996062992125985480, -2.675196850393700920 ) ) ;
#17471 = CARTESIAN_POINT ( 'NONE',  ( 0.2690288713910767848, -0.6692913385826773087, -0.1292274648535924053 ) ) ;
#17472 = CARTESIAN_POINT ( 'NONE',  ( 1.325459317585302665, -0.004921259842519870586, -0.3153832671262229437 ) ) ;
#17473 = CARTESIAN_POINT ( 'NONE',  ( 0.03280839895013198948, -0.6692913385826773087, -0.1292274648535924053 ) ) ;
#17474 = CARTESIAN_POINT ( 'NONE',  ( 0.5905511811023629321, -0.6692913385826771977, 8.415575281601705876E-17 ) ) ;
#17475 = CARTESIAN_POINT ( 'NONE',  ( 0.1998031496062992740, 0.3460692066303959757, -1.876640419947506411 ) ) ;
#17476 = CARTESIAN_POINT ( 'NONE',  ( 0.1058382717557500713, -0.3949938075777409408, -1.345144356955380704 ) ) ;
#17477 = CARTESIAN_POINT ( 'NONE',  ( -0.4589048803027434009, 1.413024577066673615, 1.023935092353904563 ) ) ;
#17478 = CARTESIAN_POINT ( 'NONE',  ( 3.911446811352371711, 1.694514647449913092, 0.4479265895742980397 ) ) ;
#17479 = CARTESIAN_POINT ( 'NONE',  ( -9.594673741351313045E-17, 0.3917322834645670104, -0.4645669291338582751 ) ) ;
#17480 = CARTESIAN_POINT ( 'NONE',  ( -0.3740157480314953431, -0.4536011799217368745, -0.2665933059059886201 ) ) ;
#17481 = CARTESIAN_POINT ( 'NONE',  ( -0.7677165354330699465, 0.1660481256975885056, 0.3530559997133364547 ) ) ;
#17482 = CARTESIAN_POINT ( 'NONE',  ( 0.5774278215223103139, -0.6046776061558809534, -0.2411417322834644161 ) ) ;
#17483 = CARTESIAN_POINT ( 'NONE',  ( -0.3420746716998660508, -0.1974969037888706924, -2.176509186351706759 ) ) ;
#17484 = CARTESIAN_POINT ( 'NONE',  ( 0.9776902887139113929, -0.6692913385826773087, -0.1292274648535924053 ) ) ;
#17485 = CARTESIAN_POINT ( 'NONE',  ( 1.601049868766404982, 0.2306618581243848609, 0.2411417322834645549 ) ) ;
#17486 = CARTESIAN_POINT ( 'NONE',  ( 1.312335958005249825, 0.2306618581243847221, -0.2411417322834647770 ) ) ;
#17487 = CARTESIAN_POINT ( 'NONE',  ( 0.4091458600556404646, -0.2362204724409448231, -2.467191601049868677 ) ) ;
#17488 = CARTESIAN_POINT ( 'NONE',  ( -0.3460692066303958092, -0.1998031496062994683, -1.784776902887138972 ) ) ;
#17489 = CARTESIAN_POINT ( 'NONE',  ( 0.4091458600556403535, 0.2362204724409449896, -2.727690288713910949 ) ) ;
#17490 = CARTESIAN_POINT ( 'NONE',  ( 1.003937007874016185, 0.1660481256975883668, -0.3530559997133364547 ) ) ;
#17491 = CARTESIAN_POINT ( 'NONE',  ( 0.5052493438320215802, 0.2952755905511811885, 0.1292274648535926551 ) ) ;
#17492 = CARTESIAN_POINT ( 'NONE',  ( 1.200787401574803681, -0.4536011799217368745, -0.2665933059059886201 ) ) ;
#17494 = CARTESIAN_POINT ( 'NONE',  ( 1.548556430446194954, -0.6046776061558807314, 0.2411417322834647770 ) ) ;
#17493 = CARTESIAN_POINT ( 'NONE',  ( 1.660104986876641320, -0.05778040916215522460, 0.4822834645669289988 ) ) ;
#17495 = CARTESIAN_POINT ( 'NONE',  ( -0.3917322834645669549, -0.1049643490035306603, 0.1843832020997374643 ) ) ;
#17496 = DIRECTION ( 'NONE',  ( 0.000000000000000000, 1.000000000000000000, -0.000000000000000000 ) ) ;
#17497 = CARTESIAN_POINT ( 'NONE',  ( 0.7677165354330716118, 0.1660481256975883668, -0.3530559997133364547 ) ) ;
#17498 = CARTESIAN_POINT ( 'NONE',  ( 1.614173228346457378, -0.5511811023622047445, 6.969142054262312111E-17 ) ) ;
#17499 = CARTESIAN_POINT ( 'NONE',  ( -0.4265091863517051496, 0.2952755905511810774, -0.1292274648535930714 ) ) ;
#17500 = CARTESIAN_POINT ( 'NONE',  ( -0.4068241469816267775, 0.05413385826771626580, -0.4176697321401330321 ) ) ;
#17501 = CARTESIAN_POINT ( 'NONE',  ( -1.633858267716534529, 0.1660481256975885056, 0.3530559997133364547 ) ) ;
#17502 = CARTESIAN_POINT ( 'NONE',  ( -0.1049643490035307020, 0.3917322834645669549, -0.2486876640419948270 ) ) ;
#17503 = CARTESIAN_POINT ( 'NONE',  ( -0.1958661417322836718, 0.3392501089628017219, -1.422572178477690574 ) ) ;
#17504 = CARTESIAN_POINT ( 'NONE',  ( 0.3917322834645669549, 0.1049643490035304660, -2.479002624671915900 ) ) ;
#17505 = CARTESIAN_POINT ( 'NONE',  ( 1.660104986876641320, -0.05778040916215522460, 0.4822834645669289988 ) ) ;
#17506 = ORIENTED_EDGE ( 'NONE', *, *, #76145, .F. ) ;
#17507 = CARTESIAN_POINT ( 'NONE',  ( -9.674558042662121740E-17, 0.3949938075777409963, -2.519685039370078705 ) ) ;
#17508 = ORIENTED_EDGE ( 'NONE', *, *, #42986, .F. ) ;
#17509 = CARTESIAN_POINT ( 'NONE',  ( -0.03443470937339728616, 1.062992125984252079, -1.537015892239756099 ) ) ;
#17510 = CARTESIAN_POINT ( 'NONE',  ( 1.364829396325459854, -0.5023911411419708095, -0.1820866141732282451 ) ) ;
#17511 = CARTESIAN_POINT ( 'NONE',  ( 0.1070741851644053527, 0.3996062992125986590, -1.095800524934382958 ) ) ;
#17512 = CARTESIAN_POINT ( 'NONE',  ( 1.601049868766404982, -0.5023911411419708095, -0.1820866141732282451 ) ) ;
#17513 = CARTESIAN_POINT ( 'NONE',  ( -0.09151288181857039628, 0.004960608223779798542, -0.3437734562760185186 ) ) ;
#17514 = DIRECTION ( 'NONE',  ( 0.000000000000000000, -1.000000000000000000, 0.000000000000000000 ) ) ;
#17515 = CARTESIAN_POINT ( 'NONE',  ( -0.2570577095524356759, 1.875999552332453746, 0.1790154821377908934 ) ) ;
#17516 = CARTESIAN_POINT ( 'NONE',  ( -0.2867679344610365999, 0.2867679344610364889, -0.5767716535433071723 ) ) ;
#17517 = CARTESIAN_POINT ( 'NONE',  ( -0.5905511811023613777, -0.5511811023622047445, 6.969142054262312111E-17 ) ) ;
#17518 = CARTESIAN_POINT ( 'NONE',  ( -1.286089238845143479, -0.5023911411419708095, 0.1820866141732285504 ) ) ;
#17519 = CARTESIAN_POINT ( 'NONE',  ( 0.5446194225721792126, -0.05778040916215560624, -0.4822834645669293319 ) ) ;
#17520 = CARTESIAN_POINT ( 'NONE',  ( -1.227034120734907141, -0.6692913385826773087, -0.1292274648535924053 ) ) ;
#17521 = CARTESIAN_POINT ( 'NONE',  ( 0.1958661417322834775, 0.3392501089628018884, -0.1364829396325459021 ) ) ;
#17522 = ORIENTED_EDGE ( 'NONE', *, *, #70814, .T. ) ;
#17523 = CARTESIAN_POINT ( 'NONE',  ( 1.371391076115485719, -0.6692913385826773087, -0.1292274648535924053 ) ) ;
#17524 = DIRECTION ( 'NONE',  ( 1.000000000000000000, 0.000000000000000000, 3.455050906509825972E-15 ) ) ;
#17525 = LENGTH_MEASURE_WITH_UNIT ( LENGTH_MEASURE( 0.02539999999999999897 ), #54554 );
#17526 = CARTESIAN_POINT ( 'NONE',  ( -0.2362204724409447953, -0.4091458600556404646, -1.797900262467191590 ) ) ;
#17527 = PLANE ( 'NONE',  #29077 ) ;
#17528 = ADVANCED_FACE ( 'NONE', ( #19270 ), #52498, .F. ) ;
#17529 = CARTESIAN_POINT ( 'NONE',  ( 0.1265901696524989184, 0.4724409448818898127, -0.9383202099737532054 ) ) ;
#17530 = CARTESIAN_POINT ( 'NONE',  ( -0.6889763779527552368, 0.1660481256975885056, 0.3530559997133364547 ) ) ;
#17531 = CARTESIAN_POINT ( 'NONE',  ( 0.8267716535433078384, -0.6692913385826771977, 8.415575281601705876E-17 ) ) ;
#17532 = DIRECTION ( 'NONE',  ( 0.000000000000000000, -0.000000000000000000, 1.000000000000000000 ) ) ;
#17533 = CARTESIAN_POINT ( 'NONE',  ( 1.437007874015748810, -0.5400638737290845981, -0.3530559997133363437 ) ) ;
#17534 = CARTESIAN_POINT ( 'NONE',  ( -1.305774278215222184, -0.6692913385826773087, -0.1292274648535924053 ) ) ;
#17535 = CARTESIAN_POINT ( 'NONE',  ( 0.1958661417322834497, 0.3392501089628018329, -0.5393507629583185192 ) ) ;
#17536 = CARTESIAN_POINT ( 'NONE',  ( 0.2362204724409456558, -0.1870078740157480601, -0.3641732283464567677 ) ) ;
#17537 = CARTESIAN_POINT ( 'NONE',  ( -9.594673741351313045E-17, 0.3917322834645670104, -0.5570866141732284671 ) ) ;
#17538 = CARTESIAN_POINT ( 'NONE',  ( 0.09186351706036827158, -0.004921259842519576551, 0.3153832671262227771 ) ) ;
#17539 = CARTESIAN_POINT ( 'NONE',  ( 0.7283464566929140904, -0.4536011799217368745, -0.2665933059059886201 ) ) ;
#17540 = CARTESIAN_POINT ( 'NONE',  ( 0.6758530183727039509, 0.2952755905511810774, -0.1292274648535930714 ) ) ;
#17541 = CARTESIAN_POINT ( 'NONE',  ( -0.7545931758530176614, -0.5511811023622048555, -0.09757992244046775898 ) ) ;
#17542 = CARTESIAN_POINT ( 'NONE',  ( -9.594673741351313045E-17, 0.3917322834645670104, -2.354330708661417138 ) ) ;
#17543 = CARTESIAN_POINT ( 'NONE',  ( 1.587926509186352142, 0.05413385826771666132, 0.4176697321401328100 ) ) ;
#17544 = CARTESIAN_POINT ( 'NONE',  ( -1.161417322834644716, 0.1660481256975885056, 0.3530559997133364547 ) ) ;
#17545 = CARTESIAN_POINT ( 'NONE',  ( -0.2362204724409447953, -0.4091458600556404646, -0.6148293963254594097 ) ) ;
#17546 = CARTESIAN_POINT ( 'NONE',  ( -0.1312335958005241554, 0.2306618581243848609, 0.2411417322834645549 ) ) ;
#17547 = CARTESIAN_POINT ( 'NONE',  ( -0.5183727034120726440, 0.2952755905511811885, 0.1292274648535926551 ) ) ;
#17548 = CARTESIAN_POINT ( 'NONE',  ( 1.174540682414699111, -0.2845877964562159024, 0.3641732283464567677 ) ) ;
#17549 = CARTESIAN_POINT ( 'NONE',  ( 0.2755905511811031494, -0.5511811023622047445, 6.969142054262312111E-17 ) ) ;
#17550 = CARTESIAN_POINT ( 'NONE',  ( -0.01968503937007793844, -0.5400638737290844871, 0.3530559997133364547 ) ) ;
#17551 = CARTESIAN_POINT ( 'NONE',  ( -0.9383202099737524282, -0.3162353388693409650, -0.4822834645669289433 ) ) ;
#17552 = CARTESIAN_POINT ( 'NONE',  ( -3.831929248781927200, 2.755905511811024056, 0.5314960629921259283 ) ) ;
#17553 = CARTESIAN_POINT ( 'NONE',  ( -0.4091458600556405756, 0.2362204724409446288, -0.3412073490813647969 ) ) ;
#17554 = CARTESIAN_POINT ( 'NONE',  ( 0.01312335958005323398, -0.4281496062992127816, -0.4176697321401328100 ) ) ;
#17555 = ORIENTED_EDGE ( 'NONE', *, *, #4697, .T. ) ;
#17556 = CARTESIAN_POINT ( 'NONE',  ( -0.3460692066303960313, 0.1998031496062989965, -1.992782152230971437 ) ) ;
#17557 = CARTESIAN_POINT ( 'NONE',  ( 0.9776902887139113929, 0.2952755905511811885, 0.1292274648535926551 ) ) ;
#17558 = B_SPLINE_CURVE_WITH_KNOTS ( 'NONE', 3,
 ( #70394, #80274, #48249, #29314 ),
 .UNSPECIFIED., .F., .F.,
 ( 4, 4 ),
 ( 1.734723475976807094E-18, 0.001346657832036806226 ),
 .UNSPECIFIED. ) ;
#17559 = CARTESIAN_POINT ( 'NONE',  ( -0.8398950131233589023, -0.5023911411419708095, -0.1820866141732282451 ) ) ;
#17560 = CARTESIAN_POINT ( 'NONE',  ( -0.6299212598425188991, -0.1870078740157479769, 0.4822834645669291653 ) ) ;
#17561 = CARTESIAN_POINT ( 'NONE',  ( 1.141732283464567788, -0.6692913385826771977, 8.415575281601705876E-17 ) ) ;
#17562 = CARTESIAN_POINT ( 'NONE',  ( 0.8070866141732289112, -0.5400638737290845981, -0.3530559997133363437 ) ) ;
#17563 = CARTESIAN_POINT ( 'NONE',  ( -1.541994750656167090, -0.6692913385826773087, -0.1292274648535924053 ) ) ;
#17564 = CARTESIAN_POINT ( 'NONE',  ( -0.9842519685039365918, -0.5511811023622047445, 6.969142054262312111E-17 ) ) ;
#17565 = CARTESIAN_POINT ( 'NONE',  ( 0.1070741851644053527, 0.3996062992125985480, -0.07020997375328086321 ) ) ;
#17566 = CARTESIAN_POINT ( 'NONE',  ( -0.1070741851644056997, 0.3996062992125986035, -0.3215223097112860362 ) ) ;
#17567 = CARTESIAN_POINT ( 'NONE',  ( 0.1974969037888704704, 0.3420746716998660508, -0.3018372703412073865 ) ) ;
#17568 = CARTESIAN_POINT ( 'NONE',  ( 0.03178304480586199854, -0.3983403474834772418, -9.560572922657961637E-16 ) ) ;
#17569 = CARTESIAN_POINT ( 'NONE',  ( 0.6430446194225728496, -0.004921259842519576551, 0.3153832671262227771 ) ) ;
#17570 = CARTESIAN_POINT ( 'NONE',  ( 0.5380577427821529035, 0.05413385826771626580, -0.4176697321401330321 ) ) ;
#17571 = CARTESIAN_POINT ( 'NONE',  ( 0.2140388612101737920, -0.2035438835850314487, 0.1320934087364891707 ) ) ;
#17572 = CARTESIAN_POINT ( 'NONE',  ( 0.2891555358219910499, -0.2891555358219909944, -0.9625984251968502381 ) ) ;
#17573 = CARTESIAN_POINT ( 'NONE',  ( 0.7020997375328090762, -0.2845877964562159024, 0.3641732283464567677 ) ) ;
#17574 = CARTESIAN_POINT ( 'NONE',  ( -0.4921259842519677963, 0.1660481256975883668, -0.3530559997133364547 ) ) ;
#17575 = CARTESIAN_POINT ( 'NONE',  ( -0.7545931758530176614, -0.6692913385826773087, -0.1292274648535924053 ) ) ;
#17576 = CARTESIAN_POINT ( 'NONE',  ( 1.148293963254593875, -0.6692913385826771977, 0.1292274648535927661 ) ) ;
#17577 = CARTESIAN_POINT ( 'NONE',  ( -0.4724409448818899238, 0.1265901696524986686, -1.292650918635170454 ) ) ;
#17578 = CARTESIAN_POINT ( 'NONE',  ( 0.2925321140481932369, -0.2925321140481931814, -2.460629921259842146 ) ) ;
#17579 = CARTESIAN_POINT ( 'NONE',  ( -0.2493438320209966919, -0.004921259842519870586, -0.3153832671262229437 ) ) ;
#17580 =( BOUNDED_SURFACE ( )  B_SPLINE_SURFACE ( 3, 2, ( 
 ( #22890, #3544, #54877, #60777, #47309, #16183, #34705, #41830, #72999, #17017, #61189, #54456, #3128, #42657, #48558, #22484, #16597, #15351, #41013, #60367, #2715, #54036, #28793, #48147, #35527, #80584, #42242, #67937, #61615, #3957, #69582, #30445, #19055, #56110, #75082, #43471, #17429, #70399, #37995, #43884, #83037, #76723, #43060, #11929, #68757, #37584, #75497, #31682, #6430, #81816, #30855, #32100, #69167, #56520, #44703, #31264, #63257, #24126, #57342, #12755, #44293, #49387, #12339, #38412, #11100, #64094, #76319, #36757, #25361, #51024, #57760, #23716, #5598, #62433, #82222, #4770, #24542, #49795, #17836, #24941, #56931, #11518, #37174, #62854, #50206, #75904, #5190, #18243, #82627, #50613, #18649, #69984, #63671, #6012, #45550, #7268, #64508, #78408, #78825, #72083, #46808, #72499, #40508, #13592, #52699, #46389, #40093, #66190, #33367, #65780, #6846, #70832, #33778, #26200, #20738, #27038, #58605, #39247, #39672, #14848, #59441, #34193, #45124, #19474, #71664, #64930, #14441, #8526, #122, #25777, #1794, #38830, #32940, #974, #21153, #51438, #8112, #19902, #13180, #71247, #26628, #77141, #52282, #32516, #51861, #58178, #27455, #547, #65363, #77568, #77987, #20316, #45968, #53115, #59030, #14015, #7700, #1385, #59858, #53537, #67431, #15263, #16092, #15681, #68267, #16511, #29527, #73757, #2209, #2630, #48055, #40923, #34615, #35025, #48881, #66604, #60280, #28286, #53948, #8938, #79661, #21977, #74164, #41737, #61101, #48463, #47639, #73334, #42154, #22397, #22806, #3452, #41342, #67021, #9354, #67849, #9765, #35436, #60689, #35854, #3039, #28704, #54366, #29117, #80078, #54787, #80490, #10188, #61522, #3868, #55190, #80897, #23211, #74581, #16926, #42564, #10603, #27877, #79245, #21560, #47222, #72911, #11003, #51652, #19265, #38627, #25995, #42969, #36662, #19688, #83250, #339, #64305, #68664, #62336, #81723, #77357, #76937, #25573, #4674, #13387, #17743, #6222, #38209, #6639, #43372, #32311, #74994, #30346, #57974, #56013, #45346, #71042, #69072, #11421, #39039, #58399, #24032, #49701, #64724, #63884, #75397, #7063, #31898, #57559, #17339, #32732, #759, #26420, #52073, #77780, #20114, #51238, #45761, #71460, #36260, #61929, #70615, #4272, #44918, #23622, #29933, #12970, #55597, #81308, #49292, #52909, #53333, #2836, #47431, #47846, #58827, #33158, #2005, #27250, #66396, #22189, #79872, #54157, #73124, #52493, #46604, #14646, #9155, #65152, #40711, #33572, #1184, #59234, #72300, #13807, #1595, #39466, #39890, #46184, #8734, #7489, #79042, #7911, #26835, #78202, #28499, #34404, #47014, #60486, #20532, #66822, #71881, #14230, #21361, #65577, #72708, #78623, #20947, #53741, #34828, #27667, #40303, #65983, #15055, #8321, #33987, #59649, #60072, #2427, #28083, #15474, #79449, #21769, #41131, #68871, #49087, #23010, #42770, #43174, #55809, #9563, #35234, #36879, #30567, #11219, #80289, #35647, #81516, #23837, #49505, #22603, #36059, #48263, #62557, #73960, #41544, #9978, #67233, #4892, #4478, #10402, #75198, #56232, #60897, #61731, #3249, #4068, #41949, #17542, #81930, #16306, #80697, #24241, #61308, #48678, #73552, #81104, #29735, #67644, #15896, #28912, #10804, #54576, #62139, #3665, #29328, #54989, #68466, #74373, #16717, #42357, #68055, #55398, #23421, #74787, #17138, #36464, #30148, #19581, #77252, #51136, #38107, #32626, #17950, #43587, #76430, #25888, #70941, #69288, #25470, #58289, #11635, #62970, #76018, #76831, #654, #19163, #83150, #70509, #51548, #30967, #82737, #44813, #70094, #49914, #24653, #5308, #37295, #75612, #82335, #45241, #56634, #12041, #32211, #69697, #50321, #12867, #13286, #6541, #38524, #31794, #38938, #64207, #12448, #64619, #6956, #57870, #18360, #236, #44004, #6122, #57457, #37697, #50731, #63372, #5707, #31378, #57043, #25056 ),
 ( #18758, #44402, #63783, #40610, #46494, #2320, #79346, #20007, #14547, #45658, #40199, #78095, #34303, #9048, #33045, #33471, #34723, #46079, #59133, #21667, #33882, #72190, #58714, #59964, #15368, #46910, #51969, #14952, #47326, #71354, #41029, #78933, #13700, #27980, #53639, #73017, #66715, #65882, #39356, #1491, #26311, #27144, #60383, #77677, #27564, #8218, #65040, #7377, #1079, #52808, #26732, #52386, #20426, #1903, #71772, #14125, #39778, #65472, #53223, #7806, #21256, #59548, #72605, #78518, #20842, #66293, #8632, #22906, #2732, #60793, #41442, #22083, #36774, #35129, #62041, #15790, #48164, #68372, #22501, #9456, #81006, #81417, #42673, #35962, #67952, #75098, #74688, #48574, #55708, #30046, #10710, #3146, #36367, #61631, #42257, #10295, #28809, #43076, #54893, #47742, #80598, #28393, #4378, #16615, #9874, #73859, #23733, #3973, #54473, #49404, #80186, #54052, #16200, #79766, #17446, #17034, #74271, #68773, #11117, #73440, #29637, #67126, #55297, #41847, #67537, #35543, #61204, #3561, #29226, #23320, #48990, #51037, #24955, #37598, #43486, #31696, #70413, #69998, #4786, #12353, #76738, #81832, #12769, #18663, #24142, #57355, #83051, #25374, #38426, #31280, #49813, #75919, #62450, #11944, #44716, #19068, #44308, #56945, #30463, #75513, #17852, #63272, #64108, #6443, #69182, #38009, #56126, #62870, #82238, #43900, #11533, #37190, #5206, #30870, #56536, #24557, #5612, #63687, #50223, #18258, #69597, #6025, #82642, #50628, #76333, #3419, #30311, #67398, #16474, #36626, #74129, #61068, #49257, #49669, #10967, #4234, #36224, #43335, #42932, #16891, #24001, #81690, #62303, #54752, #4640, #29898, #10566, #61893, #29082, #11386, #23175, #73720, #48845, #5063, #55979, #68232, #61484, #42121, #75359, #55562, #3833, #23586, #17707, #69036, #16059, #41706, #37043, #62725, #54332, #80458, #67816, #80042, #22361, #48020, #22767, #42530, #48430, #9733, #35404, #74959, #10153, #68627, #35819, #29493, #55152, #17305, #80863, #74546, #81270, #64372, #19760, #44572, #18114, #63542, #30732, #31549, #407, #58042, #31966, #18923, #13452, #82093, #24407, #57206, #6709, #51723, #50077, #6291, #39108, #75773, #43747, #56798, #57627, #64790, #58492, #63954, #51304, #32378, #11803, #5875, #25641, #50893, #56395, #5470, #69453, #37458, #63131, #31132, #26064, #82498, #76185, #13041, #50481, #24814, #77006, #77425, #70688, #19339, #12619, #45413, #44989, #76593, #71109, #18522, #38694, #44165, #69858, #12209, #70264, #38277, #37867, #82907, #25228, #45374, #76966, #12169, #37826, #64332, #367, #10625, #61953, #70643, #63503, #36281, #57588, #23644, #69820, #42589, #83278, #58002, #51264, #26022, #51681, #19715, #75016, #31926, #25601, #19295, #71070, #12578, #44946, #68289, #48903, #12999, #4293, #38655, #6249, #5835, #17362, #18884, #77384, #6669, #13413, #23234, #80919, #50856, #44128, #32340, #61545, #3889, #29549, #55211, #16947, #74604, #29956, #55621, #81330, #31508, #49315, #57168, #82867, #25190, #38235, #76556, #44533, #70223, #63913, #65181, #8349, #66011, #14260, #78229, #78651, #28113, #72736, #73151, #788, #58427, #27278, #52521, #34016, #47457, #21794, #79478, #15082, #77810, #71909, #39918, #34435, #7090, #59677, #58855, #26448, #1212, #65607, #39069, #26862, #64751, #7518, #71488, #2032, #32760, #20973, #33186, #52101, #20140, #53767, #27698, #72328, #2455, #45789, #8760, #13836, #39494, #46632, #20563, #14675, #46214, #7938, #79072, #60101, #52938, #33599, #59264, #40332, #1621, #53362, #21388, #47043, #40741, #66424, #41568, #67257, #47871, #22214, #73575, #29761, #80721, #16743, #4092, #15921, #9590, #81131, #61334, #61755, #42383, #35259, #60924, #3274, #55423, #55012, #3688, #28935, #74817, #80313, #67669, #16331, #68082, #22628, #10426, #54183, #54604, #9180, #36084, #81543 ),
 ( #79896, #23447, #10829, #49111, #17162, #48289, #73985, #41975, #42795, #23035, #29353, #10005, #68490, #35670, #48701, #74400, #36489, #62165, #4505, #30172, #55835, #34852, #23862, #49529, #15500, #41158, #66847, #60514, #2862, #28525, #75637, #83178, #76045, #49939, #70124, #37323, #82361, #56257, #12475, #70539, #63811, #38554, #64234, #32240, #5334, #44430, #38138, #31824, #57899, #25086, #57485, #81953, #62581, #25499, #17976, #6150, #18786, #50347, #30992, #31406, #6569, #51164, #25918, #36905, #11247, #63399, #56660, #76860, #265, #75222, #17567, #19192, #30591, #24680, #18389, #12895, #43200, #44842, #11665, #4923, #62995, #44031, #68895, #69723, #24266, #43613, #69314, #12067, #37725, #57070, #5734, #82764, #50759, #76460, #46528, #1522, #14983, #6987, #21289, #51578, #45272, #59164, #32655, #7835, #7411, #59999, #8249, #46943, #65503, #77280, #77706, #39813, #58322, #26340, #26761, #40642, #684, #52001, #20036, #45687, #71384, #13733, #39388, #65912, #33502, #52839, #40230, #65073, #33081, #33914, #14157, #58748, #72635, #27176, #1110, #20876, #66324, #59578, #70968, #13313, #8664, #34335, #2355, #52416, #78125, #1936, #27598, #53258, #20459, #78551, #46111, #19610, #71806, #38966, #72228, #64649, #14578, #78969, #48194, #4003, #81038, #21697, #16230, #47360, #41877, #79800, #35992, #10740, #34755, #35163, #36397, #47776, #60824, #23350, #35575, #73890, #60415, #61662, #17067, #48606, #53671, #16647, #49022, #73049, #42704, #80628, #15399, #29668, #55329, #74718, #68401, #67571, #41060, #3175, #28011, #28840, #62072, #79378, #29257, #9903, #66749, #9084, #2766, #54502, #28425, #54085, #22116, #3592, #73477, #15827, #41475, #67160, #54921, #9489, #22939, #61237, #74301, #80216, #22532, #42288, #67985, #10330, #4410, #62484, #43107, #23766, #38454, #36807, #63715, #17476, #49843, #70029, #24174, #11149, #82672, #83082, #44338, #37629, #69629, #76767, #76363, #50253, #57391, #31727, #12382, #4818, #38040, #63305, #43935, #11974, #30496, #6056, #37224, #17882, #68803, #30078, #25404, #18290, #11565, #18696, #5643, #31310, #51067, #56159, #81862, #19097, #75951, #50663, #56974, #75542, #43517, #69217, #44746, #24988, #70441, #62901, #12799, #5236, #56567, #30900, #55741, #82268, #81449, #24586, #49437, #75131, #65402, #46843, #78448, #13632, #39284, #65817, #1834, #13222, #64549, #72119, #64971, #38870, #59067, #26241, #71284, #45167, #1422, #59480, #52738, #27494, #53151, #21189, #77608, #33405, #27078, #20774, #72537, #14056, #46428, #70873, #51479, #14478, #6886, #40131, #7739, #7307, #19941, #20355, #78863, #8150, #14885, #25819, #166, #52320, #45591, #33815, #64140, #6473, #32143, #57799, #19514, #32977, #58644, #77182, #32556, #58219, #585, #51901, #1012, #26665, #78026, #46006, #71702, #39711, #72946, #9798, #74616, #22430, #34651, #2246, #27912, #29561, #35470, #73789, #3901, #79280, #10221, #40545, #34232, #48089, #21595, #80112, #79696, #48915, #80525, #35888, #54400, #66225, #66641, #28739, #47257, #15298, #15717, #55223, #40959, #8978, #60315, #2664, #28323, #53984, #22013, #22837, #59894, #53571, #80930, #23245, #61558, #47673, #73368, #48496, #74197, #16543, #41373, #3073, #67054, #8563, #9387, #35057, #60723, #16125, #41771, #54821, #67464, #42188, #61134, #3486, #29152, #67883, #5133, #68698, #24885, #82978, #23657, #24069, #25297, #36697, #49738, #69924, #24481, #37115, #49327, #50554, #5950, #37525, #42599, #5540, #12280, #61966, #31619, #69523, #4305, #76257, #18592, #44235, #57281, #30798, #29968, #75438, #16960, #17777, #37936, #63613, #18186, #56463, #50963, #68301, #10637, #43410, #36292, #55633, #81342, #75844, #75029, #17374, #43004, #11039, #43819, #62372, #11873, #50147, #63200, #4710, #30384, #69109, #31205, #62799, #56050, #81759, #11457 ),
 ( #56872, #82165, #82566, #19411, #52640, #58114, #45486, #77502, #20254, #480, #71600, #32039, #45062, #70338, #77923, #59377, #7638, #26136, #51797, #78344, #14377, #25714, #77078, #1326, #19837, #51374, #13952, #39610, #26566, #40035, #57698, #46328, #76660, #12693, #910, #60, #32875, #32452, #1735, #33308, #72021, #7204, #18993, #70765, #64865, #13115, #38767, #71183, #65721, #64444, #6780, #13525, #39181, #58544, #52220, #45903, #58969, #65299, #26975, #20675, #8053, #33715, #27391, #44642, #38352, #64027, #6367, #79184, #15198, #16032, #9294, #15618, #21500, #29054, #34550, #21913, #53884, #80014, #60216, #47993, #8462, #47158, #46747, #54301, #35788, #67371, #2566, #28225, #54725, #74100, #2147, #53474, #61040, #79598, #27814, #73692, #40857, #47575, #34131, #41678, #48400, #9705, #16446, #42091, #10124, #66541, #22332, #35376, #3390, #61456, #2978, #80430, #59793, #40445, #22740, #72849, #67787, #3804, #73269, #8874, #34964, #53052, #78764, #21088, #14789, #72440, #41275, #66961, #66125, #60627, #28643, #69833, #5445, #68201, #62275, #30284, #24788, #80834, #56369, #49229, #16863, #74932, #4612, #37840, #17277, #12183, #55533, #61866, #82068, #63518, #11359, #23558, #74515, #42500, #18498, #44141, #63107, #29466, #10539, #48816, #17680, #42905, #24381, #55124, #23147, #36196, #31106, #4207, #55950, #81663, #50457, #29871, #50053, #68600, #81242, #10940, #23973, #36597, #49641, #75333, #43310, #69008, #75748, #37017, #62698, #5037, #30706, #18088, #43723, #69427, #11780, #76161, #37433, #82473, #56773, #82883, #13427, #44547, #45387, #44961, #14273, #45804, #58869, #19732, #5848, #31940, #77398, #70237, #63928, #64346, #78244, #12592, #6264, #57601, #83291, #38250, #25614, #51277, #20154, #71084, #7103, #77824, #76980, #19309, #71501, #51695, #52116, #32773, #70658, #13014, #38668, #13849, #39083, #64764, #6683, #65195, #32354, #58015, #380, #58441, #26036, #802, #26465, #39507, #25203, #7532, #71923, #33204, #1227, #26876, #52536, #20576, #46227, #39935, #31524, #57181, #50869, #76569, #18897, #73902, #46647, #61674, #62083, #55342, #30090, #55753, #23778, #80228, #36004, #29679, #23362, #49449, #16660, #49033, #72341, #52950, #17078, #9502, #4015, #10343, #41890, #22544, #22952, #67583, #36408, #10751, #67997, #54933, #75143, #33614, #59277, #9915, #42715, #4424, #1633, #42300, #17488, #27292, #78664, #35175, #81050, #65621, #74729, #68411, #81461, #7952, #14689, #16243, #20985, #3604, #40345, #67173, #60836, #3188, #28852, #54514, #48207, #35587, #61250, #29269, #80640, #48619, #74313, #38466, #83094, #76374, #25001, #32155, #31739, #5655, #12811, #70453, #51079, #43531, #25415, #18707, #82683, #50675, #17894, #19109, #75964, #56579, #81874, #77193, #76777, #56986, #50266, #62915, #64151, #44349, #18302, #12394, #6485, #44757, #62496, #4831, #57811, #178, #25831, #49855, #5248, #51490, #43119, #68816, #75555, #31321, #69230, #11162, #11578, #36821, #30912, #30509, #56171, #57403, #63317, #24186, #37237, #82280, #70040, #24598, #38051, #43946, #69641, #11986, #37640, #63727, #6067, #39299, #52333, #72550, #27090, #39723, #51914, #27508, #8575, #40144, #45179, #8162, #14897, #64562, #34246, #72133, #6899, #53165, #78878, #21201, #59908, #33417, #32570, #78039, #19525, #58232, #53584, #46856, #59079, #26678, #64986, #40557, #78461, #20369, #14491, #66238, #1847, #38883, #599, #2261, #27926, #70884, #26255, #7321, #13233, #77621, #19954, #45604, #65416, #71298, #13646, #32990, #58659, #1025, #46021, #71715, #33827, #7752, #14070, #1434, #52753, #20786, #46442, #65829, #59493, #3918, #61985, #2679, #3091, #4322, #15734, #28755, #48933, #3503, #16143, #28339, #29579, #68317, #16561, #21611, #67901, #74634, #40975, #10654, #48516, #66657, #55242, #80949, #23264 ) ),
 .UNSPECIFIED., .F., .F., .F. ) 
 B_SPLINE_SURFACE_WITH_KNOTS ( ( 4, 4 ),
 ( 3, 2, 2, 2, 2, 2, 2, 2, 2, 2, 2, 2, 2, 2, 2, 2, 2, 2, 2, 2, 2, 2, 2, 2, 2, 2, 2, 2, 2, 2, 2, 2, 2, 2, 2, 2, 2, 2, 2, 2, 2, 2, 2, 2, 2, 2, 2, 2, 2, 2, 2, 2, 2, 2, 2, 2, 2, 2, 2, 2, 2, 2, 2, 2, 2, 2, 2, 2, 2, 2, 2, 2, 2, 2, 2, 2, 2, 2, 2, 2, 2, 2, 2, 2, 2, 2, 2, 2, 2, 2, 2, 2, 2, 2, 2, 2, 2, 2, 2, 2, 2, 2, 2, 2, 2, 2, 2, 2, 2, 2, 2, 2, 2, 2, 2, 2, 2, 2, 2, 2, 2, 2, 2, 2, 2, 2, 2, 2, 2, 2, 2, 2, 2, 2, 2, 2, 2, 2, 2, 2, 2, 2, 2, 2, 2, 2, 2, 2, 2, 2, 2, 2, 2, 2, 2, 2, 2, 2, 2, 2, 2, 2, 2, 2, 2, 2, 2, 2, 2, 2, 2, 2, 2, 2, 2, 2, 2, 2, 2, 2, 2, 2, 2, 2, 2, 2, 2, 2, 2, 2, 2, 2, 2, 2, 2, 2, 2, 2, 2, 2, 2, 2, 2, 2, 2, 2, 2, 2, 2, 2, 2, 2, 2, 2, 2, 2, 2, 2, 2, 2, 2, 2, 2, 2, 2, 2, 2, 2, 2, 2, 2, 2, 2, 2, 2, 2, 2, 3 ),
 ( 0.000000000000000000, 1.000000000000000000 ),
 ( 0.000000000000000000, 0.004166666666666666609, 0.008333333333333333218, 0.01250000000000000069, 0.01666666666666666644, 0.02083333333333333218, 0.02500000000000000139, 0.02916666666666666713, 0.03333333333333333287, 0.03749999999999999861, 0.04166666666666666435, 0.04583333333333333010, 0.05000000000000000278, 0.05416666666666666852, 0.05833333333333333426, 0.06250000000000000000, 0.06666666666666666574, 0.07083333333333333148, 0.07499999999999999722, 0.07916666666666666297, 0.08333333333333332871, 0.08749999999999999445, 0.09166666666666666019, 0.09583333333333333981, 0.1000000000000000056, 0.1041666666666666713, 0.1083333333333333370, 0.1125000000000000028, 0.1166666666666666685, 0.1208333333333333343, 0.1250000000000000000, 0.1291666666666666796, 0.1333333333333333315, 0.1375000000000000111, 0.1416666666666666630, 0.1458333333333333426, 0.1499999999999999944, 0.1541666666666666741, 0.1583333333333333259, 0.1625000000000000056, 0.1666666666666666574, 0.1708333333333333370, 0.1749999999999999889, 0.1791666666666666685, 0.1833333333333333204, 0.1875000000000000000, 0.1916666666666666796, 0.1958333333333333315, 0.2000000000000000111, 0.2041666666666666630, 0.2083333333333333426, 0.2124999999999999944, 0.2166666666666666741, 0.2208333333333333259, 0.2250000000000000056, 0.2291666666666666574, 0.2333333333333333370, 0.2374999999999999889, 0.2416666666666666685, 0.2458333333333333204, 0.2500000000000000000, 0.2541666666666666519, 0.2583333333333333592, 0.2625000000000000111, 0.2666666666666666630, 0.2708333333333333148, 0.2750000000000000222, 0.2791666666666666741, 0.2833333333333333259, 0.2874999999999999778, 0.2916666666666666852, 0.2958333333333333370, 0.2999999999999999889, 0.3041666666666666408, 0.3083333333333333481, 0.3125000000000000000, 0.3166666666666666519, 0.3208333333333333592, 0.3250000000000000111, 0.3291666666666666630, 0.3333333333333333148, 0.3375000000000000222, 0.3416666666666666741, 0.3458333333333333259, 0.3499999999999999778, 0.3541666666666666852, 0.3583333333333333370, 0.3624999999999999889, 0.3666666666666666408, 0.3708333333333333481, 0.3750000000000000000, 0.3791666666666666519, 0.3833333333333333592, 0.3875000000000000111, 0.3916666666666666630, 0.3958333333333333148, 0.4000000000000000222, 0.4041666666666666741, 0.4083333333333333259, 0.4124999999999999778, 0.4166666666666666852, 0.4208333333333333370, 0.4249999999999999889, 0.4291666666666666408, 0.4333333333333333481, 0.4375000000000000000, 0.4416666666666666519, 0.4458333333333333592, 0.4500000000000000111, 0.4541666666666666630, 0.4583333333333333148, 0.4625000000000000222, 0.4666666666666666741, 0.4708333333333333259, 0.4749999999999999778, 0.4791666666666666852, 0.4833333333333333370, 0.4874999999999999889, 0.4916666666666666408, 0.4958333333333333481, 0.5000000000000000000, 0.5041666666666666519, 0.5083333333333333037, 0.5124999999999999556, 0.5166666666666667185, 0.5208333333333333703, 0.5250000000000000222, 0.5291666666666666741, 0.5333333333333333259, 0.5374999999999999778, 0.5416666666666666297, 0.5458333333333332815, 0.5500000000000000444, 0.5541666666666666963, 0.5583333333333333481, 0.5625000000000000000, 0.5666666666666666519, 0.5708333333333333037, 0.5749999999999999556, 0.5791666666666667185, 0.5833333333333333703, 0.5875000000000000222, 0.5916666666666666741, 0.5958333333333333259, 0.5999999999999999778, 0.6041666666666666297, 0.6083333333333332815, 0.6125000000000000444, 0.6166666666666666963, 0.6208333333333333481, 0.6250000000000000000, 0.6291666666666666519, 0.6333333333333333037, 0.6374999999999999556, 0.6416666666666667185, 0.6458333333333333703, 0.6500000000000000222, 0.6541666666666666741, 0.6583333333333333259, 0.6624999999999999778, 0.6666666666666666297, 0.6708333333333332815, 0.6750000000000000444, 0.6791666666666666963, 0.6833333333333333481, 0.6875000000000000000, 0.6916666666666666519, 0.6958333333333333037, 0.6999999999999999556, 0.7041666666666667185, 0.7083333333333333703, 0.7125000000000000222, 0.7166666666666666741, 0.7208333333333333259, 0.7249999999999999778, 0.7291666666666666297, 0.7333333333333332815, 0.7375000000000000444, 0.7416666666666666963, 0.7458333333333333481, 0.7500000000000000000, 0.7541666666666666519, 0.7583333333333333037, 0.7624999999999999556, 0.7666666666666667185, 0.7708333333333333703, 0.7750000000000000222, 0.7791666666666666741, 0.7833333333333333259, 0.7874999999999999778, 0.7916666666666666297, 0.7958333333333332815, 0.8000000000000000444, 0.8041666666666666963, 0.8083333333333333481, 0.8125000000000000000, 0.8166666666666666519, 0.8208333333333333037, 0.8249999999999999556, 0.8291666666666667185, 0.8333333333333333703, 0.8375000000000000222, 0.8416666666666666741, 0.8458333333333333259, 0.8499999999999999778, 0.8541666666666666297, 0.8583333333333332815, 0.8625000000000000444, 0.8666666666666666963, 0.8708333333333333481, 0.8750000000000000000, 0.8791666666666666519, 0.8833333333333333037, 0.8874999999999999556, 0.8916666666666667185, 0.8958333333333333703, 0.9000000000000000222, 0.9041666666666666741, 0.9083333333333333259, 0.9124999999999999778, 0.9166666666666666297, 0.9208333333333332815, 0.9250000000000000444, 0.9291666666666666963, 0.9333333333333333481, 0.9375000000000000000, 0.9416666666666666519, 0.9458333333333333037, 0.9499999999999999556, 0.9541666666666667185, 0.9583333333333333703, 0.9625000000000000222, 0.9666666666666666741, 0.9708333333333333259, 0.9749999999999999778, 0.9791666666666666297, 0.9833333333333332815, 0.9875000000000000444 ),
 .UNSPECIFIED. ) 
 GEOMETRIC_REPRESENTATION_ITEM ( )  RATIONAL_B_SPLINE_SURFACE ( (
 ( 1.000000000000000000, 0.9659258262890683122, 1.000000000000000000, 0.9659258262890683122, 1.000000000000000000, 0.9659258262890683122, 1.000000000000000000, 0.9659258262890683122, 1.000000000000000000, 0.9659258262890683122, 1.000000000000000000, 0.9659258262890683122, 1.000000000000000000, 0.9659258262890683122, 1.000000000000000000, 0.9659258262890683122, 1.000000000000000000, 0.9659258262890683122, 1.000000000000000000, 0.9659258262890683122, 1.000000000000000000, 0.9659258262890683122, 1.000000000000000000, 0.9659258262890683122, 1.000000000000000000, 0.9659258262890683122, 1.000000000000000000, 0.9659258262890683122, 1.000000000000000000, 0.9659258262890683122, 1.000000000000000000, 0.9659258262890683122, 1.000000000000000000, 0.9659258262890683122, 1.000000000000000000, 0.9659258262890683122, 1.000000000000000000, 0.9659258262890683122, 1.000000000000000000, 0.9659258262890683122, 1.000000000000000000, 0.9659258262890683122, 1.000000000000000000, 0.9659258262890683122, 1.000000000000000000, 0.9659258262890683122, 1.000000000000000000, 0.9659258262890683122, 1.000000000000000000, 0.9659258262890683122, 1.000000000000000000, 0.9659258262890683122, 1.000000000000000000, 0.9659258262890683122, 1.000000000000000000, 0.9659258262890683122, 1.000000000000000000, 0.9659258262890683122, 1.000000000000000000, 0.9659258262890683122, 1.000000000000000000, 0.9659258262890683122, 1.000000000000000000, 0.9659258262890683122, 1.000000000000000000, 0.9659258262890683122, 1.000000000000000000, 0.9659258262890683122, 1.000000000000000000, 0.9659258262890683122, 1.000000000000000000, 0.9659258262890683122, 1.000000000000000000, 0.9659258262890683122, 1.000000000000000000, 0.9659258262890683122, 1.000000000000000000, 0.9659258262890683122, 1.000000000000000000, 0.9659258262890683122, 1.000000000000000000, 0.9659258262890683122, 1.000000000000000000, 0.9659258262890683122, 1.000000000000000000, 0.9659258262890683122, 1.000000000000000000, 0.9659258262890683122, 1.000000000000000000, 0.9659258262890683122, 1.000000000000000000, 0.9659258262890683122, 1.000000000000000000, 0.9659258262890683122, 1.000000000000000000, 0.9659258262890683122, 1.000000000000000000, 0.9659258262890683122, 1.000000000000000000, 0.9659258262890683122, 1.000000000000000000, 0.9659258262890683122, 1.000000000000000000, 0.9659258262890683122, 1.000000000000000000, 0.9659258262890683122, 1.000000000000000000, 0.9659258262890683122, 1.000000000000000000, 0.9659258262890683122, 1.000000000000000000, 0.9659258262890683122, 1.000000000000000000, 0.9659258262890683122, 1.000000000000000000, 0.9659258262890683122, 1.000000000000000000, 0.9659258262890683122, 1.000000000000000000, 0.9659258262890683122, 1.000000000000000000, 0.9659258262890683122, 1.000000000000000000, 0.9659258262890683122, 1.000000000000000000, 0.9659258262890683122, 1.000000000000000000, 0.9659258262890683122, 1.000000000000000000, 0.9659258262890683122, 1.000000000000000000, 0.9659258262890683122, 1.000000000000000000, 0.9659258262890683122, 1.000000000000000000, 0.9659258262890683122, 1.000000000000000000, 0.9659258262890683122, 1.000000000000000000, 0.9659258262890683122, 1.000000000000000000, 0.9659258262890683122, 1.000000000000000000, 0.9659258262890683122, 1.000000000000000000, 0.9659258262890683122, 1.000000000000000000, 0.9659258262890683122, 1.000000000000000000, 0.9659258262890683122, 1.000000000000000000, 0.9659258262890683122, 1.000000000000000000, 0.9659258262890683122, 1.000000000000000000, 0.9659258262890683122, 1.000000000000000000, 0.9659258262890683122, 1.000000000000000000, 0.9659258262890683122, 1.000000000000000000, 0.9659258262890683122, 1.000000000000000000, 0.9659258262890683122, 1.000000000000000000, 0.9659258262890683122, 1.000000000000000000, 0.9659258262890683122, 1.000000000000000000, 0.9659258262890683122, 1.000000000000000000, 0.9659258262890683122, 1.000000000000000000, 0.9659258262890683122, 1.000000000000000000, 0.9659258262890683122, 1.000000000000000000, 0.9659258262890683122, 1.000000000000000000, 0.9659258262890683122, 1.000000000000000000, 0.9659258262890683122, 1.000000000000000000, 0.9659258262890683122, 1.000000000000000000, 0.9659258262890683122, 1.000000000000000000, 0.9659258262890683122, 1.000000000000000000, 0.9659258262890683122, 1.000000000000000000, 0.9659258262890683122, 1.000000000000000000, 0.9659258262890683122, 1.000000000000000000, 0.9659258262890683122, 1.000000000000000000, 0.9659258262890683122, 1.000000000000000000, 0.9659258262890683122, 1.000000000000000000, 0.9659258262890683122, 1.000000000000000000, 0.9659258262890683122, 1.000000000000000000, 0.9659258262890683122, 1.000000000000000000, 0.9659258262890683122, 1.000000000000000000, 0.9659258262890683122, 1.000000000000000000, 0.9659258262890683122, 1.000000000000000000, 0.9659258262890683122, 1.000000000000000000, 0.9659258262890683122, 1.000000000000000000, 0.9659258262890683122, 1.000000000000000000, 0.9659258262890683122, 1.000000000000000000, 0.9659258262890683122, 1.000000000000000000, 0.9659258262890683122, 1.000000000000000000, 0.9659258262890683122, 1.000000000000000000, 0.9659258262890683122, 1.000000000000000000, 0.9659258262890683122, 1.000000000000000000, 0.9659258262890683122, 1.000000000000000000, 0.9659258262890683122, 1.000000000000000000, 0.9659258262890683122, 1.000000000000000000, 0.9659258262890683122, 1.000000000000000000, 0.9659258262890683122, 1.000000000000000000, 0.9659258262890683122, 1.000000000000000000, 0.9659258262890683122, 1.000000000000000000, 0.9659258262890683122, 1.000000000000000000, 0.9659258262890683122, 1.000000000000000000, 0.9659258262890683122, 1.000000000000000000, 0.9659258262890683122, 1.000000000000000000, 0.9659258262890683122, 1.000000000000000000, 0.9659258262890683122, 1.000000000000000000, 0.9659258262890683122, 1.000000000000000000, 0.9659258262890683122, 1.000000000000000000, 0.9659258262890683122, 1.000000000000000000, 0.9659258262890683122, 1.000000000000000000, 0.9659258262890683122, 1.000000000000000000, 0.9659258262890683122, 1.000000000000000000, 0.9659258262890683122, 1.000000000000000000, 0.9659258262890683122, 1.000000000000000000, 0.9659258262890683122, 1.000000000000000000, 0.9659258262890683122, 1.000000000000000000, 0.9659258262890683122, 1.000000000000000000, 0.9659258262890683122, 1.000000000000000000, 0.9659258262890683122, 1.000000000000000000, 0.9659258262890683122, 1.000000000000000000, 0.9659258262890683122, 1.000000000000000000, 0.9659258262890683122, 1.000000000000000000, 0.9659258262890683122, 1.000000000000000000, 0.9659258262890683122, 1.000000000000000000, 0.9659258262890683122, 1.000000000000000000, 0.9659258262890683122, 1.000000000000000000, 0.9659258262890683122, 1.000000000000000000, 0.9659258262890683122, 1.000000000000000000, 0.9659258262890683122, 1.000000000000000000, 0.9659258262890683122, 1.000000000000000000, 0.9659258262890683122, 1.000000000000000000, 0.9659258262890683122, 1.000000000000000000, 0.9659258262890683122, 1.000000000000000000, 0.9659258262890683122, 1.000000000000000000, 0.9659258262890683122, 1.000000000000000000, 0.9659258262890683122, 1.000000000000000000, 0.9659258262890683122, 1.000000000000000000, 0.9659258262890683122, 1.000000000000000000, 0.9659258262890683122, 1.000000000000000000, 0.9659258262890683122, 1.000000000000000000, 0.9659258262890683122, 1.000000000000000000, 0.9659258262890683122, 1.000000000000000000, 0.9659258262890683122, 1.000000000000000000, 0.9659258262890683122, 1.000000000000000000, 0.9659258262890683122, 1.000000000000000000, 0.9659258262890683122, 1.000000000000000000, 0.9659258262890683122, 1.000000000000000000, 0.9659258262890683122, 1.000000000000000000, 0.9659258262890683122, 1.000000000000000000, 0.9659258262890683122, 1.000000000000000000, 0.9659258262890683122, 1.000000000000000000, 0.9659258262890683122, 1.000000000000000000, 0.9659258262890683122, 1.000000000000000000, 0.9659258262890683122, 1.000000000000000000, 0.9659258262890683122, 1.000000000000000000, 0.9659258262890683122, 1.000000000000000000, 0.9659258262890683122, 1.000000000000000000, 0.9659258262890683122, 1.000000000000000000, 0.9659258262890683122, 1.000000000000000000, 0.9659258262890683122, 1.000000000000000000, 0.9659258262890683122, 1.000000000000000000, 0.9659258262890683122, 1.000000000000000000, 0.9659258262890683122, 1.000000000000000000, 0.9659258262890683122, 1.000000000000000000, 0.9659258262890683122, 1.000000000000000000, 0.9659258262890683122, 1.000000000000000000, 0.9659258262890683122, 1.000000000000000000, 0.9659258262890683122, 1.000000000000000000, 0.9659258262890683122, 1.000000000000000000, 0.9659258262890683122, 1.000000000000000000, 0.9659258262890683122, 1.000000000000000000, 0.9659258262890683122, 1.000000000000000000, 0.9659258262890683122, 1.000000000000000000, 0.9659258262890683122, 1.000000000000000000, 0.9659258262890683122, 1.000000000000000000, 0.9659258262890683122, 1.000000000000000000, 0.9659258262890683122, 1.000000000000000000, 0.9659258262890683122, 1.000000000000000000, 0.9659258262890683122, 1.000000000000000000, 0.9659258262890683122, 1.000000000000000000, 0.9659258262890683122, 1.000000000000000000, 0.9659258262890683122, 1.000000000000000000, 0.9659258262890683122, 1.000000000000000000, 0.9659258262890683122, 1.000000000000000000, 0.9659258262890683122, 1.000000000000000000, 0.9659258262890683122, 1.000000000000000000, 0.9659258262890683122, 1.000000000000000000, 0.9659258262890683122, 1.000000000000000000, 0.9659258262890683122, 1.000000000000000000, 0.9659258262890683122, 1.000000000000000000, 0.9659258262890683122, 1.000000000000000000, 0.9659258262890683122, 1.000000000000000000, 0.9659258262890683122, 1.000000000000000000, 0.9659258262890683122, 1.000000000000000000, 0.9659258262890683122, 1.000000000000000000, 0.9659258262890683122, 1.000000000000000000, 0.9659258262890683122, 1.000000000000000000, 0.9659258262890683122, 1.000000000000000000, 0.9659258262890683122, 1.000000000000000000, 0.9659258262890683122, 1.000000000000000000, 0.9659258262890683122, 1.000000000000000000, 0.9659258262890683122, 1.000000000000000000, 0.9659258262890683122, 1.000000000000000000, 0.9659258262890683122, 1.000000000000000000, 0.9659258262890683122, 1.000000000000000000, 0.9659258262890683122, 1.000000000000000000, 0.9659258262890683122, 1.000000000000000000, 0.9659258262890683122, 1.000000000000000000, 0.9659258262890683122, 1.000000000000000000, 0.9659258262890683122, 1.000000000000000000, 0.9659258262890683122, 1.000000000000000000, 0.9659258262890683122, 1.000000000000000000, 0.9659258262890683122, 1.000000000000000000, 0.9659258262890683122, 1.000000000000000000, 0.9659258262890683122, 1.000000000000000000),
 ( 0.8047378541243613848, 0.7773170766911654539, 0.8047378541243613848, 0.7773170766911654539, 0.8047378541243613848, 0.7773170766911654539, 0.8047378541243613848, 0.7773170766911654539, 0.8047378541243613848, 0.7773170766911654539, 0.8047378541243613848, 0.7773170766911654539, 0.8047378541243613848, 0.7773170766911654539, 0.8047378541243613848, 0.7773170766911654539, 0.8047378541243613848, 0.7773170766911654539, 0.8047378541243613848, 0.7773170766911654539, 0.8047378541243613848, 0.7773170766911654539, 0.8047378541243613848, 0.7773170766911654539, 0.8047378541243613848, 0.7773170766911654539, 0.8047378541243613848, 0.7773170766911654539, 0.8047378541243613848, 0.7773170766911654539, 0.8047378541243613848, 0.7773170766911654539, 0.8047378541243613848, 0.7773170766911654539, 0.8047378541243613848, 0.7773170766911654539, 0.8047378541243613848, 0.7773170766911654539, 0.8047378541243613848, 0.7773170766911654539, 0.8047378541243613848, 0.7773170766911654539, 0.8047378541243613848, 0.7773170766911654539, 0.8047378541243613848, 0.7773170766911654539, 0.8047378541243613848, 0.7773170766911654539, 0.8047378541243613848, 0.7773170766911654539, 0.8047378541243613848, 0.7773170766911654539, 0.8047378541243613848, 0.7773170766911654539, 0.8047378541243613848, 0.7773170766911654539, 0.8047378541243613848, 0.7773170766911654539, 0.8047378541243613848, 0.7773170766911654539, 0.8047378541243613848, 0.7773170766911654539, 0.8047378541243613848, 0.7773170766911654539, 0.8047378541243613848, 0.7773170766911654539, 0.8047378541243613848, 0.7773170766911654539, 0.8047378541243613848, 0.7773170766911654539, 0.8047378541243613848, 0.7773170766911654539, 0.8047378541243613848, 0.7773170766911654539, 0.8047378541243613848, 0.7773170766911654539, 0.8047378541243613848, 0.7773170766911654539, 0.8047378541243613848, 0.7773170766911654539, 0.8047378541243613848, 0.7773170766911654539, 0.8047378541243613848, 0.7773170766911654539, 0.8047378541243613848, 0.7773170766911654539, 0.8047378541243613848, 0.7773170766911654539, 0.8047378541243613848, 0.7773170766911654539, 0.8047378541243613848, 0.7773170766911654539, 0.8047378541243613848, 0.7773170766911654539, 0.8047378541243613848, 0.7773170766911654539, 0.8047378541243613848, 0.7773170766911654539, 0.8047378541243613848, 0.7773170766911654539, 0.8047378541243613848, 0.7773170766911654539, 0.8047378541243613848, 0.7773170766911654539, 0.8047378541243613848, 0.7773170766911654539, 0.8047378541243613848, 0.7773170766911654539, 0.8047378541243613848, 0.7773170766911654539, 0.8047378541243613848, 0.7773170766911654539, 0.8047378541243613848, 0.7773170766911654539, 0.8047378541243613848, 0.7773170766911654539, 0.8047378541243613848, 0.7773170766911654539, 0.8047378541243613848, 0.7773170766911654539, 0.8047378541243613848, 0.7773170766911654539, 0.8047378541243613848, 0.7773170766911654539, 0.8047378541243613848, 0.7773170766911654539, 0.8047378541243613848, 0.7773170766911654539, 0.8047378541243613848, 0.7773170766911654539, 0.8047378541243613848, 0.7773170766911654539, 0.8047378541243613848, 0.7773170766911654539, 0.8047378541243613848, 0.7773170766911654539, 0.8047378541243613848, 0.7773170766911654539, 0.8047378541243613848, 0.7773170766911654539, 0.8047378541243613848, 0.7773170766911654539, 0.8047378541243613848, 0.7773170766911654539, 0.8047378541243613848, 0.7773170766911654539, 0.8047378541243613848, 0.7773170766911654539, 0.8047378541243613848, 0.7773170766911654539, 0.8047378541243613848, 0.7773170766911654539, 0.8047378541243613848, 0.7773170766911654539, 0.8047378541243613848, 0.7773170766911654539, 0.8047378541243613848, 0.7773170766911654539, 0.8047378541243613848, 0.7773170766911654539, 0.8047378541243613848, 0.7773170766911654539, 0.8047378541243613848, 0.7773170766911654539, 0.8047378541243613848, 0.7773170766911654539, 0.8047378541243613848, 0.7773170766911654539, 0.8047378541243613848, 0.7773170766911654539, 0.8047378541243613848, 0.7773170766911654539, 0.8047378541243613848, 0.7773170766911654539, 0.8047378541243613848, 0.7773170766911654539, 0.8047378541243613848, 0.7773170766911654539, 0.8047378541243613848, 0.7773170766911654539, 0.8047378541243613848, 0.7773170766911654539, 0.8047378541243613848, 0.7773170766911654539, 0.8047378541243613848, 0.7773170766911654539, 0.8047378541243613848, 0.7773170766911654539, 0.8047378541243613848, 0.7773170766911654539, 0.8047378541243613848, 0.7773170766911654539, 0.8047378541243613848, 0.7773170766911654539, 0.8047378541243613848, 0.7773170766911654539, 0.8047378541243613848, 0.7773170766911654539, 0.8047378541243613848, 0.7773170766911654539, 0.8047378541243613848, 0.7773170766911654539, 0.8047378541243613848, 0.7773170766911654539, 0.8047378541243613848, 0.7773170766911654539, 0.8047378541243613848, 0.7773170766911654539, 0.8047378541243613848, 0.7773170766911654539, 0.8047378541243613848, 0.7773170766911654539, 0.8047378541243613848, 0.7773170766911654539, 0.8047378541243613848, 0.7773170766911654539, 0.8047378541243613848, 0.7773170766911654539, 0.8047378541243613848, 0.7773170766911654539, 0.8047378541243613848, 0.7773170766911654539, 0.8047378541243613848, 0.7773170766911654539, 0.8047378541243613848, 0.7773170766911654539, 0.8047378541243613848, 0.7773170766911654539, 0.8047378541243613848, 0.7773170766911654539, 0.8047378541243613848, 0.7773170766911654539, 0.8047378541243613848, 0.7773170766911654539, 0.8047378541243613848, 0.7773170766911654539, 0.8047378541243613848, 0.7773170766911654539, 0.8047378541243613848, 0.7773170766911654539, 0.8047378541243613848, 0.7773170766911654539, 0.8047378541243613848, 0.7773170766911654539, 0.8047378541243613848, 0.7773170766911654539, 0.8047378541243613848, 0.7773170766911654539, 0.8047378541243613848, 0.7773170766911654539, 0.8047378541243613848, 0.7773170766911654539, 0.8047378541243613848, 0.7773170766911654539, 0.8047378541243613848, 0.7773170766911654539, 0.8047378541243613848, 0.7773170766911654539, 0.8047378541243613848, 0.7773170766911654539, 0.8047378541243613848, 0.7773170766911654539, 0.8047378541243613848, 0.7773170766911654539, 0.8047378541243613848, 0.7773170766911654539, 0.8047378541243613848, 0.7773170766911654539, 0.8047378541243613848, 0.7773170766911654539, 0.8047378541243613848, 0.7773170766911654539, 0.8047378541243613848, 0.7773170766911654539, 0.8047378541243613848, 0.7773170766911654539, 0.8047378541243613848, 0.7773170766911654539, 0.8047378541243613848, 0.7773170766911654539, 0.8047378541243613848, 0.7773170766911654539, 0.8047378541243613848, 0.7773170766911654539, 0.8047378541243613848, 0.7773170766911654539, 0.8047378541243613848, 0.7773170766911654539, 0.8047378541243613848, 0.7773170766911654539, 0.8047378541243613848, 0.7773170766911654539, 0.8047378541243613848, 0.7773170766911654539, 0.8047378541243613848, 0.7773170766911654539, 0.8047378541243613848, 0.7773170766911654539, 0.8047378541243613848, 0.7773170766911654539, 0.8047378541243613848, 0.7773170766911654539, 0.8047378541243613848, 0.7773170766911654539, 0.8047378541243613848, 0.7773170766911654539, 0.8047378541243613848, 0.7773170766911654539, 0.8047378541243613848, 0.7773170766911654539, 0.8047378541243613848, 0.7773170766911654539, 0.8047378541243613848, 0.7773170766911654539, 0.8047378541243613848, 0.7773170766911654539, 0.8047378541243613848, 0.7773170766911654539, 0.8047378541243613848, 0.7773170766911654539, 0.8047378541243613848, 0.7773170766911654539, 0.8047378541243613848, 0.7773170766911654539, 0.8047378541243613848, 0.7773170766911654539, 0.8047378541243613848, 0.7773170766911654539, 0.8047378541243613848, 0.7773170766911654539, 0.8047378541243613848, 0.7773170766911654539, 0.8047378541243613848, 0.7773170766911654539, 0.8047378541243613848, 0.7773170766911654539, 0.8047378541243613848, 0.7773170766911654539, 0.8047378541243613848, 0.7773170766911654539, 0.8047378541243613848, 0.7773170766911654539, 0.8047378541243613848, 0.7773170766911654539, 0.8047378541243613848, 0.7773170766911654539, 0.8047378541243613848, 0.7773170766911654539, 0.8047378541243613848, 0.7773170766911654539, 0.8047378541243613848, 0.7773170766911654539, 0.8047378541243613848, 0.7773170766911654539, 0.8047378541243613848, 0.7773170766911654539, 0.8047378541243613848, 0.7773170766911654539, 0.8047378541243613848, 0.7773170766911654539, 0.8047378541243613848, 0.7773170766911654539, 0.8047378541243613848, 0.7773170766911654539, 0.8047378541243613848, 0.7773170766911654539, 0.8047378541243613848, 0.7773170766911654539, 0.8047378541243613848, 0.7773170766911654539, 0.8047378541243613848, 0.7773170766911654539, 0.8047378541243613848, 0.7773170766911654539, 0.8047378541243613848, 0.7773170766911654539, 0.8047378541243613848, 0.7773170766911654539, 0.8047378541243613848, 0.7773170766911654539, 0.8047378541243613848, 0.7773170766911654539, 0.8047378541243613848, 0.7773170766911654539, 0.8047378541243613848, 0.7773170766911654539, 0.8047378541243613848, 0.7773170766911654539, 0.8047378541243613848, 0.7773170766911654539, 0.8047378541243613848, 0.7773170766911654539, 0.8047378541243613848, 0.7773170766911654539, 0.8047378541243613848, 0.7773170766911654539, 0.8047378541243613848, 0.7773170766911654539, 0.8047378541243613848, 0.7773170766911654539, 0.8047378541243613848, 0.7773170766911654539, 0.8047378541243613848, 0.7773170766911654539, 0.8047378541243613848, 0.7773170766911654539, 0.8047378541243613848, 0.7773170766911654539, 0.8047378541243613848, 0.7773170766911654539, 0.8047378541243613848, 0.7773170766911654539, 0.8047378541243613848, 0.7773170766911654539, 0.8047378541243613848, 0.7773170766911654539, 0.8047378541243613848, 0.7773170766911654539, 0.8047378541243613848, 0.7773170766911654539, 0.8047378541243613848, 0.7773170766911654539, 0.8047378541243613848, 0.7773170766911654539, 0.8047378541243613848, 0.7773170766911654539, 0.8047378541243613848, 0.7773170766911654539, 0.8047378541243613848, 0.7773170766911654539, 0.8047378541243613848, 0.7773170766911654539, 0.8047378541243613848, 0.7773170766911654539, 0.8047378541243613848, 0.7773170766911654539, 0.8047378541243613848, 0.7773170766911654539, 0.8047378541243613848, 0.7773170766911654539, 0.8047378541243613848, 0.7773170766911654539, 0.8047378541243613848, 0.7773170766911654539, 0.8047378541243613848, 0.7773170766911654539, 0.8047378541243613848, 0.7773170766911654539, 0.8047378541243613848, 0.7773170766911654539, 0.8047378541243613848, 0.7773170766911654539, 0.8047378541243613848, 0.7773170766911654539, 0.8047378541243613848, 0.7773170766911654539, 0.8047378541243613848, 0.7773170766911654539, 0.8047378541243613848, 0.7773170766911654539, 0.8047378541243613848, 0.7773170766911654539, 0.8047378541243613848, 0.7773170766911654539, 0.8047378541243613848, 0.7773170766911654539, 0.8047378541243613848, 0.7773170766911654539, 0.8047378541243613848, 0.7773170766911654539, 0.8047378541243613848, 0.7773170766911654539, 0.8047378541243613848, 0.7773170766911654539, 0.8047378541243613848),
 ( 0.8047378541243613848, 0.7773170766911654539, 0.8047378541243613848, 0.7773170766911654539, 0.8047378541243613848, 0.7773170766911654539, 0.8047378541243613848, 0.7773170766911654539, 0.8047378541243613848, 0.7773170766911654539, 0.8047378541243613848, 0.7773170766911654539, 0.8047378541243613848, 0.7773170766911654539, 0.8047378541243613848, 0.7773170766911654539, 0.8047378541243613848, 0.7773170766911654539, 0.8047378541243613848, 0.7773170766911654539, 0.8047378541243613848, 0.7773170766911654539, 0.8047378541243613848, 0.7773170766911654539, 0.8047378541243613848, 0.7773170766911654539, 0.8047378541243613848, 0.7773170766911654539, 0.8047378541243613848, 0.7773170766911654539, 0.8047378541243613848, 0.7773170766911654539, 0.8047378541243613848, 0.7773170766911654539, 0.8047378541243613848, 0.7773170766911654539, 0.8047378541243613848, 0.7773170766911654539, 0.8047378541243613848, 0.7773170766911654539, 0.8047378541243613848, 0.7773170766911654539, 0.8047378541243613848, 0.7773170766911654539, 0.8047378541243613848, 0.7773170766911654539, 0.8047378541243613848, 0.7773170766911654539, 0.8047378541243613848, 0.7773170766911654539, 0.8047378541243613848, 0.7773170766911654539, 0.8047378541243613848, 0.7773170766911654539, 0.8047378541243613848, 0.7773170766911654539, 0.8047378541243613848, 0.7773170766911654539, 0.8047378541243613848, 0.7773170766911654539, 0.8047378541243613848, 0.7773170766911654539, 0.8047378541243613848, 0.7773170766911654539, 0.8047378541243613848, 0.7773170766911654539, 0.8047378541243613848, 0.7773170766911654539, 0.8047378541243613848, 0.7773170766911654539, 0.8047378541243613848, 0.7773170766911654539, 0.8047378541243613848, 0.7773170766911654539, 0.8047378541243613848, 0.7773170766911654539, 0.8047378541243613848, 0.7773170766911654539, 0.8047378541243613848, 0.7773170766911654539, 0.8047378541243613848, 0.7773170766911654539, 0.8047378541243613848, 0.7773170766911654539, 0.8047378541243613848, 0.7773170766911654539, 0.8047378541243613848, 0.7773170766911654539, 0.8047378541243613848, 0.7773170766911654539, 0.8047378541243613848, 0.7773170766911654539, 0.8047378541243613848, 0.7773170766911654539, 0.8047378541243613848, 0.7773170766911654539, 0.8047378541243613848, 0.7773170766911654539, 0.8047378541243613848, 0.7773170766911654539, 0.8047378541243613848, 0.7773170766911654539, 0.8047378541243613848, 0.7773170766911654539, 0.8047378541243613848, 0.7773170766911654539, 0.8047378541243613848, 0.7773170766911654539, 0.8047378541243613848, 0.7773170766911654539, 0.8047378541243613848, 0.7773170766911654539, 0.8047378541243613848, 0.7773170766911654539, 0.8047378541243613848, 0.7773170766911654539, 0.8047378541243613848, 0.7773170766911654539, 0.8047378541243613848, 0.7773170766911654539, 0.8047378541243613848, 0.7773170766911654539, 0.8047378541243613848, 0.7773170766911654539, 0.8047378541243613848, 0.7773170766911654539, 0.8047378541243613848, 0.7773170766911654539, 0.8047378541243613848, 0.7773170766911654539, 0.8047378541243613848, 0.7773170766911654539, 0.8047378541243613848, 0.7773170766911654539, 0.8047378541243613848, 0.7773170766911654539, 0.8047378541243613848, 0.7773170766911654539, 0.8047378541243613848, 0.7773170766911654539, 0.8047378541243613848, 0.7773170766911654539, 0.8047378541243613848, 0.7773170766911654539, 0.8047378541243613848, 0.7773170766911654539, 0.8047378541243613848, 0.7773170766911654539, 0.8047378541243613848, 0.7773170766911654539, 0.8047378541243613848, 0.7773170766911654539, 0.8047378541243613848, 0.7773170766911654539, 0.8047378541243613848, 0.7773170766911654539, 0.8047378541243613848, 0.7773170766911654539, 0.8047378541243613848, 0.7773170766911654539, 0.8047378541243613848, 0.7773170766911654539, 0.8047378541243613848, 0.7773170766911654539, 0.8047378541243613848, 0.7773170766911654539, 0.8047378541243613848, 0.7773170766911654539, 0.8047378541243613848, 0.7773170766911654539, 0.8047378541243613848, 0.7773170766911654539, 0.8047378541243613848, 0.7773170766911654539, 0.8047378541243613848, 0.7773170766911654539, 0.8047378541243613848, 0.7773170766911654539, 0.8047378541243613848, 0.7773170766911654539, 0.8047378541243613848, 0.7773170766911654539, 0.8047378541243613848, 0.7773170766911654539, 0.8047378541243613848, 0.7773170766911654539, 0.8047378541243613848, 0.7773170766911654539, 0.8047378541243613848, 0.7773170766911654539, 0.8047378541243613848, 0.7773170766911654539, 0.8047378541243613848, 0.7773170766911654539, 0.8047378541243613848, 0.7773170766911654539, 0.8047378541243613848, 0.7773170766911654539, 0.8047378541243613848, 0.7773170766911654539, 0.8047378541243613848, 0.7773170766911654539, 0.8047378541243613848, 0.7773170766911654539, 0.8047378541243613848, 0.7773170766911654539, 0.8047378541243613848, 0.7773170766911654539, 0.8047378541243613848, 0.7773170766911654539, 0.8047378541243613848, 0.7773170766911654539, 0.8047378541243613848, 0.7773170766911654539, 0.8047378541243613848, 0.7773170766911654539, 0.8047378541243613848, 0.7773170766911654539, 0.8047378541243613848, 0.7773170766911654539, 0.8047378541243613848, 0.7773170766911654539, 0.8047378541243613848, 0.7773170766911654539, 0.8047378541243613848, 0.7773170766911654539, 0.8047378541243613848, 0.7773170766911654539, 0.8047378541243613848, 0.7773170766911654539, 0.8047378541243613848, 0.7773170766911654539, 0.8047378541243613848, 0.7773170766911654539, 0.8047378541243613848, 0.7773170766911654539, 0.8047378541243613848, 0.7773170766911654539, 0.8047378541243613848, 0.7773170766911654539, 0.8047378541243613848, 0.7773170766911654539, 0.8047378541243613848, 0.7773170766911654539, 0.8047378541243613848, 0.7773170766911654539, 0.8047378541243613848, 0.7773170766911654539, 0.8047378541243613848, 0.7773170766911654539, 0.8047378541243613848, 0.7773170766911654539, 0.8047378541243613848, 0.7773170766911654539, 0.8047378541243613848, 0.7773170766911654539, 0.8047378541243613848, 0.7773170766911654539, 0.8047378541243613848, 0.7773170766911654539, 0.8047378541243613848, 0.7773170766911654539, 0.8047378541243613848, 0.7773170766911654539, 0.8047378541243613848, 0.7773170766911654539, 0.8047378541243613848, 0.7773170766911654539, 0.8047378541243613848, 0.7773170766911654539, 0.8047378541243613848, 0.7773170766911654539, 0.8047378541243613848, 0.7773170766911654539, 0.8047378541243613848, 0.7773170766911654539, 0.8047378541243613848, 0.7773170766911654539, 0.8047378541243613848, 0.7773170766911654539, 0.8047378541243613848, 0.7773170766911654539, 0.8047378541243613848, 0.7773170766911654539, 0.8047378541243613848, 0.7773170766911654539, 0.8047378541243613848, 0.7773170766911654539, 0.8047378541243613848, 0.7773170766911654539, 0.8047378541243613848, 0.7773170766911654539, 0.8047378541243613848, 0.7773170766911654539, 0.8047378541243613848, 0.7773170766911654539, 0.8047378541243613848, 0.7773170766911654539, 0.8047378541243613848, 0.7773170766911654539, 0.8047378541243613848, 0.7773170766911654539, 0.8047378541243613848, 0.7773170766911654539, 0.8047378541243613848, 0.7773170766911654539, 0.8047378541243613848, 0.7773170766911654539, 0.8047378541243613848, 0.7773170766911654539, 0.8047378541243613848, 0.7773170766911654539, 0.8047378541243613848, 0.7773170766911654539, 0.8047378541243613848, 0.7773170766911654539, 0.8047378541243613848, 0.7773170766911654539, 0.8047378541243613848, 0.7773170766911654539, 0.8047378541243613848, 0.7773170766911654539, 0.8047378541243613848, 0.7773170766911654539, 0.8047378541243613848, 0.7773170766911654539, 0.8047378541243613848, 0.7773170766911654539, 0.8047378541243613848, 0.7773170766911654539, 0.8047378541243613848, 0.7773170766911654539, 0.8047378541243613848, 0.7773170766911654539, 0.8047378541243613848, 0.7773170766911654539, 0.8047378541243613848, 0.7773170766911654539, 0.8047378541243613848, 0.7773170766911654539, 0.8047378541243613848, 0.7773170766911654539, 0.8047378541243613848, 0.7773170766911654539, 0.8047378541243613848, 0.7773170766911654539, 0.8047378541243613848, 0.7773170766911654539, 0.8047378541243613848, 0.7773170766911654539, 0.8047378541243613848, 0.7773170766911654539, 0.8047378541243613848, 0.7773170766911654539, 0.8047378541243613848, 0.7773170766911654539, 0.8047378541243613848, 0.7773170766911654539, 0.8047378541243613848, 0.7773170766911654539, 0.8047378541243613848, 0.7773170766911654539, 0.8047378541243613848, 0.7773170766911654539, 0.8047378541243613848, 0.7773170766911654539, 0.8047378541243613848, 0.7773170766911654539, 0.8047378541243613848, 0.7773170766911654539, 0.8047378541243613848, 0.7773170766911654539, 0.8047378541243613848, 0.7773170766911654539, 0.8047378541243613848, 0.7773170766911654539, 0.8047378541243613848, 0.7773170766911654539, 0.8047378541243613848, 0.7773170766911654539, 0.8047378541243613848, 0.7773170766911654539, 0.8047378541243613848, 0.7773170766911654539, 0.8047378541243613848, 0.7773170766911654539, 0.8047378541243613848, 0.7773170766911654539, 0.8047378541243613848, 0.7773170766911654539, 0.8047378541243613848, 0.7773170766911654539, 0.8047378541243613848, 0.7773170766911654539, 0.8047378541243613848, 0.7773170766911654539, 0.8047378541243613848, 0.7773170766911654539, 0.8047378541243613848, 0.7773170766911654539, 0.8047378541243613848, 0.7773170766911654539, 0.8047378541243613848, 0.7773170766911654539, 0.8047378541243613848, 0.7773170766911654539, 0.8047378541243613848, 0.7773170766911654539, 0.8047378541243613848, 0.7773170766911654539, 0.8047378541243613848, 0.7773170766911654539, 0.8047378541243613848, 0.7773170766911654539, 0.8047378541243613848, 0.7773170766911654539, 0.8047378541243613848, 0.7773170766911654539, 0.8047378541243613848, 0.7773170766911654539, 0.8047378541243613848, 0.7773170766911654539, 0.8047378541243613848, 0.7773170766911654539, 0.8047378541243613848, 0.7773170766911654539, 0.8047378541243613848, 0.7773170766911654539, 0.8047378541243613848, 0.7773170766911654539, 0.8047378541243613848, 0.7773170766911654539, 0.8047378541243613848, 0.7773170766911654539, 0.8047378541243613848, 0.7773170766911654539, 0.8047378541243613848, 0.7773170766911654539, 0.8047378541243613848, 0.7773170766911654539, 0.8047378541243613848, 0.7773170766911654539, 0.8047378541243613848, 0.7773170766911654539, 0.8047378541243613848, 0.7773170766911654539, 0.8047378541243613848, 0.7773170766911654539, 0.8047378541243613848, 0.7773170766911654539, 0.8047378541243613848, 0.7773170766911654539, 0.8047378541243613848, 0.7773170766911654539, 0.8047378541243613848, 0.7773170766911654539, 0.8047378541243613848, 0.7773170766911654539, 0.8047378541243613848, 0.7773170766911654539, 0.8047378541243613848, 0.7773170766911654539, 0.8047378541243613848, 0.7773170766911654539, 0.8047378541243613848, 0.7773170766911654539, 0.8047378541243613848, 0.7773170766911654539, 0.8047378541243613848, 0.7773170766911654539, 0.8047378541243613848, 0.7773170766911654539, 0.8047378541243613848, 0.7773170766911654539, 0.8047378541243613848),
 ( 1.000000000000000000, 0.9659258262890683122, 1.000000000000000000, 0.9659258262890683122, 1.000000000000000000, 0.9659258262890683122, 1.000000000000000000, 0.9659258262890683122, 1.000000000000000000, 0.9659258262890683122, 1.000000000000000000, 0.9659258262890683122, 1.000000000000000000, 0.9659258262890683122, 1.000000000000000000, 0.9659258262890683122, 1.000000000000000000, 0.9659258262890683122, 1.000000000000000000, 0.9659258262890683122, 1.000000000000000000, 0.9659258262890683122, 1.000000000000000000, 0.9659258262890683122, 1.000000000000000000, 0.9659258262890683122, 1.000000000000000000, 0.9659258262890683122, 1.000000000000000000, 0.9659258262890683122, 1.000000000000000000, 0.9659258262890683122, 1.000000000000000000, 0.9659258262890683122, 1.000000000000000000, 0.9659258262890683122, 1.000000000000000000, 0.9659258262890683122, 1.000000000000000000, 0.9659258262890683122, 1.000000000000000000, 0.9659258262890683122, 1.000000000000000000, 0.9659258262890683122, 1.000000000000000000, 0.9659258262890683122, 1.000000000000000000, 0.9659258262890683122, 1.000000000000000000, 0.9659258262890683122, 1.000000000000000000, 0.9659258262890683122, 1.000000000000000000, 0.9659258262890683122, 1.000000000000000000, 0.9659258262890683122, 1.000000000000000000, 0.9659258262890683122, 1.000000000000000000, 0.9659258262890683122, 1.000000000000000000, 0.9659258262890683122, 1.000000000000000000, 0.9659258262890683122, 1.000000000000000000, 0.9659258262890683122, 1.000000000000000000, 0.9659258262890683122, 1.000000000000000000, 0.9659258262890683122, 1.000000000000000000, 0.9659258262890683122, 1.000000000000000000, 0.9659258262890683122, 1.000000000000000000, 0.9659258262890683122, 1.000000000000000000, 0.9659258262890683122, 1.000000000000000000, 0.9659258262890683122, 1.000000000000000000, 0.9659258262890683122, 1.000000000000000000, 0.9659258262890683122, 1.000000000000000000, 0.9659258262890683122, 1.000000000000000000, 0.9659258262890683122, 1.000000000000000000, 0.9659258262890683122, 1.000000000000000000, 0.9659258262890683122, 1.000000000000000000, 0.9659258262890683122, 1.000000000000000000, 0.9659258262890683122, 1.000000000000000000, 0.9659258262890683122, 1.000000000000000000, 0.9659258262890683122, 1.000000000000000000, 0.9659258262890683122, 1.000000000000000000, 0.9659258262890683122, 1.000000000000000000, 0.9659258262890683122, 1.000000000000000000, 0.9659258262890683122, 1.000000000000000000, 0.9659258262890683122, 1.000000000000000000, 0.9659258262890683122, 1.000000000000000000, 0.9659258262890683122, 1.000000000000000000, 0.9659258262890683122, 1.000000000000000000, 0.9659258262890683122, 1.000000000000000000, 0.9659258262890683122, 1.000000000000000000, 0.9659258262890683122, 1.000000000000000000, 0.9659258262890683122, 1.000000000000000000, 0.9659258262890683122, 1.000000000000000000, 0.9659258262890683122, 1.000000000000000000, 0.9659258262890683122, 1.000000000000000000, 0.9659258262890683122, 1.000000000000000000, 0.9659258262890683122, 1.000000000000000000, 0.9659258262890683122, 1.000000000000000000, 0.9659258262890683122, 1.000000000000000000, 0.9659258262890683122, 1.000000000000000000, 0.9659258262890683122, 1.000000000000000000, 0.9659258262890683122, 1.000000000000000000, 0.9659258262890683122, 1.000000000000000000, 0.9659258262890683122, 1.000000000000000000, 0.9659258262890683122, 1.000000000000000000, 0.9659258262890683122, 1.000000000000000000, 0.9659258262890683122, 1.000000000000000000, 0.9659258262890683122, 1.000000000000000000, 0.9659258262890683122, 1.000000000000000000, 0.9659258262890683122, 1.000000000000000000, 0.9659258262890683122, 1.000000000000000000, 0.9659258262890683122, 1.000000000000000000, 0.9659258262890683122, 1.000000000000000000, 0.9659258262890683122, 1.000000000000000000, 0.9659258262890683122, 1.000000000000000000, 0.9659258262890683122, 1.000000000000000000, 0.9659258262890683122, 1.000000000000000000, 0.9659258262890683122, 1.000000000000000000, 0.9659258262890683122, 1.000000000000000000, 0.9659258262890683122, 1.000000000000000000, 0.9659258262890683122, 1.000000000000000000, 0.9659258262890683122, 1.000000000000000000, 0.9659258262890683122, 1.000000000000000000, 0.9659258262890683122, 1.000000000000000000, 0.9659258262890683122, 1.000000000000000000, 0.9659258262890683122, 1.000000000000000000, 0.9659258262890683122, 1.000000000000000000, 0.9659258262890683122, 1.000000000000000000, 0.9659258262890683122, 1.000000000000000000, 0.9659258262890683122, 1.000000000000000000, 0.9659258262890683122, 1.000000000000000000, 0.9659258262890683122, 1.000000000000000000, 0.9659258262890683122, 1.000000000000000000, 0.9659258262890683122, 1.000000000000000000, 0.9659258262890683122, 1.000000000000000000, 0.9659258262890683122, 1.000000000000000000, 0.9659258262890683122, 1.000000000000000000, 0.9659258262890683122, 1.000000000000000000, 0.9659258262890683122, 1.000000000000000000, 0.9659258262890683122, 1.000000000000000000, 0.9659258262890683122, 1.000000000000000000, 0.9659258262890683122, 1.000000000000000000, 0.9659258262890683122, 1.000000000000000000, 0.9659258262890683122, 1.000000000000000000, 0.9659258262890683122, 1.000000000000000000, 0.9659258262890683122, 1.000000000000000000, 0.9659258262890683122, 1.000000000000000000, 0.9659258262890683122, 1.000000000000000000, 0.9659258262890683122, 1.000000000000000000, 0.9659258262890683122, 1.000000000000000000, 0.9659258262890683122, 1.000000000000000000, 0.9659258262890683122, 1.000000000000000000, 0.9659258262890683122, 1.000000000000000000, 0.9659258262890683122, 1.000000000000000000, 0.9659258262890683122, 1.000000000000000000, 0.9659258262890683122, 1.000000000000000000, 0.9659258262890683122, 1.000000000000000000, 0.9659258262890683122, 1.000000000000000000, 0.9659258262890683122, 1.000000000000000000, 0.9659258262890683122, 1.000000000000000000, 0.9659258262890683122, 1.000000000000000000, 0.9659258262890683122, 1.000000000000000000, 0.9659258262890683122, 1.000000000000000000, 0.9659258262890683122, 1.000000000000000000, 0.9659258262890683122, 1.000000000000000000, 0.9659258262890683122, 1.000000000000000000, 0.9659258262890683122, 1.000000000000000000, 0.9659258262890683122, 1.000000000000000000, 0.9659258262890683122, 1.000000000000000000, 0.9659258262890683122, 1.000000000000000000, 0.9659258262890683122, 1.000000000000000000, 0.9659258262890683122, 1.000000000000000000, 0.9659258262890683122, 1.000000000000000000, 0.9659258262890683122, 1.000000000000000000, 0.9659258262890683122, 1.000000000000000000, 0.9659258262890683122, 1.000000000000000000, 0.9659258262890683122, 1.000000000000000000, 0.9659258262890683122, 1.000000000000000000, 0.9659258262890683122, 1.000000000000000000, 0.9659258262890683122, 1.000000000000000000, 0.9659258262890683122, 1.000000000000000000, 0.9659258262890683122, 1.000000000000000000, 0.9659258262890683122, 1.000000000000000000, 0.9659258262890683122, 1.000000000000000000, 0.9659258262890683122, 1.000000000000000000, 0.9659258262890683122, 1.000000000000000000, 0.9659258262890683122, 1.000000000000000000, 0.9659258262890683122, 1.000000000000000000, 0.9659258262890683122, 1.000000000000000000, 0.9659258262890683122, 1.000000000000000000, 0.9659258262890683122, 1.000000000000000000, 0.9659258262890683122, 1.000000000000000000, 0.9659258262890683122, 1.000000000000000000, 0.9659258262890683122, 1.000000000000000000, 0.9659258262890683122, 1.000000000000000000, 0.9659258262890683122, 1.000000000000000000, 0.9659258262890683122, 1.000000000000000000, 0.9659258262890683122, 1.000000000000000000, 0.9659258262890683122, 1.000000000000000000, 0.9659258262890683122, 1.000000000000000000, 0.9659258262890683122, 1.000000000000000000, 0.9659258262890683122, 1.000000000000000000, 0.9659258262890683122, 1.000000000000000000, 0.9659258262890683122, 1.000000000000000000, 0.9659258262890683122, 1.000000000000000000, 0.9659258262890683122, 1.000000000000000000, 0.9659258262890683122, 1.000000000000000000, 0.9659258262890683122, 1.000000000000000000, 0.9659258262890683122, 1.000000000000000000, 0.9659258262890683122, 1.000000000000000000, 0.9659258262890683122, 1.000000000000000000, 0.9659258262890683122, 1.000000000000000000, 0.9659258262890683122, 1.000000000000000000, 0.9659258262890683122, 1.000000000000000000, 0.9659258262890683122, 1.000000000000000000, 0.9659258262890683122, 1.000000000000000000, 0.9659258262890683122, 1.000000000000000000, 0.9659258262890683122, 1.000000000000000000, 0.9659258262890683122, 1.000000000000000000, 0.9659258262890683122, 1.000000000000000000, 0.9659258262890683122, 1.000000000000000000, 0.9659258262890683122, 1.000000000000000000, 0.9659258262890683122, 1.000000000000000000, 0.9659258262890683122, 1.000000000000000000, 0.9659258262890683122, 1.000000000000000000, 0.9659258262890683122, 1.000000000000000000, 0.9659258262890683122, 1.000000000000000000, 0.9659258262890683122, 1.000000000000000000, 0.9659258262890683122, 1.000000000000000000, 0.9659258262890683122, 1.000000000000000000, 0.9659258262890683122, 1.000000000000000000, 0.9659258262890683122, 1.000000000000000000, 0.9659258262890683122, 1.000000000000000000, 0.9659258262890683122, 1.000000000000000000, 0.9659258262890683122, 1.000000000000000000, 0.9659258262890683122, 1.000000000000000000, 0.9659258262890683122, 1.000000000000000000, 0.9659258262890683122, 1.000000000000000000, 0.9659258262890683122, 1.000000000000000000, 0.9659258262890683122, 1.000000000000000000, 0.9659258262890683122, 1.000000000000000000, 0.9659258262890683122, 1.000000000000000000, 0.9659258262890683122, 1.000000000000000000, 0.9659258262890683122, 1.000000000000000000, 0.9659258262890683122, 1.000000000000000000, 0.9659258262890683122, 1.000000000000000000, 0.9659258262890683122, 1.000000000000000000, 0.9659258262890683122, 1.000000000000000000, 0.9659258262890683122, 1.000000000000000000, 0.9659258262890683122, 1.000000000000000000, 0.9659258262890683122, 1.000000000000000000, 0.9659258262890683122, 1.000000000000000000, 0.9659258262890683122, 1.000000000000000000, 0.9659258262890683122, 1.000000000000000000, 0.9659258262890683122, 1.000000000000000000, 0.9659258262890683122, 1.000000000000000000, 0.9659258262890683122, 1.000000000000000000, 0.9659258262890683122, 1.000000000000000000, 0.9659258262890683122, 1.000000000000000000, 0.9659258262890683122, 1.000000000000000000, 0.9659258262890683122, 1.000000000000000000, 0.9659258262890683122, 1.000000000000000000, 0.9659258262890683122, 1.000000000000000000, 0.9659258262890683122, 1.000000000000000000, 0.9659258262890683122, 1.000000000000000000, 0.9659258262890683122, 1.000000000000000000, 0.9659258262890683122, 1.000000000000000000) ) ) 
 REPRESENTATION_ITEM ( '' )  SURFACE ( )  );
#17581 = VERTEX_POINT ( 'NONE', #45351 ) ;
#17582 = CARTESIAN_POINT ( 'NONE',  ( 0.1958661417322836718, -0.3392501089628017219, -0.7185232527897132959 ) ) ;
#17583 = ORIENTED_EDGE ( 'NONE', *, *, #66595, .T. ) ;
#17584 = CARTESIAN_POINT ( 'NONE',  ( -0.8267716535433065062, -0.6692913385826771977, 8.415575281601705876E-17 ) ) ;
#17585 = CARTESIAN_POINT ( 'NONE',  ( -0.1902887139107604098, 0.2952755905511810774, -0.1292274648535930714 ) ) ;
#17586 = CARTESIAN_POINT ( 'NONE',  ( -0.3674540682414689785, 0.2306618581243848609, 0.2411417322834645549 ) ) ;
#17587 = CARTESIAN_POINT ( 'NONE',  ( 0.3346456692913393205, -0.5400638737290845981, -0.3530559997133363437 ) ) ;
#17588 = CARTESIAN_POINT ( 'NONE',  ( -0.4396325459317577122, -0.6692913385826773087, -0.1292274648535924053 ) ) ;
#17589 = CARTESIAN_POINT ( 'NONE',  ( -1.227034120734907141, -0.6692913385826773087, -0.1292274648535924053 ) ) ;
#17590 =( GEOMETRIC_REPRESENTATION_CONTEXT ( 3 ) GLOBAL_UNCERTAINTY_ASSIGNED_CONTEXT ( ( #60484 ) ) GLOBAL_UNIT_ASSIGNED_CONTEXT ( ( #6359, #38344, #5942 ) ) REPRESENTATION_CONTEXT ( 'NONE', 'WORKASPACE' ) );
#17591 = CARTESIAN_POINT ( 'NONE',  ( -0.6167979002624665030, 0.05413385826771666132, 0.4176697321401328100 ) ) ;
#17592 = CARTESIAN_POINT ( 'NONE',  ( 0.9383202099737536495, -0.3162353388693405765, 0.4822834645669290543 ) ) ;
#17593 = CARTESIAN_POINT ( 'NONE',  ( 0.6299212598425204535, -0.1870078740157479769, 0.4822834645669291653 ) ) ;
#17594 = CARTESIAN_POINT ( 'NONE',  ( 0.1958661417322836440, -0.3392501089628017219, -1.186351706036745446 ) ) ;
#17595 = CARTESIAN_POINT ( 'NONE',  ( -0.5577427821522301654, -0.2845877964562159024, 0.3641732283464567677 ) ) ;
#17596 = VERTEX_POINT ( 'NONE', #25165 ) ;
#17597 = CARTESIAN_POINT ( 'NONE',  ( 0.1058382717557500713, -0.3949938075777409408, -1.660104986876640654 ) ) ;
#17598 = ORIENTED_EDGE ( 'NONE', *, *, #18267, .F. ) ;
#17599 = CARTESIAN_POINT ( 'NONE',  ( -1.318897637795274802, -0.4536011799217368745, -0.2665933059059886201 ) ) ;
#17600 = CARTESIAN_POINT ( 'NONE',  ( -1.069553805774277722, -0.6692913385826773087, -0.1292274648535924053 ) ) ;
#17601 = CARTESIAN_POINT ( 'NONE',  ( -0.3871391076115476282, -0.05778040916215522460, 0.4822834645669289988 ) ) ;
#17602 = LINE ( 'NONE', #10040, #51520 ) ;
#17603 = CARTESIAN_POINT ( 'NONE',  ( -0.8136482939632537770, -0.6046776061558807314, 0.2411417322834647770 ) ) ;
#17604 = CARTESIAN_POINT ( 'NONE',  ( -1.017060367454067249, -0.3162353388693409650, -0.4822834645669289433 ) ) ;
#17605 = DIRECTION ( 'NONE',  ( -3.096699300667737957E-16, 1.000000000000000000, -0.000000000000000000 ) ) ;
#17606 = CARTESIAN_POINT ( 'NONE',  ( -0.4359958488159583201, 1.724409448818897905, -3.912791665790201101 ) ) ;
#17607 = CARTESIAN_POINT ( 'NONE',  ( 0.7874015748031503170, -0.1870078740157480601, -0.3641732283464567677 ) ) ;
#17608 = DIRECTION ( 'NONE',  ( 0.000000000000000000, -1.000000000000000000, 0.000000000000000000 ) ) ;
#17609 = CARTESIAN_POINT ( 'NONE',  ( -0.3917322834645670104, -7.196005306013484475E-17, 0.1909448818897636901 ) ) ;
#17610 = CARTESIAN_POINT ( 'NONE',  ( -0.02624671916010428221, -0.5023911411419708095, 0.1820866141732285504 ) ) ;
#17611 = CARTESIAN_POINT ( 'NONE',  ( -0.4527559055118102749, -0.5400638737290845981, -0.3530559997133363437 ) ) ;
#17612 = CARTESIAN_POINT ( 'NONE',  ( 3.911297246792111881, 1.384105334947628885, 0.4492278415794215274 ) ) ;
#17613 = CARTESIAN_POINT ( 'NONE',  ( 0.05249343832021075018, -0.6046776061558807314, 0.2411417322834647770 ) ) ;
#17614 = ORIENTED_EDGE ( 'NONE', *, *, #26633, .T. ) ;
#17615 = CARTESIAN_POINT ( 'NONE',  ( 0.1070741851644054915, -0.3996062992125986035, -1.975065616797900381 ) ) ;
#17616 = CARTESIAN_POINT ( 'NONE',  ( 0.000000000000000000, 0.4201155382560080032, 0.000000000000000000 ) ) ;
#17617 = VERTEX_POINT ( 'NONE', #25578 ) ;
#17618 = CARTESIAN_POINT ( 'NONE',  ( 0.3996062992125984925, 0.1070741851644054637, -1.461286089238844843 ) ) ;
#17619 = DIRECTION ( 'NONE',  ( 1.408710688920637755E-15, -1.000000000000000000, 4.918487082195260922E-30 ) ) ;
#17620 = CARTESIAN_POINT ( 'NONE',  ( -0.7217847769028863381, -0.004921259842519870586, -0.3153832671262229437 ) ) ;
#17621 = CARTESIAN_POINT ( 'NONE',  ( -0.8595800524934373854, -0.3162353388693409650, -0.4822834645669289433 ) ) ;
#17622 = CARTESIAN_POINT ( 'NONE',  ( -0.1265901696524986964, -0.4724409448818899238, -0.2296587926509186250 ) ) ;
#17623 = DIRECTION ( 'NONE',  ( 0.000000000000000000, -1.000000000000000000, 0.000000000000000000 ) ) ;
#17624 = CARTESIAN_POINT ( 'NONE',  ( -0.3392501089628017219, -0.1958661417322836718, 0.1128608923884514836 ) ) ;
#17625 = CARTESIAN_POINT ( 'NONE',  ( 1.496062992125985147, -0.1870078740157479769, 0.4822834645669291653 ) ) ;
#17626 = CARTESIAN_POINT ( 'NONE',  ( 0.2624671916010504757, -0.6046776061558809534, -0.2411417322834644161 ) ) ;
#17627 = CARTESIAN_POINT ( 'NONE',  ( 0.4002624671916016896, -0.05778040916215522460, 0.4822834645669289988 ) ) ;
#17628 = CARTESIAN_POINT ( 'NONE',  ( -0.8136482939632537770, 0.1283753931104746893, -0.1820866141732285504 ) ) ;
#17629 = CARTESIAN_POINT ( 'NONE',  ( -0.2362204724409442680, -0.1870078740157480879, -0.4822834645669291653 ) ) ;
#17630 = CARTESIAN_POINT ( 'NONE',  ( 0.1265901696524989462, 0.4724409448818897572, -2.432414698162729039 ) ) ;
#17631 = CARTESIAN_POINT ( 'NONE',  ( -1.056430446194224881, 0.2952755905511810774, -0.1292274648535930714 ) ) ;
#17632 = CARTESIAN_POINT ( 'NONE',  ( 0.3420746716998660508, -0.1974969037888704149, -2.229002624671915900 ) ) ;
#17633 = CARTESIAN_POINT ( 'NONE',  ( 1.200787401574803681, -0.4536011799217368745, -0.2665933059059886201 ) ) ;
#17634 = CARTESIAN_POINT ( 'NONE',  ( -0.2952755905511804668, 0.07958543189024085140, 0.2665933059059887866 ) ) ;
#17635 = CARTESIAN_POINT ( 'NONE',  ( 0.9842519685039378130, -0.5511811023622047445, 6.969142054262312111E-17 ) ) ;
#17636 = CARTESIAN_POINT ( 'NONE',  ( -1.417322834645668772, -0.1870078740157479769, 0.4822834645669291653 ) ) ;
#17637 = VECTOR ( 'NONE', #78588, 39.37007874015748143 ) ;
#17638 = CARTESIAN_POINT ( 'NONE',  ( -1.023622047244093558, -0.1870078740157479769, 0.3641732283464567677 ) ) ;
#17639 = CARTESIAN_POINT ( 'NONE',  ( -0.4091458600556402980, -0.2362204724409451284, -2.176509186351706315 ) ) ;
#17640 = CARTESIAN_POINT ( 'NONE',  ( 0.5971128608923891301, 0.1771653543307087075, -0.09757992244046823083 ) ) ;
#17641 = CARTESIAN_POINT ( 'NONE',  ( -0.4855643044619415427, 0.05413385826771626580, -0.4176697321401330321 ) ) ;
#17642 = FACE_OUTER_BOUND ( 'NONE', #25546, .T. ) ;
#17643 = CARTESIAN_POINT ( 'NONE',  ( -0.01312335958005186876, -0.004921259842519870586, -0.3153832671262229437 ) ) ;
#17644 = CARTESIAN_POINT ( 'NONE',  ( 0.4724409448818898682, 2.892866454678787531E-17, -0.9822834645669291653 ) ) ;
#17645 = CARTESIAN_POINT ( 'NONE',  ( 0.5774278215223104249, 0.2306618581243848609, 0.2411417322834645549 ) ) ;
#17646 = CYLINDRICAL_SURFACE ( 'NONE', #18304, 0.4724409448818898682 ) ;
#17647 = CARTESIAN_POINT ( 'NONE',  ( 1.528871391076116026, -0.5511811023622048555, -0.09757992244046775898 ) ) ;
#17648 = CARTESIAN_POINT ( 'NONE',  ( -0.9908136482939626788, -0.6692913385826773087, -0.1292274648535924053 ) ) ;
#17649 = CARTESIAN_POINT ( 'NONE',  ( -0.2099737532808391705, 0.1283753931104748280, 0.1820866141732283561 ) ) ;
#17650 = CARTESIAN_POINT ( 'NONE',  ( 1.036041590146032698, 3.421639014772782816E-16, 0.3464511005275203726 ) ) ;
#17651 = CARTESIAN_POINT ( 'NONE',  ( 0.1181102362204730916, -0.5511811023622047445, 6.969142054262312111E-17 ) ) ;
#17652 = AXIS2_PLACEMENT_3D ( 'NONE', #58166, #1782, #53103 ) ;
#17653 = EDGE_CURVE ( 'NONE', #81379, #38353, #33199, .T. ) ;
#17654 = CARTESIAN_POINT ( 'NONE',  ( -0.3674540682414689785, 0.2306618581243848609, 0.2411417322834645549 ) ) ;
#17655 = CARTESIAN_POINT ( 'NONE',  ( -0.3460692066303957537, -0.1998031496062994405, -0.6017060367454067915 ) ) ;
#17656 = ADVANCED_FACE ( 'NONE', ( #58405 ), #51242, .T. ) ;
#17657 = CARTESIAN_POINT ( 'NONE',  ( -0.3392501089628019995, 0.1958661417322832277, -2.158136482939632561 ) ) ;
#17658 = CARTESIAN_POINT ( 'NONE',  ( 0.8070866141732288002, 0.07958543189024085140, 0.2665933059059887866 ) ) ;
#17659 = CARTESIAN_POINT ( 'NONE',  ( -0.4068241469816264999, -0.4281496062992124485, 0.4176697321401328655 ) ) ;
#17660 = CARTESIAN_POINT ( 'NONE',  ( -0.9120734908136475250, -0.6692913385826773087, -0.1292274648535924053 ) ) ;
#17661 = CARTESIAN_POINT ( 'NONE',  ( -0.8923884514435688198, -0.5023911411419708095, 0.1820866141732285504 ) ) ;
#17662 = CARTESIAN_POINT ( 'NONE',  ( -3.924551336943372881, 1.180704189158721329, 0.3131659068132852108 ) ) ;
#17663 = CARTESIAN_POINT ( 'NONE',  ( -0.1115485564304453947, -0.6692913385826771977, 0.1292274648535927661 ) ) ;
#17664 = CARTESIAN_POINT ( 'NONE',  ( -1.187664041994750175, -0.08942795157528024563, -0.3641732283464568787 ) ) ;
#17665 = CARTESIAN_POINT ( 'NONE',  ( -1.522309711286088607, -0.6046776061558807314, 0.2411417322834647770 ) ) ;
#17666 = CARTESIAN_POINT ( 'NONE',  ( -0.5314960629921123836, 2.755905511811024056, -3.900966923095591454 ) ) ;
#17667 = ORIENTED_EDGE ( 'NONE', *, *, #11964, .F. ) ;
#17668 = CARTESIAN_POINT ( 'NONE',  ( -1.568241469816272105, -0.08942795157527998196, 0.3641732283464567121 ) ) ;
#17669 = CARTESIAN_POINT ( 'NONE',  ( -1.246719160104986512, 0.05413385826771666132, 0.4176697321401328100 ) ) ;
#17670 = CARTESIAN_POINT ( 'NONE',  ( -0.9055118110236215490, 0.2952755905511811885, 0.000000000000000000 ) ) ;
#17671 = CARTESIAN_POINT ( 'NONE',  ( 1.568241469816273437, -0.3162353388693405765, 0.4822834645669290543 ) ) ;
#17672 = CARTESIAN_POINT ( 'NONE',  ( 0.1049643490035304938, -0.3917322834645669549, -1.429790026246719359 ) ) ;
#17673 = CARTESIAN_POINT ( 'NONE',  ( -0.2143816077119332086, 0.3285422586334138528, -1.220472440944882386 ) ) ;
#17674 = EDGE_CURVE ( 'NONE', #60217, #63415, #12555, .T. ) ;
#17675 = CARTESIAN_POINT ( 'NONE',  ( 0.7939632545931766261, -0.3162353388693409650, -0.4822834645669289433 ) ) ;
#17676 = CARTESIAN_POINT ( 'NONE',  ( 0.2755905511811031494, 0.2952755905511811885, 0.000000000000000000 ) ) ;
#17677 = DIRECTION ( 'NONE',  ( -0.000000000000000000, -1.000000000000000000, -0.000000000000000000 ) ) ;
#17678 = CARTESIAN_POINT ( 'NONE',  ( -0.1998031496062994405, 0.3460692066303957537, -2.452099737532808188 ) ) ;
#17679 = CARTESIAN_POINT ( 'NONE',  ( 1.345144356955381593, -0.2845877964562161244, -0.3641732283464567121 ) ) ;
#17680 = CARTESIAN_POINT ( 'NONE',  ( 0.3460692066303959757, -0.1998031496062991907, -0.8923884514435694859 ) ) ;
#17681 = ORIENTED_EDGE ( 'NONE', *, *, #39809, .F. ) ;
#17682 = CARTESIAN_POINT ( 'NONE',  ( -0.9645669291338575535, 0.07958543189024071263, -0.2665933059059888421 ) ) ;
#17683 = CARTESIAN_POINT ( 'NONE',  ( -0.3392501089628017219, -0.1958661417322836718, -2.564304461942256808 ) ) ;
#17684 = ORIENTED_EDGE ( 'NONE', *, *, #63827, .T. ) ;
#17685 = CARTESIAN_POINT ( 'NONE',  ( 0.4461942257217855201, -0.6046776061558807314, 0.2411417322834647770 ) ) ;
#17686 = CARTESIAN_POINT ( 'NONE',  ( -0.2296587926509179312, -0.3162353388693409650, -0.4822834645669289433 ) ) ;
#17687 = CARTESIAN_POINT ( 'NONE',  ( -1.030183727034119867, -0.3162353388693405765, 0.4822834645669290543 ) ) ;
#17688 = CARTESIAN_POINT ( 'NONE',  ( 1.135170603674541256, -0.6692913385826773087, -0.1292274648535924053 ) ) ;
#17689 = CARTESIAN_POINT ( 'NONE',  ( 1.555118110236221041, 0.1660481256975883668, -0.3530559997133364547 ) ) ;
#17690 = CARTESIAN_POINT ( 'NONE',  ( 0.000000000000000000, 0.000000000000000000, 0.000000000000000000 ) ) ;
#17691 = CARTESIAN_POINT ( 'NONE',  ( -0.1181102362204717315, -0.6692913385826771977, 8.415575281601705876E-17 ) ) ;
#17692 = AXIS2_PLACEMENT_3D ( 'NONE', #9428, #1871, #28362 ) ;
#17693 = CARTESIAN_POINT ( 'NONE',  ( -1.220472440944881054, -0.6692913385826771977, 8.415575281601705876E-17 ) ) ;
#17694 = DIRECTION ( 'NONE',  ( 1.000000000000000000, -0.000000000000000000, -0.000000000000000000 ) ) ;
#17695 = CARTESIAN_POINT ( 'NONE',  ( 0.4734688692633114981, 1.503144958756604366, -2.556625226394979578 ) ) ;
#17696 = CARTESIAN_POINT ( 'NONE',  ( 4.797336870675656522E-17, -0.3917322834645670104, -2.683070866141731958 ) ) ;
#17697 = CARTESIAN_POINT ( 'NONE',  ( 0.9973753280839902091, -0.5023911411419708095, 0.1820866141732285504 ) ) ;
#17698 = ORIENTED_EDGE ( 'NONE', *, *, #74163, .T. ) ;
#17699 = CARTESIAN_POINT ( 'NONE',  ( -0.3949938075777409408, -0.1058382717557502933, -0.2034120734908137218 ) ) ;
#17700 = CARTESIAN_POINT ( 'NONE',  ( -0.9317585301837263412, -0.4281496062992127816, -0.4176697321401328100 ) ) ;
#17701 = EDGE_LOOP ( 'NONE', ( #52951, #36072, #42734, #40595 ) ) ;
#17702 = CARTESIAN_POINT ( 'NONE',  ( 0.1443569553805781891, -0.3690944881889763329, 0.3153832671262228327 ) ) ;
#17703 = CARTESIAN_POINT ( 'NONE',  ( -1.548556430446193399, 0.2306618581243848609, 0.2411417322834645549 ) ) ;
#17704 = CARTESIAN_POINT ( 'NONE',  ( 0.3740157480314966754, 0.1660481256975883668, -0.3530559997133364547 ) ) ;
#17705 = CARTESIAN_POINT ( 'NONE',  ( 0.5774278215223103139, -0.6046776061558809534, -0.2411417322834644161 ) ) ;
#17706 = CARTESIAN_POINT ( 'NONE',  ( -0.6430446194225716283, -0.4281496062992124485, 0.4176697321401328655 ) ) ;
#17707 = CARTESIAN_POINT ( 'NONE',  ( -0.3917322834645670659, -7.196005306013484475E-17, -1.295951074312022833 ) ) ;
#17708 = CARTESIAN_POINT ( 'NONE',  ( -1.115485564304461219, 0.05413385826771626580, -0.4176697321401330321 ) ) ;
#17709 = CARTESIAN_POINT ( 'NONE',  ( 0.2867679344610365999, -0.2867679344610365444, -2.702755905511810663 ) ) ;
#17710 = CARTESIAN_POINT ( 'NONE',  ( 1.108923884514436242, -0.08942795157527998196, 0.3641732283464567121 ) ) ;
#17711 = CARTESIAN_POINT ( 'NONE',  ( -1.049868766404198794, -0.6046776061558807314, 0.2411417322834647770 ) ) ;
#17712 = CARTESIAN_POINT ( 'NONE',  ( 1.082677165354331228, 0.1660481256975883668, -0.3530559997133364547 ) ) ;
#17713 = CARTESIAN_POINT ( 'NONE',  ( 1.351706036745407680, 0.05413385826771666132, 0.4176697321401328100 ) ) ;
#17714 = CARTESIAN_POINT ( 'NONE',  ( -0.3996062992125986035, -0.1070741851644056997, -0.8333333333333332593 ) ) ;
#17715 = CARTESIAN_POINT ( 'NONE',  ( -1.541994750656167090, 0.2952755905511811885, 0.1292274648535926551 ) ) ;
#17716 = CARTESIAN_POINT ( 'NONE',  ( 0.2925321140481932369, 0.2925321140481932369, -0.3720472440944882497 ) ) ;
#17717 = CARTESIAN_POINT ( 'NONE',  ( 0.2952755905511816326, -0.5400638737290844871, 0.3530559997133364547 ) ) ;
#17718 = CARTESIAN_POINT ( 'NONE',  ( 0.3460692066303959757, -0.1998031496062991907, -2.309711286089239035 ) ) ;
#17719 =( BOUNDED_SURFACE ( )  B_SPLINE_SURFACE ( 1, 2, ( 
 ( #82402, #69355, #81588, #49155, #74861, #11287, #17609, #12518, #50799, #38179, #37364, #56299, #68529, #81996, #18828, #75266, #56703, #49570, #11709, #76500, #76086, #17203, #70165, #5778, #57111, #62206, #62624, #44474, #10870, #36947, #12109, #69764, #31035, #37767, #4136, #5374, #24720, #23905, #24310, #29801, #4543, #4967, #63036, #42836, #44072, #82805, #30634, #30214, #55462, #68938, #31447, #49980, #36530, #25129, #81171, #23489, #55876, #75678, #18018, #43653, #58365, #77324, #13775, #71428, #77749, #25961, #39007, #51207, #78592, #19653, #58795, #45315, #6191, #39432, #14617, #14200, #20082, #71010, #57529, #13354, #78170, #7030, #46571, #65548, #64274, #20917, #45732, #1153, #6609, #31869, #70584, #51619, #46155, #71850, #27220, #25541, #64691, #32699, #44884, #39857, #26804, #12938, #72269, #7879, #19234, #728, #33543, #59205, #83220, #52044, #76904, #65118, #32280, #1566, #26386, #38596, #57940, #7455, #33125, #306, #52462, #20501, #52881, #63854, #27638, #61175, #81801, #16584, #68742, #4755, #67505, #42643, #16167, #1974, #72678, #4346, #74240, #36335, #55265, #53300, #42229, #40271, #62009, #8290, #30431, #65954, #75481, #36741, #35932, #30013, #79012, #11084, #61599, #62417, #80975, #23288, #56096, #9840, #46984, #33958, #59620, #21332, #74659, #55676, #17416, #41813, #81385, #48958, #35511, #67924, #24112, #17003, #10679, #3945, #49781, #3529, #29195, #54862, #80567, #22878, #48540, #68340, #10264, #23701, #29604, #49372, #75068, #43046, #69968, #12322, #19455, #50191, #56915, #63243, #37980, #25758, #12735, #45106, #37160, #11504, #30840, #5583, #64074, #24525, #76305, #51420, #69567, #18634, #31249, #82611, #31665, #44278, #50597, #5994, #69153, #57326, #19037, #57742, #24928, #6411, #104, #77122, #32081, #83020, #63655, #18229, #62842, #5176, #25343, #37569, #17822, #43455, #56505, #44684, #51005, #76704, #70380, #82207, #38394, #75888, #43868, #11915, #56362, #81655, #80423, #75740, #69001, #62688, #67779, #68194, #82061, #74093, #16855, #17672, #75326, #36590, #43303, #43716, #10933, #62268, #29459, #42898, #23966, #16439, #11352, #55526, #55940, #4605, #42084, #35779, #55117, #49633, #10117, #68592, #37010, #5030, #30698, #61448, #80826, #30277, #24374, #50045, #35368, #18081, #9698, #3795, #22734, #36187, #42490, #10532, #61033, #3383, #49219, #74925, #17270, #23551, #23140, #61859, #48393, #29045, #48809, #54716, #74508, #4200, #29864, #81235, #19722, #83284, #76562, #63099, #18890, #373, #12585, #52108, #71077, #69826, #795, #51270, #64338, #12175, #11773, #76151, #31516, #51688, #77391, #32766, #31099, #57174, #44539, #50449, #45380, #6675, #18491, #77816, #13419, #24781, #70230, #39076, #64757, #5438, #57594, #56766, #25607, #37833, #7096, #50862, #44134, #63511, #76972, #44954, #5841, #82872, #25196, #58433, #26456, #82465, #38243, #20147, #63920, #69418, #37426, #6255, #70650, #31932, #19302, #13005, #32347, #38661, #58008, #26028, #33194, #78657, #45796, #66430, #13842, #9185, #71494, #79903, #41163, #40338, #8765, #1219, #15505, #66018, #66853, #2038, #59682, #34857, #71916, #52529, #39500, #65188, #7524, #79077, #34440, #21799, #26868, #8354, #60519, #46220, #20978, #21393, #78236, #60107, #2868, #46638, #20569, #58862, #27283, #28118, #65614, #14266, #40746, #28531, #2460, #47049, #27703, #59269, #39925, #34022, #1626, #72741, #54188, #53367, #53773, #7945, #33606, #15088, #52943, #79485, #47463, #72333, #14681, #73155, #11794, #3821, #50067, #48833, #49245, #63121, #55141, #81259, #82083, #56384, #17696, #24397, #24804, #75348, #43324, #10555, #23990, #5052, #80852, #75762, #36614, #37032, #69024, #23164, #16880, #36213, #62714, #74534, #49658, #30722, #43737, #18104, #42518, #61882, #11375, #69442, #37447, #16463, #5459, #74117, #68221 ),
 ( #55966, #31121, #4223, #42108, #29887, #55550, #56788, #82488, #67805, #35807, #23574, #74948, #17294, #10142, #61473, #42921, #29482, #68616, #10956, #62292, #4629, #30300, #81679, #38684, #69847, #64362, #18912, #58458, #31956, #25217, #5863, #6699, #26053, #50883, #70253, #76583, #39521, #20167, #37856, #12608, #7546, #25630, #77838, #13862, #44562, #51712, #38266, #12198, #82897, #13442, #83308, #45403, #32368, #63532, #51293, #50471, #71099, #18512, #65209, #76175, #1241, #63943, #58032, #395, #58882, #6280, #76996, #57617, #77413, #33219, #818, #44155, #31539, #57195, #19327, #44979, #52131, #70675, #13031, #19749, #39098, #64780, #7118, #32789, #26480, #45817, #71516, #2481, #20589, #79508, #66877, #47898, #66039, #79928, #73606, #67284, #28556, #21824, #8788, #21000, #71937, #14286, #34042, #40359, #35288, #15948, #60950, #60130, #79098, #7966, #21417, #41594, #14704, #47487, #72356, #34461, #9617, #15529, #28140, #26890, #39950, #2892, #1649, #2060, #52549, #33629, #59705, #34880, #9207, #53796, #60541, #78258, #73179, #41187, #46662, #54212, #22243, #59292, #46241, #72762, #65636, #27306, #52965, #78679, #8377, #27724, #53391, #47071, #15113, #40767, #66452, #35697, #48729, #81571, #68923, #81981, #28965, #11272, #3300, #55040, #16358, #29787, #36110, #61782, #4949, #24295, #42822, #68515, #49556, #10856, #3716, #4122, #56284, #17189, #55861, #23473, #43637, #54629, #49965, #75663, #69340, #16773, #74011, #36516, #67697, #36931, #18003, #11691, #37348, #62192, #4529, #74426, #55448, #42003, #80342, #42411, #23890, #68108, #22655, #30199, #48314, #62609, #75250, #10456, #10033, #81157, #17594, #49140, #61364, #30619, #29380, #80747, #43226, #23061, #74845, #5359, #69748, #25112, #45299, #70995, #26369, #24705, #50784, #38164, #44056, #13338, #290, #12094, #45716, #38992, #18413, #12503, #64675, #32682, #56688, #51191, #82387, #76889, #31432, #7014, #44459, #37752, #63427, #19219, #38581, #5763, #82790, #57095, #52027, #58349, #50373, #76485, #20064, #63838, #710, #77733, #18812, #64260, #70150, #76071, #6176, #25946, #31851, #57926, #44869, #57513, #83204, #63021, #51604, #31020, #71413, #25526, #13760, #70568, #12922, #77309, #6594, #32266, #19639, #9112, #78996, #53285, #34784, #65530, #33109, #66778, #46555, #41089, #72663, #60027, #15429, #20485, #59605, #2795, #39841, #72253, #15012, #78154, #53697, #60443, #14602, #14183, #39417, #20902, #21725, #59190, #46139, #34361, #28454, #79406, #40668, #21316, #52866, #7863, #33941, #78576, #66353, #73079, #46969, #40256, #58777, #65939, #47388, #8275, #22146, #54114, #33527, #79829, #8691, #2382, #1549, #65101, #71834, #27203, #47804, #73507, #7438, #1137, #1960, #27622, #28039, #26787, #52444, #22563, #81890, #49465, #54531, #48635, #75159, #68833, #9520, #4031, #35192, #29696, #67601, #23793, #80657, #73920, #80247, #55358, #74746, #16261, #35604, #41907, #4850, #11179, #3207, #61266, #56188, #74330, #43136, #62512, #9932, #17095, #3620, #60853, #48224, #62099, #16677, #10766, #81064, #28869, #42316, #15855, #36426, #67189, #30525, #41504, #49872, #36839, #10359, #4441, #29287, #24201, #36019, #54950, #23380, #49048, #22969, #68015, #61691, #42730, #68426, #17504, #30107, #55769, #81476, #56595, #12410, #38900, #75979, #25018, #25431, #30928, #6502, #45199, #50691, #50281, #75572, #57003, #57828, #12001, #82295, #70471, #70901, #32172, #51097, #57419, #5670, #18319, #70056, #31337, #76794, #83112, #6083, #37655, #76389, #62931, #6917, #82699, #12828, #18722, #17912, #19125, #26272, #38485, #44774, #69657, #37255, #5264, #44364, #38068, #616, #64579, #43548, #64169, #63744, #24614, #31757, #32588, #63333, #196, #25848, #51508, #58251, #77212, #19541, #13251, #43961, #69248, #11595, #28259, #42127, #34166, #60253 ) ),
 .UNSPECIFIED., .F., .F., .F. ) 
 B_SPLINE_SURFACE_WITH_KNOTS ( ( 2, 2 ),
 ( 3, 2, 2, 2, 2, 2, 2, 2, 2, 2, 2, 2, 2, 2, 2, 2, 2, 2, 2, 2, 2, 2, 2, 2, 2, 2, 2, 2, 2, 2, 2, 2, 2, 2, 2, 2, 2, 2, 2, 2, 2, 2, 2, 2, 2, 2, 2, 2, 2, 2, 2, 2, 2, 2, 2, 2, 2, 2, 2, 2, 2, 2, 2, 2, 2, 2, 2, 2, 2, 2, 2, 2, 2, 2, 2, 2, 2, 2, 2, 2, 2, 2, 2, 2, 2, 2, 2, 2, 2, 2, 2, 2, 2, 2, 2, 2, 2, 2, 2, 2, 2, 2, 2, 2, 2, 2, 2, 2, 2, 2, 2, 2, 2, 2, 2, 2, 2, 2, 2, 2, 2, 2, 2, 2, 2, 2, 2, 2, 2, 2, 2, 2, 2, 2, 2, 2, 2, 2, 2, 2, 2, 2, 2, 2, 2, 2, 2, 2, 2, 2, 2, 2, 2, 2, 2, 2, 2, 2, 2, 2, 2, 2, 2, 2, 2, 2, 2, 2, 2, 2, 2, 2, 2, 2, 2, 2, 2, 2, 2, 2, 2, 2, 2, 2, 2, 2, 2, 2, 2, 2, 2, 2, 2, 2, 2, 2, 2, 2, 2, 2, 2, 2, 2, 2, 2, 2, 2, 2, 2, 2, 2, 2, 2, 2, 2, 2, 2, 2, 2, 2, 2, 2, 2, 2, 2, 2, 2, 2, 2, 2, 2, 2, 2, 2, 2, 2, 2, 3 ),
 ( 0.000000000000000000, 1.000000000000000000 ),
 ( 0.000000000000000000, 0.004166666666666666609, 0.008333333333333333218, 0.01250000000000000069, 0.01666666666666666644, 0.02083333333333333218, 0.02500000000000000139, 0.02916666666666666713, 0.03333333333333333287, 0.03749999999999999861, 0.04166666666666666435, 0.04583333333333333010, 0.05000000000000000278, 0.05416666666666666852, 0.05833333333333333426, 0.06250000000000000000, 0.06666666666666666574, 0.07083333333333333148, 0.07499999999999999722, 0.07916666666666666297, 0.08333333333333332871, 0.08749999999999999445, 0.09166666666666666019, 0.09583333333333333981, 0.1000000000000000056, 0.1041666666666666713, 0.1083333333333333370, 0.1125000000000000028, 0.1166666666666666685, 0.1208333333333333343, 0.1250000000000000000, 0.1291666666666666796, 0.1333333333333333315, 0.1375000000000000111, 0.1416666666666666630, 0.1458333333333333426, 0.1499999999999999944, 0.1541666666666666741, 0.1583333333333333259, 0.1625000000000000056, 0.1666666666666666574, 0.1708333333333333370, 0.1749999999999999889, 0.1791666666666666685, 0.1833333333333333204, 0.1875000000000000000, 0.1916666666666666796, 0.1958333333333333315, 0.2000000000000000111, 0.2041666666666666630, 0.2083333333333333426, 0.2124999999999999944, 0.2166666666666666741, 0.2208333333333333259, 0.2250000000000000056, 0.2291666666666666574, 0.2333333333333333370, 0.2374999999999999889, 0.2416666666666666685, 0.2458333333333333204, 0.2500000000000000000, 0.2541666666666666519, 0.2583333333333333592, 0.2625000000000000111, 0.2666666666666666630, 0.2708333333333333148, 0.2750000000000000222, 0.2791666666666666741, 0.2833333333333333259, 0.2874999999999999778, 0.2916666666666666852, 0.2958333333333333370, 0.2999999999999999889, 0.3041666666666666408, 0.3083333333333333481, 0.3125000000000000000, 0.3166666666666666519, 0.3208333333333333592, 0.3250000000000000111, 0.3291666666666666630, 0.3333333333333333148, 0.3375000000000000222, 0.3416666666666666741, 0.3458333333333333259, 0.3499999999999999778, 0.3541666666666666852, 0.3583333333333333370, 0.3624999999999999889, 0.3666666666666666408, 0.3708333333333333481, 0.3750000000000000000, 0.3791666666666666519, 0.3833333333333333592, 0.3875000000000000111, 0.3916666666666666630, 0.3958333333333333148, 0.4000000000000000222, 0.4041666666666666741, 0.4083333333333333259, 0.4124999999999999778, 0.4166666666666666852, 0.4208333333333333370, 0.4249999999999999889, 0.4291666666666666408, 0.4333333333333333481, 0.4375000000000000000, 0.4416666666666666519, 0.4458333333333333592, 0.4500000000000000111, 0.4541666666666666630, 0.4583333333333333148, 0.4625000000000000222, 0.4666666666666666741, 0.4708333333333333259, 0.4749999999999999778, 0.4791666666666666852, 0.4833333333333333370, 0.4874999999999999889, 0.4916666666666666408, 0.4958333333333333481, 0.5000000000000000000, 0.5041666666666666519, 0.5083333333333333037, 0.5124999999999999556, 0.5166666666666667185, 0.5208333333333333703, 0.5250000000000000222, 0.5291666666666666741, 0.5333333333333333259, 0.5374999999999999778, 0.5416666666666666297, 0.5458333333333332815, 0.5500000000000000444, 0.5541666666666666963, 0.5583333333333333481, 0.5625000000000000000, 0.5666666666666666519, 0.5708333333333333037, 0.5749999999999999556, 0.5791666666666667185, 0.5833333333333333703, 0.5875000000000000222, 0.5916666666666666741, 0.5958333333333333259, 0.5999999999999999778, 0.6041666666666666297, 0.6083333333333332815, 0.6125000000000000444, 0.6166666666666666963, 0.6208333333333333481, 0.6250000000000000000, 0.6291666666666666519, 0.6333333333333333037, 0.6374999999999999556, 0.6416666666666667185, 0.6458333333333333703, 0.6500000000000000222, 0.6541666666666666741, 0.6583333333333333259, 0.6624999999999999778, 0.6666666666666666297, 0.6708333333333332815, 0.6750000000000000444, 0.6791666666666666963, 0.6833333333333333481, 0.6875000000000000000, 0.6916666666666666519, 0.6958333333333333037, 0.6999999999999999556, 0.7041666666666667185, 0.7083333333333333703, 0.7125000000000000222, 0.7166666666666666741, 0.7208333333333333259, 0.7249999999999999778, 0.7291666666666666297, 0.7333333333333332815, 0.7375000000000000444, 0.7416666666666666963, 0.7458333333333333481, 0.7500000000000000000, 0.7541666666666666519, 0.7583333333333333037, 0.7624999999999999556, 0.7666666666666667185, 0.7708333333333333703, 0.7750000000000000222, 0.7791666666666666741, 0.7833333333333333259, 0.7874999999999999778, 0.7916666666666666297, 0.7958333333333332815, 0.8000000000000000444, 0.8041666666666666963, 0.8083333333333333481, 0.8125000000000000000, 0.8166666666666666519, 0.8208333333333333037, 0.8249999999999999556, 0.8291666666666667185, 0.8333333333333333703, 0.8375000000000000222, 0.8416666666666666741, 0.8458333333333333259, 0.8499999999999999778, 0.8541666666666666297, 0.8583333333333332815, 0.8625000000000000444, 0.8666666666666666963, 0.8708333333333333481, 0.8750000000000000000, 0.8791666666666666519, 0.8833333333333333037, 0.8874999999999999556, 0.8916666666666667185, 0.8958333333333333703, 0.9000000000000000222, 0.9041666666666666741, 0.9083333333333333259, 0.9124999999999999778, 0.9166666666666666297, 0.9208333333333332815, 0.9250000000000000444, 0.9291666666666666963, 0.9333333333333333481, 0.9375000000000000000, 0.9416666666666666519, 0.9458333333333333037, 0.9499999999999999556, 0.9541666666666667185, 0.9583333333333333703, 0.9625000000000000222, 0.9666666666666666741, 0.9708333333333333259, 0.9749999999999999778, 0.9791666666666666297, 0.9833333333333332815, 0.9875000000000000444 ),
 .UNSPECIFIED. ) 
 GEOMETRIC_REPRESENTATION_ITEM ( )  RATIONAL_B_SPLINE_SURFACE ( (
 ( 1.000000000000000000, 0.9659258262890683122, 1.000000000000000000, 0.9659258262890683122, 1.000000000000000000, 0.9659258262890683122, 1.000000000000000000, 0.9659258262890683122, 1.000000000000000000, 0.9659258262890683122, 1.000000000000000000, 0.9659258262890683122, 1.000000000000000000, 0.9659258262890683122, 1.000000000000000000, 0.9659258262890683122, 1.000000000000000000, 0.9659258262890683122, 1.000000000000000000, 0.9659258262890683122, 1.000000000000000000, 0.9659258262890683122, 1.000000000000000000, 0.9659258262890683122, 1.000000000000000000, 0.9659258262890683122, 1.000000000000000000, 0.9659258262890683122, 1.000000000000000000, 0.9659258262890683122, 1.000000000000000000, 0.9659258262890683122, 1.000000000000000000, 0.9659258262890683122, 1.000000000000000000, 0.9659258262890683122, 1.000000000000000000, 0.9659258262890683122, 1.000000000000000000, 0.9659258262890683122, 1.000000000000000000, 0.9659258262890683122, 1.000000000000000000, 0.9659258262890683122, 1.000000000000000000, 0.9659258262890683122, 1.000000000000000000, 0.9659258262890683122, 1.000000000000000000, 0.9659258262890683122, 1.000000000000000000, 0.9659258262890683122, 1.000000000000000000, 0.9659258262890683122, 1.000000000000000000, 0.9659258262890683122, 1.000000000000000000, 0.9659258262890683122, 1.000000000000000000, 0.9659258262890683122, 1.000000000000000000, 0.9659258262890683122, 1.000000000000000000, 0.9659258262890683122, 1.000000000000000000, 0.9659258262890683122, 1.000000000000000000, 0.9659258262890683122, 1.000000000000000000, 0.9659258262890683122, 1.000000000000000000, 0.9659258262890683122, 1.000000000000000000, 0.9659258262890683122, 1.000000000000000000, 0.9659258262890683122, 1.000000000000000000, 0.9659258262890683122, 1.000000000000000000, 0.9659258262890683122, 1.000000000000000000, 0.9659258262890683122, 1.000000000000000000, 0.9659258262890683122, 1.000000000000000000, 0.9659258262890683122, 1.000000000000000000, 0.9659258262890683122, 1.000000000000000000, 0.9659258262890683122, 1.000000000000000000, 0.9659258262890683122, 1.000000000000000000, 0.9659258262890683122, 1.000000000000000000, 0.9659258262890683122, 1.000000000000000000, 0.9659258262890683122, 1.000000000000000000, 0.9659258262890683122, 1.000000000000000000, 0.9659258262890683122, 1.000000000000000000, 0.9659258262890683122, 1.000000000000000000, 0.9659258262890683122, 1.000000000000000000, 0.9659258262890683122, 1.000000000000000000, 0.9659258262890683122, 1.000000000000000000, 0.9659258262890683122, 1.000000000000000000, 0.9659258262890683122, 1.000000000000000000, 0.9659258262890683122, 1.000000000000000000, 0.9659258262890683122, 1.000000000000000000, 0.9659258262890683122, 1.000000000000000000, 0.9659258262890683122, 1.000000000000000000, 0.9659258262890683122, 1.000000000000000000, 0.9659258262890683122, 1.000000000000000000, 0.9659258262890683122, 1.000000000000000000, 0.9659258262890683122, 1.000000000000000000, 0.9659258262890683122, 1.000000000000000000, 0.9659258262890683122, 1.000000000000000000, 0.9659258262890683122, 1.000000000000000000, 0.9659258262890683122, 1.000000000000000000, 0.9659258262890683122, 1.000000000000000000, 0.9659258262890683122, 1.000000000000000000, 0.9659258262890683122, 1.000000000000000000, 0.9659258262890683122, 1.000000000000000000, 0.9659258262890683122, 1.000000000000000000, 0.9659258262890683122, 1.000000000000000000, 0.9659258262890683122, 1.000000000000000000, 0.9659258262890683122, 1.000000000000000000, 0.9659258262890683122, 1.000000000000000000, 0.9659258262890683122, 1.000000000000000000, 0.9659258262890683122, 1.000000000000000000, 0.9659258262890683122, 1.000000000000000000, 0.9659258262890683122, 1.000000000000000000, 0.9659258262890683122, 1.000000000000000000, 0.9659258262890683122, 1.000000000000000000, 0.9659258262890683122, 1.000000000000000000, 0.9659258262890683122, 1.000000000000000000, 0.9659258262890683122, 1.000000000000000000, 0.9659258262890683122, 1.000000000000000000, 0.9659258262890683122, 1.000000000000000000, 0.9659258262890683122, 1.000000000000000000, 0.9659258262890683122, 1.000000000000000000, 0.9659258262890683122, 1.000000000000000000, 0.9659258262890683122, 1.000000000000000000, 0.9659258262890683122, 1.000000000000000000, 0.9659258262890683122, 1.000000000000000000, 0.9659258262890683122, 1.000000000000000000, 0.9659258262890683122, 1.000000000000000000, 0.9659258262890683122, 1.000000000000000000, 0.9659258262890683122, 1.000000000000000000, 0.9659258262890683122, 1.000000000000000000, 0.9659258262890683122, 1.000000000000000000, 0.9659258262890683122, 1.000000000000000000, 0.9659258262890683122, 1.000000000000000000, 0.9659258262890683122, 1.000000000000000000, 0.9659258262890683122, 1.000000000000000000, 0.9659258262890683122, 1.000000000000000000, 0.9659258262890683122, 1.000000000000000000, 0.9659258262890683122, 1.000000000000000000, 0.9659258262890683122, 1.000000000000000000, 0.9659258262890683122, 1.000000000000000000, 0.9659258262890683122, 1.000000000000000000, 0.9659258262890683122, 1.000000000000000000, 0.9659258262890683122, 1.000000000000000000, 0.9659258262890683122, 1.000000000000000000, 0.9659258262890683122, 1.000000000000000000, 0.9659258262890683122, 1.000000000000000000, 0.9659258262890683122, 1.000000000000000000, 0.9659258262890683122, 1.000000000000000000, 0.9659258262890683122, 1.000000000000000000, 0.9659258262890683122, 1.000000000000000000, 0.9659258262890683122, 1.000000000000000000, 0.9659258262890683122, 1.000000000000000000, 0.9659258262890683122, 1.000000000000000000, 0.9659258262890683122, 1.000000000000000000, 0.9659258262890683122, 1.000000000000000000, 0.9659258262890683122, 1.000000000000000000, 0.9659258262890683122, 1.000000000000000000, 0.9659258262890683122, 1.000000000000000000, 0.9659258262890683122, 1.000000000000000000, 0.9659258262890683122, 1.000000000000000000, 0.9659258262890683122, 1.000000000000000000, 0.9659258262890683122, 1.000000000000000000, 0.9659258262890683122, 1.000000000000000000, 0.9659258262890683122, 1.000000000000000000, 0.9659258262890683122, 1.000000000000000000, 0.9659258262890683122, 1.000000000000000000, 0.9659258262890683122, 1.000000000000000000, 0.9659258262890683122, 1.000000000000000000, 0.9659258262890683122, 1.000000000000000000, 0.9659258262890683122, 1.000000000000000000, 0.9659258262890683122, 1.000000000000000000, 0.9659258262890683122, 1.000000000000000000, 0.9659258262890683122, 1.000000000000000000, 0.9659258262890683122, 1.000000000000000000, 0.9659258262890683122, 1.000000000000000000, 0.9659258262890683122, 1.000000000000000000, 0.9659258262890683122, 1.000000000000000000, 0.9659258262890683122, 1.000000000000000000, 0.9659258262890683122, 1.000000000000000000, 0.9659258262890683122, 1.000000000000000000, 0.9659258262890683122, 1.000000000000000000, 0.9659258262890683122, 1.000000000000000000, 0.9659258262890683122, 1.000000000000000000, 0.9659258262890683122, 1.000000000000000000, 0.9659258262890683122, 1.000000000000000000, 0.9659258262890683122, 1.000000000000000000, 0.9659258262890683122, 1.000000000000000000, 0.9659258262890683122, 1.000000000000000000, 0.9659258262890683122, 1.000000000000000000, 0.9659258262890683122, 1.000000000000000000, 0.9659258262890683122, 1.000000000000000000, 0.9659258262890683122, 1.000000000000000000, 0.9659258262890683122, 1.000000000000000000, 0.9659258262890683122, 1.000000000000000000, 0.9659258262890683122, 1.000000000000000000, 0.9659258262890683122, 1.000000000000000000, 0.9659258262890683122, 1.000000000000000000, 0.9659258262890683122, 1.000000000000000000, 0.9659258262890683122, 1.000000000000000000, 0.9659258262890683122, 1.000000000000000000, 0.9659258262890683122, 1.000000000000000000, 0.9659258262890683122, 1.000000000000000000, 0.9659258262890683122, 1.000000000000000000, 0.9659258262890683122, 1.000000000000000000, 0.9659258262890683122, 1.000000000000000000, 0.9659258262890683122, 1.000000000000000000, 0.9659258262890683122, 1.000000000000000000, 0.9659258262890683122, 1.000000000000000000, 0.9659258262890683122, 1.000000000000000000, 0.9659258262890683122, 1.000000000000000000, 0.9659258262890683122, 1.000000000000000000, 0.9659258262890683122, 1.000000000000000000, 0.9659258262890683122, 1.000000000000000000, 0.9659258262890683122, 1.000000000000000000, 0.9659258262890683122, 1.000000000000000000, 0.9659258262890683122, 1.000000000000000000, 0.9659258262890683122, 1.000000000000000000, 0.9659258262890683122, 1.000000000000000000, 0.9659258262890683122, 1.000000000000000000, 0.9659258262890683122, 1.000000000000000000, 0.9659258262890683122, 1.000000000000000000, 0.9659258262890683122, 1.000000000000000000, 0.9659258262890683122, 1.000000000000000000, 0.9659258262890683122, 1.000000000000000000, 0.9659258262890683122, 1.000000000000000000, 0.9659258262890683122, 1.000000000000000000, 0.9659258262890683122, 1.000000000000000000, 0.9659258262890683122, 1.000000000000000000, 0.9659258262890683122, 1.000000000000000000, 0.9659258262890683122, 1.000000000000000000, 0.9659258262890683122, 1.000000000000000000, 0.9659258262890683122, 1.000000000000000000, 0.9659258262890683122, 1.000000000000000000, 0.9659258262890683122, 1.000000000000000000, 0.9659258262890683122, 1.000000000000000000, 0.9659258262890683122, 1.000000000000000000, 0.9659258262890683122, 1.000000000000000000, 0.9659258262890683122, 1.000000000000000000, 0.9659258262890683122, 1.000000000000000000, 0.9659258262890683122, 1.000000000000000000, 0.9659258262890683122, 1.000000000000000000, 0.9659258262890683122, 1.000000000000000000, 0.9659258262890683122, 1.000000000000000000, 0.9659258262890683122, 1.000000000000000000, 0.9659258262890683122, 1.000000000000000000, 0.9659258262890683122, 1.000000000000000000, 0.9659258262890683122, 1.000000000000000000, 0.9659258262890683122, 1.000000000000000000, 0.9659258262890683122, 1.000000000000000000, 0.9659258262890683122, 1.000000000000000000, 0.9659258262890683122, 1.000000000000000000, 0.9659258262890683122, 1.000000000000000000, 0.9659258262890683122, 1.000000000000000000, 0.9659258262890683122, 1.000000000000000000, 0.9659258262890683122, 1.000000000000000000, 0.9659258262890683122, 1.000000000000000000, 0.9659258262890683122, 1.000000000000000000, 0.9659258262890683122, 1.000000000000000000, 0.9659258262890683122, 1.000000000000000000, 0.9659258262890683122, 1.000000000000000000, 0.9659258262890683122, 1.000000000000000000, 0.9659258262890683122, 1.000000000000000000, 0.9659258262890683122, 1.000000000000000000, 0.9659258262890683122, 1.000000000000000000, 0.9659258262890683122, 1.000000000000000000, 0.9659258262890683122, 1.000000000000000000, 0.9659258262890683122, 1.000000000000000000),
 ( 1.000000000000000000, 0.9659258262890683122, 1.000000000000000000, 0.9659258262890683122, 1.000000000000000000, 0.9659258262890683122, 1.000000000000000000, 0.9659258262890683122, 1.000000000000000000, 0.9659258262890683122, 1.000000000000000000, 0.9659258262890683122, 1.000000000000000000, 0.9659258262890683122, 1.000000000000000000, 0.9659258262890683122, 1.000000000000000000, 0.9659258262890683122, 1.000000000000000000, 0.9659258262890683122, 1.000000000000000000, 0.9659258262890683122, 1.000000000000000000, 0.9659258262890683122, 1.000000000000000000, 0.9659258262890683122, 1.000000000000000000, 0.9659258262890683122, 1.000000000000000000, 0.9659258262890683122, 1.000000000000000000, 0.9659258262890683122, 1.000000000000000000, 0.9659258262890683122, 1.000000000000000000, 0.9659258262890683122, 1.000000000000000000, 0.9659258262890683122, 1.000000000000000000, 0.9659258262890683122, 1.000000000000000000, 0.9659258262890683122, 1.000000000000000000, 0.9659258262890683122, 1.000000000000000000, 0.9659258262890683122, 1.000000000000000000, 0.9659258262890683122, 1.000000000000000000, 0.9659258262890683122, 1.000000000000000000, 0.9659258262890683122, 1.000000000000000000, 0.9659258262890683122, 1.000000000000000000, 0.9659258262890683122, 1.000000000000000000, 0.9659258262890683122, 1.000000000000000000, 0.9659258262890683122, 1.000000000000000000, 0.9659258262890683122, 1.000000000000000000, 0.9659258262890683122, 1.000000000000000000, 0.9659258262890683122, 1.000000000000000000, 0.9659258262890683122, 1.000000000000000000, 0.9659258262890683122, 1.000000000000000000, 0.9659258262890683122, 1.000000000000000000, 0.9659258262890683122, 1.000000000000000000, 0.9659258262890683122, 1.000000000000000000, 0.9659258262890683122, 1.000000000000000000, 0.9659258262890683122, 1.000000000000000000, 0.9659258262890683122, 1.000000000000000000, 0.9659258262890683122, 1.000000000000000000, 0.9659258262890683122, 1.000000000000000000, 0.9659258262890683122, 1.000000000000000000, 0.9659258262890683122, 1.000000000000000000, 0.9659258262890683122, 1.000000000000000000, 0.9659258262890683122, 1.000000000000000000, 0.9659258262890683122, 1.000000000000000000, 0.9659258262890683122, 1.000000000000000000, 0.9659258262890683122, 1.000000000000000000, 0.9659258262890683122, 1.000000000000000000, 0.9659258262890683122, 1.000000000000000000, 0.9659258262890683122, 1.000000000000000000, 0.9659258262890683122, 1.000000000000000000, 0.9659258262890683122, 1.000000000000000000, 0.9659258262890683122, 1.000000000000000000, 0.9659258262890683122, 1.000000000000000000, 0.9659258262890683122, 1.000000000000000000, 0.9659258262890683122, 1.000000000000000000, 0.9659258262890683122, 1.000000000000000000, 0.9659258262890683122, 1.000000000000000000, 0.9659258262890683122, 1.000000000000000000, 0.9659258262890683122, 1.000000000000000000, 0.9659258262890683122, 1.000000000000000000, 0.9659258262890683122, 1.000000000000000000, 0.9659258262890683122, 1.000000000000000000, 0.9659258262890683122, 1.000000000000000000, 0.9659258262890683122, 1.000000000000000000, 0.9659258262890683122, 1.000000000000000000, 0.9659258262890683122, 1.000000000000000000, 0.9659258262890683122, 1.000000000000000000, 0.9659258262890683122, 1.000000000000000000, 0.9659258262890683122, 1.000000000000000000, 0.9659258262890683122, 1.000000000000000000, 0.9659258262890683122, 1.000000000000000000, 0.9659258262890683122, 1.000000000000000000, 0.9659258262890683122, 1.000000000000000000, 0.9659258262890683122, 1.000000000000000000, 0.9659258262890683122, 1.000000000000000000, 0.9659258262890683122, 1.000000000000000000, 0.9659258262890683122, 1.000000000000000000, 0.9659258262890683122, 1.000000000000000000, 0.9659258262890683122, 1.000000000000000000, 0.9659258262890683122, 1.000000000000000000, 0.9659258262890683122, 1.000000000000000000, 0.9659258262890683122, 1.000000000000000000, 0.9659258262890683122, 1.000000000000000000, 0.9659258262890683122, 1.000000000000000000, 0.9659258262890683122, 1.000000000000000000, 0.9659258262890683122, 1.000000000000000000, 0.9659258262890683122, 1.000000000000000000, 0.9659258262890683122, 1.000000000000000000, 0.9659258262890683122, 1.000000000000000000, 0.9659258262890683122, 1.000000000000000000, 0.9659258262890683122, 1.000000000000000000, 0.9659258262890683122, 1.000000000000000000, 0.9659258262890683122, 1.000000000000000000, 0.9659258262890683122, 1.000000000000000000, 0.9659258262890683122, 1.000000000000000000, 0.9659258262890683122, 1.000000000000000000, 0.9659258262890683122, 1.000000000000000000, 0.9659258262890683122, 1.000000000000000000, 0.9659258262890683122, 1.000000000000000000, 0.9659258262890683122, 1.000000000000000000, 0.9659258262890683122, 1.000000000000000000, 0.9659258262890683122, 1.000000000000000000, 0.9659258262890683122, 1.000000000000000000, 0.9659258262890683122, 1.000000000000000000, 0.9659258262890683122, 1.000000000000000000, 0.9659258262890683122, 1.000000000000000000, 0.9659258262890683122, 1.000000000000000000, 0.9659258262890683122, 1.000000000000000000, 0.9659258262890683122, 1.000000000000000000, 0.9659258262890683122, 1.000000000000000000, 0.9659258262890683122, 1.000000000000000000, 0.9659258262890683122, 1.000000000000000000, 0.9659258262890683122, 1.000000000000000000, 0.9659258262890683122, 1.000000000000000000, 0.9659258262890683122, 1.000000000000000000, 0.9659258262890683122, 1.000000000000000000, 0.9659258262890683122, 1.000000000000000000, 0.9659258262890683122, 1.000000000000000000, 0.9659258262890683122, 1.000000000000000000, 0.9659258262890683122, 1.000000000000000000, 0.9659258262890683122, 1.000000000000000000, 0.9659258262890683122, 1.000000000000000000, 0.9659258262890683122, 1.000000000000000000, 0.9659258262890683122, 1.000000000000000000, 0.9659258262890683122, 1.000000000000000000, 0.9659258262890683122, 1.000000000000000000, 0.9659258262890683122, 1.000000000000000000, 0.9659258262890683122, 1.000000000000000000, 0.9659258262890683122, 1.000000000000000000, 0.9659258262890683122, 1.000000000000000000, 0.9659258262890683122, 1.000000000000000000, 0.9659258262890683122, 1.000000000000000000, 0.9659258262890683122, 1.000000000000000000, 0.9659258262890683122, 1.000000000000000000, 0.9659258262890683122, 1.000000000000000000, 0.9659258262890683122, 1.000000000000000000, 0.9659258262890683122, 1.000000000000000000, 0.9659258262890683122, 1.000000000000000000, 0.9659258262890683122, 1.000000000000000000, 0.9659258262890683122, 1.000000000000000000, 0.9659258262890683122, 1.000000000000000000, 0.9659258262890683122, 1.000000000000000000, 0.9659258262890683122, 1.000000000000000000, 0.9659258262890683122, 1.000000000000000000, 0.9659258262890683122, 1.000000000000000000, 0.9659258262890683122, 1.000000000000000000, 0.9659258262890683122, 1.000000000000000000, 0.9659258262890683122, 1.000000000000000000, 0.9659258262890683122, 1.000000000000000000, 0.9659258262890683122, 1.000000000000000000, 0.9659258262890683122, 1.000000000000000000, 0.9659258262890683122, 1.000000000000000000, 0.9659258262890683122, 1.000000000000000000, 0.9659258262890683122, 1.000000000000000000, 0.9659258262890683122, 1.000000000000000000, 0.9659258262890683122, 1.000000000000000000, 0.9659258262890683122, 1.000000000000000000, 0.9659258262890683122, 1.000000000000000000, 0.9659258262890683122, 1.000000000000000000, 0.9659258262890683122, 1.000000000000000000, 0.9659258262890683122, 1.000000000000000000, 0.9659258262890683122, 1.000000000000000000, 0.9659258262890683122, 1.000000000000000000, 0.9659258262890683122, 1.000000000000000000, 0.9659258262890683122, 1.000000000000000000, 0.9659258262890683122, 1.000000000000000000, 0.9659258262890683122, 1.000000000000000000, 0.9659258262890683122, 1.000000000000000000, 0.9659258262890683122, 1.000000000000000000, 0.9659258262890683122, 1.000000000000000000, 0.9659258262890683122, 1.000000000000000000, 0.9659258262890683122, 1.000000000000000000, 0.9659258262890683122, 1.000000000000000000, 0.9659258262890683122, 1.000000000000000000, 0.9659258262890683122, 1.000000000000000000, 0.9659258262890683122, 1.000000000000000000, 0.9659258262890683122, 1.000000000000000000, 0.9659258262890683122, 1.000000000000000000, 0.9659258262890683122, 1.000000000000000000, 0.9659258262890683122, 1.000000000000000000, 0.9659258262890683122, 1.000000000000000000, 0.9659258262890683122, 1.000000000000000000, 0.9659258262890683122, 1.000000000000000000, 0.9659258262890683122, 1.000000000000000000, 0.9659258262890683122, 1.000000000000000000, 0.9659258262890683122, 1.000000000000000000, 0.9659258262890683122, 1.000000000000000000, 0.9659258262890683122, 1.000000000000000000, 0.9659258262890683122, 1.000000000000000000, 0.9659258262890683122, 1.000000000000000000, 0.9659258262890683122, 1.000000000000000000, 0.9659258262890683122, 1.000000000000000000, 0.9659258262890683122, 1.000000000000000000, 0.9659258262890683122, 1.000000000000000000, 0.9659258262890683122, 1.000000000000000000, 0.9659258262890683122, 1.000000000000000000, 0.9659258262890683122, 1.000000000000000000, 0.9659258262890683122, 1.000000000000000000, 0.9659258262890683122, 1.000000000000000000, 0.9659258262890683122, 1.000000000000000000, 0.9659258262890683122, 1.000000000000000000, 0.9659258262890683122, 1.000000000000000000, 0.9659258262890683122, 1.000000000000000000, 0.9659258262890683122, 1.000000000000000000, 0.9659258262890683122, 1.000000000000000000, 0.9659258262890683122, 1.000000000000000000, 0.9659258262890683122, 1.000000000000000000, 0.9659258262890683122, 1.000000000000000000, 0.9659258262890683122, 1.000000000000000000, 0.9659258262890683122, 1.000000000000000000, 0.9659258262890683122, 1.000000000000000000, 0.9659258262890683122, 1.000000000000000000, 0.9659258262890683122, 1.000000000000000000, 0.9659258262890683122, 1.000000000000000000, 0.9659258262890683122, 1.000000000000000000, 0.9659258262890683122, 1.000000000000000000, 0.9659258262890683122, 1.000000000000000000, 0.9659258262890683122, 1.000000000000000000, 0.9659258262890683122, 1.000000000000000000, 0.9659258262890683122, 1.000000000000000000, 0.9659258262890683122, 1.000000000000000000, 0.9659258262890683122, 1.000000000000000000, 0.9659258262890683122, 1.000000000000000000, 0.9659258262890683122, 1.000000000000000000, 0.9659258262890683122, 1.000000000000000000, 0.9659258262890683122, 1.000000000000000000, 0.9659258262890683122, 1.000000000000000000, 0.9659258262890683122, 1.000000000000000000, 0.9659258262890683122, 1.000000000000000000, 0.9659258262890683122, 1.000000000000000000, 0.9659258262890683122, 1.000000000000000000, 0.9659258262890683122, 1.000000000000000000, 0.9659258262890683122, 1.000000000000000000) ) ) 
 REPRESENTATION_ITEM ( '' )  SURFACE ( )  );
#17720 = CARTESIAN_POINT ( 'NONE',  ( -0.2867679344610365999, 0.2867679344610364889, -1.521653543307086354 ) ) ;
#17721 = B_SPLINE_CURVE_WITH_KNOTS ( 'NONE', 3,
 ( #15885, #14220, #33977, #39880 ),
 .UNSPECIFIED., .F., .F.,
 ( 4, 4 ),
 ( 9.959548797825900302E-07, 0.001423907596959053667 ),
 .UNSPECIFIED. ) ;
#17722 = CARTESIAN_POINT ( 'NONE',  ( -1.601049868766403650, 0.1283753931104746893, -0.1820866141732285504 ) ) ;
#17723 = CARTESIAN_POINT ( 'NONE',  ( 0.6824146981627303710, -0.5023911411419708095, 0.1820866141732285504 ) ) ;
#17724 = CARTESIAN_POINT ( 'NONE',  ( 0.8727034120734912248, -0.3162353388693409650, -0.4822834645669289433 ) ) ;
#17725 = CARTESIAN_POINT ( 'NONE',  ( 0.3458507752293908943, 0.3458507752293908943, -1.159448818897637734 ) ) ;
#17726 = CARTESIAN_POINT ( 'NONE',  ( 0.8989501312335964611, 0.1771653543307087630, 0.09757992244046791164 ) ) ;
#17727 = CARTESIAN_POINT ( 'NONE',  ( 0.4593175853018379162, -0.4281496062992124485, 0.4176697321401328655 ) ) ;
#17728 = CARTESIAN_POINT ( 'NONE',  ( -0.2891555358219911054, 0.2891555358219909388, -0.8838582677165351953 ) ) ;
#17729 = CARTESIAN_POINT ( 'NONE',  ( -0.9514435695538050464, -0.3162353388693405765, 0.4822834645669290543 ) ) ;
#17730 = PLANE ( 'NONE',  #49890 ) ;
#17731 = CARTESIAN_POINT ( 'NONE',  ( 0.9383202099737536495, -0.2845877964562159024, 0.3641732283464567677 ) ) ;
#17732 = CARTESIAN_POINT ( 'NONE',  ( -0.1312335958005241554, 0.2306618581243848609, 0.2411417322834645549 ) ) ;
#17733 = FACE_OUTER_BOUND ( 'NONE', #71756, .T. ) ;
#17734 = CARTESIAN_POINT ( 'NONE',  ( -0.3215223097112853146, -0.3162353388693405765, 0.4822834645669290543 ) ) ;
#17735 = CARTESIAN_POINT ( 'NONE',  ( -0.05249343832020911260, 0.1283753931104748280, 0.1820866141732283561 ) ) ;
#17736 = DIRECTION ( 'NONE',  ( -1.000000000000000000, -0.000000000000000000, -0.000000000000000000 ) ) ;
#17737 = CARTESIAN_POINT ( 'NONE',  ( -0.1902887139107604098, -0.6692913385826771977, 0.1292274648535927661 ) ) ;
#17738 = CARTESIAN_POINT ( 'NONE',  ( 0.8464566929133865436, 0.07958543189024071263, -0.2665933059059888421 ) ) ;
#17739 = LINE ( 'NONE', #43368, #62645 ) ;
#17740 = EDGE_CURVE ( 'NONE', #11614, #30580, #77437, .T. ) ;
#17741 = CARTESIAN_POINT ( 'NONE',  ( -0.2925321140481930149, -0.2925321140481933480, -1.553149606299212726 ) ) ;
#17742 = CARTESIAN_POINT ( 'NONE',  ( 0.5446194225721792126, -0.3162353388693405765, 0.4822834645669290543 ) ) ;
#17743 = CARTESIAN_POINT ( 'NONE',  ( -0.1049643490035307020, 0.3917322834645669549, -1.416010498687664043 ) ) ;
#17744 = CARTESIAN_POINT ( 'NONE',  ( 1.174540682414699111, -0.2845877964562159024, 0.3641732283464567677 ) ) ;
#17745 = CARTESIAN_POINT ( 'NONE',  ( 0.4827800718432856963, 2.459406111854941508E-15, 0.4281989832122449768 ) ) ;
#17746 = CARTESIAN_POINT ( 'NONE',  ( -0.5839895013123351797, 0.1771653543307087075, -0.09757992244046823083 ) ) ;
#17747 = CARTESIAN_POINT ( 'NONE',  ( -0.9055118110236215490, 0.1771653543307087630, 0.000000000000000000 ) ) ;
#17748 = CARTESIAN_POINT ( 'NONE',  ( -0.4593175853018364174, -0.4281496062992127816, -0.4176697321401328100 ) ) ;
#17749 = CARTESIAN_POINT ( 'NONE',  ( 1.056430446194226658, 0.1771653543307087630, 0.09757992244046791164 ) ) ;
#17750 = CARTESIAN_POINT ( 'NONE',  ( -1.725721784776902190, -0.08942795157527998196, 0.3641732283464567121 ) ) ;
#17751 = CARTESIAN_POINT ( 'NONE',  ( 1.614173228346457378, 0.1771653543307087630, 0.000000000000000000 ) ) ;
#17752 = CARTESIAN_POINT ( 'NONE',  ( 0.3018372703412079971, 0.05413385826771626580, -0.4176697321401330321 ) ) ;
#17753 = CARTESIAN_POINT ( 'NONE',  ( 1.161417322834646493, -0.5400638737290844871, 0.3530559997133364547 ) ) ;
#17754 = CARTESIAN_POINT ( 'NONE',  ( 0.1341320108093697061, 1.082050302230247896, -1.868011637380655232 ) ) ;
#17755 = CARTESIAN_POINT ( 'NONE',  ( 0.1181102362204730916, -0.6692913385826771977, 8.415575281601705876E-17 ) ) ;
#17756 = CARTESIAN_POINT ( 'NONE',  ( 0.1049643490035303689, 0.3917322834645670104, -1.180446194225722056 ) ) ;
#17757 = CARTESIAN_POINT ( 'NONE',  ( 0.6955380577427828781, -0.4281496062992124485, 0.4176697321401328655 ) ) ;
#17758 = CARTESIAN_POINT ( 'NONE',  ( 0.5118110236220480003, -0.6692913385826771977, 8.415575281601705876E-17 ) ) ;
#17759 = DIRECTION ( 'NONE',  ( -0.000000000000000000, -1.000000000000000000, -0.000000000000000000 ) ) ;
#17760 = CARTESIAN_POINT ( 'NONE',  ( 0.3215223097112867578, -0.2845877964562161244, -0.3641732283464567121 ) ) ;
#17761 = CARTESIAN_POINT ( 'NONE',  ( 1.253280839895013710, -0.05778040916215560624, -0.4822834645669293319 ) ) ;
#17762 = CARTESIAN_POINT ( 'NONE',  ( 0.1115485564304467270, -0.5511811023622048555, -0.09757992244046775898 ) ) ;
#17763 = CARTESIAN_POINT ( 'NONE',  ( -0.3805774278215216522, 0.05413385826771666132, 0.4176697321401328100 ) ) ;
#17764 = CARTESIAN_POINT ( 'NONE',  ( 0.1377952755905518800, -0.5400638737290844871, 0.3530559997133364547 ) ) ;
#17765 = CARTESIAN_POINT ( 'NONE',  ( -0.7742782152230962556, -0.4281496062992127816, -0.4176697321401328100 ) ) ;
#17766 = CARTESIAN_POINT ( 'NONE',  ( -0.4527559055118102749, 0.07958543189024085140, 0.2665933059059887866 ) ) ;
#17767 = CARTESIAN_POINT ( 'NONE',  ( 0.9908136482939640111, 0.2952755905511810774, -0.1292274648535930714 ) ) ;
#17768 = CARTESIAN_POINT ( 'NONE',  ( 1.010498687664042716, -0.3690944881889763329, 0.3153832671262228327 ) ) ;
#17769 = CARTESIAN_POINT ( 'NONE',  ( 0.2099737532808405305, -0.6046776061558807314, 0.2411417322834647770 ) ) ;
#17771 = CARTESIAN_POINT ( 'NONE',  ( 1.587926509186352142, 0.05413385826771666132, 0.4176697321401328100 ) ) ;
#17770 = CARTESIAN_POINT ( 'NONE',  ( -0.4724409448818898682, 5.785732909357575061E-17, -2.755905511811024056 ) ) ;
#17772 = CARTESIAN_POINT ( 'NONE',  ( 0.4177787735907000366, 1.299212598425196985, -1.382006255033530806 ) ) ;
#17773 = CARTESIAN_POINT ( 'NONE',  ( 0.2867679344610366554, 0.2867679344610366554, -2.177165354330708347 ) ) ;
#17774 = CARTESIAN_POINT ( 'NONE',  ( -1.292650918635170010, 0.2952755905511810774, -0.1292274648535930714 ) ) ;
#17775 = CARTESIAN_POINT ( 'NONE',  ( -0.7808398950131225646, -0.05778040916215522460, 0.4822834645669289988 ) ) ;
#17776 = CARTESIAN_POINT ( 'NONE',  ( 0.4724409448818897572, -0.1265901696524988906, -0.2690288713910760632 ) ) ;
#17777 = CARTESIAN_POINT ( 'NONE',  ( 0.1058382717557500713, -0.3949938075777409408, -2.762467191601050587 ) ) ;
#17778 = ORIENTED_EDGE ( 'NONE', *, *, #9570, .T. ) ;
#17779 = CARTESIAN_POINT ( 'NONE',  ( 0.2952755905511819101, 0.07958543189024071263, -0.2665933059059888421 ) ) ;
#17780 = CARTESIAN_POINT ( 'NONE',  ( 0.2867679344610365999, 0.2867679344610365999, -1.232283464566929387 ) ) ;
#17781 = CARTESIAN_POINT ( 'NONE',  ( 0.4986876640419954376, 0.2306618581243848609, 0.2411417322834645549 ) ) ;
#17782 = CARTESIAN_POINT ( 'NONE',  ( 0.4724409448818897572, -0.1265901696524988906, -2.316272965879265122 ) ) ;
#17783 = CARTESIAN_POINT ( 'NONE',  ( 0.9973753280839902091, 0.2306618581243847221, -0.2411417322834647770 ) ) ;
#17784 = DIRECTION ( 'NONE',  ( 1.000000000000000000, 0.000000000000000000, 3.455050906509825972E-15 ) ) ;
#17785 = CARTESIAN_POINT ( 'NONE',  ( 1.200787401574803681, 0.1660481256975885056, 0.3530559997133364547 ) ) ;
#17786 = CARTESIAN_POINT ( 'NONE',  ( 1.410761154855643795, -0.2845877964562159024, 0.3641732283464567677 ) ) ;
#17787 = CARTESIAN_POINT ( 'NONE',  ( 8.195543980992789655E-16, -0.1870078740157480879, -0.4822834645669291653 ) ) ;
#17788 = CARTESIAN_POINT ( 'NONE',  ( -0.1049643490035301746, -0.3917322834645670659, -0.7821329151892896236 ) ) ;
#17789 = CARTESIAN_POINT ( 'NONE',  ( -0.3083989501312330295, -0.3162353388693409650, -0.4822834645669289433 ) ) ;
#17790 = CARTESIAN_POINT ( 'NONE',  ( -0.8464566929133852113, -0.4536011799217368745, -0.2665933059059886201 ) ) ;
#17791 = CARTESIAN_POINT ( 'NONE',  ( 0.2821522309711292364, -0.6692913385826771977, 0.1292274648535927661 ) ) ;
#17792 = CARTESIAN_POINT ( 'NONE',  ( -0.5905511811023615998, 0.2952755905511811885, 0.000000000000000000 ) ) ;
#17793 = DIRECTION ( 'NONE',  ( -0.000000000000000000, -1.000000000000000000, 8.673617379884024625E-16 ) ) ;
#17794 = CARTESIAN_POINT ( 'NONE',  ( -0.5314960629921224866, 2.755905511811024056, -0.9881811337016660479 ) ) ;
#17795 = ORIENTED_EDGE ( 'NONE', *, *, #79452, .F. ) ;
#17796 = CARTESIAN_POINT ( 'NONE',  ( -0.3917322834645670104, -0.1049643490035307020, -1.932434013944568818 ) ) ;
#17797 = CARTESIAN_POINT ( 'NONE',  ( 0.4855643044619430415, -0.4281496062992127816, -0.4176697321401328100 ) ) ;
#17798 = CARTESIAN_POINT ( 'NONE',  ( -0.5052493438320203589, -0.6692913385826771977, 0.1292274648535927661 ) ) ;
#17799 = CARTESIAN_POINT ( 'NONE',  ( -1.522309711286088607, -0.6046776061558807314, 0.2411417322834647770 ) ) ;
#17800 = EDGE_CURVE ( 'NONE', #59008, #81558, #66142, .T. ) ;
#17801 = CARTESIAN_POINT ( 'NONE',  ( 0.6496062992125991586, 0.1660481256975885056, 0.3530559997133364547 ) ) ;
#17802 = CARTESIAN_POINT ( 'NONE',  ( 0.6299212598425204535, -0.1870078740157480879, -0.4822834645669291653 ) ) ;
#17803 = CARTESIAN_POINT ( 'NONE',  ( -0.1049643490035302024, -0.3917322834645671215, -1.574146981627296604 ) ) ;
#17804 = CARTESIAN_POINT ( 'NONE',  ( -0.8530183727034112984, -0.4281496062992127816, -0.4176697321401328100 ) ) ;
#17805 = CARTESIAN_POINT ( 'NONE',  ( 0.1968503937007881344, -0.6692913385826771977, 8.415575281601705876E-17 ) ) ;
#17806 = CARTESIAN_POINT ( 'NONE',  ( -0.4527559055118102749, -0.5400638737290845981, -0.3530559997133363437 ) ) ;
#17807 = EDGE_CURVE ( 'NONE', #59927, #74430, #15792, .T. ) ;
#17808 = CARTESIAN_POINT ( 'NONE',  ( 0.3543307086614181922, -0.5511811023622047445, 6.969142054262312111E-17 ) ) ;
#17809 = CARTESIAN_POINT ( 'NONE',  ( 1.660104986876641320, -0.08942795157527998196, 0.3641732283464567121 ) ) ;
#17810 = CARTESIAN_POINT ( 'NONE',  ( -0.2858256400101373829, -0.07430968296373896553, 5.862902060615214239 ) ) ;
#17811 = CARTESIAN_POINT ( 'NONE',  ( -0.1443569553805768291, 0.05413385826771666132, 0.4176697321401328100 ) ) ;
#17812 = CONICAL_SURFACE ( 'NONE', #58086, 1.968503937007874072, 0.7853981633974500554 ) ;
#17813 = CARTESIAN_POINT ( 'NONE',  ( 0.2362204724409451007, -0.4091458600556402980, -0.9560367454068241511 ) ) ;
#17814 = CARTESIAN_POINT ( 'NONE',  ( -1.627296587926508442, 0.2306618581243848609, 0.2411417322834645549 ) ) ;
#17815 = CARTESIAN_POINT ( 'NONE',  ( 0.3917322834645669549, 0.1049643490035304660, -2.793963254593175183 ) ) ;
#17816 = ORIENTED_EDGE ( 'NONE', *, *, #10592, .F. ) ;
#17817 = VERTEX_POINT ( 'NONE', #60078 ) ;
#17818 = CARTESIAN_POINT ( 'NONE',  ( 0.4986876640419954376, -0.6046776061558809534, -0.2411417322834644161 ) ) ;
#17819 = CARTESIAN_POINT ( 'NONE',  ( 0.05905511811023681640, 0.07958543189024071263, -0.2665933059059888421 ) ) ;
#17821 = CARTESIAN_POINT ( 'NONE',  ( 0.6299212598424784870, 1.724409448818897905, 3.937007874015796105 ) ) ;
#17820 = CARTESIAN_POINT ( 'NONE',  ( -1.018726825260306112, 1.601686773136587805, 0.4703072575216136197 ) ) ;
#17822 = CARTESIAN_POINT ( 'NONE',  ( 0.1958661417322836440, -0.3392501089628017219, -1.278871391076115582 ) ) ;
#17823 = CARTESIAN_POINT ( 'NONE',  ( 0.2362204724409449064, 0.4091458600556404646, 0.09383202099737532331 ) ) ;
#17824 = CARTESIAN_POINT ( 'NONE',  ( 0.3030275874994733387, -1.017388752436352087E-17, -0.3627985898453451874 ) ) ;
#17825 = CARTESIAN_POINT ( 'NONE',  ( 0.1070741851644054776, -0.3996062992125984925, -2.839238845144356649 ) ) ;
#17826 = CARTESIAN_POINT ( 'NONE',  ( 0.3674540682414705883, 0.2306618581243847221, -0.2411417322834647770 ) ) ;
#17827 = CARTESIAN_POINT ( 'NONE',  ( -1.043307086614172041, -0.5400638737290844871, 0.3530559997133364547 ) ) ;
#17828 = CARTESIAN_POINT ( 'NONE',  ( -1.364829396325458521, 0.2306618581243847221, -0.2411417322834647770 ) ) ;
#17829 = CARTESIAN_POINT ( 'NONE',  ( 0.7808398950131240079, -0.3162353388693405765, 0.4822834645669290543 ) ) ;
#17830 = CARTESIAN_POINT ( 'NONE',  ( 0.7414698162729663755, -0.6692913385826773087, -0.1292274648535924053 ) ) ;
#17831 = CARTESIAN_POINT ( 'NONE',  ( 1.279527559055118724, -0.4536011799217368745, -0.2665933059059886201 ) ) ;
#17832 = CARTESIAN_POINT ( 'NONE',  ( 1.391076115485564868, 0.1283753931104746893, -0.1820866141732285504 ) ) ;
#17833 = CARTESIAN_POINT ( 'NONE',  ( -0.9514435695538050464, -0.05778040916215560624, -0.4822834645669293319 ) ) ;
#17834 = CARTESIAN_POINT ( 'NONE',  ( -0.1998031496062991630, -0.3460692066303959202, -0.4573490813648293796 ) ) ;
#17835 = CARTESIAN_POINT ( 'NONE',  ( 1.666666666666667185, 0.05413385826771666132, 0.4176697321401328100 ) ) ;
#17836 = CARTESIAN_POINT ( 'NONE',  ( -0.3917322834645670104, -7.196005306013484475E-17, -0.3464566929133857665 ) ) ;
#17837 = CARTESIAN_POINT ( 'NONE',  ( -0.1246719160104980823, -0.6692913385826773087, -0.1292274648535924053 ) ) ;
#17839 = CARTESIAN_POINT ( 'NONE',  ( 0.4606732211678797317, 2.401574803149606030, -0.5309055118110237448 ) ) ;
#17838 = CARTESIAN_POINT ( 'NONE',  ( 1.338582677165355062, -0.1870078740157479769, 0.4822834645669291653 ) ) ;
#17840 = CARTESIAN_POINT ( 'NONE',  ( -1.469816272965878357, -0.5023911411419708095, -0.1820866141732282451 ) ) ;
#17841 = CARTESIAN_POINT ( 'NONE',  ( 0.4068241469816281097, 0.05413385826771666132, 0.4176697321401328100 ) ) ;
#17842 = CARTESIAN_POINT ( 'NONE',  ( 0.9383202099737536495, -0.2845877964562159024, 0.3641732283464567677 ) ) ;
#17843 = CARTESIAN_POINT ( 'NONE',  ( 0.3917322834645668994, -0.1049643490035303134, -1.608904568732596685 ) ) ;
#17844 = CARTESIAN_POINT ( 'NONE',  ( -1.325459317585300889, -0.3690944881889765550, -0.3153832671262227771 ) ) ;
#17845 = CARTESIAN_POINT ( 'NONE',  ( 1.115485564304462551, -0.4281496062992127816, -0.4176697321401328100 ) ) ;
#17846 = CARTESIAN_POINT ( 'NONE',  ( -0.5249343832020990641, 0.2306618581243848609, 0.2411417322834645549 ) ) ;
#17847 = CARTESIAN_POINT ( 'NONE',  ( -0.6167979002624665030, -0.004921259842519576551, 0.3153832671262227771 ) ) ;
#17848 = CARTESIAN_POINT ( 'NONE',  ( -0.6692913385826764205, -0.6692913385826771977, 8.415575281601705876E-17 ) ) ;
#17849 = CARTESIAN_POINT ( 'NONE',  ( 1.476377952755906442, -0.5400638737290844871, 0.3530559997133364547 ) ) ;
#17850 = CARTESIAN_POINT ( 'NONE',  ( -0.5380577427821514602, -0.4281496062992127816, -0.4176697321401328100 ) ) ;
#17851 = CARTESIAN_POINT ( 'NONE',  ( 1.410761154855643795, -0.05778040916215560624, -0.4822834645669293319 ) ) ;
#17852 = CARTESIAN_POINT ( 'NONE',  ( 0.3392501089628018884, -0.1958661417322833942, -0.8891269273303956666 ) ) ;
#17853 = CARTESIAN_POINT ( 'NONE',  ( -1.102362204724408601, -0.1870078740157480601, -0.3641732283464567677 ) ) ;
#17854 = CARTESIAN_POINT ( 'NONE',  ( 1.044155967855882050, 1.298756420147472390, 0.4111758506720307738 ) ) ;
#17855 = CARTESIAN_POINT ( 'NONE',  ( 1.364829396325459854, -0.6046776061558809534, -0.2411417322834644161 ) ) ;
#17856 = CARTESIAN_POINT ( 'NONE',  ( 0.1265901696524989462, 0.4724409448818897572, -2.117454068241469756 ) ) ;
#17857 = CARTESIAN_POINT ( 'NONE',  ( -1.082677165354329896, 0.1660481256975885056, 0.3530559997133364547 ) ) ;
#17858 = CARTESIAN_POINT ( 'NONE',  ( -1.614173228346455824, 0.1771653543307087630, 0.000000000000000000 ) ) ;
#17859 = CARTESIAN_POINT ( 'NONE',  ( -0.5183727034120726440, -0.5511811023622048555, -0.09757992244046775898 ) ) ;
#17860 = CARTESIAN_POINT ( 'NONE',  ( -1.640419947506561060, 0.05413385826771666132, 0.4176697321401328100 ) ) ;
#17861 = CARTESIAN_POINT ( 'NONE',  ( -0.2690288713910754526, -0.6692913385826771977, 0.1292274648535927661 ) ) ;
#17862 = CARTESIAN_POINT ( 'NONE',  ( -0.07217847769028787330, -0.08942795157527998196, 0.3641732283464567121 ) ) ;
#17863 = CARTESIAN_POINT ( 'NONE',  ( -1.082677165354329896, 0.07958543189024085140, 0.2665933059059887866 ) ) ;
#17864 = CARTESIAN_POINT ( 'NONE',  ( 1.561679790026247350, -0.3690944881889763329, 0.3153832671262228327 ) ) ;
#17865 = AXIS2_PLACEMENT_3D ( 'NONE', #10381, #10787, #55380 ) ;
#17866 = CARTESIAN_POINT ( 'NONE',  ( 0.8530183727034128527, -0.4281496062992124485, 0.4176697321401328655 ) ) ;
#17867 = DIRECTION ( 'NONE',  ( 0.000000000000000000, 1.000000000000000000, 0.000000000000000000 ) ) ;
#17868 = CARTESIAN_POINT ( 'NONE',  ( 0.3608923884514443348, -0.5511811023622046335, 0.09757992244046803654 ) ) ;
#17869 = CARTESIAN_POINT ( 'NONE',  ( 0.2690288713910767848, 0.2952755905511811885, 0.1292274648535926551 ) ) ;
#17870 = CARTESIAN_POINT ( 'NONE',  ( 1.089238845144357537, -0.3690944881889763329, 0.3153832671262228327 ) ) ;
#17871 = ORIENTED_EDGE ( 'NONE', *, *, #76605, .T. ) ;
#17872 = CARTESIAN_POINT ( 'NONE',  ( -1.233595800524933894, -0.6046776061558809534, -0.2411417322834644161 ) ) ;
#17873 = CARTESIAN_POINT ( 'NONE',  ( -1.515748031496062076, -0.5400638737290844871, 0.3530559997133364547 ) ) ;
#17874 = CARTESIAN_POINT ( 'NONE',  ( -0.08530183727034056085, -0.05778040916215560624, -0.4822834645669293319 ) ) ;
#17875 = CARTESIAN_POINT ( 'NONE',  ( -2.138259192565297173, 1.653403552777525487, -0.4602852883866582201 ) ) ;
#17876 = CARTESIAN_POINT ( 'NONE',  ( 0.1998031496062994128, -0.3460692066303957537, -2.530839895013123453 ) ) ;
#17877 = CARTESIAN_POINT ( 'NONE',  ( 0.5249343832021003964, 0.2306618581243847221, -0.2411417322834647770 ) ) ;
#17878 = CARTESIAN_POINT ( 'NONE',  ( 1.456692913385827515, 0.1771653543307087630, 0.000000000000000000 ) ) ;
#17879 = CARTESIAN_POINT ( 'NONE',  ( -0.1377952755905504645, -0.5400638737290845981, -0.3530559997133363437 ) ) ;
#17880 = CARTESIAN_POINT ( 'NONE',  ( 0.9842519685039375910, 0.2952755905511811885, 0.000000000000000000 ) ) ;
#17881 = CARTESIAN_POINT ( 'NONE',  ( 0.2925321140481932369, 0.2925321140481932369, -2.027559055118109743 ) ) ;
#17882 = CARTESIAN_POINT ( 'NONE',  ( 0.1058382717557500713, -0.3949938075777409408, -1.502624671916010790 ) ) ;
#17883 = CARTESIAN_POINT ( 'NONE',  ( -0.4104818416650150570, 1.299051044647045128, 1.044297694901411555 ) ) ;
#17884 = LINE ( 'NONE', #62903, #76222 ) ;
#17885 = CARTESIAN_POINT ( 'NONE',  ( -0.1958661417322834220, -0.3392501089628018884, -0.5301837270341206443 ) ) ;
#17886 = CARTESIAN_POINT ( 'NONE',  ( -0.7283464566929126471, 0.07958543189024071263, -0.2665933059059888421 ) ) ;
#17887 = CARTESIAN_POINT ( 'NONE',  ( -0.6364829396325453192, -0.3162353388693405765, 0.4822834645669290543 ) ) ;
#17888 = CARTESIAN_POINT ( 'NONE',  ( 0.5183727034120741983, 0.2952755905511810774, -0.1292274648535930714 ) ) ;
#17889 = CARTESIAN_POINT ( 'NONE',  ( -0.1058382717557503072, 0.3949938075777408852, -2.603018372703412187 ) ) ;
#17890 = CARTESIAN_POINT ( 'NONE',  ( 1.023622047244095334, -0.1870078740157479769, 0.4822834645669291653 ) ) ;
#17891 = CARTESIAN_POINT ( 'NONE',  ( -1.397637795275589623, -0.5400638737290845981, -0.3530559997133363437 ) ) ;
#17892 = CARTESIAN_POINT ( 'NONE',  ( 0.8530183727034126306, 0.05413385826771626580, -0.4176697321401330321 ) ) ;
#17893 = FACE_OUTER_BOUND ( 'NONE', #83208, .T. ) ;
#17894 = CARTESIAN_POINT ( 'NONE',  ( -0.1998031496062994683, 0.3460692066303958092, -2.060367454068241511 ) ) ;
#17895 = CARTESIAN_POINT ( 'NONE',  ( 1.482939632545932307, -0.4281496062992124485, 0.4176697321401328655 ) ) ;
#17896 = CARTESIAN_POINT ( 'NONE',  ( 0.9973753280839902091, 0.2306618581243847221, -0.2411417322834647770 ) ) ;
#17897 = EDGE_CURVE ( 'NONE', #75063, #3939, #42675, .T. ) ;
#17898 = CARTESIAN_POINT ( 'NONE',  ( 0.5905511811023629321, -0.6692913385826771977, 8.415575281601705876E-17 ) ) ;
#17899 = CARTESIAN_POINT ( 'NONE',  ( 1.187664041994751285, -0.2845877964562161244, -0.3641732283464567121 ) ) ;
#17901 = CARTESIAN_POINT ( 'NONE',  ( -1.430446194225720724, 0.05413385826771626580, -0.4176697321401330321 ) ) ;
#17900 = CARTESIAN_POINT ( 'NONE',  ( -1.607611548556429737, 0.1771653543307087075, -0.09757992244046823083 ) ) ;
#17902 = CARTESIAN_POINT ( 'NONE',  ( -0.1958661417322834220, -0.3392501089628018884, -0.1502624671916011345 ) ) ;
#17903 =( NAMED_UNIT ( * ) SI_UNIT ( $, .STERADIAN. ) SOLID_ANGLE_UNIT ( ) );
#17904 = CARTESIAN_POINT ( 'NONE',  ( 0.9186351706036752773, 0.2306618581243847221, -0.2411417322834647770 ) ) ;
#17905 = CIRCLE ( 'NONE', #67656, 2.165354330708661568 ) ;
#17906 = CARTESIAN_POINT ( 'NONE',  ( 1.653543307086614789, -0.1870078740157479769, 0.3641732283464567677 ) ) ;
#17907 = CARTESIAN_POINT ( 'NONE',  ( -0.2952755905511804668, 0.1660481256975885056, 0.3530559997133364547 ) ) ;
#17908 = CARTESIAN_POINT ( 'NONE',  ( -0.8070866141732276899, -0.5400638737290844871, 0.3530559997133364547 ) ) ;
#17909 = CARTESIAN_POINT ( 'NONE',  ( -1.482939632545930975, 0.05413385826771666132, 0.4176697321401328100 ) ) ;
#17910 = CARTESIAN_POINT ( 'NONE',  ( -9.594673741351313045E-17, 0.3917322834645670104, -0.3996062992125985480 ) ) ;
#17911 = CARTESIAN_POINT ( 'NONE',  ( -9.594673741351313045E-17, 0.3917322834645670104, -1.409448818897637734 ) ) ;
#17912 = CARTESIAN_POINT ( 'NONE',  ( -0.1958661417322834220, -0.3392501089628018884, -2.734908136482939511 ) ) ;
#17913 = CARTESIAN_POINT ( 'NONE',  ( 1.686351706036745890, 0.2952755905511811885, 0.1292274648535926551 ) ) ;
#17914 = ORIENTED_EDGE ( 'NONE', *, *, #3352, .T. ) ;
#17915 = CARTESIAN_POINT ( 'NONE',  ( -0.1974969037888706647, 0.3420746716998658843, -2.847769028871391495 ) ) ;
#17916 = ORIENTED_EDGE ( 'NONE', *, *, #8023, .T. ) ;
#17917 = CARTESIAN_POINT ( 'NONE',  ( -0.01277272433825534827, 0.004960608223779807216, -0.3437734562760184631 ) ) ;
#17918 = CARTESIAN_POINT ( 'NONE',  ( 1.535433070866142335, -0.5511811023622047445, 6.969142054262312111E-17 ) ) ;
#17919 = CARTESIAN_POINT ( 'NONE',  ( 0.3996062992125986590, -0.1070741851644053111, -1.371391076115485053 ) ) ;
#17920 = CARTESIAN_POINT ( 'NONE',  ( 1.141392835773559211, 0.3937007874015747699, 1.339227481442854195 ) ) ;
#17921 = CARTESIAN_POINT ( 'NONE',  ( 0.000000000000000000, 0.000000000000000000, 0.1181102362204724116 ) ) ;
#17922 = CARTESIAN_POINT ( 'NONE',  ( -0.3129921259842520787, 1.496062992125984259, 2.300774849103979725E-17 ) ) ;
#17923 = CARTESIAN_POINT ( 'NONE',  ( 0.2867679344610365999, -0.2867679344610365444, -0.4980314960629922405 ) ) ;
#17924 = VECTOR ( 'NONE', #25188, 39.37007874015748143 ) ;
#17925 = CARTESIAN_POINT ( 'NONE',  ( -0.8923884514435688198, -0.5023911411419708095, 0.1820866141732285504 ) ) ;
#17926 = CARTESIAN_POINT ( 'NONE',  ( -1.108923884514435132, -0.2845877964562159024, 0.3641732283464567677 ) ) ;
#17927 = CARTESIAN_POINT ( 'NONE',  ( -1.364829396325458521, -0.6046776061558807314, 0.2411417322834647770 ) ) ;
#17928 = CARTESIAN_POINT ( 'NONE',  ( 0.01312335958005323398, 0.05413385826771666132, 0.4176697321401328100 ) ) ;
#17929 = CARTESIAN_POINT ( 'NONE',  ( -1.384514435695537005, -0.6692913385826773087, -0.1292274648535924053 ) ) ;
#17930 = ORIENTED_EDGE ( 'NONE', *, *, #20551, .T. ) ;
#17931 = CARTESIAN_POINT ( 'NONE',  ( -1.633858267716534529, 0.1660481256975885056, 0.3530559997133364547 ) ) ;
#17932 = FACE_OUTER_BOUND ( 'NONE', #78665, .T. ) ;
#17933 = CARTESIAN_POINT ( 'NONE',  ( 0.4724409448818898682, 2.892866454678787531E-17, -1.850393700787401619 ) ) ;
#17934 = PLANE ( 'NONE',  #12973 ) ;
#17935 = CARTESIAN_POINT ( 'NONE',  ( -0.6102362204724400829, -0.4536011799217368745, -0.2665933059059886201 ) ) ;
#17936 = CARTESIAN_POINT ( 'NONE',  ( -1.095800524934382292, -0.3162353388693409650, -0.4822834645669289433 ) ) ;
#17937 = CARTESIAN_POINT ( 'NONE',  ( 1.010498687664042716, -0.4281496062992124485, 0.4176697321401328655 ) ) ;
#17938 = ORIENTED_EDGE ( 'NONE', *, *, #69071, .T. ) ;
#17940 = CARTESIAN_POINT ( 'NONE',  ( -0.4653577321740608452, 1.629972608277046708, 2.575297182719555877 ) ) ;
#17939 = CARTESIAN_POINT ( 'NONE',  ( 0.000000000000000000, 0.000000000000000000, 0.000000000000000000 ) ) ;
#17941 = CARTESIAN_POINT ( 'NONE',  ( 1.627296587926509996, -0.6046776061558807314, 0.2411417322834647770 ) ) ;
#17942 = CARTESIAN_POINT ( 'NONE',  ( -1.391076115485563758, 0.2306618581243848609, 0.2411417322834645549 ) ) ;
#17943 = CARTESIAN_POINT ( 'NONE',  ( 0.3917322834645669549, 2.398668435337827645E-17, -0.3556237288375834749 ) ) ;
#17944 = CARTESIAN_POINT ( 'NONE',  ( 0.2034120734908142214, 0.1771653543307087075, -0.09757992244046823083 ) ) ;
#17945 = CARTESIAN_POINT ( 'NONE',  ( 0.3392501089628018329, 0.1958661417322835607, -0.6883202099737534274 ) ) ;
#17946 = CARTESIAN_POINT ( 'NONE',  ( -0.2230971128608915943, -0.004921259842519576551, 0.3153832671262227771 ) ) ;
#17947 = CARTESIAN_POINT ( 'NONE',  ( 0.6036745406824153282, -0.5023911411419708095, 0.1820866141732285504 ) ) ;
#17948 = CARTESIAN_POINT ( 'NONE',  ( 0.4921259842519691285, 0.1660481256975885056, 0.3530559997133364547 ) ) ;
#17949 = CARTESIAN_POINT ( 'NONE',  ( -0.6561679790026240244, 0.1283753931104746893, -0.1820866141732285504 ) ) ;
#17950 = CARTESIAN_POINT ( 'NONE',  ( -0.1049643490035302024, -0.3917322834645671215, -2.583989501312335513 ) ) ;
#17951 = CARTESIAN_POINT ( 'NONE',  ( 1.069553805774278610, -0.6692913385826771977, 0.1292274648535927661 ) ) ;
#17952 = CARTESIAN_POINT ( 'NONE',  ( -0.8267716535433065062, 0.2952755905511811885, 0.000000000000000000 ) ) ;
#17953 = CARTESIAN_POINT ( 'NONE',  ( -0.3458507752293906723, -0.3458507752293910609, -0.9232283464566929387 ) ) ;
#17954 = CARTESIAN_POINT ( 'NONE',  ( 0.01968503937007930540, 0.1660481256975885056, 0.3530559997133364547 ) ) ;
#17955 = CARTESIAN_POINT ( 'NONE',  ( -0.5380577427821514602, 0.05413385826771666132, 0.4176697321401328100 ) ) ;
#17956 = CARTESIAN_POINT ( 'NONE',  ( 1.246719160104987623, -0.004921259842519870586, -0.3153832671262229437 ) ) ;
#17957 = CARTESIAN_POINT ( 'NONE',  ( -0.07874015748031421014, -0.1870078740157480601, -0.3641732283464567677 ) ) ;
#17958 = CARTESIAN_POINT ( 'NONE',  ( -0.1115485564304456306, 0.2952755905511810774, -0.1292274648535930714 ) ) ;
#17959 = CARTESIAN_POINT ( 'NONE',  ( -1.017060367454067249, -0.05778040916215522460, 0.4822834645669289988 ) ) ;
#17960 = CARTESIAN_POINT ( 'NONE',  ( -3.900966923095587457, 2.682389230697235671, 0.5314960629921258173 ) ) ;
#17961 = CARTESIAN_POINT ( 'NONE',  ( 1.601049868766404982, -0.5023911411419708095, -0.1820866141732282451 ) ) ;
#17962 = CONICAL_SURFACE ( 'NONE', #54228, 0.4923228346456693938, 0.7853981633974415066 ) ;
#17963 = CARTESIAN_POINT ( 'NONE',  ( -0.1049868766404193215, -0.6046776061558807314, 0.2411417322834647770 ) ) ;
#17964 = VERTEX_POINT ( 'NONE', #23735 ) ;
#17965 = CARTESIAN_POINT ( 'NONE',  ( 0.3996062992125984925, 0.1070741851644054637, -2.091207349081364519 ) ) ;
#17966 = CARTESIAN_POINT ( 'NONE',  ( 1.174540682414699111, -0.05778040916215560624, -0.4822834645669293319 ) ) ;
#17967 = CARTESIAN_POINT ( 'NONE',  ( -0.4527559055118102749, 0.07958543189024085140, 0.2665933059059887866 ) ) ;
#17968 = CARTESIAN_POINT ( 'NONE',  ( -0.5052493438320203589, -0.6692913385826771977, 0.1292274648535927661 ) ) ;
#17969 = CARTESIAN_POINT ( 'NONE',  ( 1.358267716535433323, 0.1660481256975885056, 0.3530559997133364547 ) ) ;
#17970 = CARTESIAN_POINT ( 'NONE',  ( 0.9908136482939640111, -0.6692913385826771977, 0.1292274648535927661 ) ) ;
#17971 = CARTESIAN_POINT ( 'NONE',  ( -0.3372635250547070807, 0.3676148930005934123, -0.006554863637384360751 ) ) ;
#17972 = CARTESIAN_POINT ( 'NONE',  ( -1.076115485564303809, 0.1283753931104748280, 0.1820866141732283561 ) ) ;
#17973 = CARTESIAN_POINT ( 'NONE',  ( -9.787531504996566615E-17, 0.3996062992125985480, -0.8641732283464567121 ) ) ;
#17974 = CARTESIAN_POINT ( 'NONE',  ( 0.3996062992125986035, 2.446882876249141962E-17, -1.062992125984252079 ) ) ;
#17975 = CIRCLE ( 'NONE', #16606, 3.937007874015748143 ) ;
#17976 = CARTESIAN_POINT ( 'NONE',  ( -0.3949938075777409963, -7.255918531996591613E-17, -0.1968503937007874682 ) ) ;
#17977 = CARTESIAN_POINT ( 'NONE',  ( 0.3227188174119076658, 1.189353863002647449, 2.759699577397270343 ) ) ;
#17978 = CARTESIAN_POINT ( 'NONE',  ( 1.233595800524935227, 0.1283753931104746893, -0.1820866141732285504 ) ) ;
#17979 = CARTESIAN_POINT ( 'NONE',  ( 0.8136482939632553313, 0.1283753931104748280, 0.1820866141732283561 ) ) ;
#17980 = CARTESIAN_POINT ( 'NONE',  ( 0.5643044619422579178, -0.4281496062992127816, -0.4176697321401328100 ) ) ;
#17981 = CARTESIAN_POINT ( 'NONE',  ( 1.495848283907322829E-16, 0.4201155382560080032, 1.198416298106748767 ) ) ;
#17982 = CARTESIAN_POINT ( 'NONE',  ( 0.1974969037888706092, -0.3420746716998660508, -1.428477690288714186 ) ) ;
#17983 = CARTESIAN_POINT ( 'NONE',  ( 0.6496062992125991586, -0.4536011799217368745, -0.2665933059059886201 ) ) ;
#17984 = EDGE_CURVE ( 'NONE', #4208, #2914, #3974, .T. ) ;
#17985 = CARTESIAN_POINT ( 'NONE',  ( -0.2493438320209966919, -0.4281496062992124485, 0.4176697321401328655 ) ) ;
#17986 = CARTESIAN_POINT ( 'NONE',  ( -0.9186351706036736120, -0.6046776061558809534, -0.2411417322834644161 ) ) ;
#17987 = CARTESIAN_POINT ( 'NONE',  ( 1.240157480314961314, 0.1660481256975883668, -0.3530559997133364547 ) ) ;
#17988 = CARTESIAN_POINT ( 'NONE',  ( -0.4091458600556405756, 0.2362204724409446288, -1.286089238845144367 ) ) ;
#17989 = CARTESIAN_POINT ( 'NONE',  ( 4.893765752498283924E-17, -0.3996062992125986035, -2.755905511811023612 ) ) ;
#17990 = CARTESIAN_POINT ( 'NONE',  ( 0.05905511811023681640, 0.07958543189024071263, -0.2665933059059888421 ) ) ;
#17991 = ORIENTED_EDGE ( 'NONE', *, *, #52780, .F. ) ;
#17992 = CARTESIAN_POINT ( 'NONE',  ( -0.1049643490035307158, 0.3917322834645670104, -0.9481820454406320042 ) ) ;
#17993 = ORIENTED_EDGE ( 'NONE', *, *, #24157, .F. ) ;
#17994 = CARTESIAN_POINT ( 'NONE',  ( -0.8923884514435688198, 0.2306618581243847221, -0.2411417322834647770 ) ) ;
#17995 = CARTESIAN_POINT ( 'NONE',  ( -0.3149606299212590610, -0.1870078740157480879, -0.4822834645669291653 ) ) ;
#17996 = CARTESIAN_POINT ( 'NONE',  ( -0.3805774278215216522, 0.05413385826771666132, 0.4176697321401328100 ) ) ;
#17997 = DIMENSIONAL_EXPONENTS ( 1.000000000000000000, 0.000000000000000000, 0.000000000000000000, 0.000000000000000000, 0.000000000000000000, 0.000000000000000000, 0.000000000000000000 ) ;
#17998 = CARTESIAN_POINT ( 'NONE',  ( 0.5183727034120741983, -0.6692913385826771977, 0.1292274648535927661 ) ) ;
#17999 = CARTESIAN_POINT ( 'NONE',  ( -0.4002624671916004129, -0.3162353388693405765, 0.4822834645669290543 ) ) ;
#18000 = CARTESIAN_POINT ( 'NONE',  ( -1.489501312335957062, -0.05778040916215522460, 0.4822834645669289988 ) ) ;
#18001 = CARTESIAN_POINT ( 'NONE',  ( -0.8989501312335946848, 0.2952755905511810774, -0.1292274648535930714 ) ) ;
#18002 = CARTESIAN_POINT ( 'NONE',  ( 0.5708661417322841158, -0.5400638737290845981, -0.3530559997133363437 ) ) ;
#18003 = CARTESIAN_POINT ( 'NONE',  ( 0.3917322834645670104, 2.398668435337828261E-17, -1.055118110236220375 ) ) ;
#18004 = CARTESIAN_POINT ( 'NONE',  ( -0.4068241469816264999, -0.3690944881889763329, 0.3153832671262228327 ) ) ;
#18005 = ORIENTED_EDGE ( 'NONE', *, *, #32101, .T. ) ;
#18006 = CARTESIAN_POINT ( 'NONE',  ( -0.1974969037888706647, 0.3420746716998658843, -1.587926509186351920 ) ) ;
#18007 = ORIENTED_EDGE ( 'NONE', *, *, #11474, .T. ) ;
#18008 = CARTESIAN_POINT ( 'NONE',  ( -1.128608923884513837, -0.5023911411419708095, 0.1820866141732285504 ) ) ;
#18009 = CARTESIAN_POINT ( 'NONE',  ( -1.003937007874014853, 0.1660481256975885056, 0.3530559997133364547 ) ) ;
#18010 = CARTESIAN_POINT ( 'NONE',  ( -0.7020997375328074108, -0.05778040916215522460, 0.4822834645669289988 ) ) ;
#18011 = CARTESIAN_POINT ( 'NONE',  ( -0.3460692066303960868, 0.1998031496062990242, -0.1837270341207349056 ) ) ;
#18012 = CARTESIAN_POINT ( 'NONE',  ( -0.6692913385826764205, -0.6692913385826771977, 8.415575281601705876E-17 ) ) ;
#18013 = CARTESIAN_POINT ( 'NONE',  ( -0.8989501312335946848, 0.2952755905511810774, -0.1292274648535930714 ) ) ;
#18014 = CARTESIAN_POINT ( 'NONE',  ( 1.436417322834644406, 0.8346805926620876059, 0.3149606299212598381 ) ) ;
#18015 = LINE ( 'NONE', #43238, #20075 ) ;
#18016 = CARTESIAN_POINT ( 'NONE',  ( 0.4527559055118117182, 0.07958543189024071263, -0.2665933059059888421 ) ) ;
#18017 = DIRECTION ( 'NONE',  ( 0.000000000000000000, 0.000000000000000000, -1.000000000000000000 ) ) ;
#18018 = CARTESIAN_POINT ( 'NONE',  ( -0.1958661417322834220, -0.3392501089628018884, -0.1502624671916011345 ) ) ;
#18019 = CARTESIAN_POINT ( 'NONE',  ( -0.1181102362204717315, 0.1771653543307087630, 0.000000000000000000 ) ) ;
#18020 = AXIS2_PLACEMENT_3D ( 'NONE', #81374, #67494, #74648 ) ;
#18021 = CARTESIAN_POINT ( 'NONE',  ( -0.1771653543307080136, 0.1660481256975883668, -0.3530559997133364547 ) ) ;
#18022 = CARTESIAN_POINT ( 'NONE',  ( 1.601049868766404982, 0.2306618581243848609, 0.2411417322834645549 ) ) ;
#18023 = CARTESIAN_POINT ( 'NONE',  ( -0.1771653543307080136, 0.1660481256975883668, -0.3530559997133364547 ) ) ;
#18024 = ORIENTED_EDGE ( 'NONE', *, *, #58932, .F. ) ;
#18025 = CARTESIAN_POINT ( 'NONE',  ( -0.3996062992125987146, 0.1070741851644051862, -2.237532808398950301 ) ) ;
#18026 = DIRECTION ( 'NONE',  ( 0.000000000000000000, 0.000000000000000000, -1.000000000000000000 ) ) ;
#18027 = VERTEX_POINT ( 'NONE', #74273 ) ;
#18028 = CARTESIAN_POINT ( 'NONE',  ( 0.2925321140481932369, 0.2925321140481932369, -1.789370078740157410 ) ) ;
#18029 = CARTESIAN_POINT ( 'NONE',  ( -0.1829408352246092440, 0.2319625946588664833, 0.1465682319128801259 ) ) ;
#18030 = CARTESIAN_POINT ( 'NONE',  ( -0.9842519685039365918, -0.5511811023622047445, 6.969142054262312111E-17 ) ) ;
#18031 = CARTESIAN_POINT ( 'NONE',  ( -1.463254593175852492, -0.6692913385826773087, -0.1292274648535924053 ) ) ;
#18032 = CARTESIAN_POINT ( 'NONE',  ( -0.2362204724409447953, -0.4091458600556404646, -0.3805774278215223183 ) ) ;
#18033 = CARTESIAN_POINT ( 'NONE',  ( -0.7426113562971994320, 2.199547029021313715, 0.5309055118110236338 ) ) ;
#18034 = CARTESIAN_POINT ( 'NONE',  ( 0.3917322834645670104, 2.398668435337828261E-17, 0.04724409448818902429 ) ) ;
#18035 = CARTESIAN_POINT ( 'NONE',  ( 1.266404199475066328, -0.3162353388693409650, -0.4822834645669289433 ) ) ;
#18036 = CARTESIAN_POINT ( 'NONE',  ( 0.4527559055118117182, -0.5400638737290844871, 0.3530559997133364547 ) ) ;
#18037 = CARTESIAN_POINT ( 'NONE',  ( 0.2034120734908144990, -0.6692913385826771977, 0.1292274648535927661 ) ) ;
#18038 = CARTESIAN_POINT ( 'NONE',  ( -1.272965879265091305, -0.004921259842519870586, -0.3153832671262229437 ) ) ;
#18039 = CARTESIAN_POINT ( 'NONE',  ( -0.2493438320209966919, 0.05413385826771626580, -0.4176697321401330321 ) ) ;
#18040 = CARTESIAN_POINT ( 'NONE',  ( -0.4724409448818899238, 0.1265901696524986686, -2.471784776902887337 ) ) ;
#18041 = CARTESIAN_POINT ( 'NONE',  ( -0.9842519685039365918, -0.6692913385826771977, 8.415575281601705876E-17 ) ) ;
#18042 = CIRCLE ( 'NONE', #16724, 3.937007874015748143 ) ;
#18043 = CARTESIAN_POINT ( 'NONE',  ( -9.674558042662122972E-17, 0.3949938075777409963, -2.281496062992126372 ) ) ;
#18044 = CARTESIAN_POINT ( 'NONE',  ( 1.377952755905512472, -0.5511811023622047445, 6.969142054262312111E-17 ) ) ;
#18045 = CARTESIAN_POINT ( 'NONE',  ( -0.1640419947506555343, -0.2845877964562159024, 0.3641732283464567677 ) ) ;
#18046 = CARTESIAN_POINT ( 'NONE',  ( 1.345144356955381593, -0.08942795157527998196, 0.3641732283464567121 ) ) ;
#18047 = CARTESIAN_POINT ( 'NONE',  ( -1.476377952755905110, -0.5400638737290845981, -0.3530559997133363437 ) ) ;
#18048 = CARTESIAN_POINT ( 'NONE',  ( -0.9448818897637790704, -0.1870078740157480601, -0.3641732283464567677 ) ) ;
#18049 = CARTESIAN_POINT ( 'NONE',  ( -1.559171609364246924, 0.000000000000000000, 0.4177787735906735578 ) ) ;
#18050 = CARTESIAN_POINT ( 'NONE',  ( 0.6233595800524942554, -0.08942795157528024563, -0.3641732283464568787 ) ) ;
#18051 = CARTESIAN_POINT ( 'NONE',  ( -0.3937007874015740483, -0.1870078740157479769, 0.4822834645669291653 ) ) ;
#18052 = CARTESIAN_POINT ( 'NONE',  ( 0.2755905511811031494, 0.2952755905511811885, 0.000000000000000000 ) ) ;
#18053 = CARTESIAN_POINT ( 'NONE',  ( -0.02624671916010428221, 0.1283753931104746893, -0.1820866141732285504 ) ) ;
#18054 = CARTESIAN_POINT ( 'NONE',  ( -0.1265901696524993347, 0.4724409448818896462, -1.028215223097112663 ) ) ;
#18055 = CARTESIAN_POINT ( 'NONE',  ( 0.8136482939632553313, -0.6046776061558809534, -0.2411417322834644161 ) ) ;
#18056 = CARTESIAN_POINT ( 'NONE',  ( 1.948818897637795367, 0.000000000000000000, 5.701968306260621233 ) ) ;
#18057 = CARTESIAN_POINT ( 'NONE',  ( 1.227034120734908917, -0.5511811023622046335, 0.09757992244046803654 ) ) ;
#18058 = CARTESIAN_POINT ( 'NONE',  ( -1.122047244094487306, -0.5400638737290844871, 0.3530559997133364547 ) ) ;
#18059 = CARTESIAN_POINT ( 'NONE',  ( -0.2296587926509179312, -0.08942795157527998196, 0.3641732283464567121 ) ) ;
#18060 = LINE ( 'NONE', #50428, #56922 ) ;
#18061 = CARTESIAN_POINT ( 'NONE',  ( 0.1640419947506569498, -0.08942795157527998196, 0.3641732283464567121 ) ) ;
#18062 = CARTESIAN_POINT ( 'NONE',  ( -1.213910761154854745, 0.2952755905511810774, -0.1292274648535930714 ) ) ;
#18063 = CARTESIAN_POINT ( 'NONE',  ( -0.3412073490813641308, 0.2306618581243847221, -0.2411417322834647770 ) ) ;
#18064 = CARTESIAN_POINT ( 'NONE',  ( 4.893765752498283308E-17, -0.3996062992125985480, -0.6279527559055118058 ) ) ;
#18065 = CARTESIAN_POINT ( 'NONE',  ( 4.797336870675656522E-17, -0.3917322834645670104, -2.053149606299212948 ) ) ;
#18066 = CARTESIAN_POINT ( 'NONE',  ( 0.6824146981627303710, 0.1283753931104746893, -0.1820866141732285504 ) ) ;
#18067 = CARTESIAN_POINT ( 'NONE',  ( -0.3280839895013117347, 0.05413385826771626580, -0.4176697321401330321 ) ) ;
#18068 = CARTESIAN_POINT ( 'NONE',  ( -0.6627296587926501115, 0.2952755905511810774, -0.1292274648535930714 ) ) ;
#18069 = CARTESIAN_POINT ( 'NONE',  ( -0.9776902887139098386, 0.1771653543307087075, -0.09757992244046823083 ) ) ;
#18070 = DIRECTION ( 'NONE',  ( 0.000000000000000000, 0.000000000000000000, 1.000000000000000000 ) ) ;
#18071 = CARTESIAN_POINT ( 'NONE',  ( -0.1968503937007867743, 0.2952755905511811885, 0.000000000000000000 ) ) ;
#18072 = CARTESIAN_POINT ( 'NONE',  ( -1.437007874015747477, -0.4536011799217367080, 0.2665933059059888421 ) ) ;
#18073 = CARTESIAN_POINT ( 'NONE',  ( -1.358267716535432434, -0.5400638737290844871, 0.3530559997133364547 ) ) ;
#18074 = CARTESIAN_POINT ( 'NONE',  ( -0.4091458600556405756, 0.2362204724409446288, -2.230971128608923770 ) ) ;
#18075 = ORIENTED_EDGE ( 'NONE', *, *, #82328, .T. ) ;
#18076 = CIRCLE ( 'NONE', #50316, 2.559055118110236560 ) ;
#18077 = LINE ( 'NONE', #24777, #6857 ) ;
#18078 = CARTESIAN_POINT ( 'NONE',  ( -1.417322834645668772, -0.1870078740157479769, 0.4822834645669291653 ) ) ;
#18079 = CARTESIAN_POINT ( 'NONE',  ( -0.8530183727034112984, -0.4281496062992127816, -0.4176697321401328100 ) ) ;
#18080 = CARTESIAN_POINT ( 'NONE',  ( -1.646981627296586703, -0.05778040916215522460, 0.4822834645669289988 ) ) ;
#18081 = CARTESIAN_POINT ( 'NONE',  ( 0.3917322834645669549, 0.1049643490035304660, -1.626640419947506411 ) ) ;
#18082 = CARTESIAN_POINT ( 'NONE',  ( -1.559171609364246924, 0.3937007874015748254, 0.4177787735906735578 ) ) ;
#18083 = CARTESIAN_POINT ( 'NONE',  ( 1.036745406824147731, 0.05413385826771666132, 0.4176697321401328100 ) ) ;
#18084 = CARTESIAN_POINT ( 'NONE',  ( 0.4461942257217856311, 0.2306618581243847221, -0.2411417322834647770 ) ) ;
#18085 = CARTESIAN_POINT ( 'NONE',  ( -0.1265901696524993347, 0.4724409448818896462, -0.4790026246719158998 ) ) ;
#18086 = CARTESIAN_POINT ( 'NONE',  ( 0.3996062992125985480, 2.446882876249141654E-17, -2.557086614173228689 ) ) ;
#18087 = CARTESIAN_POINT ( 'NONE',  ( 1.102362204724410155, -0.1870078740157479769, 0.3641732283464567677 ) ) ;
#18088 = CARTESIAN_POINT ( 'NONE',  ( 0.3996062992125986035, 0.1070741851644054776, -1.069553805774278166 ) ) ;
#18089 = ORIENTED_EDGE ( 'NONE', *, *, #33244, .F. ) ;
#18091 = CARTESIAN_POINT ( 'NONE',  ( -0.2867679344610365999, 0.2867679344610364889, -2.531496062992125484 ) ) ;
#18090 = CONICAL_SURFACE ( 'NONE', #81245, 2.401574803149606918, 0.7125723459225955514 ) ;
#18092 = ORIENTED_EDGE ( 'NONE', *, *, #39798, .F. ) ;
#18093 = CARTESIAN_POINT ( 'NONE',  ( 0.4265091863517067039, -0.6692913385826773087, -0.1292274648535924053 ) ) ;
#18094 = CARTESIAN_POINT ( 'NONE',  ( -0.7545931758530177724, 0.2952755905511811885, 0.1292274648535926551 ) ) ;
#18095 =( REPRESENTATION_RELATIONSHIP ('NONE','NONE', #79348, #76132 ) REPRESENTATION_RELATIONSHIP_WITH_TRANSFORMATION ( #80164 )SHAPE_REPRESENTATION_RELATIONSHIP( ) );
#18096 = CARTESIAN_POINT ( 'NONE',  ( 1.555118110236221041, -0.5400638737290844871, 0.3530559997133364547 ) ) ;
#18097 = CARTESIAN_POINT ( 'NONE',  ( 0.9645669291338591078, -0.5400638737290845981, -0.3530559997133363437 ) ) ;
#18098 = CARTESIAN_POINT ( 'NONE',  ( 1.627296587926509996, -0.6046776061558807314, 0.2411417322834647770 ) ) ;
#18099 = DIRECTION ( 'NONE',  ( -0.4999999999999955036, -0.7071067811865522357, -0.4999999999999977796 ) ) ;
#18100 = CARTESIAN_POINT ( 'NONE',  ( -0.2296587926509179312, -0.05778040916215522460, 0.4822834645669289988 ) ) ;
#18101 = CARTESIAN_POINT ( 'NONE',  ( -1.391076115485563314, -0.6046776061558809534, -0.2411417322834644161 ) ) ;
#18102 = CARTESIAN_POINT ( 'NONE',  ( -1.574803149606298192, -0.1870078740157480879, -0.4822834645669291653 ) ) ;
#18103 = CARTESIAN_POINT ( 'NONE',  ( 1.692913385826772421, 0.2952755905511811885, 0.000000000000000000 ) ) ;
#18104 = CARTESIAN_POINT ( 'NONE',  ( -0.2867679344610364334, -0.2867679344610367109, -2.820866141732283339 ) ) ;
#18105 = CARTESIAN_POINT ( 'NONE',  ( 0.8530183727034128527, -0.3690944881889763329, 0.3153832671262228327 ) ) ;
#18106 = ORIENTED_EDGE ( 'NONE', *, *, #30053, .F. ) ;
#18107 = CARTESIAN_POINT ( 'NONE',  ( 0.3949938075777409963, 2.418639510665530435E-17, -0.2755905511811024278 ) ) ;
#18108 = EDGE_LOOP ( 'NONE', ( #21522, #63769, #53206, #35290 ) ) ;
#18109 = CARTESIAN_POINT ( 'NONE',  ( -0.1706036745406816491, -0.3690944881889763329, 0.3153832671262228327 ) ) ;
#18110 = CARTESIAN_POINT ( 'NONE',  ( -1.633858267716534529, -0.5400638737290845981, -0.3530559997133363437 ) ) ;
#18111 = CARTESIAN_POINT ( 'NONE',  ( 0.4855643044619428750, 0.05413385826771666132, 0.4176697321401328100 ) ) ;
#18112 = CARTESIAN_POINT ( 'NONE',  ( 0.4461942257217855201, -0.6046776061558807314, 0.2411417322834647770 ) ) ;
#18113 = CARTESIAN_POINT ( 'NONE',  ( -0.4068241469816267775, 0.05413385826771626580, -0.4176697321401330321 ) ) ;
#18114 = CARTESIAN_POINT ( 'NONE',  ( 4.797336870675656522E-17, -0.3917322834645670659, -1.492801468012810329 ) ) ;
#18115 = CARTESIAN_POINT ( 'NONE',  ( -1.062992125984250968, -0.6692913385826771977, 8.415575281601705876E-17 ) ) ;
#18116 = CARTESIAN_POINT ( 'NONE',  ( -0.3917322834645670104, -7.196005306013484475E-17, -2.643700787401574548 ) ) ;
#18117 = CARTESIAN_POINT ( 'NONE',  ( 1.404199475065617264, -0.3690944881889763329, 0.3153832671262228327 ) ) ;
#18118 = CARTESIAN_POINT ( 'NONE',  ( -0.9055118110236215490, -0.6692913385826771977, 8.415575281601705876E-17 ) ) ;
#18119 = CARTESIAN_POINT ( 'NONE',  ( 1.036745406824147731, 0.05413385826771666132, 0.4176697321401328100 ) ) ;
#18120 = CARTESIAN_POINT ( 'NONE',  ( 1.141732283464567788, -0.6692913385826771977, 8.415575281601705876E-17 ) ) ;
#18121 = ADVANCED_FACE ( 'NONE', ( #74689 ), #16617, .T. ) ;
#18122 = CARTESIAN_POINT ( 'NONE',  ( -0.1070741851644051862, -0.3996062992125987146, -0.7020997375328084100 ) ) ;
#18123 = CARTESIAN_POINT ( 'NONE',  ( -1.220472440944881054, 0.2952755905511811885, 0.000000000000000000 ) ) ;
#18124 = CARTESIAN_POINT ( 'NONE',  ( -0.3996062992125985480, -7.340648628747423112E-17, -0.4311023622047244208 ) ) ;
#18125 = CARTESIAN_POINT ( 'NONE',  ( 0.2362204724409456558, -0.1870078740157480879, -0.4822834645669291653 ) ) ;
#18126 = CARTESIAN_POINT ( 'NONE',  ( 0.1998031496062994405, -0.3460692066303958092, -2.296587926509186417 ) ) ;
#18127 = CARTESIAN_POINT ( 'NONE',  ( -0.3917322834645670104, -7.196005306013484475E-17, -1.541338582677165503 ) ) ;
#18128 = CARTESIAN_POINT ( 'NONE',  ( 1.601049868766404982, -0.6046776061558809534, -0.2411417322834644161 ) ) ;
#18129 = CARTESIAN_POINT ( 'NONE',  ( 0.2952755905511819101, 0.07958543189024071263, -0.2665933059059888421 ) ) ;
#18130 = CARTESIAN_POINT ( 'NONE',  ( 0.8792650918635177559, -0.4281496062992127816, -0.4176697321401328100 ) ) ;
#18131 = CARTESIAN_POINT ( 'NONE',  ( -0.3458507752293909498, 0.3458507752293907833, -1.041338582677165281 ) ) ;
#18132 = CARTESIAN_POINT ( 'NONE',  ( 0.9317585301837276734, -0.004921259842519870586, -0.3153832671262229437 ) ) ;
#18133 = CARTESIAN_POINT ( 'NONE',  ( 0.4855643044619428750, 0.05413385826771666132, 0.4176697321401328100 ) ) ;
#18134 = CARTESIAN_POINT ( 'NONE',  ( 4.837279021331061486E-17, -0.3949938075777409963, -1.100393700787401619 ) ) ;
#18135 = CARTESIAN_POINT ( 'NONE',  ( -0.9711286089238838626, -0.6046776061558807314, 0.2411417322834647770 ) ) ;
#18136 = CARTESIAN_POINT ( 'NONE',  ( -0.1690661813110308498, 0.02791078216816347476, -0.4328096321851898631 ) ) ;
#18137 = AXIS2_PLACEMENT_3D ( 'NONE', #8195, #26289, #33024 ) ;
#18138 = CARTESIAN_POINT ( 'NONE',  ( 0.7742782152230978099, -0.3690944881889763329, 0.3153832671262228327 ) ) ;
#18139 = CARTESIAN_POINT ( 'NONE',  ( 0.1246719160104994284, 0.2066929133858267098, -0.1054918080437494132 ) ) ;
#18140 = CARTESIAN_POINT ( 'NONE',  ( -0.3477690288713905509, -0.6692913385826771977, 0.1292274648535927661 ) ) ;
#18141 = CARTESIAN_POINT ( 'NONE',  ( 0.3018372703412079971, -0.004921259842519870586, -0.3153832671262229437 ) ) ;
#18142 = CARTESIAN_POINT ( 'NONE',  ( -2.857004350179353391, 1.081388112195873497, 0.1351566381870255573 ) ) ;
#18143 = CARTESIAN_POINT ( 'NONE',  ( -0.1771653543307080136, -0.5400638737290844871, 0.3530559997133364547 ) ) ;
#18144 = CARTESIAN_POINT ( 'NONE',  ( 0.8989501312335963501, -0.5511811023622048555, -0.09757992244046775898 ) ) ;
#18145 = CARTESIAN_POINT ( 'NONE',  ( -1.113858370737681902, -4.850200619981615293E-15, -0.3791475997938227316 ) ) ;
#18146 = CARTESIAN_POINT ( 'NONE',  ( -9.787531504996566615E-17, 0.3996062992125985480, -1.651574803149606474 ) ) ;
#18147 = CARTESIAN_POINT ( 'NONE',  ( 0.1574803149606306130, -0.1870078740157480879, -0.4822834645669291653 ) ) ;
#18148 = ADVANCED_FACE ( 'NONE', ( #78628 ), #50715, .T. ) ;
#18149 = CARTESIAN_POINT ( 'NONE',  ( 1.095800524934383846, -0.08942795157528024563, -0.3641732283464568787 ) ) ;
#18150 = CARTESIAN_POINT ( 'NONE',  ( 0.1837270341207354329, 0.2306618581243848609, 0.2411417322834645549 ) ) ;
#18151 = CARTESIAN_POINT ( 'NONE',  ( -0.4921259842519677963, -0.4536011799217367080, 0.2665933059059888421 ) ) ;
#18152 = CIRCLE ( 'NONE', #7386, 3.543307086614174484 ) ;
#18153 = CARTESIAN_POINT ( 'NONE',  ( -0.6364829396325453192, -0.2845877964562159024, 0.3641732283464567677 ) ) ;
#18154 = CARTESIAN_POINT ( 'NONE',  ( -0.2034120734908128059, 0.2952755905511811885, 0.1292274648535926551 ) ) ;
#18155 = CARTESIAN_POINT ( 'NONE',  ( 0.1574803149606306130, -0.1870078740157479769, 0.4822834645669291653 ) ) ;
#18156 = CARTESIAN_POINT ( 'NONE',  ( 0.9514435695538062676, -0.2845877964562161244, -0.3641732283464567121 ) ) ;
#18157 = CARTESIAN_POINT ( 'NONE',  ( 1.374111566022513293E-16, 1.062992125984252745, -1.122047244094488194 ) ) ;
#18158 = CARTESIAN_POINT ( 'NONE',  ( 1.469816272965879911, 0.1283753931104746893, -0.1820866141732285504 ) ) ;
#18159 = EDGE_CURVE ( 'NONE', #27377, #33346, #63157, .T. ) ;
#18160 = CARTESIAN_POINT ( 'NONE',  ( 0.8070866141732289112, -0.5400638737290845981, -0.3530559997133363437 ) ) ;
#18161 = CARTESIAN_POINT ( 'NONE',  ( -1.603475055217291612, 1.819038169495759361, 0.04573490813648255215 ) ) ;
#18162 = CARTESIAN_POINT ( 'NONE',  ( -0.3871391076115479057, -0.3162353388693409650, -0.4822834645669289433 ) ) ;
#18163 = CARTESIAN_POINT ( 'NONE',  ( -0.1958661417322836718, 0.3392501089628017219, -1.042650918635170676 ) ) ;
#18164 = CARTESIAN_POINT ( 'NONE',  ( 0.9317585301837276734, 0.05413385826771626580, -0.4176697321401330321 ) ) ;
#18165 = CARTESIAN_POINT ( 'NONE',  ( 0.4068241469816281097, 0.05413385826771666132, 0.4176697321401328100 ) ) ;
#18166 = CARTESIAN_POINT ( 'NONE',  ( -0.4323334181381108254, 1.341458022389044658, -3.913202610827236860 ) ) ;
#18167 = CARTESIAN_POINT ( 'NONE',  ( 0.3674540682414705883, -0.5023911411419708095, 0.1820866141732285504 ) ) ;
#18168 = CARTESIAN_POINT ( 'NONE',  ( 1.010498687664042716, -0.4281496062992124485, 0.4176697321401328655 ) ) ;
#18169 = CARTESIAN_POINT ( 'NONE',  ( 0.07217847769028949700, -0.08942795157528024563, -0.3641732283464568787 ) ) ;
#18170 = CARTESIAN_POINT ( 'NONE',  ( -0.4658792650918627265, -0.3162353388693409650, -0.4822834645669289433 ) ) ;
#18171 = LINE ( 'NONE', #9473, #32670 ) ;
#18172 = CARTESIAN_POINT ( 'NONE',  ( 0.09842519685039434474, -0.5400638737290845981, -0.3530559997133363437 ) ) ;
#18173 = CARTESIAN_POINT ( 'NONE',  ( -0.8989501312335946848, -0.6692913385826771977, 0.1292274648535927661 ) ) ;
#18174 = CARTESIAN_POINT ( 'NONE',  ( -0.1181102362204717315, 0.1771653543307087630, 0.000000000000000000 ) ) ;
#18175 = CARTESIAN_POINT ( 'NONE',  ( 0.3083989501312343062, -0.3162353388693405765, 0.4822834645669290543 ) ) ;
#18176 = CARTESIAN_POINT ( 'NONE',  ( 1.076115485564305141, 0.1283753931104746893, -0.1820866141732285504 ) ) ;
#18177 = CARTESIAN_POINT ( 'NONE',  ( -0.3543307086614165824, 0.2952755905511811885, 0.000000000000000000 ) ) ;
#18178 = CARTESIAN_POINT ( 'NONE',  ( 1.161417322834646271, 0.1012011053420775880, -0.2882089793578257453 ) ) ;
#18180 = CARTESIAN_POINT ( 'NONE',  ( 1.227034120734908917, -0.6692913385826771977, 0.1292274648535927661 ) ) ;
#18179 = CARTESIAN_POINT ( 'NONE',  ( -0.3836918680457887532, -2.191421614605370878E-15, 0.4445507791589071167 ) ) ;
#18181 = CARTESIAN_POINT ( 'NONE',  ( -2.362204724409448620, 1.929133858267716661, -2.474278114140802984E-14 ) ) ;
#18182 = CARTESIAN_POINT ( 'NONE',  ( -0.1958661417322836718, 0.3392501089628017219, -2.052493438320210029 ) ) ;
#18183 = CARTESIAN_POINT ( 'NONE',  ( -1.332020997375327642, -0.05778040916215522460, 0.4822834645669289988 ) ) ;
#18184 = CARTESIAN_POINT ( 'NONE',  ( -0.9251968503937002541, 0.1660481256975885056, 0.3530559997133364547 ) ) ;
#18185 = CARTESIAN_POINT ( 'NONE',  ( 0.4091458600556403535, 0.2362204724409449896, -0.2887139107611548794 ) ) ;
#18186 = CARTESIAN_POINT ( 'NONE',  ( 0.3420746716998660508, -0.1974969037888703871, -2.782152230971128848 ) ) ;
#18187 = ORIENTED_EDGE ( 'NONE', *, *, #77172, .T. ) ;
#18188 = CARTESIAN_POINT ( 'NONE',  ( 0.4921259842519691285, -0.4536011799217368745, -0.2665933059059886201 ) ) ;
#18189 = CARTESIAN_POINT ( 'NONE',  ( 0.2867679344610365999, -0.2867679344610365444, -1.507874015748031260 ) ) ;
#18190 = CARTESIAN_POINT ( 'NONE',  ( 0.7217847769028878924, -0.4281496062992127816, -0.4176697321401328100 ) ) ;
#18191 = CARTESIAN_POINT ( 'NONE',  ( -0.2362204724409447953, -0.4091458600556404646, -2.270341207349081181 ) ) ;
#18192 = CARTESIAN_POINT ( 'NONE',  ( -0.03443470937339727228, 0.2755905511811023723, -1.417921404050779710 ) ) ;
#18193 = CARTESIAN_POINT ( 'NONE',  ( -0.4133858267716528645, -0.4536011799217367080, 0.2665933059059888421 ) ) ;
#18194 = CARTESIAN_POINT ( 'NONE',  ( 1.403614904275686858E-14, 1.537401574803149984, -3.937007874015761910 ) ) ;
#18195 = CARTESIAN_POINT ( 'NONE',  ( 1.056430446194226658, 0.2952755905511811885, 0.1292274648535926551 ) ) ;
#18196 = CARTESIAN_POINT ( 'NONE',  ( 1.548556430446194954, -0.5023911411419708095, 0.1820866141732285504 ) ) ;
#18197 = CARTESIAN_POINT ( 'NONE',  ( 0.08530183727034192087, -0.05778040916215522460, 0.4822834645669289988 ) ) ;
#18198 = CARTESIAN_POINT ( 'NONE',  ( 0.1958661417322834497, 0.3392501089628018329, -0.8543113928795783574 ) ) ;
#18199 = CARTESIAN_POINT ( 'NONE',  ( -0.5183727034120726440, 0.2952755905511811885, 0.1292274648535926551 ) ) ;
#18200 = CARTESIAN_POINT ( 'NONE',  ( -1.279527559055116948, -0.4536011799217367080, 0.2665933059059888421 ) ) ;
#18201 = CARTESIAN_POINT ( 'NONE',  ( -0.4068241469816267775, 0.05413385826771626580, -0.4176697321401330321 ) ) ;
#18202 = CARTESIAN_POINT ( 'NONE',  ( -0.09156050430092219083, -0.3808816823641230087, -1.492482962822815952E-17 ) ) ;
#18203 = CARTESIAN_POINT ( 'NONE',  ( -0.3335738234991588169, 1.199759523613727952, -1.973797438880085187 ) ) ;
#18204 = ORIENTED_EDGE ( 'NONE', *, *, #9628, .T. ) ;
#18205 = CARTESIAN_POINT ( 'NONE',  ( 0.2867679344610366554, 0.2867679344610366554, -2.181777845965566343 ) ) ;
#18206 = CARTESIAN_POINT ( 'NONE',  ( 0.3215223097112867578, -0.3162353388693409650, -0.4822834645669289433 ) ) ;
#18207 = ORIENTED_EDGE ( 'NONE', *, *, #82686, .F. ) ;
#18208 = VECTOR ( 'NONE', #29297, 39.37007874015748143 ) ;
#18209 = CARTESIAN_POINT ( 'NONE',  ( -0.5314960629921254842, -0.5400638737290845981, -0.3530559997133363437 ) ) ;
#18210 = CARTESIAN_POINT ( 'NONE',  ( -1.469816272965878357, 0.2306618581243848609, 0.2411417322834645549 ) ) ;
#18211 = CARTESIAN_POINT ( 'NONE',  ( 0.5839895013123367340, -0.6692913385826773087, -0.1292274648535924053 ) ) ;
#18212 = CARTESIAN_POINT ( 'NONE',  ( -0.1181102362204717315, -0.6692913385826771977, 8.415575281601705876E-17 ) ) ;
#18213 = CARTESIAN_POINT ( 'NONE',  ( 4.797336870675656522E-17, -0.3917322834645670104, -1.580708661417322913 ) ) ;
#18214 = CARTESIAN_POINT ( 'NONE',  ( -0.8989501312335946848, 0.2952755905511810774, -0.1292274648535930714 ) ) ;
#18215 = CARTESIAN_POINT ( 'NONE',  ( 0.4068241469816281097, 0.05413385826771666132, 0.4176697321401328100 ) ) ;
#18216 = CARTESIAN_POINT ( 'NONE',  ( -0.6167979002624665030, -0.4281496062992127816, -0.4176697321401328100 ) ) ;
#18217 = CARTESIAN_POINT ( 'NONE',  ( 0.4461942257217856311, 0.1283753931104746893, -0.1820866141732285504 ) ) ;
#18218 = CARTESIAN_POINT ( 'NONE',  ( -0.2952755905511810774, 1.832348042626885162E-19, 5.524802951929911998 ) ) ;
#18219 = CARTESIAN_POINT ( 'NONE',  ( -0.06561679790026180015, -0.4281496062992127816, -0.4176697321401328100 ) ) ;
#18220 = CARTESIAN_POINT ( 'NONE',  ( 0.000000000000000000, 2.716535433070866645, 0.000000000000000000 ) ) ;
#18221 = CARTESIAN_POINT ( 'NONE',  ( 1.594488188976378673, 0.1660481256975885056, 0.3530559997133364547 ) ) ;
#18222 = CARTESIAN_POINT ( 'NONE',  ( -0.3917322834645670104, -7.196005306013484475E-17, -2.866141732283464361 ) ) ;
#18223 = ORIENTED_EDGE ( 'NONE', *, *, #57314, .T. ) ;
#18224 = ORIENTED_EDGE ( 'NONE', *, *, #72350, .F. ) ;
#18225 = CARTESIAN_POINT ( 'NONE',  ( 0.9120734908136490793, 0.2952755905511810774, -0.1292274648535930714 ) ) ;
#18226 = CARTESIAN_POINT ( 'NONE',  ( 0.2493438320209980519, -0.3690944881889765550, -0.3153832671262227771 ) ) ;
#18228 = CYLINDRICAL_SURFACE ( 'NONE', #12908, 0.2952755905511810774 ) ;
#18227 = CARTESIAN_POINT ( 'NONE',  ( 0.000000000000000000, 2.165354330708661568, 0.000000000000000000 ) ) ;
#18229 = CARTESIAN_POINT ( 'NONE',  ( -0.2867679344610364334, -0.2867679344610367109, -1.246062992125984481 ) ) ;
#18230 = CARTESIAN_POINT ( 'NONE',  ( -0.1265901696524993347, 0.4724409448818895907, 0.07414698162729659037 ) ) ;
#18231 = CARTESIAN_POINT ( 'NONE',  ( 0.7205944486920661252, 7.754911898504981261E-16, 0.3627989612356142257 ) ) ;
#18232 = CARTESIAN_POINT ( 'NONE',  ( 0.1974969037888704704, 0.3420746716998660508, 0.09383202099737533719 ) ) ;
#18233 = CARTESIAN_POINT ( 'NONE',  ( 0.3608923884514443348, 0.2952755905511810774, -0.1292274648535930714 ) ) ;
#18234 = CARTESIAN_POINT ( 'NONE',  ( -1.227034120734907141, -0.6692913385826773087, -0.1292274648535924053 ) ) ;
#18235 = CARTESIAN_POINT ( 'NONE',  ( -1.272965879265091305, -0.4281496062992124485, 0.4176697321401328655 ) ) ;
#18236 = CARTESIAN_POINT ( 'NONE',  ( 0.4527559055118117182, -0.5400638737290844871, 0.3530559997133364547 ) ) ;
#18237 = CARTESIAN_POINT ( 'NONE',  ( 0.9055118110236227702, -0.6692913385826771977, 8.415575281601705876E-17 ) ) ;
#18238 = CARTESIAN_POINT ( 'NONE',  ( 1.561679790026247350, -0.004921259842519870586, -0.3153832671262229437 ) ) ;
#18239 = CARTESIAN_POINT ( 'NONE',  ( 1.325459317585302665, -0.3690944881889763329, 0.3153832671262228327 ) ) ;
#18240 = CARTESIAN_POINT ( 'NONE',  ( -0.8464566929133852113, 0.1660481256975885056, 0.3530559997133364547 ) ) ;
#18241 = CARTESIAN_POINT ( 'NONE',  ( 0.2925321140481932369, -0.2925321140481931814, -0.6476377952755905110 ) ) ;
#18242 = CARTESIAN_POINT ( 'NONE',  ( -1.601049868766403650, 0.1283753931104746893, -0.1820866141732285504 ) ) ;
#18243 = CARTESIAN_POINT ( 'NONE',  ( 0.2867679344610365999, -0.2867679344610365444, -0.4055118110236220486 ) ) ;
#18244 = CARTESIAN_POINT ( 'NONE',  ( -0.2165354330708654795, 0.1660481256975885056, 0.3530559997133364547 ) ) ;
#18246 = CARTESIAN_POINT ( 'NONE',  ( -0.4671901501889756392, 1.453473631083801676, 2.153053328784569231 ) ) ;
#18245 = CARTESIAN_POINT ( 'NONE',  ( 0.9514435695538062676, -0.3162353388693409650, -0.4822834645669289433 ) ) ;
#18247 = CARTESIAN_POINT ( 'NONE',  ( -1.463254593175852492, -0.5511811023622048555, -0.09757992244046775898 ) ) ;
#18248 = CARTESIAN_POINT ( 'NONE',  ( 0.03937007874015833325, -0.6692913385826771977, 8.415575281601705876E-17 ) ) ;
#18249 = CARTESIAN_POINT ( 'NONE',  ( 0.6955380577427828781, -0.004921259842519870586, -0.3153832671262229437 ) ) ;
#18250 = CARTESIAN_POINT ( 'NONE',  ( -1.601049868766403650, -0.5023911411419708095, 0.1820866141732285504 ) ) ;
#18251 = CARTESIAN_POINT ( 'NONE',  ( 1.089238845144357759, 0.05413385826771626580, -0.4176697321401330321 ) ) ;
#18252 = CARTESIAN_POINT ( 'NONE',  ( 0.000000000000000000, 0.000000000000000000, 0.000000000000000000 ) ) ;
#18253 = CARTESIAN_POINT ( 'NONE',  ( -0.4855643044619415427, -0.3690944881889763329, 0.3153832671262228327 ) ) ;
#18254 = CARTESIAN_POINT ( 'NONE',  ( -0.7152230971128602510, -0.05778040916215560624, -0.4822834645669293319 ) ) ;
#18255 = CARTESIAN_POINT ( 'NONE',  ( -1.594488188976377119, 0.07958543189024071263, -0.2665933059059888421 ) ) ;
#18256 = CARTESIAN_POINT ( 'NONE',  ( -1.141732283464566011, -0.6692913385826771977, 8.415575281601705876E-17 ) ) ;
#18257 = CARTESIAN_POINT ( 'NONE',  ( 1.207349081364829990, 0.2306618581243848609, 0.2411417322834645549 ) ) ;
#18258 = CARTESIAN_POINT ( 'NONE',  ( -0.1049643490035302301, -0.3917322834645671770, -1.013798843340894207 ) ) ;
#18259 = CARTESIAN_POINT ( 'NONE',  ( -1.312335958005248715, 0.1283753931104748280, 0.1820866141732283561 ) ) ;
#18260 = CARTESIAN_POINT ( 'NONE',  ( 1.016821367227983552, 1.505646504554443821, 0.4744094488188977388 ) ) ;
#18261 = CARTESIAN_POINT ( 'NONE',  ( 1.279527559055118724, 0.1660481256975885056, 0.3530559997133364547 ) ) ;
#18262 = CARTESIAN_POINT ( 'NONE',  ( 0.2362204724409451007, -0.4091458600556402980, -2.373359580052493367 ) ) ;
#18263 = AXIS2_PLACEMENT_3D ( 'NONE', #61598, #17002, #3944 ) ;
#18264 = CARTESIAN_POINT ( 'NONE',  ( -1.443569553805773564, -0.6046776061558807314, 0.2411417322834647770 ) ) ;
#18265 = CARTESIAN_POINT ( 'NONE',  ( -1.489501312335957062, -0.08942795157527998196, 0.3641732283464567121 ) ) ;
#18266 = CARTESIAN_POINT ( 'NONE',  ( -1.010498687664041384, -0.3690944881889765550, -0.3153832671262227771 ) ) ;
#18267 = EDGE_CURVE ( 'NONE', #60047, #35589, #67954, .T. ) ;
#18268 = FACE_OUTER_BOUND ( 'NONE', #83116, .T. ) ;
#18269 = CARTESIAN_POINT ( 'NONE',  ( -0.3018372703412066094, -0.4281496062992127816, -0.4176697321401328100 ) ) ;
#18270 = CARTESIAN_POINT ( 'NONE',  ( -0.01312335958005186876, -0.004921259842519870586, -0.3153832671262229437 ) ) ;
#18271 = CARTESIAN_POINT ( 'NONE',  ( -1.233595800524933894, 0.1283753931104748280, 0.1820866141732283561 ) ) ;
#18272 = CARTESIAN_POINT ( 'NONE',  ( 1.325459317585302665, -0.004921259842519870586, -0.3153832671262229437 ) ) ;
#18273 = CARTESIAN_POINT ( 'NONE',  ( 0.9580052493438327987, -0.4281496062992127816, -0.4176697321401328100 ) ) ;
#18274 = FACE_OUTER_BOUND ( 'NONE', #49544, .T. ) ;
#18275 = CARTESIAN_POINT ( 'NONE',  ( 0.08530183727034192087, -0.08942795157527998196, 0.3641732283464567121 ) ) ;
#18276 = CARTESIAN_POINT ( 'NONE',  ( 0.6102362204724416372, 0.1660481256975883668, -0.3530559997133364547 ) ) ;
#18277 = ADVANCED_FACE ( 'NONE', ( #47022 ), #62043, .F. ) ;
#18278 = CARTESIAN_POINT ( 'NONE',  ( 0.8727034120734912248, -0.2845877964562161244, -0.3641732283464567121 ) ) ;
#18279 = ORIENTED_EDGE ( 'NONE', *, *, #63984, .T. ) ;
#18280 = CARTESIAN_POINT ( 'NONE',  ( 1.482939632545932307, 0.05413385826771626580, -0.4176697321401330321 ) ) ;
#18281 = CARTESIAN_POINT ( 'NONE',  ( -1.377952755905511140, -0.6692913385826771977, 8.415575281601705876E-17 ) ) ;
#18282 = CARTESIAN_POINT ( 'NONE',  ( -0.1574803149606292529, -0.1870078740157479769, 0.4822834645669291653 ) ) ;
#18283 = CARTESIAN_POINT ( 'NONE',  ( 0.3460692066303959202, 0.1998031496062993295, -0.1312335958005249603 ) ) ;
#18284 = CARTESIAN_POINT ( 'NONE',  ( 0.2925321140481932369, -0.2925321140481931814, -2.694881889763780070 ) ) ;
#18285 = CARTESIAN_POINT ( 'NONE',  ( 0.5971128608923890191, -0.6692913385826771977, 0.1292274648535927661 ) ) ;
#18286 = CARTESIAN_POINT ( 'NONE',  ( 1.259842519685040019, -0.1870078740157479769, 0.3641732283464567677 ) ) ;
#18287 = CARTESIAN_POINT ( 'NONE',  ( 0.1115485564304470323, 0.2952755905511811885, 0.1292274648535926551 ) ) ;
#18288 = CARTESIAN_POINT ( 'NONE',  ( 0.3280839895013130669, 0.05413385826771666132, 0.4176697321401328100 ) ) ;
#18289 = CARTESIAN_POINT ( 'NONE',  ( -0.1998031496062991907, -0.3460692066303959757, -2.270341207349081181 ) ) ;
#18290 = CARTESIAN_POINT ( 'NONE',  ( 0.3949938075777411073, -0.1058382717557499464, -1.528871391076115804 ) ) ;
#18291 = CARTESIAN_POINT ( 'NONE',  ( -0.3996062992125986035, -7.340648628747425578E-17, -2.716535433070865757 ) ) ;
#18292 = CARTESIAN_POINT ( 'NONE',  ( 3.908320185825791881, 1.537401574803149984, 0.4744094488188975722 ) ) ;
#18293 = CARTESIAN_POINT ( 'NONE',  ( -0.2867679344610364334, -0.2867679344610367109, -0.6811023622047243098 ) ) ;
#18294 = CARTESIAN_POINT ( 'NONE',  ( -0.3280839895013117347, -0.3690944881889763329, 0.3153832671262228327 ) ) ;
#18295 = CARTESIAN_POINT ( 'NONE',  ( -0.6496062992125976043, -0.5400638737290844871, 0.3530559997133364547 ) ) ;
#18296 = CARTESIAN_POINT ( 'NONE',  ( -0.3949938075777409963, -7.255918531996591613E-17, -2.478346456692914312 ) ) ;
#18297 = EDGE_CURVE ( 'NONE', #80751, #30111, #74208, .T. ) ;
#18298 = CARTESIAN_POINT ( 'NONE',  ( 0.8858267716535438430, 0.1660481256975885056, 0.3530559997133364547 ) ) ;
#18299 = CARTESIAN_POINT ( 'NONE',  ( -1.456692913385826182, 0.2952755905511811885, 0.000000000000000000 ) ) ;
#18300 = CARTESIAN_POINT ( 'NONE',  ( 0.8005249343832027131, 0.05413385826771666132, 0.4176697321401328100 ) ) ;
#18301 = CARTESIAN_POINT ( 'NONE',  ( -0.4724409448818899238, 0.1265901696524986686, -2.709973753280840114 ) ) ;
#18302 = CARTESIAN_POINT ( 'NONE',  ( 0.1998031496062994405, -0.3460692066303958092, -2.139107611548556331 ) ) ;
#18303 = FACE_OUTER_BOUND ( 'NONE', #80659, .T. ) ;
#18304 = AXIS2_PLACEMENT_3D ( 'NONE', #24348, #50017, #31905 ) ;
#18305 = AXIS2_PLACEMENT_3D ( 'NONE', #5200, #57349, #76730 ) ;
#18306 = CARTESIAN_POINT ( 'NONE',  ( 0.7152230971128614723, -0.3162353388693409650, -0.4822834645669289433 ) ) ;
#18307 = CARTESIAN_POINT ( 'NONE',  ( 0.6496062992125991586, 0.1660481256975885056, 0.3530559997133364547 ) ) ;
#18308 = EDGE_CURVE ( 'NONE', #66895, #22673, #8740, .T. ) ;
#18309 = CARTESIAN_POINT ( 'NONE',  ( 1.332020997375328974, -0.08942795157528024563, -0.3641732283464568787 ) ) ;
#18310 = CARTESIAN_POINT ( 'NONE',  ( 1.312335958005250269, -0.6046776061558807314, 0.2411417322834647770 ) ) ;
#18311 = CARTESIAN_POINT ( 'NONE',  ( -0.2867679344610364334, -0.2867679344610367109, -0.3011811023622048000 ) ) ;
#18312 = CARTESIAN_POINT ( 'NONE',  ( 0.9514435695538062676, -0.3162353388693409650, -0.4822834645669289433 ) ) ;
#18313 = CARTESIAN_POINT ( 'NONE',  ( 1.437007874015748810, -0.4536011799217368745, -0.2665933059059886201 ) ) ;
#18314 = CARTESIAN_POINT ( 'NONE',  ( -0.3018372703412066094, 0.05413385826771666132, 0.4176697321401328100 ) ) ;
#18315 = CARTESIAN_POINT ( 'NONE',  ( -0.9055118110236215490, 0.2952755905511811885, 0.000000000000000000 ) ) ;
#18316 = CARTESIAN_POINT ( 'NONE',  ( 1.259842519685040019, -0.1870078740157479769, 0.4822834645669291653 ) ) ;
#18317 = CARTESIAN_POINT ( 'NONE',  ( 0.3392501089628018884, -0.1958661417322834220, -0.6620734908136483021 ) ) ;
#18318 = CARTESIAN_POINT ( 'NONE',  ( 0.2867679344610365999, 0.2867679344610365999, -1.547244094488189115 ) ) ;
#18319 = CARTESIAN_POINT ( 'NONE',  ( 0.2867679344610365999, 0.2867679344610365999, -2.649606299212598604 ) ) ;
#18320 = EDGE_CURVE ( 'NONE', #65211, #32057, #7731, .T. ) ;
#18321 = CARTESIAN_POINT ( 'NONE',  ( -1.522309711286088607, -0.5023911411419708095, 0.1820866141732285504 ) ) ;
#18322 = ORIENTED_EDGE ( 'NONE', *, *, #2729, .F. ) ;
#18323 = CARTESIAN_POINT ( 'NONE',  ( -0.2891555358219911054, 0.2891555358219909388, -2.539370078740157854 ) ) ;
#18324 = ORIENTED_EDGE ( 'NONE', *, *, #19808, .F. ) ;
#18325 = CARTESIAN_POINT ( 'NONE',  ( -0.3503937007874015630, 0.3733313776025731778, -0.01968503937007957602 ) ) ;
#18326 = CONICAL_SURFACE ( 'NONE', #19691, 2.362204724409449508, 0.8726646259971704289 ) ;
#18327 = CARTESIAN_POINT ( 'NONE',  ( 1.463254593175853824, 0.1771653543307087075, -0.09757992244046823083 ) ) ;
#18328 = CARTESIAN_POINT ( 'NONE',  ( -0.1998031496062991907, -0.3460692066303959757, -1.482939632545931863 ) ) ;
#18329 = CARTESIAN_POINT ( 'NONE',  ( 1.509186351706037543, -0.004921259842519576551, 0.3153832671262227771 ) ) ;
#18330 = CARTESIAN_POINT ( 'NONE',  ( 5.785732909357575061E-17, -0.4724409448818898682, -0.7854330708661416693 ) ) ;
#18331 = CARTESIAN_POINT ( 'NONE',  ( 0.2460629921259843422, 0.000000000000000000, 0.000000000000000000 ) ) ;
#18332 = DIRECTION ( 'NONE',  ( 0.000000000000000000, 1.000000000000000000, -0.000000000000000000 ) ) ;
#18333 = CARTESIAN_POINT ( 'NONE',  ( 4.797336870675656522E-17, -0.3917322834645670104, -0.3208661417322835607 ) ) ;
#18334 = CARTESIAN_POINT ( 'NONE',  ( -0.9251968503937002541, -0.4536011799217368745, -0.2665933059059886201 ) ) ;
#18335 = CARTESIAN_POINT ( 'NONE',  ( -1.194225721784776262, -0.004921259842519870586, -0.3153832671262229437 ) ) ;
#18336 = CARTESIAN_POINT ( 'NONE',  ( -1.082677165354329896, -0.5400638737290845981, -0.3530559997133363437 ) ) ;
#18337 = CARTESIAN_POINT ( 'NONE',  ( 0.2296587926509192634, -0.05778040916215560624, -0.4822834645669293319 ) ) ;
#18338 = CARTESIAN_POINT ( 'NONE',  ( 1.614173228346457378, 0.2952755905511811885, 0.000000000000000000 ) ) ;
#18339 = VERTEX_POINT ( 'NONE', #10297 ) ;
#18340 = CARTESIAN_POINT ( 'NONE',  ( 1.384514435695538337, -0.6692913385826771977, 0.1292274648535927661 ) ) ;
#18341 = CARTESIAN_POINT ( 'NONE',  ( -1.115485564304460997, 0.009842519685039147898, -0.3409548833797004797 ) ) ;
#18342 = DIRECTION ( 'NONE',  ( 0.000000000000000000, 0.000000000000000000, 1.000000000000000000 ) ) ;
#18343 = CARTESIAN_POINT ( 'NONE',  ( 0.1265901696524990294, -0.4724409448818896462, -2.132545931758530244 ) ) ;
#18344 = DIRECTION ( 'NONE',  ( -1.000000000000000000, -2.312964634635741971E-16, 0.000000000000000000 ) ) ;
#18345 = CARTESIAN_POINT ( 'NONE',  ( -0.5380577427821514602, -0.004921259842519576551, 0.3153832671262227771 ) ) ;
#18346 = CARTESIAN_POINT ( 'NONE',  ( -1.286089238845143479, 0.2306618581243847221, -0.2411417322834647770 ) ) ;
#18347 = CARTESIAN_POINT ( 'NONE',  ( 0.8464566929133866546, -0.5400638737290844871, 0.3530559997133364547 ) ) ;
#18348 = VERTEX_POINT ( 'NONE', #56947 ) ;
#18350 = CARTESIAN_POINT ( 'NONE',  ( 1.614173228346456712, 0.4410134679336843999, 0.1372047244094478646 ) ) ;
#18349 = CARTESIAN_POINT ( 'NONE',  ( -1.586052503253847057, 1.574803149606300412, -0.1653254495020572423 ) ) ;
#18351 = CARTESIAN_POINT ( 'NONE',  ( 1.548556430446194954, 0.2306618581243847221, -0.2411417322834647770 ) ) ;
#18352 = CARTESIAN_POINT ( 'NONE',  ( -1.423884514435694859, -0.3162353388693405765, 0.4822834645669290543 ) ) ;
#18353 = CARTESIAN_POINT ( 'NONE',  ( -0.3917322834645669549, -7.196005306013483243E-17, -0.2768835713572685431 ) ) ;
#18354 = CARTESIAN_POINT ( 'NONE',  ( -0.3740157480314953431, -0.4536011799217368745, -0.2665933059059886201 ) ) ;
#18355 = CARTESIAN_POINT ( 'NONE',  ( 4.797336870675656522E-17, -0.3917322834645670104, -0.7933070866141732624 ) ) ;
#18356 = CARTESIAN_POINT ( 'NONE',  ( -0.6561679790026240244, 0.1283753931104746893, -0.1820866141732285504 ) ) ;
#18357 = CARTESIAN_POINT ( 'NONE',  ( 0.4002624671916016896, -0.2845877964562161244, -0.3641732283464567121 ) ) ;
#18358 = CARTESIAN_POINT ( 'NONE',  ( 0.05905511811023681640, 0.1660481256975883668, -0.3530559997133364547 ) ) ;
#18359 = CARTESIAN_POINT ( 'NONE',  ( -0.8005249343832011588, -0.004921259842519870586, -0.3153832671262229437 ) ) ;
#18360 = CARTESIAN_POINT ( 'NONE',  ( -0.3917322834645669549, -0.1049643490035306603, -2.872703412073490448 ) ) ;
#18361 = CARTESIAN_POINT ( 'NONE',  ( 0.9776902887139113929, 0.2952755905511811885, 0.1292274648535926551 ) ) ;
#18362 = AXIS2_PLACEMENT_3D ( 'NONE', #68760, #45128, #69986 ) ;
#18363 = CARTESIAN_POINT ( 'NONE',  ( -0.9120734908136475250, -0.6692913385826773087, -0.1292274648535924053 ) ) ;
#18364 = CIRCLE ( 'NONE', #39875, 1.122047244094488194 ) ;
#18365 = CARTESIAN_POINT ( 'NONE',  ( 0.4724409448818898682, 2.892866454678787531E-17, -0.9822834645669291653 ) ) ;
#18366 = AXIS2_PLACEMENT_3D ( 'NONE', #46475, #26713, #52790 ) ;
#18367 = CARTESIAN_POINT ( 'NONE',  ( -0.5314960629921254842, -0.5400638737290845981, -0.3530559997133363437 ) ) ;
#18368 = EDGE_CURVE ( 'NONE', #46245, #76474, #29228, .T. ) ;
#18369 = CARTESIAN_POINT ( 'NONE',  ( -0.9973753280839886548, 0.2306618581243848609, 0.2411417322834645549 ) ) ;
#18370 = CARTESIAN_POINT ( 'NONE',  ( 1.253280839895013710, -0.08942795157528024563, -0.3641732283464568787 ) ) ;
#18371 = CARTESIAN_POINT ( 'NONE',  ( 0.2034120734908142214, 0.1771653543307087075, -0.09757992244046823083 ) ) ;
#18372 = CARTESIAN_POINT ( 'NONE',  ( -0.3937007874015740483, -0.1870078740157480879, -0.4822834645669291653 ) ) ;
#18373 = CARTESIAN_POINT ( 'NONE',  ( -1.115485564304461219, 0.05413385826771626580, -0.4176697321401330321 ) ) ;
#18374 = DIRECTION ( 'NONE',  ( 0.000000000000000000, -0.000000000000000000, 1.000000000000000000 ) ) ;
#18375 = CARTESIAN_POINT ( 'NONE',  ( 0.5314960629921395840, 2.559055118110236560, -3.900966923095588346 ) ) ;
#18376 = CARTESIAN_POINT ( 'NONE',  ( -0.3608923884514428360, 0.2952755905511811885, 0.1292274648535926551 ) ) ;
#18377 = CARTESIAN_POINT ( 'NONE',  ( -0.9383202099737524282, -0.05778040916215522460, 0.4822834645669289988 ) ) ;
#18378 = ORIENTED_EDGE ( 'NONE', *, *, #27425, .F. ) ;
#18379 = CARTESIAN_POINT ( 'NONE',  ( 0.3460692066303958092, 0.1998031496062993018, -1.782808398950131101 ) ) ;
#18380 = CARTESIAN_POINT ( 'NONE',  ( 1.227034120734908917, -0.6692913385826771977, 0.1292274648535927661 ) ) ;
#18381 = CARTESIAN_POINT ( 'NONE',  ( -0.7742782152230965886, -0.004921259842519576551, 0.3153832671262227771 ) ) ;
#18382 = CARTESIAN_POINT ( 'NONE',  ( -0.9908136482939626788, -0.6692913385826773087, -0.1292274648535924053 ) ) ;
#18383 = CARTESIAN_POINT ( 'NONE',  ( 1.115485564304462551, -0.4281496062992127816, -0.4176697321401328100 ) ) ;
#18384 = CARTESIAN_POINT ( 'NONE',  ( 0.7480314960629927956, 0.2952755905511811885, 0.000000000000000000 ) ) ;
#18385 = DIRECTION ( 'NONE',  ( 0.000000000000000000, -1.000000000000000000, 0.000000000000000000 ) ) ;
#18386 = CARTESIAN_POINT ( 'NONE',  ( -1.213910761154854745, 0.1771653543307087075, -0.09757992244046823083 ) ) ;
#18387 = CARTESIAN_POINT ( 'NONE',  ( 0.1070741851644053527, 0.3996062992125985480, -0.5426509186351704539 ) ) ;
#18388 = CARTESIAN_POINT ( 'NONE',  ( 0.1070741851644053527, 0.3996062992125986590, -1.095800524934382958 ) ) ;
#18389 = CARTESIAN_POINT ( 'NONE',  ( -0.1974969037888706647, 0.3420746716998658843, -0.3280839895013124563 ) ) ;
#18390 = CARTESIAN_POINT ( 'NONE',  ( 0.4122368018044499927, 1.300920202588029317, 2.666527984212822666 ) ) ;
#18391 = CARTESIAN_POINT ( 'NONE',  ( 1.213910761154856299, 0.1771653543307087630, 0.09757992244046791164 ) ) ;
#18392 = CARTESIAN_POINT ( 'NONE',  ( 0.7349081364829402885, -0.5023911411419708095, -0.1820866141732282451 ) ) ;
#18393 = CARTESIAN_POINT ( 'NONE',  ( 0.7217847769028878924, -0.4281496062992127816, -0.4176697321401328100 ) ) ;
#18394 = CARTESIAN_POINT ( 'NONE',  ( 0.2726377952755905665, -0.1133856558944469489, 0.1574803149606299191 ) ) ;
#18395 = CARTESIAN_POINT ( 'NONE',  ( 0.1058382717557499880, 0.3949938075777409408, -1.487532808398950523 ) ) ;
#18396 = CARTESIAN_POINT ( 'NONE',  ( 0.8136482939632553313, -0.5023911411419708095, -0.1820866141732282451 ) ) ;
#18397 = CARTESIAN_POINT ( 'NONE',  ( -0.1312335958005241554, -0.6046776061558809534, -0.2411417322834644161 ) ) ;
#18398 = CARTESIAN_POINT ( 'NONE',  ( -1.207349081364828436, -0.6046776061558807314, 0.2411417322834647770 ) ) ;
#18399 = CARTESIAN_POINT ( 'NONE',  ( 1.181102362204725198, -0.1870078740157479769, 0.4822834645669291653 ) ) ;
#18400 = CARTESIAN_POINT ( 'NONE',  ( -0.2362204724409447953, -0.4091458600556404646, -1.640419947506561726 ) ) ;
#18401 = CARTESIAN_POINT ( 'NONE',  ( -0.7414698162729651543, 0.2952755905511810219, -0.1292274648535930437 ) ) ;
#18402 = CARTESIAN_POINT ( 'NONE',  ( 0.07217847769028949700, -0.08942795157528024563, -0.3641732283464568787 ) ) ;
#18403 = ORIENTED_EDGE ( 'NONE', *, *, #25337, .T. ) ;
#18404 = ORIENTED_EDGE ( 'NONE', *, *, #20837, .T. ) ;
#18405 = CARTESIAN_POINT ( 'NONE',  ( -0.7152230971128602510, -0.05778040916215560624, -0.4822834645669293319 ) ) ;
#18406 = CARTESIAN_POINT ( 'NONE',  ( -0.5708661417322825615, -0.5400638737290844871, 0.3530559997133364547 ) ) ;
#18407 = CARTESIAN_POINT ( 'NONE',  ( -0.6889763779527552368, 0.1660481256975885056, 0.3530559997133364547 ) ) ;
#18408 = CARTESIAN_POINT ( 'NONE',  ( 0.4330708661417329575, 0.2952755905511811885, 0.000000000000000000 ) ) ;
#18409 = CARTESIAN_POINT ( 'NONE',  ( -0.4199475065616791736, -0.6046776061558807314, 0.2411417322834647770 ) ) ;
#18410 = CARTESIAN_POINT ( 'NONE',  ( -1.377952755905511140, -0.6692913385826771977, 8.415575281601705876E-17 ) ) ;
#18411 = CARTESIAN_POINT ( 'NONE',  ( -1.017060367454067249, -0.3162353388693409650, -0.4822834645669289433 ) ) ;
#18412 = CARTESIAN_POINT ( 'NONE',  ( 0.8989501312335963501, -0.6692913385826773087, -0.1292274648535924053 ) ) ;
#18413 = CARTESIAN_POINT ( 'NONE',  ( 0.1958661417322836440, -0.3392501089628017219, -1.343832020997375531 ) ) ;
#18414 = CARTESIAN_POINT ( 'NONE',  ( -0.3674540682414689785, 0.1283753931104748280, 0.1820866141732283561 ) ) ;
#18415 = VERTEX_POINT ( 'NONE', #11946 ) ;
#18416 = CARTESIAN_POINT ( 'NONE',  ( -0.3949938075777411628, 0.1058382717557497937, -1.607611548556430847 ) ) ;
#18417 = VECTOR ( 'NONE', #51331, 39.37007874015748143 ) ;
#18418 = ORIENTED_EDGE ( 'NONE', *, *, #10568, .F. ) ;
#18419 = CARTESIAN_POINT ( 'NONE',  ( -1.194225721784776262, -0.004921259842519870586, -0.3153832671262229437 ) ) ;
#18420 = VECTOR ( 'NONE', #75796, 39.37007874015748143 ) ;
#18421 = CARTESIAN_POINT ( 'NONE',  ( -1.187664041994749731, -0.3162353388693405765, 0.4822834645669290543 ) ) ;
#18422 = CARTESIAN_POINT ( 'NONE',  ( -1.056430446194224881, -0.6692913385826771977, 0.1292274648535927661 ) ) ;
#18423 = CARTESIAN_POINT ( 'NONE',  ( 0.1070741851644053527, 0.3996062992125986590, -0.1509186351706036655 ) ) ;
#18424 = CARTESIAN_POINT ( 'NONE',  ( -1.194225721784776262, 0.05413385826771626580, -0.4176697321401330321 ) ) ;
#18425 = CARTESIAN_POINT ( 'NONE',  ( -0.8727034120734901146, -0.05778040916215560624, -0.4822834645669293319 ) ) ;
#18426 = DIRECTION ( 'NONE',  ( -1.000000000000000000, -3.190296047773437643E-16, 0.000000000000000000 ) ) ;
#18427 = CARTESIAN_POINT ( 'NONE',  ( -1.692913385826770645, 0.2952755905511811885, 0.000000000000000000 ) ) ;
#18428 = CARTESIAN_POINT ( 'NONE',  ( 0.6824146981627303710, -0.5023911411419708095, 0.1820866141732285504 ) ) ;
#18429 = DIRECTION ( 'NONE',  ( 0.000000000000000000, 0.000000000000000000, -1.000000000000000000 ) ) ;
#18430 = CARTESIAN_POINT ( 'NONE',  ( -1.614173228346457378, 2.157411728916712068, 0.1372047244094476981 ) ) ;
#18431 = CARTESIAN_POINT ( 'NONE',  ( -0.1509186351706028884, -0.08942795157527998196, 0.3641732283464567121 ) ) ;
#18432 = CARTESIAN_POINT ( 'NONE',  ( -0.3018372703412066094, -0.4281496062992127816, -0.4176697321401328100 ) ) ;
#18433 = CARTESIAN_POINT ( 'NONE',  ( 1.305774278215223960, 0.2952755905511810774, -0.1292274648535930714 ) ) ;
#18434 = CARTESIAN_POINT ( 'NONE',  ( -0.6430446194225712953, 0.05413385826771626580, -0.4176697321401330321 ) ) ;
#18435 = ORIENTED_EDGE ( 'NONE', *, *, #32130, .T. ) ;
#18436 = CARTESIAN_POINT ( 'NONE',  ( -0.3460692066303958092, -0.1998031496062994683, -2.099737532808398921 ) ) ;
#18437 = CARTESIAN_POINT ( 'NONE',  ( -1.559171609364246924, 0.3937007874015748254, 0.7327394035119333404 ) ) ;
#18438 = ORIENTED_EDGE ( 'NONE', *, *, #75948, .F. ) ;
#18439 = CARTESIAN_POINT ( 'NONE',  ( 0.3460692066303959202, -0.1998031496062991630, -1.441601049868766582 ) ) ;
#18440 = CARTESIAN_POINT ( 'NONE',  ( 1.148293963254593653, 0.2952755905511810774, -0.1292274648535930714 ) ) ;
#18441 = CARTESIAN_POINT ( 'NONE',  ( -1.056430446194224881, 0.1771653543307087075, -0.09757992244046823083 ) ) ;
#18442 = CARTESIAN_POINT ( 'NONE',  ( -1.397637795275589623, 0.1660481256975885056, 0.3530559997133364547 ) ) ;
#18443 = CARTESIAN_POINT ( 'NONE',  ( -0.4724409448818898682, -8.678599364036362592E-17, -0.8267716535433070613 ) ) ;
#18444 = PLANE ( 'NONE',  #51938 ) ;
#18445 = CARTESIAN_POINT ( 'NONE',  ( -0.3917322834645669549, -0.1049643490035306603, -2.807742782152229832 ) ) ;
#18446 = CARTESIAN_POINT ( 'NONE',  ( 1.404199475065617708, 0.05413385826771626580, -0.4176697321401330321 ) ) ;
#18447 = CYLINDRICAL_SURFACE ( 'NONE', #950, 0.4744094488188972947 ) ;
#18448 = CARTESIAN_POINT ( 'NONE',  ( 0.1377952755905518800, 0.1660481256975883668, -0.3530559997133364547 ) ) ;
#18449 = CARTESIAN_POINT ( 'NONE',  ( -0.9580052493438311334, -0.004921259842519870586, -0.3153832671262229437 ) ) ;
#18450 = CARTESIAN_POINT ( 'NONE',  ( -0.3346456692913377662, -0.5400638737290844871, 0.3530559997133364547 ) ) ;
#18451 = CARTESIAN_POINT ( 'NONE',  ( -1.157146581871515012E-16, 0.4724409448818898682, -2.596456692913385655 ) ) ;
#18452 = CARTESIAN_POINT ( 'NONE',  ( -0.6692913385826764205, -0.6692913385826771977, 8.415575281601705876E-17 ) ) ;
#18453 = CARTESIAN_POINT ( 'NONE',  ( -0.3420746716998660508, -0.1974969037888706924, -2.176509186351706759 ) ) ;
#18454 = CARTESIAN_POINT ( 'NONE',  ( 1.240157480314961314, -0.4536011799217367080, 0.2665933059059888421 ) ) ;
#18455 = CARTESIAN_POINT ( 'NONE',  ( -0.2624671916010490880, 0.1283753931104746893, -0.1820866141732285504 ) ) ;
#18456 = CARTESIAN_POINT ( 'NONE',  ( 0.7020997375328090762, -0.2845877964562159024, 0.3641732283464567677 ) ) ;
#18457 = CARTESIAN_POINT ( 'NONE',  ( -1.489501312335957062, -0.3162353388693409650, -0.4822834645669289433 ) ) ;
#18458 = CARTESIAN_POINT ( 'NONE',  ( 0.1265901696524990572, -0.4724409448818897017, -2.209317585301837195 ) ) ;
#18459 = CARTESIAN_POINT ( 'NONE',  ( 0.5905511811023629321, 0.1771653543307087630, 0.000000000000000000 ) ) ;
#18460 = CARTESIAN_POINT ( 'NONE',  ( -0.8858267716535425107, -0.5400638737290844871, 0.3530559997133364547 ) ) ;
#18461 = CARTESIAN_POINT ( 'NONE',  ( 1.089942661822472569, 9.906153642143428645E-17, -0.3464511005275205946 ) ) ;
#18462 = CARTESIAN_POINT ( 'NONE',  ( 0.006561679790026889343, -0.2845877964562161244, -0.3641732283464567121 ) ) ;
#18463 = CARTESIAN_POINT ( 'NONE',  ( -1.673228346456691717, 0.07958543189024071263, -0.2665933059059888421 ) ) ;
#18464 = EDGE_CURVE ( 'NONE', #21784, #38952, #31993, .T. ) ;
#18465 = CARTESIAN_POINT ( 'NONE',  ( 0.7283464566929143125, 0.1660481256975885056, 0.3530559997133364547 ) ) ;
#18466 = FACE_OUTER_BOUND ( 'NONE', #10958, .T. ) ;
#18467 = CARTESIAN_POINT ( 'NONE',  ( 1.548556430446194954, -0.5023911411419708095, 0.1820866141732285504 ) ) ;
#18468 = CARTESIAN_POINT ( 'NONE',  ( -1.220472440944881054, 0.2952755905511811885, 0.000000000000000000 ) ) ;
#18469 = CARTESIAN_POINT ( 'NONE',  ( -0.1246719160104980823, -0.5511811023622048555, -0.09757992244046775898 ) ) ;
#18470 = CARTESIAN_POINT ( 'NONE',  ( -1.614173228346456712, 0.9921945702958917535, -0.1372047244094478091 ) ) ;
#18471 = CARTESIAN_POINT ( 'NONE',  ( 0.2559055118110243332, -0.4536011799217368745, -0.2665933059059886201 ) ) ;
#18472 = CARTESIAN_POINT ( 'NONE',  ( -1.364829396325458521, 0.2306618581243847221, -0.2411417322834647770 ) ) ;
#18473 = CARTESIAN_POINT ( 'NONE',  ( -0.6758530183727028406, 0.2952755905511811885, 0.1292274648535926551 ) ) ;
#18474 = CARTESIAN_POINT ( 'NONE',  ( -0.3996062992125986590, 0.1070741851644051723, -0.8969816272965877024 ) ) ;
#18475 = VECTOR ( 'NONE', #10712, 39.37007874015748143 ) ;
#18476 = CARTESIAN_POINT ( 'NONE',  ( -0.1049643490035302024, -0.3917322834645671215, -2.361548556430446144 ) ) ;
#18477 = CARTESIAN_POINT ( 'NONE',  ( 0.4199475065616803948, -0.5023911411419708095, -0.1820866141732282451 ) ) ;
#18478 = CARTESIAN_POINT ( 'NONE',  ( -0.5249343832020990641, 0.2306618581243848609, 0.2411417322834645549 ) ) ;
#18479 = CARTESIAN_POINT ( 'NONE',  ( -0.9055118110236215490, -0.6692913385826771977, 8.415575281601705876E-17 ) ) ;
#18480 = CARTESIAN_POINT ( 'NONE',  ( -0.9580052493438311334, -0.004921259842519870586, -0.3153832671262229437 ) ) ;
#18481 = CARTESIAN_POINT ( 'NONE',  ( -3.923618555848779721, 1.191084733186814848, -0.3246066631975622618 ) ) ;
#18482 = CARTESIAN_POINT ( 'NONE',  ( 0.03280839895013198948, -0.6692913385826773087, -0.1292274648535924053 ) ) ;
#18483 = CARTESIAN_POINT ( 'NONE',  ( -1.555118110236219930, 0.07958543189024085140, 0.2665933059059887866 ) ) ;
#18484 = CARTESIAN_POINT ( 'NONE',  ( 1.555118110236221041, -0.5400638737290844871, 0.3530559997133364547 ) ) ;
#18485 = FACE_OUTER_BOUND ( 'NONE', #4399, .T. ) ;
#18486 = EDGE_LOOP ( 'NONE', ( #76033, #45701, #481, #9692 ) ) ;
#18487 = DIRECTION ( 'NONE',  ( -5.329070518200751394E-15, 0.000000000000000000, -1.000000000000000000 ) ) ;
#18488 = CARTESIAN_POINT ( 'NONE',  ( -1.528871391076114250, 0.2952755905511810774, -0.1292274648535930714 ) ) ;
#18489 = CARTESIAN_POINT ( 'NONE',  ( -0.8005249343832013809, -0.4281496062992124485, 0.4176697321401328655 ) ) ;
#18490 = CARTESIAN_POINT ( 'NONE',  ( 1.496062992125984703, -0.1870078740157480879, -0.4822834645669291653 ) ) ;
#18491 = CARTESIAN_POINT ( 'NONE',  ( 0.3392501089628018329, 0.1958661417322835607, -1.948162729658792891 ) ) ;
#18492 = CARTESIAN_POINT ( 'NONE',  ( -0.3527845929029426175, 0.1716039559346188292, -1.220472440944881720 ) ) ;
#18493 = CARTESIAN_POINT ( 'NONE',  ( 0.7545931758530189937, 0.2952755905511810774, -0.1292274648535930714 ) ) ;
#18494 = CARTESIAN_POINT ( 'NONE',  ( 0.1837270341207357105, -0.6046776061558809534, -0.2411417322834644161 ) ) ;
#18495 = LINE ( 'NONE', #50050, #71805 ) ;
#18496 = FACE_OUTER_BOUND ( 'NONE', #47706, .T. ) ;
#18497 = CARTESIAN_POINT ( 'NONE',  ( 1.167979002624672580, -0.004921259842519870586, -0.3153832671262229437 ) ) ;
#18498 = CARTESIAN_POINT ( 'NONE',  ( -0.1998031496062991907, -0.3460692066303959757, -0.8530183727034120755 ) ) ;
#18499 = ORIENTED_EDGE ( 'NONE', *, *, #12912, .F. ) ;
#18500 = CARTESIAN_POINT ( 'NONE',  ( 0.2867679344610365999, -0.2867679344610365444, -2.767716535433069946 ) ) ;
#18501 = ORIENTED_EDGE ( 'NONE', *, *, #29024, .F. ) ;
#18502 = CARTESIAN_POINT ( 'NONE',  ( 0.2952755905511816326, -0.5400638737290844871, 0.3530559997133364547 ) ) ;
#18503 = CARTESIAN_POINT ( 'NONE',  ( -0.7217847769028863381, 0.05413385826771626580, -0.4176697321401330321 ) ) ;
#18504 = CARTESIAN_POINT ( 'NONE',  ( 1.594488188976378673, 0.1660481256975885056, 0.3530559997133364547 ) ) ;
#18505 = CARTESIAN_POINT ( 'NONE',  ( 0.6102362204724416372, 0.1660481256975883668, -0.3530559997133364547 ) ) ;
#18506 = CARTESIAN_POINT ( 'NONE',  ( 1.469816272965879911, -0.6046776061558807314, 0.2411417322834647770 ) ) ;
#18507 = CARTESIAN_POINT ( 'NONE',  ( 1.607611548556431069, 0.2952755905511811885, 0.1292274648535926551 ) ) ;
#18508 = CARTESIAN_POINT ( 'NONE',  ( 0.04593175853018440641, -0.6692913385826771977, 0.1292274648535927661 ) ) ;
#18509 = CARTESIAN_POINT ( 'NONE',  ( -1.213910761154854745, -0.6692913385826771977, 0.1292274648535927661 ) ) ;
#18510 = CARTESIAN_POINT ( 'NONE',  ( 1.607611548556431069, 0.2952755905511811885, 0.1292274648535926551 ) ) ;
#18511 = FACE_OUTER_BOUND ( 'NONE', #14521, .T. ) ;
#18512 = CARTESIAN_POINT ( 'NONE',  ( -0.2867679344610364334, -0.2867679344610367109, -0.2086614173228345248 ) ) ;
#18513 = CARTESIAN_POINT ( 'NONE',  ( 1.023622047244095334, -0.1870078740157479769, 0.3641732283464567677 ) ) ;
#18514 = ORIENTED_EDGE ( 'NONE', *, *, #63922, .T. ) ;
#18515 = CARTESIAN_POINT ( 'NONE',  ( -0.2891555358219911054, 0.2891555358219909388, -0.1771653543307087630 ) ) ;
#18516 = ORIENTED_EDGE ( 'NONE', *, *, #45608, .F. ) ;
#18517 = CARTESIAN_POINT ( 'NONE',  ( 0.1509186351706042484, -0.2845877964562159024, 0.3641732283464567677 ) ) ;
#18518 = FACE_OUTER_BOUND ( 'NONE', #73790, .T. ) ;
#18519 = CARTESIAN_POINT ( 'NONE',  ( 0.6364829396325465405, -0.05778040916215522460, 0.4822834645669289988 ) ) ;
#18520 = CARTESIAN_POINT ( 'NONE',  ( 0.2230971128608929543, 0.05413385826771626580, -0.4176697321401330321 ) ) ;
#18521 = CARTESIAN_POINT ( 'NONE',  ( -0.6102362204724400829, 0.1660481256975885056, 0.3530559997133364547 ) ) ;
#18522 = CARTESIAN_POINT ( 'NONE',  ( 0.2867679344610366554, -0.2867679344610365999, -1.827447137304149205 ) ) ;
#18523 = CARTESIAN_POINT ( 'NONE',  ( -1.233595800524933894, -0.6046776061558809534, -0.2411417322834644161 ) ) ;
#18524 = CARTESIAN_POINT ( 'NONE',  ( 0.1049643490035304938, -0.3917322834645669549, -2.689632545931758489 ) ) ;
#18525 = CARTESIAN_POINT ( 'NONE',  ( 1.456692913385827515, 0.1771653543307087630, 0.000000000000000000 ) ) ;
#18526 = CARTESIAN_POINT ( 'NONE',  ( -1.351706036745406347, -0.4281496062992124485, 0.4176697321401328655 ) ) ;
#18527 = CARTESIAN_POINT ( 'NONE',  ( 0.9973753280839902091, -0.6046776061558807314, 0.2411417322834647770 ) ) ;
#18528 = CARTESIAN_POINT ( 'NONE',  ( 1.318897637795276356, -0.5400638737290844871, 0.3530559997133364547 ) ) ;
#18529 = CARTESIAN_POINT ( 'NONE',  ( 0.1070741851644054915, -0.3996062992125986035, -0.7152230971128609172 ) ) ;
#18530 = CARTESIAN_POINT ( 'NONE',  ( -1.174540682414697335, -0.3162353388693409650, -0.4822834645669289433 ) ) ;
#18531 = CARTESIAN_POINT ( 'NONE',  ( -0.3996062992125984925, -0.1070741851644056858, -0.2801837270341207553 ) ) ;
#18532 = CARTESIAN_POINT ( 'NONE',  ( 0.2925321140481932369, -0.2925321140481931814, -0.1751968503937008370 ) ) ;
#18533 = CARTESIAN_POINT ( 'NONE',  ( -0.03937007874015669567, -0.6692913385826771977, 8.415575281601705876E-17 ) ) ;
#18534 = CARTESIAN_POINT ( 'NONE',  ( 4.893765752498283924E-17, -0.3996062992125986035, -2.755905511811023612 ) ) ;
#18535 = CARTESIAN_POINT ( 'NONE',  ( 0.2867679344610365999, -0.2867679344610365444, -1.757874015748031260 ) ) ;
#18536 = VECTOR ( 'NONE', #60196, 39.37007874015748143 ) ;
#18537 = CARTESIAN_POINT ( 'NONE',  ( 1.555118110236221041, 0.1660481256975883668, -0.3530559997133364547 ) ) ;
#18538 = CARTESIAN_POINT ( 'NONE',  ( 0.03937007874015833325, -0.5511811023622047445, 6.969142054262312111E-17 ) ) ;
#18539 = CARTESIAN_POINT ( 'NONE',  ( 1.076115485564305141, -0.6046776061558807314, 0.2411417322834647770 ) ) ;
#18540 = CARTESIAN_POINT ( 'NONE',  ( -0.4724409448818899238, 0.1265901696524986686, -1.684383202099737353 ) ) ;
#18541 = CARTESIAN_POINT ( 'NONE',  ( 0.1640419947506569498, -0.2845877964562161244, -0.3641732283464567121 ) ) ;
#18542 = CARTESIAN_POINT ( 'NONE',  ( 0.4330708661417329575, -0.6692913385826771977, 8.415575281601705876E-17 ) ) ;
#18543 = CARTESIAN_POINT ( 'NONE',  ( 0.1058382717557499880, 0.3949938075777409408, -1.015091863517060489 ) ) ;
#18544 = CARTESIAN_POINT ( 'NONE',  ( -0.8070866141732276899, -0.5400638737290844871, 0.3530559997133364547 ) ) ;
#18545 = CARTESIAN_POINT ( 'NONE',  ( -0.1837270341207340729, 0.2306618581243847221, -0.2411417322834647770 ) ) ;
#18546 = CARTESIAN_POINT ( 'NONE',  ( 0.7414698162729663755, -0.5511811023622048555, -0.09757992244046775898 ) ) ;
#18547 = CARTESIAN_POINT ( 'NONE',  ( -0.2821522309711278487, 0.2952755905511811885, 0.1292274648535926551 ) ) ;
#18548 = CARTESIAN_POINT ( 'NONE',  ( 0.1377952755905518800, 0.07958543189024071263, -0.2665933059059888421 ) ) ;
#18549 = CARTESIAN_POINT ( 'NONE',  ( -2.723802780027896553, 1.230840736494979604, -0.3632157284009264187 ) ) ;
#18550 = CARTESIAN_POINT ( 'NONE',  ( -0.2165354330708654795, -0.5400638737290845981, -0.3530559997133363437 ) ) ;
#18551 = CARTESIAN_POINT ( 'NONE',  ( 0.3346456692913390985, 0.07958543189024085140, 0.2665933059059887866 ) ) ;
#18552 = CARTESIAN_POINT ( 'NONE',  ( 0.1070741851644054776, -0.3996062992125984925, -1.579396325459317740 ) ) ;
#18553 = CARTESIAN_POINT ( 'NONE',  ( 0.4068241469816281097, 0.05413385826771666132, 0.4176697321401328100 ) ) ;
#18554 = EDGE_CURVE ( 'NONE', #28061, #73460, #39994, .T. ) ;
#18555 = CARTESIAN_POINT ( 'NONE',  ( 1.049868766404200349, 0.1283753931104748280, 0.1820866141732283561 ) ) ;
#18556 = CARTESIAN_POINT ( 'NONE',  ( -0.1678194419220245537, 3.103433371374072050E-15, -0.4281989832122387041 ) ) ;
#18557 = CARTESIAN_POINT ( 'NONE',  ( -0.5511811023622041894, -0.1870078740157480601, -0.3641732283464567677 ) ) ;
#18558 = CARTESIAN_POINT ( 'NONE',  ( -0.8267716535433065062, -0.5511811023622047445, 6.969142054262312111E-17 ) ) ;
#18559 = CARTESIAN_POINT ( 'NONE',  ( -0.4330708661417315697, -0.6692913385826771977, 8.415575281601705876E-17 ) ) ;
#18560 = EDGE_CURVE ( 'NONE', #6101, #48718, #18665, .T. ) ;
#18561 = CARTESIAN_POINT ( 'NONE',  ( 0.2952755905511816326, -0.5400638737290844871, 0.3530559997133364547 ) ) ;
#18562 = CARTESIAN_POINT ( 'NONE',  ( 1.095800524934383846, -0.08942795157528024563, -0.3641732283464568787 ) ) ;
#18563 = DIRECTION ( 'NONE',  ( 0.000000000000000000, 0.000000000000000000, -1.000000000000000000 ) ) ;
#18564 = CARTESIAN_POINT ( 'NONE',  ( 1.377952755905512472, -0.5511811023622047445, 6.969142054262312111E-17 ) ) ;
#18565 = CARTESIAN_POINT ( 'NONE',  ( 0.6627296587926517768, -0.6692913385826773087, -0.1292274648535924053 ) ) ;
#18566 = CARTESIAN_POINT ( 'NONE',  ( -1.586052503253846169, 1.850393700787402729, -0.1653254495020583803 ) ) ;
#18567 = CARTESIAN_POINT ( 'NONE',  ( -0.07217847769028813698, -0.3162353388693409650, -0.4822834645669289433 ) ) ;
#18568 = CARTESIAN_POINT ( 'NONE',  ( -0.1958661417322836718, 0.3392501089628017219, -1.200131233595800540 ) ) ;
#18569 = CARTESIAN_POINT ( 'NONE',  ( 0.9186351706036752773, 0.2306618581243847221, -0.2411417322834647770 ) ) ;
#18570 = CARTESIAN_POINT ( 'NONE',  ( 0.5774278215223104249, 0.2306618581243848609, 0.2411417322834645549 ) ) ;
#18571 = DIRECTION ( 'NONE',  ( 1.000000000000000000, 0.000000000000000000, -0.000000000000000000 ) ) ;
#18572 = CARTESIAN_POINT ( 'NONE',  ( 0.3740157480314966754, -0.4536011799217367080, 0.2665933059059888421 ) ) ;
#18573 = CARTESIAN_POINT ( 'NONE',  ( 1.154855643044620184, -0.6046776061558807314, 0.2411417322834647770 ) ) ;
#18574 = CARTESIAN_POINT ( 'NONE',  ( -0.4396325459317579898, 0.1771653543307087630, 0.09757992244046791164 ) ) ;
#18575 = CARTESIAN_POINT ( 'NONE',  ( -0.5052493438320203589, 0.2952755905511810774, -0.1292274648535930714 ) ) ;
#18576 = CARTESIAN_POINT ( 'NONE',  ( 0.000000000000000000, 1.724409448818900570, 2.362204724409448620 ) ) ;
#18577 = CARTESIAN_POINT ( 'NONE',  ( 0.2165354330708668673, 0.1660481256975883668, -0.3530559997133364547 ) ) ;
#18578 = CARTESIAN_POINT ( 'NONE',  ( -0.7545931758530176614, -0.6692913385826773087, -0.1292274648535924053 ) ) ;
#18579 = CARTESIAN_POINT ( 'NONE',  ( -0.8070866141732276899, -0.4536011799217367080, 0.2665933059059888421 ) ) ;
#18580 = CARTESIAN_POINT ( 'NONE',  ( 0.5118110236220478892, 0.2952755905511811885, 0.000000000000000000 ) ) ;
#18581 = CARTESIAN_POINT ( 'NONE',  ( -1.292650918635170010, -0.6692913385826771977, 0.1292274648535927661 ) ) ;
#18582 = CARTESIAN_POINT ( 'NONE',  ( -0.5314960629921250401, 0.1660481256975885056, 0.3530559997133364547 ) ) ;
#18583 = CARTESIAN_POINT ( 'NONE',  ( 0.4724409448818898682, 2.892866454678787531E-17, -0.5905511811023621549 ) ) ;
#18585 = CARTESIAN_POINT ( 'NONE',  ( 1.489501312335958172, -0.05778040916215560624, -0.4822834645669293319 ) ) ;
#18584 = FACE_OUTER_BOUND ( 'NONE', #69127, .T. ) ;
#18586 = CARTESIAN_POINT ( 'NONE',  ( -0.3149606299212633354, 2.165354330708661568, 1.076935383196057305 ) ) ;
#18587 = B_SPLINE_CURVE_WITH_KNOTS ( 'NONE', 3,
 ( #15684, #35857, #9355, #10604, #74995, #23623, #62337 ),
 .UNSPECIFIED., .F., .F.,
 ( 4, 3, 4 ),
 ( 0.000000000000000000, 0.001246232571205245976, 0.002492492258783242029 ),
 .UNSPECIFIED. ) ;
#18588 = VECTOR ( 'NONE', #27915, 39.37007874015748143 ) ;
#18589 = CARTESIAN_POINT ( 'NONE',  ( -1.469816272965878357, 0.2306618581243848609, 0.2411417322834645549 ) ) ;
#18590 = CARTESIAN_POINT ( 'NONE',  ( -0.9186351706036736120, 0.2306618581243848609, 0.2411417322834645549 ) ) ;
#18591 = CARTESIAN_POINT ( 'NONE',  ( -0.2362204724409447953, -0.4091458600556404646, -0.2230971128608923715 ) ) ;
#18592 = CARTESIAN_POINT ( 'NONE',  ( -0.3949938075777409963, -7.255918531996591613E-17, -2.716535433070866201 ) ) ;
#18593 = VERTEX_POINT ( 'NONE', #25376 ) ;
#18594 = CARTESIAN_POINT ( 'NONE',  ( 0.4986876640419954376, -0.5023911411419708095, -0.1820866141732282451 ) ) ;
#18595 = CARTESIAN_POINT ( 'NONE',  ( 0.3917322834645669549, 0.1049643490035304660, -1.376640419947506189 ) ) ;
#18596 = CARTESIAN_POINT ( 'NONE',  ( 0.6496062992125991586, 0.1660481256975885056, 0.3530559997133364547 ) ) ;
#18597 = CARTESIAN_POINT ( 'NONE',  ( 0.4724409448818898682, 2.892866454678787531E-17, -2.795275590551181022 ) ) ;
#18598 = CARTESIAN_POINT ( 'NONE',  ( 0.3149606299212737159, 2.165354330708661568, -3.937007874015761022 ) ) ;
#18599 = CARTESIAN_POINT ( 'NONE',  ( -0.5183727034120726440, 0.1771653543307087630, 0.09757992244046791164 ) ) ;
#18600 = CARTESIAN_POINT ( 'NONE',  ( 0.5314960629921371416, 2.742783277647743212, -3.197598474799420831 ) ) ;
#18601 = CARTESIAN_POINT ( 'NONE',  ( 1.102362204724410155, -0.1870078740157480879, -0.4822834645669291653 ) ) ;
#18602 = CARTESIAN_POINT ( 'NONE',  ( 0.7742782152230978099, -0.3690944881889763329, 0.3153832671262228327 ) ) ;
#18603 = CARTESIAN_POINT ( 'NONE',  ( -0.05905511811023545637, 0.1660481256975885056, 0.3530559997133364547 ) ) ;
#18604 = CARTESIAN_POINT ( 'NONE',  ( -0.3917322834645669549, -7.196005306013483243E-17, -0.5918442012785283257 ) ) ;
#18605 = CARTESIAN_POINT ( 'NONE',  ( -0.2887139107611542133, -0.6046776061558809534, -0.2411417322834644161 ) ) ;
#18606 = CARTESIAN_POINT ( 'NONE',  ( -1.384514435695537005, 0.1771653543307087630, 0.09757992244046791164 ) ) ;
#18607 = CARTESIAN_POINT ( 'NONE',  ( -0.5052493438320203589, -0.6692913385826771977, 0.1292274648535927661 ) ) ;
#18608 = DIRECTION ( 'NONE',  ( 1.000000000000000000, -0.000000000000000000, -0.000000000000000000 ) ) ;
#18609 = CARTESIAN_POINT ( 'NONE',  ( -0.1180926326102824109, 1.077616795999335242, -1.863921337943197365 ) ) ;
#18610 = ORIENTED_EDGE ( 'NONE', *, *, #71325, .T. ) ;
#18611 = CARTESIAN_POINT ( 'NONE',  ( -0.3917322834645671770, 0.1049643490035302024, -2.234271284285776371 ) ) ;
#18612 = CARTESIAN_POINT ( 'NONE',  ( 0.4330708661417329575, 0.2952755905511811885, 0.000000000000000000 ) ) ;
#18613 = ORIENTED_EDGE ( 'NONE', *, *, #11964, .T. ) ;
#18614 = CARTESIAN_POINT ( 'NONE',  ( -0.9383202099737524282, -0.05778040916215522460, 0.4822834645669289988 ) ) ;
#18615 = CARTESIAN_POINT ( 'NONE',  ( -1.555118110236219930, -0.5400638737290845981, -0.3530559997133363437 ) ) ;
#18616 = CARTESIAN_POINT ( 'NONE',  ( 0.5249343832021003964, 0.2306618581243847221, -0.2411417322834647770 ) ) ;
#18617 = CARTESIAN_POINT ( 'NONE',  ( -0.04593175853018302557, 0.2952755905511811885, 0.1292274648535926551 ) ) ;
#18618 = CARTESIAN_POINT ( 'NONE',  ( -9.594673741351313045E-17, 0.3917322834645670104, -1.501968503937008093 ) ) ;
#18619 = CARTESIAN_POINT ( 'NONE',  ( -0.8398950131233589023, -0.6046776061558809534, -0.2411417322834644161 ) ) ;
#18620 = CARTESIAN_POINT ( 'NONE',  ( -0.1443569553805765515, -0.4281496062992127816, -0.4176697321401328100 ) ) ;
#18621 = CARTESIAN_POINT ( 'NONE',  ( -1.023622047244093558, -0.1870078740157479769, 0.4822834645669291653 ) ) ;
#18622 = CARTESIAN_POINT ( 'NONE',  ( 0.3215223097112867578, -0.2845877964562161244, -0.3641732283464567121 ) ) ;
#18623 = CARTESIAN_POINT ( 'NONE',  ( -0.2917632292039850639, -0.04688088360317040765, 5.530710407408372831 ) ) ;
#18624 = CARTESIAN_POINT ( 'NONE',  ( 0.08530183727034192087, -0.3162353388693409650, -0.4822834645669289433 ) ) ;
#18625 = FACE_OUTER_BOUND ( 'NONE', #10055, .T. ) ;
#18626 = CARTESIAN_POINT ( 'NONE',  ( 1.305774278215223960, 0.2952755905511810774, -0.1292274648535930714 ) ) ;
#18627 = CARTESIAN_POINT ( 'NONE',  ( -0.2867679344610365999, 0.2867679344610364889, -2.846456692913385655 ) ) ;
#18628 = EDGE_LOOP ( 'NONE', ( #22659, #44271, #49560, #64784 ) ) ;
#18629 = ORIENTED_EDGE ( 'NONE', *, *, #55872, .F. ) ;
#18630 = CARTESIAN_POINT ( 'NONE',  ( 0.4527559055118117182, 0.1660481256975883668, -0.3530559997133364547 ) ) ;
#18631 = CARTESIAN_POINT ( 'NONE',  ( 0.04593175853018440641, 0.1771653543307087075, -0.09757992244046823083 ) ) ;
#18633 = CARTESIAN_POINT ( 'NONE',  ( -1.559171609364246924, 1.299212598425196985, 0.4177787735906735578 ) ) ;
#18632 = CARTESIAN_POINT ( 'NONE',  ( 1.568241469816273659, -0.08942795157528024563, -0.3641732283464568787 ) ) ;
#18634 = CARTESIAN_POINT ( 'NONE',  ( 0.2867679344610365999, -0.2867679344610365444, -1.127952755905512028 ) ) ;
#18635 = CARTESIAN_POINT ( 'NONE',  ( -0.3458507752293906723, -0.3458507752293910609, 0.02165354330708659653 ) ) ;
#18636 = DIRECTION ( 'NONE',  ( 0.000000000000000000, 1.000000000000000000, 0.000000000000000000 ) ) ;
#18637 = CARTESIAN_POINT ( 'NONE',  ( -1.574803149606298192, -0.1870078740157480879, -0.4822834645669291653 ) ) ;
#18638 = CARTESIAN_POINT ( 'NONE',  ( 0.1070741851644054776, -0.3996062992125984925, -2.681758530183727895 ) ) ;
#18639 = CARTESIAN_POINT ( 'NONE',  ( 0.4790026246719167324, -0.05778040916215522460, 0.4822834645669289988 ) ) ;
#18640 = CARTESIAN_POINT ( 'NONE',  ( -1.351706036745406347, -0.4281496062992124485, 0.4176697321401328655 ) ) ;
#18641 = CARTESIAN_POINT ( 'NONE',  ( -1.207349081364828880, 0.2306618581243847221, -0.2411417322834647770 ) ) ;
#18642 = CARTESIAN_POINT ( 'NONE',  ( 0.4002624671916016896, -0.3162353388693409650, -0.4822834645669289433 ) ) ;
#18643 = CARTESIAN_POINT ( 'NONE',  ( 1.148293963254593653, 0.2952755905511810774, -0.1292274648535930714 ) ) ;
#18644 = CARTESIAN_POINT ( 'NONE',  ( 1.286089238845145033, -0.5023911411419708095, -0.1820866141732282451 ) ) ;
#18645 = CARTESIAN_POINT ( 'NONE',  ( 0.8333333333333340365, -0.5511811023622046335, 0.09757992244046803654 ) ) ;
#18646 = CARTESIAN_POINT ( 'NONE',  ( -0.8595800524934373854, -0.05778040916215522460, 0.4822834645669289988 ) ) ;
#18647 = CARTESIAN_POINT ( 'NONE',  ( 0.3996062992125985480, 2.446882876249141654E-17, -0.6673228346456693272 ) ) ;
#18648 = CARTESIAN_POINT ( 'NONE',  ( 1.502624671916010790, -0.05778040916215522460, 0.4822834645669289988 ) ) ;
#18649 = CARTESIAN_POINT ( 'NONE',  ( 0.3917322834645670104, 2.398668435337828261E-17, -0.4251968503937007537 ) ) ;
#18651 = CARTESIAN_POINT ( 'NONE',  ( -0.3636368138136299444, 1.231320578257673715, 2.001016126126115235 ) ) ;
#18650 = CARTESIAN_POINT ( 'NONE',  ( 0.8595800524934390507, -0.3162353388693405765, 0.4822834645669290543 ) ) ;
#18652 = CARTESIAN_POINT ( 'NONE',  ( -1.574803149606298636, -0.1870078740157479769, 0.3641732283464567677 ) ) ;
#18653 = CARTESIAN_POINT ( 'NONE',  ( 0.1246719160104994284, 0.2952755905511810774, -0.1292274648535930714 ) ) ;
#18654 = CARTESIAN_POINT ( 'NONE',  ( 0.6561679790026253567, 0.1283753931104748280, 0.1820866141732283561 ) ) ;
#18655 = CARTESIAN_POINT ( 'NONE',  ( -1.719160104986876103, -0.004921259842519576551, 0.3153832671262227771 ) ) ;
#18656 = CARTESIAN_POINT ( 'NONE',  ( 0.9448818897637802916, -0.1870078740157480879, -0.4822834645669291653 ) ) ;
#18657 = LINE ( 'NONE', #12347, #826 ) ;
#18658 = CARTESIAN_POINT ( 'NONE',  ( -0.6233595800524928121, -0.08942795157527998196, 0.3641732283464567121 ) ) ;
#18659 = CARTESIAN_POINT ( 'NONE',  ( -0.7808398950131225646, -0.05778040916215522460, 0.4822834645669289988 ) ) ;
#18660 = CARTESIAN_POINT ( 'NONE',  ( 1.384514435695538559, 0.2952755905511810774, -0.1292274648535930714 ) ) ;
#18661 = CARTESIAN_POINT ( 'NONE',  ( -1.240157480314959759, 0.1660481256975885056, 0.3530559997133364547 ) ) ;
#18662 = CARTESIAN_POINT ( 'NONE',  ( 1.266404199475066328, -0.3162353388693409650, -0.4822834645669289433 ) ) ;
#18663 = CARTESIAN_POINT ( 'NONE',  ( 0.1049643490035303967, 0.3917322834645670659, -0.7775783708999494115 ) ) ;
#18664 = CARTESIAN_POINT ( 'NONE',  ( -1.397637795275589623, -0.4536011799217368745, -0.2665933059059886201 ) ) ;
#18665 = LINE ( 'NONE', #43902, #3431 ) ;
#18666 = CARTESIAN_POINT ( 'NONE',  ( 1.082677165354331228, -0.5400638737290844871, 0.3530559997133364547 ) ) ;
#18667 = CARTESIAN_POINT ( 'NONE',  ( 0.4724409448818898682, 2.892866454678787531E-17, -2.557086614173228689 ) ) ;
#18668 = CARTESIAN_POINT ( 'NONE',  ( -1.423884514435694859, -0.3162353388693405765, 0.4822834645669290543 ) ) ;
#18669 = CARTESIAN_POINT ( 'NONE',  ( -1.463254593175852492, 0.1771653543307087630, 0.09757992244046791164 ) ) ;
#18670 = CARTESIAN_POINT ( 'NONE',  ( -0.9776902887139098386, -0.5511811023622046335, 0.09757992244046803654 ) ) ;
#18671 = CARTESIAN_POINT ( 'NONE',  ( 1.033875059083676717, 1.724409448818897905, -0.4359958488159719758 ) ) ;
#18672 = CARTESIAN_POINT ( 'NONE',  ( -0.5249343832020990641, 0.2306618581243848609, 0.2411417322834645549 ) ) ;
#18673 = CARTESIAN_POINT ( 'NONE',  ( 0.006561679790026889343, -0.2845877964562161244, -0.3641732283464567121 ) ) ;
#18674 = CARTESIAN_POINT ( 'NONE',  ( -1.581364829396324945, -0.2845877964562159024, 0.3641732283464567677 ) ) ;
#18675 = CARTESIAN_POINT ( 'NONE',  ( 0.9514435695538062676, -0.08942795157527998196, 0.3641732283464567121 ) ) ;
#18676 = CARTESIAN_POINT ( 'NONE',  ( 0.7874015748031503170, -0.1870078740157480879, -0.4822834645669291653 ) ) ;
#18677 = CARTESIAN_POINT ( 'NONE',  ( 1.581364829396326277, -0.05778040916215522460, 0.4822834645669289988 ) ) ;
#18678 = CARTESIAN_POINT ( 'NONE',  ( 0.1049868766404206816, 0.1283753931104748280, 0.1820866141732283561 ) ) ;
#18679 = CARTESIAN_POINT ( 'NONE',  ( 0.5249343832021005074, -0.6046776061558807314, 0.2411417322834647770 ) ) ;
#18680 = EDGE_CURVE ( 'NONE', #23049, #65196, #43015, .T. ) ;
#18681 = CARTESIAN_POINT ( 'NONE',  ( 0.5249343832021003964, 0.1283753931104746893, -0.1820866141732285504 ) ) ;
#18682 = ORIENTED_EDGE ( 'NONE', *, *, #57389, .T. ) ;
#18683 = CARTESIAN_POINT ( 'NONE',  ( -1.561679790026246017, -0.4281496062992127816, -0.4176697321401328100 ) ) ;
#18684 = ADVANCED_FACE ( 'NONE', ( #70416 ), #49124, .F. ) ;
#18685 =( BOUNDED_CURVE ( )  B_SPLINE_CURVE ( 2, ( #5504, #25262, #62338, #50516, #5911, #82128, #51338, #77042, #18150, #69489, #82531, #24849, #30348 ),
 .UNSPECIFIED., .F., .F. ) 
 B_SPLINE_CURVE_WITH_KNOTS ( ( 3, 2, 2, 2, 2, 2, 3 ),
 ( 0.4006038219075281348, 0.4015151515151514916, 0.4053030303030302761, 0.4090909090909091161, 0.4128787878787879007, 0.4166666666666666852, 0.4175779962742901530 ),
 .UNSPECIFIED. ) 
 CURVE ( )  GEOMETRIC_REPRESENTATION_ITEM ( )  RATIONAL_B_SPLINE_CURVE ( ( 0.9875488213027530104, 0.9918020599134685922, 1.000000000000000000, 0.9659258262890683122, 1.000000000000000000, 0.9659258262890683122, 1.000000000000000000, 0.9659258262890683122, 1.000000000000000000, 0.9659258262890683122, 1.000000000000000000, 0.9918020599134675930, 0.9875488213027519002 ) ) 
 REPRESENTATION_ITEM ( '' )  );
#18686 = CARTESIAN_POINT ( 'NONE',  ( -1.410761154855641575, -0.3162353388693409650, -0.4822834645669289433 ) ) ;
#18687 = CARTESIAN_POINT ( 'NONE',  ( -0.03937007874015669567, -0.6692913385826771977, 8.415575281601705876E-17 ) ) ;
#18688 = CARTESIAN_POINT ( 'NONE',  ( -0.2925321140481930704, -0.2925321140481933480, -0.2165354330708661734 ) ) ;
#18689 = CARTESIAN_POINT ( 'NONE',  ( -0.1998031496062991630, -0.3460692066303959202, -2.819553805774277944 ) ) ;
#18690 = CARTESIAN_POINT ( 'NONE',  ( 0.4658792650918640033, -0.3162353388693405765, 0.4822834645669290543 ) ) ;
#18691 = CARTESIAN_POINT ( 'NONE',  ( 1.069553805774278610, -0.5511811023622046335, 0.09757992244046803654 ) ) ;
#18692 = CARTESIAN_POINT ( 'NONE',  ( -0.2362204724409440182, -0.1870078740157479769, 0.4822834645669291653 ) ) ;
#18694 = AXIS2_PLACEMENT_3D ( 'NONE', #65783, #78412, #26203 ) ;
#18693 = CARTESIAN_POINT ( 'NONE',  ( 0.4133858267716541968, -0.5400638737290845981, -0.3530559997133363437 ) ) ;
#18695 = CARTESIAN_POINT ( 'NONE',  ( 0.1998031496062992740, 0.3460692066303959757, -2.034120734908136718 ) ) ;
#18696 = CARTESIAN_POINT ( 'NONE',  ( 0.3949938075777409408, 0.1058382717557500574, -1.541994750656168200 ) ) ;
#18697 = CARTESIAN_POINT ( 'NONE',  ( 0.3996062992125986035, 2.446882876249141962E-17, -2.952755905511811108 ) ) ;
#18698 = DIRECTION ( 'NONE',  ( 1.000000000000000000, 3.469446951953613203E-16, 0.000000000000000000 ) ) ;
#18699 = CARTESIAN_POINT ( 'NONE',  ( -0.1049643490035301885, -0.3917322834645671215, -0.6942257217847767059 ) ) ;
#18700 = CARTESIAN_POINT ( 'NONE',  ( -0.3346456692913377662, -0.4536011799217367080, 0.2665933059059888421 ) ) ;
#18701 = CARTESIAN_POINT ( 'NONE',  ( -1.102362204724408601, -0.1870078740157479769, 0.4822834645669291653 ) ) ;
#18702 = CARTESIAN_POINT ( 'NONE',  ( 0.1974969037888704704, 0.3420746716998660508, -2.425853018372703396 ) ) ;
#18703 = CARTESIAN_POINT ( 'NONE',  ( 0.8595800524934390507, -0.3162353388693405765, 0.4822834645669290543 ) ) ;
#18704 = EDGE_CURVE ( 'NONE', #5673, #64597, #45996, .T. ) ;
#18705 = CARTESIAN_POINT ( 'NONE',  ( -1.614173228346455824, 0.2952755905511811885, 0.000000000000000000 ) ) ;
#18706 = CARTESIAN_POINT ( 'NONE',  ( 0.7545931758530188826, -0.6692913385826771977, 0.1292274648535927661 ) ) ;
#18707 = CARTESIAN_POINT ( 'NONE',  ( 0.1070741851644053527, 0.3996062992125986590, -2.040682414698162361 ) ) ;
#18708 = CARTESIAN_POINT ( 'NONE',  ( 1.646981627296588035, -0.3162353388693405765, 0.4822834645669290543 ) ) ;
#18709 = ADVANCED_FACE ( 'NONE', ( #7712 ), #716, .F. ) ;
#18710 = CARTESIAN_POINT ( 'NONE',  ( 1.102362204724410155, -0.1870078740157479769, 0.4822834645669291653 ) ) ;
#18711 = CARTESIAN_POINT ( 'NONE',  ( 0.5314960629921264834, 0.1660481256975883668, -0.3530559997133364547 ) ) ;
#18712 = CARTESIAN_POINT ( 'NONE',  ( 0.7611548556430451917, -0.5023911411419708095, 0.1820866141732285504 ) ) ;
#18713 = CARTESIAN_POINT ( 'NONE',  ( 1.154855643044620184, -0.6046776061558807314, 0.2411417322834647770 ) ) ;
#18714 = CARTESIAN_POINT ( 'NONE',  ( 0.2867679344610365999, -0.2867679344610365444, -0.3405511811023621549 ) ) ;
#18715 = CARTESIAN_POINT ( 'NONE',  ( -1.586052503253845503, 2.125984251968505045, 0.1653254495020588799 ) ) ;
#18716 = CARTESIAN_POINT ( 'NONE',  ( 0.6167979002624679463, 0.05413385826771626580, -0.4176697321401330321 ) ) ;
#18717 = CARTESIAN_POINT ( 'NONE',  ( -1.128608923884513837, -0.6046776061558807314, 0.2411417322834647770 ) ) ;
#18718 = CARTESIAN_POINT ( 'NONE',  ( -0.8792650918635160906, 0.05413385826771626580, -0.4176697321401330321 ) ) ;
#18719 = CARTESIAN_POINT ( 'NONE',  ( 1.266404199475066328, -0.05778040916215522460, 0.4822834645669289988 ) ) ;
#18720 = CARTESIAN_POINT ( 'NONE',  ( 0.3917322834645669549, 0.1049643490035304660, -0.3667979002624672802 ) ) ;
#18721 = CARTESIAN_POINT ( 'NONE',  ( 0.3917322834645670104, -0.1049643490035303411, -1.520997375328083656 ) ) ;
#18722 = CARTESIAN_POINT ( 'NONE',  ( -0.2867679344610364334, -0.2867679344610367109, -2.728346456692912536 ) ) ;
#18723 = EDGE_LOOP ( 'NONE', ( #60646, #49876 ) ) ;
#18724 = CARTESIAN_POINT ( 'NONE',  ( -0.1070741851644051862, -0.3996062992125987146, -0.07217847769028871985 ) ) ;
#18725 = EDGE_LOOP ( 'NONE', ( #11599, #17265, #47178, #34365 ) ) ;
#18726 = FACE_OUTER_BOUND ( 'NONE', #12056, .T. ) ;
#18727 = CARTESIAN_POINT ( 'NONE',  ( 1.417322834645670104, -0.1870078740157479769, 0.3641732283464567677 ) ) ;
#18728 = CARTESIAN_POINT ( 'NONE',  ( 4.893765752498283924E-17, -0.3996062992125986035, -1.496062992125984259 ) ) ;
#18729 = CARTESIAN_POINT ( 'NONE',  ( 1.279527559055118724, -0.4536011799217368745, -0.2665933059059886201 ) ) ;
#18730 = DIRECTION ( 'NONE',  ( 0.000000000000000000, -1.000000000000000000, 0.000000000000000000 ) ) ;
#18731 = CARTESIAN_POINT ( 'NONE',  ( -1.646051170424378096, 0.000000000000000000, -0.3464511005275205946 ) ) ;
#18732 = CARTESIAN_POINT ( 'NONE',  ( -0.5314960629921147151, 2.716535433070866645, -3.224202737261816942 ) ) ;
#18733 = CARTESIAN_POINT ( 'NONE',  ( 0.3917322834645670104, 2.398668435337828261E-17, -0.5177165354330709457 ) ) ;
#18734 = CARTESIAN_POINT ( 'NONE',  ( -0.9317585301837263412, -0.3690944881889765550, -0.3153832671262227771 ) ) ;
#18735 = CARTESIAN_POINT ( 'NONE',  ( -1.456692913385826182, -0.5511811023622047445, 6.969142054262312111E-17 ) ) ;
#18736 = CARTESIAN_POINT ( 'NONE',  ( -1.148293963254592542, 0.2952755905511811885, 0.1292274648535926551 ) ) ;
#18737 = CARTESIAN_POINT ( 'NONE',  ( 0.1377952755905518800, -0.5400638737290844871, 0.3530559997133364547 ) ) ;
#18738 = CARTESIAN_POINT ( 'NONE',  ( 1.371391076115485719, -0.6692913385826773087, -0.1292274648535924053 ) ) ;
#18739 = ORIENTED_EDGE ( 'NONE', *, *, #72215, .F. ) ;
#18740 = DIRECTION ( 'NONE',  ( 0.000000000000000000, 0.000000000000000000, 1.000000000000000000 ) ) ;
#18741 = CARTESIAN_POINT ( 'NONE',  ( 0.2362204724409449064, 0.4091458600556404646, -2.191601049868766360 ) ) ;
#18742 = CARTESIAN_POINT ( 'NONE',  ( 1.614173228346457156, 1.496062992125984037, 0.5309055118110233007 ) ) ;
#18743 = CARTESIAN_POINT ( 'NONE',  ( -0.5052493438320203589, 0.1771653543307087075, -0.09757992244046823083 ) ) ;
#18744 = CARTESIAN_POINT ( 'NONE',  ( -1.227034120734907141, -0.6692913385826773087, -0.1292274648535924053 ) ) ;
#18745 = CARTESIAN_POINT ( 'NONE',  ( 1.036745406824147731, 0.05413385826771666132, 0.4176697321401328100 ) ) ;
#18746 = ORIENTED_EDGE ( 'NONE', *, *, #4808, .T. ) ;
#18748 = CARTESIAN_POINT ( 'NONE',  ( -1.559171609364246924, 0.4110443821404751730, 0.2406134192599649890 ) ) ;
#18747 = CARTESIAN_POINT ( 'NONE',  ( 0.000000000000000000, 1.724409448818897461, 0.000000000000000000 ) ) ;
#18749 = CARTESIAN_POINT ( 'NONE',  ( 1.266404199475066328, -0.3162353388693409650, -0.4822834645669289433 ) ) ;
#18750 = CARTESIAN_POINT ( 'NONE',  ( -1.128608923884513837, -0.6046776061558807314, 0.2411417322834647770 ) ) ;
#18751 = CARTESIAN_POINT ( 'NONE',  ( 0.2867679344610365999, -0.2867679344610365999, -0.4934190044281346332 ) ) ;
#18752 = CARTESIAN_POINT ( 'NONE',  ( -0.4002624671916004129, -0.08942795157528024563, -0.3641732283464568787 ) ) ;
#18753 = CARTESIAN_POINT ( 'NONE',  ( -0.1049643490035307020, 0.3917322834645669549, -0.7211286089238846397 ) ) ;
#18754 = CARTESIAN_POINT ( 'NONE',  ( -0.5905511811023613777, -0.5511811023622047445, 6.969142054262312111E-17 ) ) ;
#18755 = CARTESIAN_POINT ( 'NONE',  ( 0.3215223097112867578, -0.08942795157527998196, 0.3641732283464567121 ) ) ;
#18756 = CARTESIAN_POINT ( 'NONE',  ( 0.01968503937007930540, 0.1660481256975885056, 0.3530559997133364547 ) ) ;
#18757 = CARTESIAN_POINT ( 'NONE',  ( -0.7349081364829387342, -0.5023911411419708095, 0.1820866141732285504 ) ) ;
#18758 = CARTESIAN_POINT ( 'NONE',  ( -9.594673741351313045E-17, 0.3917322834645670659, 0.1607418390738039049 ) ) ;
#18759 = CARTESIAN_POINT ( 'NONE',  ( 1.148293963254593653, 0.2952755905511810774, -0.1292274648535930714 ) ) ;
#18760 = EDGE_CURVE ( 'NONE', #79206, #58800, #19931, .T. ) ;
#18761 = CARTESIAN_POINT ( 'NONE',  ( -1.496062992125983815, -0.1870078740157479769, 0.4822834645669291653 ) ) ;
#18762 = CARTESIAN_POINT ( 'NONE',  ( 0.4091458600556403535, 0.2362204724409449896, -1.310367454068241511 ) ) ;
#18763 = CARTESIAN_POINT ( 'NONE',  ( -0.5643044619422565855, 0.05413385826771626580, -0.4176697321401330321 ) ) ;
#18764 = CARTESIAN_POINT ( 'NONE',  ( -0.8530183727034112984, 0.05413385826771666132, 0.4176697321401328100 ) ) ;
#18765 = CARTESIAN_POINT ( 'NONE',  ( 1.213910761154856299, 0.1771653543307087630, 0.09757992244046791164 ) ) ;
#18766 = CARTESIAN_POINT ( 'NONE',  ( -0.3937007874015740483, -0.1870078740157480601, -0.3641732283464567677 ) ) ;
#18767 = CARTESIAN_POINT ( 'NONE',  ( -0.8005249343832013809, -0.4281496062992124485, 0.4176697321401328655 ) ) ;
#18768 = CARTESIAN_POINT ( 'NONE',  ( -1.292650918635170010, 0.2952755905511810774, -0.1292274648535930714 ) ) ;
#18769 = DIRECTION ( 'NONE',  ( 1.000000000000000000, 0.000000000000000000, 0.000000000000000000 ) ) ;
#18770 = CARTESIAN_POINT ( 'NONE',  ( 1.135170603674541256, -0.5511811023622048555, -0.09757992244046775898 ) ) ;
#18771 = CARTESIAN_POINT ( 'NONE',  ( -0.4461942257217840213, -0.6046776061558809534, -0.2411417322834644161 ) ) ;
#18772 = CARTESIAN_POINT ( 'NONE',  ( -1.187664041994750175, -0.05778040916215560624, -0.4822834645669293319 ) ) ;
#18773 = ORIENTED_EDGE ( 'NONE', *, *, #53723, .T. ) ;
#18774 = CARTESIAN_POINT ( 'NONE',  ( -0.2925321140481930149, -0.2925321140481933480, -2.340551181102362488 ) ) ;
#18775 = CARTESIAN_POINT ( 'NONE',  ( -0.6889763779527552368, 0.07958543189024085140, 0.2665933059059887866 ) ) ;
#18776 = CARTESIAN_POINT ( 'NONE',  ( 1.240157480314961314, -0.5400638737290844871, 0.3530559997133364547 ) ) ;
#18777 = CARTESIAN_POINT ( 'NONE',  ( -1.036745406824146176, -0.004921259842519870586, -0.3153832671262229437 ) ) ;
#18778 = CARTESIAN_POINT ( 'NONE',  ( 0.3460692066303958092, 0.1998031496062993018, -1.310367454068241733 ) ) ;
#18779 = CARTESIAN_POINT ( 'NONE',  ( -0.9317585301837263412, 0.05413385826771666132, 0.4176697321401328100 ) ) ;
#18780 = CARTESIAN_POINT ( 'NONE',  ( 1.417322834645670104, -0.1870078740157480879, -0.4822834645669291653 ) ) ;
#18781 = CARTESIAN_POINT ( 'NONE',  ( 1.023622047244095334, -0.1870078740157479769, 0.4822834645669291653 ) ) ;
#18782 = CARTESIAN_POINT ( 'NONE',  ( 1.456692913385827515, 0.2952755905511811885, 0.000000000000000000 ) ) ;
#18783 = CARTESIAN_POINT ( 'NONE',  ( -1.325459317585300889, -0.3690944881889765550, -0.3153832671262227771 ) ) ;
#18784 = CARTESIAN_POINT ( 'NONE',  ( -0.2925321140481932369, 0.2925321140481930704, -0.7263779527559055538 ) ) ;
#18785 = CARTESIAN_POINT ( 'NONE',  ( -0.3996062992125986035, -7.340648628747425578E-17, -1.141732283464566899 ) ) ;
#18786 = CARTESIAN_POINT ( 'NONE',  ( -0.3420746716998659953, -0.1974969037888706647, -0.2099737532808399476 ) ) ;
#18787 = CARTESIAN_POINT ( 'NONE',  ( 6.267877385347666114E-17, 1.062992125984252745, 2.874015748031495843 ) ) ;
#18788 = CARTESIAN_POINT ( 'NONE',  ( 1.299212598425197429, -0.5511811023622047445, 6.969142054262312111E-17 ) ) ;
#18789 = CARTESIAN_POINT ( 'NONE',  ( 0.6955380577427828781, -0.004921259842519870586, -0.3153832671262229437 ) ) ;
#18790 = CARTESIAN_POINT ( 'NONE',  ( 0.5183727034120741983, 0.2952755905511810774, -0.1292274648535930714 ) ) ;
#18791 = CARTESIAN_POINT ( 'NONE',  ( 1.509186351706037543, -0.4281496062992127816, -0.4176697321401328100 ) ) ;
#18792 = CARTESIAN_POINT ( 'NONE',  ( 0.2891555358219910499, 0.2891555358219910499, -1.316929133858267598 ) ) ;
#18793 = CARTESIAN_POINT ( 'NONE',  ( 0.9842519685039378130, -0.5511811023622047445, 6.969142054262312111E-17 ) ) ;
#18794 = ADVANCED_FACE ( 'NONE', ( #40104 ), #65792, .F. ) ;
#18795 = CARTESIAN_POINT ( 'NONE',  ( -0.4068241469816264999, -0.4281496062992124485, 0.4176697321401328655 ) ) ;
#18796 = CARTESIAN_POINT ( 'NONE',  ( -1.364829396325458521, -0.6046776061558807314, 0.2411417322834647770 ) ) ;
#18797 = CARTESIAN_POINT ( 'NONE',  ( 0.9842519685039378130, -0.6692913385826771977, 8.415575281601705876E-17 ) ) ;
#18798 = CARTESIAN_POINT ( 'NONE',  ( 0.3458507752293908943, 0.3458507752293908943, -1.712598425196850460 ) ) ;
#18799 = CARTESIAN_POINT ( 'NONE',  ( -0.3996062992125986035, -7.340648628747425578E-17, -2.716535433070865757 ) ) ;
#18800 = ORIENTED_EDGE ( 'NONE', *, *, #48192, .T. ) ;
#18801 = ORIENTED_EDGE ( 'NONE', *, *, #73800, .T. ) ;
#18802 = CARTESIAN_POINT ( 'NONE',  ( -1.082677165354329896, 0.1660481256975885056, 0.3530559997133364547 ) ) ;
#18803 = CARTESIAN_POINT ( 'NONE',  ( -0.7808398950131222316, -0.3162353388693409650, -0.4822834645669289433 ) ) ;
#18805 = CARTESIAN_POINT ( 'NONE',  ( -0.8923884514435688198, -0.6046776061558807314, 0.2411417322834647770 ) ) ;
#18804 = CARTESIAN_POINT ( 'NONE',  ( -0.6364829396325453192, -0.08942795157528024563, -0.3641732283464568787 ) ) ;
#18806 = CARTESIAN_POINT ( 'NONE',  ( -0.2867679344610364334, -0.2867679344610368219, -1.871371760333646606 ) ) ;
#18807 = CARTESIAN_POINT ( 'NONE',  ( 0.4986876640419954376, -0.6046776061558809534, -0.2411417322834644161 ) ) ;
#18808 = CARTESIAN_POINT ( 'NONE',  ( -0.3149606299212590610, -0.1870078740157480879, -0.4822834645669291653 ) ) ;
#18809 = CARTESIAN_POINT ( 'NONE',  ( 1.437007874015748810, 0.1660481256975885056, 0.3530559997133364547 ) ) ;
#18810 = CARTESIAN_POINT ( 'NONE',  ( -0.6758530183727028406, -0.6692913385826773087, -0.1292274648535924053 ) ) ;
#18811 = CARTESIAN_POINT ( 'NONE',  ( 0.6036745406824153282, -0.6046776061558807314, 0.2411417322834647770 ) ) ;
#18812 = CARTESIAN_POINT ( 'NONE',  ( 0.3392501089628018884, -0.1958661417322834220, -1.514435695538058013 ) ) ;
#18813 = CARTESIAN_POINT ( 'NONE',  ( -0.8989501312335946848, -0.5511811023622046335, 0.09757992244046803654 ) ) ;
#18814 = ORIENTED_EDGE ( 'NONE', *, *, #4808, .F. ) ;
#18815 = CARTESIAN_POINT ( 'NONE',  ( -0.2891555358219911054, 0.2891555358219909388, -1.751968503937008093 ) ) ;
#18816 = VERTEX_POINT ( 'NONE', #13195 ) ;
#18817 = CARTESIAN_POINT ( 'NONE',  ( -1.220472440944881054, 0.1771653543307087630, 0.000000000000000000 ) ) ;
#18818 = CARTESIAN_POINT ( 'NONE',  ( -1.089238845144356427, -0.4281496062992127816, -0.4176697321401328100 ) ) ;
#18819 = CARTESIAN_POINT ( 'NONE',  ( -1.069553805774277722, -0.6692913385826773087, -0.1292274648535924053 ) ) ;
#18820 = CARTESIAN_POINT ( 'NONE',  ( 0.3460692066303959757, -0.1998031496062991907, -0.2624671916010498651 ) ) ;
#18821 = CARTESIAN_POINT ( 'NONE',  ( -1.003937007874015297, -0.5400638737290845981, -0.3530559997133363437 ) ) ;
#18822 = CARTESIAN_POINT ( 'NONE',  ( -1.148293963254592542, -0.6692913385826773087, -0.1292274648535924053 ) ) ;
#18823 = CARTESIAN_POINT ( 'NONE',  ( -1.509186351706035767, -0.4281496062992124485, 0.4176697321401328655 ) ) ;
#18824 = EDGE_CURVE ( 'NONE', #62598, #60937, #32529, .T. ) ;
#18825 = CARTESIAN_POINT ( 'NONE',  ( 3.886287458032462006, 2.755905511811024056, 0.6299212598425202314 ) ) ;
#18826 = CARTESIAN_POINT ( 'NONE',  ( 0.3805774278215230400, -0.3690944881889763329, 0.3153832671262228327 ) ) ;
#18827 = FACE_OUTER_BOUND ( 'NONE', #41191, .T. ) ;
#18828 = CARTESIAN_POINT ( 'NONE',  ( 0.1958661417322836440, -0.3392501089628017219, 0.1384514435695537171 ) ) ;
#18829 = CARTESIAN_POINT ( 'NONE',  ( -0.5446194225721777693, -0.2845877964562161244, -0.3641732283464567121 ) ) ;
#18830 = CARTESIAN_POINT ( 'NONE',  ( -0.2099737532808391705, 0.2306618581243848609, 0.2411417322834645549 ) ) ;
#18831 = ADVANCED_FACE ( 'NONE', ( #66201 ), #26214, .F. ) ;
#18832 = CARTESIAN_POINT ( 'NONE',  ( 1.167979002624672580, 0.05413385826771626580, -0.4176697321401330321 ) ) ;
#18833 = CARTESIAN_POINT ( 'NONE',  ( -0.4724409448818890911, -0.1870078740157480879, -0.4822834645669291653 ) ) ;
#18834 = EDGE_LOOP ( 'NONE', ( #11293, #73001, #38925, #72836, #42189, #54326, #46349, #71225, #72155, #47674 ) ) ;
#18835 = ORIENTED_EDGE ( 'NONE', *, *, #58189, .F. ) ;
#18836 = CARTESIAN_POINT ( 'NONE',  ( 0.3460692066303958092, 0.1998031496062993018, -1.467847769028871596 ) ) ;
#18837 = CARTESIAN_POINT ( 'NONE',  ( -0.3805774278215216522, 0.05413385826771666132, 0.4176697321401328100 ) ) ;
#18838 = CARTESIAN_POINT ( 'NONE',  ( 1.174540682414699111, -0.05778040916215560624, -0.4822834645669293319 ) ) ;
#18839 = CARTESIAN_POINT ( 'NONE',  ( -1.017060367454067249, -0.2845877964562161244, -0.3641732283464567121 ) ) ;
#18840 = CARTESIAN_POINT ( 'NONE',  ( -1.266404199475064773, -0.3162353388693405765, 0.4822834645669290543 ) ) ;
#18841 = CARTESIAN_POINT ( 'NONE',  ( -0.4091458600556402980, -0.2362204724409451284, -0.9973753280839895430 ) ) ;
#18842 = CARTESIAN_POINT ( 'NONE',  ( -0.7426113562972000981, 2.362204724409448620, 0.5309055118110236338 ) ) ;
#18843 = CARTESIAN_POINT ( 'NONE',  ( 0.1958661417322836440, -0.3392501089628017219, 0.07349081364829400387 ) ) ;
#18844 = CARTESIAN_POINT ( 'NONE',  ( 1.115485564304462551, -0.4281496062992127816, -0.4176697321401328100 ) ) ;
#18845 = CARTESIAN_POINT ( 'NONE',  ( -0.3917322834645670104, -7.196005306013484475E-17, -2.171259842519685179 ) ) ;
#18846 = CARTESIAN_POINT ( 'NONE',  ( -0.006561679790025524116, -0.05778040916215560624, -0.4822834645669293319 ) ) ;
#18847 = CARTESIAN_POINT ( 'NONE',  ( -0.9120734908136475250, -0.5511811023622048555, -0.09757992244046775898 ) ) ;
#18848 = CARTESIAN_POINT ( 'NONE',  ( -0.3740157480314953431, -0.5400638737290845981, -0.3530559997133363437 ) ) ;
#18849 = CARTESIAN_POINT ( 'NONE',  ( 0.2362204724409449064, 0.4091458600556404646, -2.740813648293963567 ) ) ;
#18850 = CARTESIAN_POINT ( 'NONE',  ( -0.8070866141732276899, -0.5400638737290844871, 0.3530559997133364547 ) ) ;
#18851 = CARTESIAN_POINT ( 'NONE',  ( -1.200787401574802349, 0.1660481256975883668, -0.3530559997133364547 ) ) ;
#18852 = CARTESIAN_POINT ( 'NONE',  ( -0.3949938075777408852, -0.1058382717557502933, -2.327427821522309870 ) ) ;
#18853 = CARTESIAN_POINT ( 'NONE',  ( 0.8989501312335963501, -0.5511811023622048555, -0.09757992244046775898 ) ) ;
#18854 = CARTESIAN_POINT ( 'NONE',  ( -0.4265091863517051496, 0.1771653543307087075, -0.09757992244046823083 ) ) ;
#18855 = CARTESIAN_POINT ( 'NONE',  ( 0.7677165354330716118, 0.07958543189024071263, -0.2665933059059888421 ) ) ;
#18856 = CARTESIAN_POINT ( 'NONE',  ( -1.614173228346456268, -0.6692913385826771977, 8.415575281601705876E-17 ) ) ;
#18857 = CARTESIAN_POINT ( 'NONE',  ( 1.384514435695538337, -0.6692913385826771977, 0.1292274648535927661 ) ) ;
#18858 = CARTESIAN_POINT ( 'NONE',  ( 0.7020997375328090762, -0.2845877964562159024, 0.3641732283464567677 ) ) ;
#18859 = CARTESIAN_POINT ( 'NONE',  ( -0.9120734908136475250, -0.6692913385826773087, -0.1292274648535924053 ) ) ;
#18860 = CARTESIAN_POINT ( 'NONE',  ( 1.194225721784777594, -0.4281496062992127816, -0.4176697321401328100 ) ) ;
#18861 = CARTESIAN_POINT ( 'NONE',  ( -0.4724409448818898682, -8.678599364036362592E-17, 0.1988188976377952832 ) ) ;
#18862 = CARTESIAN_POINT ( 'NONE',  ( -0.1706036745406816491, -0.004921259842519870586, -0.3153832671262229437 ) ) ;
#18863 = DIRECTION ( 'NONE',  ( 0.000000000000000000, 1.000000000000000000, 0.000000000000000000 ) ) ;
#18864 = CARTESIAN_POINT ( 'NONE',  ( 0.1640419947506569498, -0.3162353388693409650, -0.4822834645669289433 ) ) ;
#18865 = CARTESIAN_POINT ( 'NONE',  ( 0.6824146981627303710, 0.2306618581243847221, -0.2411417322834647770 ) ) ;
#18866 = CARTESIAN_POINT ( 'NONE',  ( 0.9908136482939640111, 0.1771653543307087075, -0.09757992244046823083 ) ) ;
#18867 = CARTESIAN_POINT ( 'NONE',  ( 0.2821522309711292364, -0.5511811023622046335, 0.09757992244046803654 ) ) ;
#18868 = CARTESIAN_POINT ( 'NONE',  ( -1.351706036745406347, 0.05413385826771626580, -0.4176697321401330321 ) ) ;
#18869 = CARTESIAN_POINT ( 'NONE',  ( -0.6955380577427815458, -0.004921259842519576551, 0.3153832671262227771 ) ) ;
#18870 = FACE_OUTER_BOUND ( 'NONE', #62194, .T. ) ;
#18871 = CARTESIAN_POINT ( 'NONE',  ( -1.115485564304461219, -0.4281496062992124485, 0.4176697321401328655 ) ) ;
#18872 = CARTESIAN_POINT ( 'NONE',  ( -0.5708661417322825615, -0.5400638737290844871, 0.3530559997133364547 ) ) ;
#18873 = CARTESIAN_POINT ( 'NONE',  ( 0.3996062992125986035, -0.1070741851644052972, -0.9757217847769029673 ) ) ;
#18874 = CARTESIAN_POINT ( 'NONE',  ( 0.3392501089628018884, -0.1958661417322834220, -2.236876640419947826 ) ) ;
#18875 = CARTESIAN_POINT ( 'NONE',  ( 0.5774278215223103139, -0.5023911411419708095, -0.1820866141732282451 ) ) ;
#18876 = CARTESIAN_POINT ( 'NONE',  ( -0.1771653543307080136, 0.1660481256975883668, -0.3530559997133364547 ) ) ;
#18877 = CARTESIAN_POINT ( 'NONE',  ( -0.6233595800524928121, -0.3162353388693409650, -0.4822834645669289433 ) ) ;
#18878 = CARTESIAN_POINT ( 'NONE',  ( -0.7611548556430438595, -0.5023911411419708095, -0.1820866141732282451 ) ) ;
#18879 = CARTESIAN_POINT ( 'NONE',  ( 0.4744094488189112835, 1.537401574803149984, -3.908320185825791881 ) ) ;
#18880 = CARTESIAN_POINT ( 'NONE',  ( 8.195543980992789655E-16, -0.1870078740157480879, -0.4822834645669291653 ) ) ;
#18881 = CARTESIAN_POINT ( 'NONE',  ( -1.712598425196849572, 0.07958543189024085140, 0.2665933059059887866 ) ) ;
#18882 = CARTESIAN_POINT ( 'NONE',  ( 1.305774278215223960, 0.2952755905511810774, -0.1292274648535930714 ) ) ;
#18883 = CARTESIAN_POINT ( 'NONE',  ( -0.2362204724409447953, -0.4091458600556404646, -0.6955380577427822120 ) ) ;
#18884 = CARTESIAN_POINT ( 'NONE',  ( 0.1049643490035304799, -0.3917322834645670104, -2.129284407645356314 ) ) ;
#18885 = VERTEX_POINT ( 'NONE', #77156 ) ;
#18886 = CARTESIAN_POINT ( 'NONE',  ( -0.7443564561544175895, 1.971400176368010237, 0.5309055118110236338 ) ) ;
#18887 = CARTESIAN_POINT ( 'NONE',  ( -1.332020997375327642, -0.3162353388693409650, -0.4822834645669289433 ) ) ;
#18888 = CARTESIAN_POINT ( 'NONE',  ( -0.9711286089238838626, -0.6046776061558807314, 0.2411417322834647770 ) ) ;
#18889 = CARTESIAN_POINT ( 'NONE',  ( -1.653543307086613234, -0.1870078740157479769, 0.4822834645669291653 ) ) ;
#18890 = CARTESIAN_POINT ( 'NONE',  ( 0.1958661417322834775, 0.3392501089628018884, -1.803805774278215202 ) ) ;
#18891 = DIRECTION ( 'NONE',  ( -3.491481338843132961E-15, 0.000000000000000000, 1.000000000000000000 ) ) ;
#18892 = CARTESIAN_POINT ( 'NONE',  ( 0.9514435695538062676, -0.3162353388693409650, -0.4822834645669289433 ) ) ;
#18893 = CARTESIAN_POINT ( 'NONE',  ( 0.06561679790026316017, -0.4281496062992124485, 0.4176697321401328655 ) ) ;
#18894 = DIRECTION ( 'NONE',  ( -3.096699300667737957E-16, 1.000000000000000000, -0.000000000000000000 ) ) ;
#18895 = CARTESIAN_POINT ( 'NONE',  ( -0.6692913385826764205, 0.2952755905511811885, 0.000000000000000000 ) ) ;
#18896 = CARTESIAN_POINT ( 'NONE',  ( 1.253280839895013710, -0.2845877964562159024, 0.3641732283464567677 ) ) ;
#18897 = CARTESIAN_POINT ( 'NONE',  ( 0.3996062992125986035, 2.446882876249141962E-17, -1.535433070866141669 ) ) ;
#18898 = VERTEX_POINT ( 'NONE', #19488 ) ;
#18899 = CARTESIAN_POINT ( 'NONE',  ( 4.797336870675656522E-17, -0.3917322834645670104, -2.905511811023621771 ) ) ;
#18900 = ORIENTED_EDGE ( 'NONE', *, *, #5310, .T. ) ;
#18901 = CARTESIAN_POINT ( 'NONE',  ( 0.6102362204724416372, -0.5400638737290844871, 0.3530559997133364547 ) ) ;
#18902 = CARTESIAN_POINT ( 'NONE',  ( -0.6036745406824141069, 0.2306618581243848609, 0.2411417322834645549 ) ) ;
#18903 = CARTESIAN_POINT ( 'NONE',  ( -1.574803149606298192, -0.1870078740157480879, -0.4822834645669291653 ) ) ;
#18904 = CARTESIAN_POINT ( 'NONE',  ( 0.7611548556430454138, 0.2306618581243847221, -0.2411417322834647770 ) ) ;
#18905 = CARTESIAN_POINT ( 'NONE',  ( 1.614173228346457378, -0.6692913385826771977, 8.415575281601705876E-17 ) ) ;
#18906 = CARTESIAN_POINT ( 'NONE',  ( 1.364829396325459854, -0.6046776061558809534, -0.2411417322834644161 ) ) ;
#18907 = CARTESIAN_POINT ( 'NONE',  ( -0.01312335958005186876, 0.05413385826771626580, -0.4176697321401330321 ) ) ;
#18908 = CARTESIAN_POINT ( 'NONE',  ( -1.404199475065615932, -0.4281496062992127816, -0.4176697321401328100 ) ) ;
#18909 = CARTESIAN_POINT ( 'NONE',  ( 1.437007874015748810, 0.1660481256975885056, 0.3530559997133364547 ) ) ;
#18910 = CARTESIAN_POINT ( 'NONE',  ( 1.581364829396326277, -0.3162353388693409650, -0.4822834645669289433 ) ) ;
#18911 =( BOUNDED_CURVE ( )  B_SPLINE_CURVE ( 2, ( #62863, #63681, #38003, #82636, #30456, #11937, #43480, #75507, #17846, #5606, #69992, #70407, #69176 ),
 .UNSPECIFIED., .F., .F. ) 
 B_SPLINE_CURVE_WITH_KNOTS ( ( 3, 2, 2, 2, 2, 2, 3 ),
 ( 0.6278765491802553722, 0.6287878787878787845, 0.6325757575757575690, 0.6363636363636363535, 0.6401515151515151381, 0.6439393939393939226, 0.6448507235470174459 ),
 .UNSPECIFIED. ) 
 CURVE ( )  GEOMETRIC_REPRESENTATION_ITEM ( )  RATIONAL_B_SPLINE_CURVE ( ( 0.9875488213027523443, 0.9918020599134680371, 1.000000000000000000, 0.9659258262890683122, 1.000000000000000000, 0.9659258262890683122, 1.000000000000000000, 0.9659258262890683122, 1.000000000000000000, 0.9659258262890683122, 1.000000000000000000, 0.9918020599134671489, 0.9875488213027514561 ) ) 
 REPRESENTATION_ITEM ( '' )  );
#18912 = CARTESIAN_POINT ( 'NONE',  ( -0.1958661417322836718, 0.3392501089628017219, -0.005249343832020950465 ) ) ;
#18913 = CARTESIAN_POINT ( 'NONE',  ( 0.8661417322834653598, -0.1870078740157479769, 0.3641732283464567677 ) ) ;
#18914 = ORIENTED_EDGE ( 'NONE', *, *, #68203, .T. ) ;
#18915 = CARTESIAN_POINT ( 'NONE',  ( -0.3949938075777411628, 0.1058382717557497937, -0.03280839895013128865 ) ) ;
#18916 = EDGE_LOOP ( 'NONE', ( #18739, #75439, #62410, #30201 ) ) ;
#18917 = CARTESIAN_POINT ( 'NONE',  ( 0.01968503937007930540, 0.07958543189024085140, 0.2665933059059887866 ) ) ;
#18918 = CARTESIAN_POINT ( 'NONE',  ( -0.3458507752293909498, 0.3458507752293908388, -0.1771653543307086520 ) ) ;
#18919 = CARTESIAN_POINT ( 'NONE',  ( 0.04593175853018440641, 0.2952755905511810774, -0.1292274648535930714 ) ) ;
#18920 = CARTESIAN_POINT ( 'NONE',  ( -0.09842519685039295696, 0.1660481256975883668, -0.3530559997133364547 ) ) ;
#18921 = EDGE_CURVE ( 'NONE', #23282, #42893, #38843, .T. ) ;
#18922 = CARTESIAN_POINT ( 'NONE',  ( -0.7545931758530177724, 0.2952755905511811885, 0.1292274648535926551 ) ) ;
#18923 = CARTESIAN_POINT ( 'NONE',  ( 0.3917322834645670104, 0.1049643490035304660, -1.538733226542994048 ) ) ;
#18924 = CARTESIAN_POINT ( 'NONE',  ( -1.167979002624671470, 0.05413385826771666132, 0.4176697321401328100 ) ) ;
#18925 = CARTESIAN_POINT ( 'NONE',  ( -0.1958661417322836718, 0.3392501089628017219, -2.774934383202099841 ) ) ;
#18926 = CARTESIAN_POINT ( 'NONE',  ( 1.154855643044620184, 0.1283753931104746893, -0.1820866141732285504 ) ) ;
#18927 = CARTESIAN_POINT ( 'NONE',  ( 1.010498687664042716, -0.4281496062992124485, 0.4176697321401328655 ) ) ;
#18928 = CARTESIAN_POINT ( 'NONE',  ( 0.5708661417322842269, 0.1660481256975885056, 0.3530559997133364547 ) ) ;
#18929 = CONICAL_SURFACE ( 'NONE', #29692, 1.889763779527559251, 0.7853981633974500554 ) ;
#18930 = CARTESIAN_POINT ( 'NONE',  ( 4.893765752498283924E-17, -0.3996062992125986035, -0.8661417322834645827 ) ) ;
#18931 = CARTESIAN_POINT ( 'NONE',  ( -1.148293963254592542, -0.6692913385826773087, -0.1292274648535924053 ) ) ;
#18932 = CARTESIAN_POINT ( 'NONE',  ( 0.2925321140481932369, 0.2925321140481932369, -0.5295275590551181688 ) ) ;
#18933 = CARTESIAN_POINT ( 'NONE',  ( 0.3996062992125984925, 0.1070741851644054637, -0.2014435695538057958 ) ) ;
#18934 = CARTESIAN_POINT ( 'NONE',  ( -0.06561679790026180015, -0.4281496062992127816, -0.4176697321401328100 ) ) ;
#18935 = CARTESIAN_POINT ( 'NONE',  ( -0.3996062992125986035, -0.1070741851644056997, -2.565616797900262647 ) ) ;
#18936 = CARTESIAN_POINT ( 'NONE',  ( -0.3392501089628017219, -0.1958661417322836718, -1.869422572178477848 ) ) ;
#18937 = CARTESIAN_POINT ( 'NONE',  ( 1.423884514435696191, -0.05778040916215522460, 0.4822834645669289988 ) ) ;
#18938 = CARTESIAN_POINT ( 'NONE',  ( 1.371391076115485941, 0.2952755905511811885, 0.1292274648535926551 ) ) ;
#18939 = CARTESIAN_POINT ( 'NONE',  ( 0.3543307086614181922, -0.5511811023622047445, 6.969142054262312111E-17 ) ) ;
#18940 = CARTESIAN_POINT ( 'NONE',  ( 0.8923884514435701520, -0.6046776061558809534, -0.2411417322834644161 ) ) ;
#18941 = CARTESIAN_POINT ( 'NONE',  ( 0.3458507752293908943, 0.3458507752293908943, -1.474409448818897683 ) ) ;
#18942 = CARTESIAN_POINT ( 'NONE',  ( 0.3083989501312343062, -0.08942795157528024563, -0.3641732283464568787 ) ) ;
#18943 = CARTESIAN_POINT ( 'NONE',  ( 0.5249343832021003964, 0.2306618581243847221, -0.2411417322834647770 ) ) ;
#18944 = CARTESIAN_POINT ( 'NONE',  ( 0.3420746716998660508, -0.1974969037888704149, -0.9691601049868767692 ) ) ;
#18945 = CARTESIAN_POINT ( 'NONE',  ( -1.318897637795274802, -0.5400638737290845981, -0.3530559997133363437 ) ) ;
#18946 = CARTESIAN_POINT ( 'NONE',  ( 0.9055118110236227702, -0.5511811023622047445, 6.969142054262312111E-17 ) ) ;
#18947 = AXIS2_PLACEMENT_3D ( 'NONE', #15191, #58961, #26128 ) ;
#18948 = CARTESIAN_POINT ( 'NONE',  ( -1.161417322834644716, 0.1660481256975885056, 0.3530559997133364547 ) ) ;
#18949 = CARTESIAN_POINT ( 'NONE',  ( -0.2559055118110230564, 0.1660481256975883668, -0.3530559997133364547 ) ) ;
#18950 = CARTESIAN_POINT ( 'NONE',  ( -0.2362204724409440182, -0.1870078740157479769, 0.3641732283464567677 ) ) ;
#18951 = FACE_OUTER_BOUND ( 'NONE', #66542, .T. ) ;
#18952 = CARTESIAN_POINT ( 'NONE',  ( -0.1509186351706028884, -0.05778040916215522460, 0.4822834645669289988 ) ) ;
#18953 = CARTESIAN_POINT ( 'NONE',  ( 0.1443569553805781891, -0.3690944881889763329, 0.3153832671262228327 ) ) ;
#18954 = CARTESIAN_POINT ( 'NONE',  ( 0.3996062992125986035, -0.1070741851644052972, -2.078083989501312345 ) ) ;
#18955 = CARTESIAN_POINT ( 'NONE',  ( 0.02624671916010564918, -0.6046776061558809534, -0.2411417322834644161 ) ) ;
#18956 = CARTESIAN_POINT ( 'NONE',  ( 1.364829396325460076, 0.1283753931104748280, 0.1820866141732283561 ) ) ;
#18957 = CARTESIAN_POINT ( 'NONE',  ( -0.1685779992553458895, 5.625543525484885637E-15, -0.3954974714151418547 ) ) ;
#18958 = CARTESIAN_POINT ( 'NONE',  ( -0.9383202099737524282, -0.08942795157527998196, 0.3641732283464567121 ) ) ;
#18959 = CARTESIAN_POINT ( 'NONE',  ( -0.6167979002624665030, -0.004921259842519576551, 0.3153832671262227771 ) ) ;
#18960 = CARTESIAN_POINT ( 'NONE',  ( -0.1049868766404193215, -0.6046776061558807314, 0.2411417322834647770 ) ) ;
#18961 = CARTESIAN_POINT ( 'NONE',  ( -0.2034120734908131112, -0.6692913385826773087, -0.1292274648535924053 ) ) ;
#18962 = CARTESIAN_POINT ( 'NONE',  ( 0.9251968503937015864, 0.07958543189024071263, -0.2665933059059888421 ) ) ;
#18963 = CARTESIAN_POINT ( 'NONE',  ( -1.732283464566928277, -0.1870078740157479769, 0.3641732283464567677 ) ) ;
#18964 = CARTESIAN_POINT ( 'NONE',  ( -1.666666666666665853, 0.05413385826771626580, -0.4176697321401330321 ) ) ;
#18965 = CARTESIAN_POINT ( 'NONE',  ( 0.8267716535433078384, -0.6692913385826771977, 8.415575281601705876E-17 ) ) ;
#18966 = CARTESIAN_POINT ( 'NONE',  ( 0.4567115769096108391, 1.408171547189567274, -2.130996229389289010 ) ) ;
#18967 = CARTESIAN_POINT ( 'NONE',  ( -0.4593175853018366950, 0.05413385826771666132, 0.4176697321401328100 ) ) ;
#18968 = CARTESIAN_POINT ( 'NONE',  ( 4.797336870675656522E-17, -0.3917322834645670104, -0.9507874015748032370 ) ) ;
#18969 = CARTESIAN_POINT ( 'NONE',  ( -1.325459317585300889, -0.4281496062992127816, -0.4176697321401328100 ) ) ;
#18970 = CARTESIAN_POINT ( 'NONE',  ( 0.9120734908136490793, 0.2952755905511810774, -0.1292274648535930714 ) ) ;
#18971 = CARTESIAN_POINT ( 'NONE',  ( 0.4593175853018380828, 0.05413385826771626580, -0.4176697321401330321 ) ) ;
#18972 = CARTESIAN_POINT ( 'NONE',  ( -0.03101198675153587700, 1.063748311984392902, -3.936916529678083254 ) ) ;
#18973 = CARTESIAN_POINT ( 'NONE',  ( 0.5708661417322842269, 0.07958543189024085140, 0.2665933059059887866 ) ) ;
#18974 = CARTESIAN_POINT ( 'NONE',  ( 1.351706036745407680, 0.05413385826771666132, 0.4176697321401328100 ) ) ;
#18975 = CARTESIAN_POINT ( 'NONE',  ( -0.4921259842519677963, -0.4536011799217367080, 0.2665933059059888421 ) ) ;
#18976 = CARTESIAN_POINT ( 'NONE',  ( -0.6496062992125976043, 0.1660481256975883668, -0.3530559997133364547 ) ) ;
#18977 = CARTESIAN_POINT ( 'NONE',  ( 0.8070866141732288002, 0.1660481256975885056, 0.3530559997133364547 ) ) ;
#18978 = CARTESIAN_POINT ( 'NONE',  ( 0.3412073490813655186, 0.2306618581243848609, 0.2411417322834645549 ) ) ;
#18979 = CARTESIAN_POINT ( 'NONE',  ( -0.5839895013123351797, -0.6692913385826771977, 0.1292274648535927661 ) ) ;
#18980 = CARTESIAN_POINT ( 'NONE',  ( -0.5446194225721777693, -0.2845877964562161244, -0.3641732283464567121 ) ) ;
#18981 = VECTOR ( 'NONE', #82461, 39.37007874015748143 ) ;
#18982 = CARTESIAN_POINT ( 'NONE',  ( 0.2952755905511816326, -0.5400638737290844871, 0.3530559997133364547 ) ) ;
#18983 = CARTESIAN_POINT ( 'NONE',  ( -1.062992125984250968, 0.2952755905511811885, 0.000000000000000000 ) ) ;
#18984 = CARTESIAN_POINT ( 'NONE',  ( -0.5511811023622038563, -0.1870078740157479769, 0.4822834645669291653 ) ) ;
#18985 = CARTESIAN_POINT ( 'NONE',  ( -0.1265901696524986964, -0.4724409448818899238, -0.5446194225721784354 ) ) ;
#18987 = CARTESIAN_POINT ( 'NONE',  ( 1.181102362204724976, -0.1870078740157480879, -0.4822834645669291653 ) ) ;
#18986 = CARTESIAN_POINT ( 'NONE',  ( -2.130073781772672259, 0.01305114060239450161, 0.4563452811745689064 ) ) ;
#18988 = CARTESIAN_POINT ( 'NONE',  ( 1.384514435695538559, 0.2952755905511810774, -0.1292274648535930714 ) ) ;
#18989 = DIRECTION ( 'NONE',  ( 1.445602896647338917E-16, 1.000000000000000000, 0.000000000000000000 ) ) ;
#18990 = CARTESIAN_POINT ( 'NONE',  ( 3.937007874015748143, 2.755905511811024056, 0.5314960629921260393 ) ) ;
#18991 = CARTESIAN_POINT ( 'NONE',  ( -0.8136482939632537770, -0.6046776061558807314, 0.2411417322834647770 ) ) ;
#18992 = CARTESIAN_POINT ( 'NONE',  ( -0.2362204724409451284, 0.4091458600556402425, -0.3280839895013123453 ) ) ;
#18993 = CARTESIAN_POINT ( 'NONE',  ( 0.3996062992125986035, 2.446882876249141962E-17, -0.1181102362204724671 ) ) ;
#18994 = EDGE_LOOP ( 'NONE', ( #23083, #37151, #14185, #55885 ) ) ;
#18995 = CARTESIAN_POINT ( 'NONE',  ( -0.1312335958005241554, -0.5023911411419708095, -0.1820866141732282451 ) ) ;
#18996 = CARTESIAN_POINT ( 'NONE',  ( -0.3392501089628017219, -0.1958661417322836718, -1.304461942257217899 ) ) ;
#18997 = CARTESIAN_POINT ( 'NONE',  ( 0.8202099737532813073, 0.2952755905511811885, 0.1292274648535926551 ) ) ;
#18998 = CARTESIAN_POINT ( 'NONE',  ( 0.2362204724409451007, -0.4091458600556402980, -2.769028871391076230 ) ) ;
#18999 = DIRECTION ( 'NONE',  ( -3.096699300667737957E-16, 1.000000000000000000, -0.000000000000000000 ) ) ;
#19000 = CARTESIAN_POINT ( 'NONE',  ( -0.4199475065616791736, -0.5023911411419708095, 0.1820866141732285504 ) ) ;
#19001 = LENGTH_MEASURE_WITH_UNIT ( LENGTH_MEASURE( 0.02539999999999999897 ), #20263 );
#19002 = CARTESIAN_POINT ( 'NONE',  ( 1.141732283464567788, -0.6692913385826771977, 8.415575281601705876E-17 ) ) ;
#19003 = CARTESIAN_POINT ( 'NONE',  ( 0.9908136482939640111, 0.1771653543307087075, -0.09757992244046823083 ) ) ;
#19004 = CARTESIAN_POINT ( 'NONE',  ( 0.1640419947506569498, -0.3162353388693409650, -0.4822834645669289433 ) ) ;
#19005 = CARTESIAN_POINT ( 'NONE',  ( -0.3392501089628018329, -0.1958661417322836440, -0.7624478758192109185 ) ) ;
#19006 = CARTESIAN_POINT ( 'NONE',  ( -0.3149606299212590610, -0.1870078740157480879, -0.4822834645669291653 ) ) ;
#19007 = CARTESIAN_POINT ( 'NONE',  ( -1.122047244094487306, -0.4536011799217367080, 0.2665933059059888421 ) ) ;
#19008 = EDGE_CURVE ( 'NONE', #27226, #34463, #561, .T. ) ;
#19009 = CARTESIAN_POINT ( 'NONE',  ( -0.4986876640419942164, -0.6046776061558807314, 0.2411417322834647770 ) ) ;
#19010 = FACE_OUTER_BOUND ( 'NONE', #56271, .T. ) ;
#19011 = DIRECTION ( 'NONE',  ( 0.000000000000000000, -0.000000000000000000, 1.000000000000000000 ) ) ;
#19012 = EDGE_LOOP ( 'NONE', ( #25528, #44144, #10144, #81437, #381, #2665 ) ) ;
#19013 = CARTESIAN_POINT ( 'NONE',  ( 0.3917322834645670104, 0.1049643490035304660, -1.853693856464253997 ) ) ;
#19014 = CARTESIAN_POINT ( 'NONE',  ( 0.4133858267716541968, 0.1660481256975885056, 0.3530559997133364547 ) ) ;
#19015 = VERTEX_POINT ( 'NONE', #9775 ) ;
#19016 = CARTESIAN_POINT ( 'NONE',  ( -0.6233595800524928121, -0.05778040916215522460, 0.4822834645669289988 ) ) ;
#19017 = CARTESIAN_POINT ( 'NONE',  ( 1.509186351706037543, -0.4281496062992127816, -0.4176697321401328100 ) ) ;
#19018 = CARTESIAN_POINT ( 'NONE',  ( 0.7086614173228352742, -0.1870078740157480879, -0.4822834645669291653 ) ) ;
#19019 = EDGE_CURVE ( 'NONE', #16885, #38903, #42576, .T. ) ;
#19020 = CARTESIAN_POINT ( 'NONE',  ( 0.08530183727034192087, -0.05778040916215522460, 0.4822834645669289988 ) ) ;
#19021 = CARTESIAN_POINT ( 'NONE',  ( -0.3917322834645670104, -7.196005306013484475E-17, -1.383858267716535417 ) ) ;
#19022 = CARTESIAN_POINT ( 'NONE',  ( -0.8267716535433065062, -0.6692913385826771977, 8.415575281601705876E-17 ) ) ;
#19023 = CARTESIAN_POINT ( 'NONE',  ( -0.09842519685039295696, -0.5400638737290844871, 0.3530559997133364547 ) ) ;
#19024 = CARTESIAN_POINT ( 'NONE',  ( -1.076115485564303809, -0.6046776061558809534, -0.2411417322834644161 ) ) ;
#19025 = CARTESIAN_POINT ( 'NONE',  ( 0.04593175853018440641, -0.5511811023622046335, 0.09757992244046803654 ) ) ;
#19026 = CARTESIAN_POINT ( 'NONE',  ( 3.937007874015748143, 2.755905511811024056, -0.5314960629921260393 ) ) ;
#19027 = CARTESIAN_POINT ( 'NONE',  ( -0.1968503937007867743, -0.6692913385826771977, 8.415575281601705876E-17 ) ) ;
#19028 = CARTESIAN_POINT ( 'NONE',  ( 2.787279214012418738, 0.000000000000000000, 0.000000000000000000 ) ) ;
#19029 = CARTESIAN_POINT ( 'NONE',  ( 1.292650918635171564, 0.2952755905511811885, 0.1292274648535926551 ) ) ;
#19030 = CARTESIAN_POINT ( 'NONE',  ( 0.3917322834645670104, -0.1049643490035303411, -2.938320209973753538 ) ) ;
#19031 = ORIENTED_EDGE ( 'NONE', *, *, #37866, .T. ) ;
#19032 = EDGE_LOOP ( 'NONE', ( #25530, #80113, #52258, #80232 ) ) ;
#19033 = CARTESIAN_POINT ( 'NONE',  ( 0.09842519685039434474, 0.1660481256975885056, 0.3530559997133364547 ) ) ;
#19034 = CARTESIAN_POINT ( 'NONE',  ( -0.4658792650918627265, -0.08942795157527998196, 0.3641732283464567121 ) ) ;
#19036 = DIRECTION ( 'NONE',  ( 1.000000000000000000, 0.000000000000000000, 0.000000000000000000 ) ) ;
#19035 = CARTESIAN_POINT ( 'NONE',  ( 1.581364829396326277, -0.2845877964562161244, -0.3641732283464567121 ) ) ;
#19037 = CARTESIAN_POINT ( 'NONE',  ( -9.594673741351313045E-17, 0.3917322834645670104, -1.187007874015748143 ) ) ;
#19038 = CARTESIAN_POINT ( 'NONE',  ( -0.4724409448818898682, -8.678599364036362592E-17, -0.1161417322834645827 ) ) ;
#19039 = CARTESIAN_POINT ( 'NONE',  ( 2.130073781772669150, 0.01305114060239445997, -0.4563452811745837834 ) ) ;
#19040 = CARTESIAN_POINT ( 'NONE',  ( 1.555118110236221041, -0.5400638737290844871, 0.3530559997133364547 ) ) ;
#19041 = CARTESIAN_POINT ( 'NONE',  ( -0.3949938075777408852, -0.1058382717557502933, 0.1922572178477690297 ) ) ;
#19042 = CARTESIAN_POINT ( 'NONE',  ( 0.4724409448818904789, -0.1870078740157479769, 0.4822834645669291653 ) ) ;
#19043 = CARTESIAN_POINT ( 'NONE',  ( -1.049868766404198794, -0.6046776061558807314, 0.2411417322834647770 ) ) ;
#19044 = CARTESIAN_POINT ( 'NONE',  ( -0.9908136482939626788, -0.6692913385826773087, -0.1292274648535924053 ) ) ;
#19045 = CARTESIAN_POINT ( 'NONE',  ( 0.2034120734908142214, 0.2952755905511810774, -0.1292274648535930714 ) ) ;
#19046 = CARTESIAN_POINT ( 'NONE',  ( 0.3949938075777409963, 2.418639510665530743E-17, -0.1948818897637795700 ) ) ;
#19047 = CARTESIAN_POINT ( 'NONE',  ( -1.496062992125983815, -0.1870078740157479769, 0.3641732283464567677 ) ) ;
#19048 = CARTESIAN_POINT ( 'NONE',  ( 0.8464566929133865436, 0.1660481256975883668, -0.3530559997133364547 ) ) ;
#19049 = CARTESIAN_POINT ( 'NONE',  ( 1.325459317585302665, -0.3690944881889763329, 0.3153832671262228327 ) ) ;
#19050 = CARTESIAN_POINT ( 'NONE',  ( 1.220472440944881942, 2.401574803149606474, -0.5309055118110238558 ) ) ;
#19051 = CARTESIAN_POINT ( 'NONE',  ( 0.7086614173228353852, -0.1870078740157479769, 0.3641732283464567677 ) ) ;
#19052 = CARTESIAN_POINT ( 'NONE',  ( -1.240157480314959759, -0.5400638737290845981, -0.3530559997133363437 ) ) ;
#19053 = CARTESIAN_POINT ( 'NONE',  ( 0.3996062992125984925, 0.1070741851644054637, -0.9888451443569553634 ) ) ;
#19054 = CARTESIAN_POINT ( 'NONE',  ( 1.122047244094488860, -0.5400638737290845981, -0.3530559997133363437 ) ) ;
#19055 = CARTESIAN_POINT ( 'NONE',  ( -0.3392501089628017219, -0.1958661417322836718, -0.04461942257217842850 ) ) ;
#19057 = CARTESIAN_POINT ( 'NONE',  ( -0.4725409811167128882, 1.494519345219277762, 2.165580946493155690 ) ) ;
#19056 = CARTESIAN_POINT ( 'NONE',  ( 0.5774278215223104249, 0.2306618581243848609, 0.2411417322834645549 ) ) ;
#19058 = CARTESIAN_POINT ( 'NONE',  ( -1.640419947506561060, -0.3690944881889765550, -0.3153832671262227771 ) ) ;
#19059 = CARTESIAN_POINT ( 'NONE',  ( 0.1049868766404206816, 0.2306618581243848609, 0.2411417322834645549 ) ) ;
#19060 = CARTESIAN_POINT ( 'NONE',  ( 0.8398950131233602345, 0.1283753931104746893, -0.1820866141732285504 ) ) ;
#19061 = CARTESIAN_POINT ( 'NONE',  ( 0.8595800524934390507, -0.3162353388693405765, 0.4822834645669290543 ) ) ;
#19062 = CARTESIAN_POINT ( 'NONE',  ( 0.6299212598425100174, 2.165354330708661568, 0.9285414500055780840 ) ) ;
#19063 = CARTESIAN_POINT ( 'NONE',  ( -0.7086614173228339419, -0.1870078740157480601, -0.3641732283464567677 ) ) ;
#19064 = CARTESIAN_POINT ( 'NONE',  ( -0.7545931758530177724, 0.2952755905511811885, 0.1292274648535926551 ) ) ;
#19065 = CARTESIAN_POINT ( 'NONE',  ( 1.561679790026247350, 0.05413385826771626580, -0.4176697321401330321 ) ) ;
#19066 = CARTESIAN_POINT ( 'NONE',  ( -1.102362204724408601, -0.1870078740157479769, 0.4822834645669291653 ) ) ;
#19067 = CARTESIAN_POINT ( 'NONE',  ( 1.023622047244095334, -0.1870078740157479769, 0.4822834645669291653 ) ) ;
#19068 = CARTESIAN_POINT ( 'NONE',  ( -0.1049643490035302301, -0.3917322834645671770, -0.8563185283802644543 ) ) ;
#19069 = CARTESIAN_POINT ( 'NONE',  ( -1.535433070866141225, -0.5511811023622047445, 6.969142054262312111E-17 ) ) ;
#19070 = CARTESIAN_POINT ( 'NONE',  ( 1.018309906596789771, 1.474507693700183308, 0.4712541672117732672 ) ) ;
#19071 = CARTESIAN_POINT ( 'NONE',  ( 0.9251968503937015864, -0.5400638737290844871, 0.3530559997133364547 ) ) ;
#19072 = CARTESIAN_POINT ( 'NONE',  ( -0.3458507752293909498, 0.3458507752293907833, -2.616141732283464805 ) ) ;
#19073 = CARTESIAN_POINT ( 'NONE',  ( -1.555118110236219930, 0.1660481256975885056, 0.3530559997133364547 ) ) ;
#19074 = CARTESIAN_POINT ( 'NONE',  ( -1.345144356955379816, -0.2845877964562159024, 0.3641732283464567677 ) ) ;
#19075 = CARTESIAN_POINT ( 'NONE',  ( -1.220472440944881054, 0.1771653543307087630, 0.000000000000000000 ) ) ;
#19076 = CARTESIAN_POINT ( 'NONE',  ( 1.620734908136483465, -0.5511811023622046335, 0.09757992244046803654 ) ) ;
#19077 = CARTESIAN_POINT ( 'NONE',  ( -0.4658792650918627265, -0.3162353388693409650, -0.4822834645669289433 ) ) ;
#19078 = CARTESIAN_POINT ( 'NONE',  ( -0.3674540682414689785, 0.1283753931104748280, 0.1820866141732283561 ) ) ;
#19079 = CARTESIAN_POINT ( 'NONE',  ( -1.535433070866141225, 0.1771653543307087630, 0.000000000000000000 ) ) ;
#19080 = CARTESIAN_POINT ( 'NONE',  ( 1.115485564304462551, -0.004921259842519576551, 0.3153832671262227771 ) ) ;
#19081 = CARTESIAN_POINT ( 'NONE',  ( 1.003937007874016407, -0.5400638737290844871, 0.3530559997133364547 ) ) ;
#19082 = CARTESIAN_POINT ( 'NONE',  ( 1.371391076115485719, -0.6692913385826773087, -0.1292274648535924053 ) ) ;
#19083 = CARTESIAN_POINT ( 'NONE',  ( -0.1115485564304453947, -0.5511811023622046335, 0.09757992244046803654 ) ) ;
#19084 = EDGE_CURVE ( 'NONE', #17596, #69360, #65097, .T. ) ;
#19085 = CARTESIAN_POINT ( 'NONE',  ( 0.3937007874015754361, -0.1870078740157479769, 0.4822834645669291653 ) ) ;
#19086 = CARTESIAN_POINT ( 'NONE',  ( 0.5577427821522314977, -0.2845877964562161244, -0.3641732283464567121 ) ) ;
#19087 = CARTESIAN_POINT ( 'NONE',  ( 1.443569553805774897, 0.2306618581243848609, 0.2411417322834645549 ) ) ;
#19088 = CARTESIAN_POINT ( 'NONE',  ( -1.496062992125983815, -0.1870078740157479769, 0.4822834645669291653 ) ) ;
#19089 = CARTESIAN_POINT ( 'NONE',  ( -0.4921259842519677963, -0.5400638737290844871, 0.3530559997133364547 ) ) ;
#19090 = CARTESIAN_POINT ( 'NONE',  ( -0.3996062992125986590, 0.1070741851644051862, -0.3477690288713910505 ) ) ;
#19091 = CARTESIAN_POINT ( 'NONE',  ( 0.1070741851644054776, -0.3996062992125984925, -2.681758530183727895 ) ) ;
#19092 = CARTESIAN_POINT ( 'NONE',  ( 0.3805774278215230400, 0.05413385826771626580, -0.4176697321401330321 ) ) ;
#19093 = CARTESIAN_POINT ( 'NONE',  ( 1.167979002624672580, -0.004921259842519870586, -0.3153832671262229437 ) ) ;
#19094 = CARTESIAN_POINT ( 'NONE',  ( -0.5643044619422565855, -0.4281496062992124485, 0.4176697321401328655 ) ) ;
#19095 = CARTESIAN_POINT ( 'NONE',  ( 0.5118110236220478892, 0.2952755905511811885, 0.000000000000000000 ) ) ;
#19096 = CARTESIAN_POINT ( 'NONE',  ( 4.893765752498283924E-17, -0.3996062992125986035, -2.125984251968504157 ) ) ;
#19097 = CARTESIAN_POINT ( 'NONE',  ( -0.1058382717557503211, 0.3949938075777409408, -1.581364829396325389 ) ) ;
#19098 = CARTESIAN_POINT ( 'NONE',  ( -0.3996062992125986035, -0.1070741851644056997, -2.723097112860892288 ) ) ;
#19099 = CARTESIAN_POINT ( 'NONE',  ( -0.4848604877838266214, -2.609869883881465018E-15, -0.3464511005275220379 ) ) ;
#19100 = CARTESIAN_POINT ( 'NONE',  ( -0.2867679344610366554, 0.2867679344610365444, -1.114173228346456490 ) ) ;
#19101 = CARTESIAN_POINT ( 'NONE',  ( -1.056430446194224881, 0.1771653543307087075, -0.09757992244046823083 ) ) ;
#19102 = CARTESIAN_POINT ( 'NONE',  ( -1.141732283464566011, -0.6692913385826771977, 8.415575281601705876E-17 ) ) ;
#19103 = VECTOR ( 'NONE', #61128, 39.37007874015748143 ) ;
#19104 = CARTESIAN_POINT ( 'NONE',  ( -0.3420746716998660508, -0.1974969037888706924, -2.648950131233596128 ) ) ;
#19105 = CARTESIAN_POINT ( 'NONE',  ( 0.9120734908136490793, 0.2952755905511810774, -0.1292274648535930714 ) ) ;
#19106 = CARTESIAN_POINT ( 'NONE',  ( 1.430446194225722500, 0.05413385826771666132, 0.4176697321401328100 ) ) ;
#19107 = CARTESIAN_POINT ( 'NONE',  ( 0.9055118110236227702, -0.6692913385826771977, 8.415575281601705876E-17 ) ) ;
#19108 = CARTESIAN_POINT ( 'NONE',  ( 0.4724409448818898682, 2.892866454678787531E-17, -2.952755905511811108 ) ) ;
#19109 = CARTESIAN_POINT ( 'NONE',  ( -0.2925321140481932924, 0.2925321140481931814, -2.066929133858267154 ) ) ;
#19110 = CARTESIAN_POINT ( 'NONE',  ( 1.522309711286089939, 0.2306618581243848609, 0.2411417322834645549 ) ) ;
#19111 = CARTESIAN_POINT ( 'NONE',  ( 0.5380577427821529035, 0.05413385826771626580, -0.4176697321401330321 ) ) ;
#19112 = CARTESIAN_POINT ( 'NONE',  ( 0.5511811023622054106, -0.1870078740157480879, -0.4822834645669291653 ) ) ;
#19113 = CARTESIAN_POINT ( 'NONE',  ( 0.7152230971128614723, -0.2845877964562161244, -0.3641732283464567121 ) ) ;
#19114 = CARTESIAN_POINT ( 'NONE',  ( 1.187664041994751285, -0.05778040916215522460, 0.4822834645669289988 ) ) ;
#19115 = CARTESIAN_POINT ( 'NONE',  ( -0.2867679344610364334, -0.2867679344610367109, 0.01377952755905502598 ) ) ;
#19116 = CARTESIAN_POINT ( 'NONE',  ( 0.5052493438320215802, 0.2952755905511811885, 0.1292274648535926551 ) ) ;
#19117 = CARTESIAN_POINT ( 'NONE',  ( 1.154855643044620184, -0.6046776061558807314, 0.2411417322834647770 ) ) ;
#19118 = CARTESIAN_POINT ( 'NONE',  ( 0.2034120734908144990, -0.6692913385826771977, 0.1292274648535927661 ) ) ;
#19119 = CARTESIAN_POINT ( 'NONE',  ( 1.272965879265092637, -0.3690944881889765550, -0.3153832671262227771 ) ) ;
#19120 = CARTESIAN_POINT ( 'NONE',  ( -0.7217847769028863381, 0.05413385826771626580, -0.4176697321401330321 ) ) ;
#19121 = CARTESIAN_POINT ( 'NONE',  ( -1.128608923884513837, -0.6046776061558807314, 0.2411417322834647770 ) ) ;
#19122 = CARTESIAN_POINT ( 'NONE',  ( 1.135170603674541256, 0.2952755905511811885, 0.1292274648535926551 ) ) ;
#19123 = CARTESIAN_POINT ( 'NONE',  ( 4.797336870675656522E-17, -0.3917322834645670104, -0.6358267716535433989 ) ) ;
#19124 = CARTESIAN_POINT ( 'NONE',  ( -0.1049643490035302024, -0.3917322834645671215, -1.639107611548556109 ) ) ;
#19125 = CARTESIAN_POINT ( 'NONE',  ( -0.1049643490035302024, -0.3917322834645671215, -2.741469816272964710 ) ) ;
#19126 = ORIENTED_EDGE ( 'NONE', *, *, #73907, .F. ) ;
#19127 = CARTESIAN_POINT ( 'NONE',  ( -0.2925321140481932924, 0.2925321140481931814, -0.01968503937007875723 ) ) ;
#19128 = ORIENTED_EDGE ( 'NONE', *, *, #83089, .F. ) ;
#19129 = CARTESIAN_POINT ( 'NONE',  ( 1.666666666666667185, 0.05413385826771666132, 0.4176697321401328100 ) ) ;
#19130 = CARTESIAN_POINT ( 'NONE',  ( 1.233595800524935227, -0.5023911411419708095, 0.1820866141732285504 ) ) ;
#19131 = CARTESIAN_POINT ( 'NONE',  ( -0.2925321140481930704, -0.2925321140481933480, -1.318897637795275690 ) ) ;
#19132 = CARTESIAN_POINT ( 'NONE',  ( 1.286089238845145033, -0.5023911411419708095, -0.1820866141732282451 ) ) ;
#19133 = CARTESIAN_POINT ( 'NONE',  ( 0.4724409448818897017, 0.1265901696524990294, -2.406167979002624246 ) ) ;
#19134 = CARTESIAN_POINT ( 'NONE',  ( -0.2512006810191820261, 1.134651008203183986, 2.808392084767333596 ) ) ;
#19135 = DIRECTION ( 'NONE',  ( 1.000000000000000000, 0.000000000000000000, -0.000000000000000000 ) ) ;
#19136 = CARTESIAN_POINT ( 'NONE',  ( 0.1958661417322836440, -0.3392501089628017219, -0.6489501312335959060 ) ) ;
#19137 = CARTESIAN_POINT ( 'NONE',  ( -0.7349081364829387342, -0.5023911411419708095, 0.1820866141732285504 ) ) ;
#19138 = CARTESIAN_POINT ( 'NONE',  ( 1.607611548556431069, 0.2952755905511811885, 0.1292274648535926551 ) ) ;
#19139 = CARTESIAN_POINT ( 'NONE',  ( -1.213910761154854745, -0.6692913385826771977, 0.1292274648535927661 ) ) ;
#19140 = CARTESIAN_POINT ( 'NONE',  ( 0.1312335958005255154, -0.6046776061558807314, 0.2411417322834647770 ) ) ;
#19141 = CARTESIAN_POINT ( 'NONE',  ( 1.318897637795276356, 0.1660481256975883668, -0.3530559997133364547 ) ) ;
#19142 = ORIENTED_EDGE ( 'NONE', *, *, #29607, .T. ) ;
#19143 = EDGE_CURVE ( 'NONE', #31453, #28229, #54477, .T. ) ;
#19144 = DIRECTION ( 'NONE',  ( 0.000000000000000000, 1.000000000000000000, 0.000000000000000000 ) ) ;
#19145 = CARTESIAN_POINT ( 'NONE',  ( -0.4091458600556402980, -0.2362204724409451284, -2.099737532808398921 ) ) ;
#19146 = DIRECTION ( 'NONE',  ( 1.000000000000000000, -0.000000000000000000, -0.000000000000000000 ) ) ;
#19147 = CARTESIAN_POINT ( 'NONE',  ( -0.5905511811023613777, -0.5511811023622047445, 6.969142054262312111E-17 ) ) ;
#19148 = CARTESIAN_POINT ( 'NONE',  ( -1.194225721784776262, -0.4281496062992124485, 0.4176697321401328655 ) ) ;
#19149 = CARTESIAN_POINT ( 'NONE',  ( 1.017060367454068803, -0.3162353388693405765, 0.4822834645669290543 ) ) ;
#19150 = VERTEX_POINT ( 'NONE', #28297 ) ;
#19152 = DIRECTION ( 'NONE',  ( -1.000000000000000000, -8.326672684688674053E-16, 0.000000000000000000 ) ) ;
#19151 = CARTESIAN_POINT ( 'NONE',  ( 0.000000000000000000, 2.755905511811024056, 0.000000000000000000 ) ) ;
#19153 = CARTESIAN_POINT ( 'NONE',  ( 1.135170603674541256, -0.6692913385826773087, -0.1292274648535924053 ) ) ;
#19154 = CARTESIAN_POINT ( 'NONE',  ( -1.154855643044618851, -0.6046776061558809534, -0.2411417322834644161 ) ) ;
#19155 = CARTESIAN_POINT ( 'NONE',  ( -9.594673741351310580E-17, 0.3917322834645669549, -0.7099544374990010009 ) ) ;
#19156 = AXIS2_PLACEMENT_3D ( 'NONE', #63761, #12846, #50301 ) ;
#19157 = CARTESIAN_POINT ( 'NONE',  ( -0.5774278215223089816, 0.1283753931104746893, -0.1820866141732285504 ) ) ;
#19158 = CARTESIAN_POINT ( 'NONE',  ( 0.1958661417322836440, -0.3392501089628017219, -0.6489501312335959060 ) ) ;
#19159 = CARTESIAN_POINT ( 'NONE',  ( -0.4724409448818890911, -0.1870078740157480601, -0.3641732283464567677 ) ) ;
#19160 = CARTESIAN_POINT ( 'NONE',  ( 0.05905511811023681640, 0.07958543189024071263, -0.2665933059059888421 ) ) ;
#19161 = CARTESIAN_POINT ( 'NONE',  ( -0.03280839895013062252, -0.6692913385826771977, 0.1292274648535927661 ) ) ;
#19162 = CARTESIAN_POINT ( 'NONE',  ( -1.318897637795274802, 0.07958543189024085140, 0.2665933059059887866 ) ) ;
#19163 = CARTESIAN_POINT ( 'NONE',  ( -9.594673741351313045E-17, 0.3917322834645670104, -2.669291338582676865 ) ) ;
#19164 = CARTESIAN_POINT ( 'NONE',  ( 1.332020997375328974, -0.05778040916215560624, -0.4822834645669293319 ) ) ;
#19165 = EDGE_CURVE ( 'NONE', #56613, #48835, #80168, .T. ) ;
#19166 = EDGE_CURVE ( 'NONE', #25602, #24503, #61112, .T. ) ;
#19167 = CARTESIAN_POINT ( 'NONE',  ( -1.364829396325458521, -0.6046776061558807314, 0.2411417322834647770 ) ) ;
#19168 = CARTESIAN_POINT ( 'NONE',  ( 0.4091458600556403535, 0.2362204724409449896, -1.152887139107611425 ) ) ;
#19169 = CARTESIAN_POINT ( 'NONE',  ( -0.2559055118110230564, 0.1660481256975883668, -0.3530559997133364547 ) ) ;
#19170 = CARTESIAN_POINT ( 'NONE',  ( -0.7742782152230962556, -0.4281496062992127816, -0.4176697321401328100 ) ) ;
#19171 = CARTESIAN_POINT ( 'NONE',  ( 0.7349081364829403995, 0.1283753931104748280, 0.1820866141732283561 ) ) ;
#19172 = CARTESIAN_POINT ( 'NONE',  ( -0.1968503937007867743, -0.5511811023622047445, 6.969142054262312111E-17 ) ) ;
#19173 = CARTESIAN_POINT ( 'NONE',  ( -0.7545931758530177724, 0.2952755905511811885, 0.1292274648535926551 ) ) ;
#19174 = CARTESIAN_POINT ( 'NONE',  ( -1.036745406824146176, -0.4281496062992124485, 0.4176697321401328655 ) ) ;
#19175 = CYLINDRICAL_SURFACE ( 'NONE', #39389, 0.4724409448818898682 ) ;
#19176 = CARTESIAN_POINT ( 'NONE',  ( 1.332020997375329197, -0.2845877964562159024, 0.3641732283464567677 ) ) ;
#19177 = CARTESIAN_POINT ( 'NONE',  ( -0.2821522309711278487, -0.6692913385826773087, -0.1292274648535924053 ) ) ;
#19178 = CARTESIAN_POINT ( 'NONE',  ( -1.371391076115484831, 0.2952755905511810774, -0.1292274648535930714 ) ) ;
#19179 = ORIENTED_EDGE ( 'NONE', *, *, #30323, .F. ) ;
#19180 = CARTESIAN_POINT ( 'NONE',  ( 0.3996062992125986035, -0.1070741851644052972, -2.393044619422572072 ) ) ;
#19181 = CARTESIAN_POINT ( 'NONE',  ( -0.8595800524934373854, -0.08942795157527998196, 0.3641732283464567121 ) ) ;
#19182 = CARTESIAN_POINT ( 'NONE',  ( 0.6430446194225728496, 0.05413385826771666132, 0.4176697321401328100 ) ) ;
#19183 = CARTESIAN_POINT ( 'NONE',  ( -0.8858267716535425107, 0.07958543189024071263, -0.2665933059059888421 ) ) ;
#19184 = CARTESIAN_POINT ( 'NONE',  ( -0.2925321140481930149, -0.2925321140481933480, -1.553149606299212726 ) ) ;
#19185 = CARTESIAN_POINT ( 'NONE',  ( -0.8005249343832013809, -0.4281496062992124485, 0.4176697321401328655 ) ) ;
#19186 = CARTESIAN_POINT ( 'NONE',  ( 0.7677165354330716118, 0.1660481256975883668, -0.3530559997133364547 ) ) ;
#19187 = CARTESIAN_POINT ( 'NONE',  ( 0.6824146981627303710, -0.6046776061558807314, 0.2411417322834647770 ) ) ;
#19188 = CARTESIAN_POINT ( 'NONE',  ( 0.5314960629921322566, 2.755905511811024056, -1.813482582612291782 ) ) ;
#19189 = CARTESIAN_POINT ( 'NONE',  ( -1.450131233595799651, -0.5511811023622046335, 0.09757992244046803654 ) ) ;
#19190 = CARTESIAN_POINT ( 'NONE',  ( 0.3460692066303958092, 0.1998031496062993018, -0.6804461942257218343 ) ) ;
#19191 = CARTESIAN_POINT ( 'NONE',  ( 0.3460692066303959757, -0.1998031496062991907, -0.7349081364829396223 ) ) ;
#19192 = CARTESIAN_POINT ( 'NONE',  ( 0.1058382717557499880, 0.3949938075777411073, -0.3083989501312336956 ) ) ;
#19193 = AXIS2_PLACEMENT_3D ( 'NONE', #76752, #17867, #49827 ) ;
#19194 = CARTESIAN_POINT ( 'NONE',  ( 0.2893091866268030499, 1.161375622156852083, -1.681321774322261042 ) ) ;
#19195 = CARTESIAN_POINT ( 'NONE',  ( 1.128608923884515169, -0.5023911411419708095, -0.1820866141732282451 ) ) ;
#19196 = CARTESIAN_POINT ( 'NONE',  ( 0.8398950131233602345, 0.1283753931104746893, -0.1820866141732285504 ) ) ;
#19197 = CARTESIAN_POINT ( 'NONE',  ( 0.2296587926509192634, -0.05778040916215560624, -0.4822834645669293319 ) ) ;
#19198 = CARTESIAN_POINT ( 'NONE',  ( -0.3458507752293906723, -0.3458507752293910609, -2.340551181102362488 ) ) ;
#19199 = CARTESIAN_POINT ( 'NONE',  ( 0.3949938075777409963, 2.418639510665530743E-17, -1.454724409448818756 ) ) ;
#19200 = CARTESIAN_POINT ( 'NONE',  ( 0.3477690288713918276, -0.5511811023622048555, -0.09757992244046775898 ) ) ;
#19201 = CARTESIAN_POINT ( 'NONE',  ( -0.8070866141732276899, 0.1660481256975883668, -0.3530559997133364547 ) ) ;
#19202 = CARTESIAN_POINT ( 'NONE',  ( -1.391076115485563314, -0.6046776061558809534, -0.2411417322834644161 ) ) ;
#19203 = CARTESIAN_POINT ( 'NONE',  ( 0.6955380577427828781, -0.4281496062992124485, 0.4176697321401328655 ) ) ;
#19204 = CARTESIAN_POINT ( 'NONE',  ( -1.157146581871515012E-16, 0.4724409448818898682, -1.574803149606299302 ) ) ;
#19205 = CARTESIAN_POINT ( 'NONE',  ( -0.7283464566929126471, 0.1660481256975883391, -0.3530559997133364547 ) ) ;
#19206 = EDGE_LOOP ( 'NONE', ( #5865, #55128, #68736, #16033, #35194, #80854, #13667, #68604, #32669, #66043, #82460, #39402, #10112, #73201 ) ) ;
#19207 = ORIENTED_EDGE ( 'NONE', *, *, #38580, .F. ) ;
#19208 = AXIS2_PLACEMENT_3D ( 'NONE', #53461, #80004, #52624 ) ;
#19209 = CARTESIAN_POINT ( 'NONE',  ( -1.450131233595799651, -0.6692913385826771977, 0.1292274648535927661 ) ) ;
#19210 = CARTESIAN_POINT ( 'NONE',  ( -0.6627296587926501115, 0.2952755905511810774, -0.1292274648535930714 ) ) ;
#19212 = CARTESIAN_POINT ( 'NONE',  ( -0.8530183727034112984, 0.05413385826771666132, 0.4176697321401328100 ) ) ;
#19211 = CARTESIAN_POINT ( 'NONE',  ( -0.9448818897637790704, -0.1870078740157480601, -0.3641732283464567677 ) ) ;
#19213 = CARTESIAN_POINT ( 'NONE',  ( -0.1958661417322836440, 0.3392501089628016664, -2.140400631724722835 ) ) ;
#19214 = CARTESIAN_POINT ( 'NONE',  ( 0.2032823926810630177, -0.2142011206082510000, 0.1316721176867485521 ) ) ;
#19215 = CARTESIAN_POINT ( 'NONE',  ( 1.443569553805774897, -0.6046776061558809534, -0.2411417322834644161 ) ) ;
#19216 = CARTESIAN_POINT ( 'NONE',  ( -0.7480314960629914633, 0.2952755905511811885, 0.000000000000000000 ) ) ;
#19217 = CARTESIAN_POINT ( 'NONE',  ( 0.4855643044619428750, 0.05413385826771666132, 0.4176697321401328100 ) ) ;
#19218 = CARTESIAN_POINT ( 'NONE',  ( -0.8595800524934373854, -0.05778040916215522460, 0.4822834645669289988 ) ) ;
#19219 = CARTESIAN_POINT ( 'NONE',  ( -0.2867679344610365999, 0.2867679344610364889, -1.429133858267716661 ) ) ;
#19220 = CARTESIAN_POINT ( 'NONE',  ( -0.7152230971128602510, -0.2845877964562159024, 0.3641732283464567677 ) ) ;
#19221 = ORIENTED_EDGE ( 'NONE', *, *, #79585, .F. ) ;
#19222 = CARTESIAN_POINT ( 'NONE',  ( -0.1974969037888706647, 0.3420746716998658843, -1.745406824146981339 ) ) ;
#19223 = ORIENTED_EDGE ( 'NONE', *, *, #54463, .F. ) ;
#19224 = CARTESIAN_POINT ( 'NONE',  ( -1.561679790026246017, -0.004921259842519576551, 0.3153832671262227771 ) ) ;
#19225 = CARTESIAN_POINT ( 'NONE',  ( -0.9055118110236215490, -0.6692913385826771977, 8.415575281601705876E-17 ) ) ;
#19226 = CARTESIAN_POINT ( 'NONE',  ( -0.9711286089238838626, 0.2306618581243847221, -0.2411417322834647770 ) ) ;
#19227 = CARTESIAN_POINT ( 'NONE',  ( 0.3996062992125986035, 2.446882876249141962E-17, -0.2755905511811023723 ) ) ;
#19228 = CARTESIAN_POINT ( 'NONE',  ( -1.108923884514435132, -0.3162353388693405765, 0.4822834645669290543 ) ) ;
#19229 = CARTESIAN_POINT ( 'NONE',  ( -1.299212598425196097, -0.6692913385826771977, 8.415575281601705876E-17 ) ) ;
#19230 = CARTESIAN_POINT ( 'NONE',  ( 0.000000000000000000, 0.03937007874015747977, 0.000000000000000000 ) ) ;
#19231 = LINE ( 'NONE', #38593, #2614 ) ;
#19232 = CARTESIAN_POINT ( 'NONE',  ( 0.6561679790026253567, -0.5023911411419708095, -0.1820866141732282451 ) ) ;
#19233 = CARTESIAN_POINT ( 'NONE',  ( 1.604771003085129433, 1.002618919725272617, -0.1466069496707750053 ) ) ;
#19234 = CARTESIAN_POINT ( 'NONE',  ( -0.3392501089628017219, -0.1958661417322836718, -0.4520997375328084655 ) ) ;
#19235 = CARTESIAN_POINT ( 'NONE',  ( -0.3280839895013117347, -0.3690944881889763329, 0.3153832671262228327 ) ) ;
#19236 = CARTESIAN_POINT ( 'NONE',  ( -0.8333333333333323711, 0.2952755905511811885, 0.1292274648535926551 ) ) ;
#19237 = CARTESIAN_POINT ( 'NONE',  ( 1.364829396325459854, -0.6046776061558809534, -0.2411417322834644161 ) ) ;
#19238 = CARTESIAN_POINT ( 'NONE',  ( -0.5511811023622038563, -0.1870078740157479769, 0.4822834645669291653 ) ) ;
#19239 = ORIENTED_EDGE ( 'NONE', *, *, #50213, .F. ) ;
#19240 = ORIENTED_EDGE ( 'NONE', *, *, #69643, .F. ) ;
#19241 = CARTESIAN_POINT ( 'NONE',  ( -0.3996062992125986590, 0.1070741851644051723, -1.841863517060367439 ) ) ;
#19242 = CARTESIAN_POINT ( 'NONE',  ( -1.056430446194224881, -0.6692913385826771977, 0.1292274648535927661 ) ) ;
#19243 = CARTESIAN_POINT ( 'NONE',  ( 1.187664041994751285, -0.3162353388693409650, -0.4822834645669289433 ) ) ;
#19244 = CARTESIAN_POINT ( 'NONE',  ( -1.345144356955379816, -0.08942795157528024563, -0.3641732283464568787 ) ) ;
#19245 = CARTESIAN_POINT ( 'NONE',  ( -1.391076115485563758, 0.2306618581243848609, 0.2411417322834645549 ) ) ;
#19246 = CARTESIAN_POINT ( 'NONE',  ( 0.4724409448818896462, 0.1265901696524990294, -0.9120734908136483021 ) ) ;
#19247 = CARTESIAN_POINT ( 'NONE',  ( 2.167269426034547308, 1.502969453419623846, 0.4732359647714768358 ) ) ;
#19248 = CARTESIAN_POINT ( 'NONE',  ( -0.1049643490035307020, 0.3917322834645669549, 0.001312335958005295946 ) ) ;
#19249 = CARTESIAN_POINT ( 'NONE',  ( -0.3917322834645671215, 0.1049643490035301469, -2.164698162729658648 ) ) ;
#19250 = CARTESIAN_POINT ( 'NONE',  ( -0.01312335958005186876, 0.05413385826771626580, -0.4176697321401330321 ) ) ;
#19251 = CARTESIAN_POINT ( 'NONE',  ( -0.8858267716535425107, -0.4536011799217367080, 0.2665933059059888421 ) ) ;
#19252 = CARTESIAN_POINT ( 'NONE',  ( -0.6561679790026240244, -0.6046776061558807314, 0.2411417322834647770 ) ) ;
#19253 = CARTESIAN_POINT ( 'NONE',  ( -0.1265901696524993347, 0.4724409448818895907, -2.760498687664041384 ) ) ;
#19254 = CARTESIAN_POINT ( 'NONE',  ( -1.253280839895012377, -0.05778040916215522460, 0.4822834645669289988 ) ) ;
#19255 = CARTESIAN_POINT ( 'NONE',  ( -1.069553805774277722, 0.2952755905511811885, 0.1292274648535926551 ) ) ;
#19256 = CARTESIAN_POINT ( 'NONE',  ( -0.08530183727034056085, -0.05778040916215560624, -0.4822834645669293319 ) ) ;
#19257 = CARTESIAN_POINT ( 'NONE',  ( 0.3949938075777409408, -0.1058382717557499186, -2.708005249343832244 ) ) ;
#19258 = CARTESIAN_POINT ( 'NONE',  ( 0.9251968503937015864, -0.4536011799217367080, 0.2665933059059888421 ) ) ;
#19259 = CARTESIAN_POINT ( 'NONE',  ( -0.6889763779527552368, -0.4536011799217368745, -0.2665933059059886201 ) ) ;
#19260 = AXIS2_PLACEMENT_3D ( 'NONE', #45359, #32746, #58413 ) ;
#19261 = CARTESIAN_POINT ( 'NONE',  ( 0.7874015748031503170, -0.1870078740157480601, -0.3641732283464567677 ) ) ;
#19262 = CARTESIAN_POINT ( 'NONE',  ( 1.220472440944882386, -0.5511811023622047445, 6.969142054262312111E-17 ) ) ;
#19263 = CARTESIAN_POINT ( 'NONE',  ( 1.568241469816273437, -0.3162353388693405765, 0.4822834645669290543 ) ) ;
#19264 = CARTESIAN_POINT ( 'NONE',  ( 0.6167979002624679463, -0.004921259842519870586, -0.3153832671262229437 ) ) ;
#19265 = CARTESIAN_POINT ( 'NONE',  ( -0.3392501089628017219, -0.1958661417322836718, -1.304461942257217899 ) ) ;
#19266 = CARTESIAN_POINT ( 'NONE',  ( -0.9317585301837263412, -0.4281496062992127816, -0.4176697321401328100 ) ) ;
#19267 = CARTESIAN_POINT ( 'NONE',  ( 1.240157480314961314, -0.5400638737290844871, 0.3530559997133364547 ) ) ;
#19268 = CARTESIAN_POINT ( 'NONE',  ( -0.3458507752293906723, -0.3458507752293910609, -0.1358267716535432879 ) ) ;
#19269 = CARTESIAN_POINT ( 'NONE',  ( -0.6692913385826764205, 0.1771653543307087630, 0.000000000000000000 ) ) ;
#19270 = FACE_OUTER_BOUND ( 'NONE', #14110, .T. ) ;
#19271 = CARTESIAN_POINT ( 'NONE',  ( 0.1312335958005257930, 0.2306618581243847221, -0.2411417322834647770 ) ) ;
#19272 = CARTESIAN_POINT ( 'NONE',  ( 0.2647380121165202049, 0.1323808228461571257, 0.1574803149606299746 ) ) ;
#19273 = AXIS2_PLACEMENT_3D ( 'NONE', #16976, #81360, #35486 ) ;
#19274 = CARTESIAN_POINT ( 'NONE',  ( 1.069553805774278610, -0.5511811023622046335, 0.09757992244046803654 ) ) ;
#19275 = CARTESIAN_POINT ( 'NONE',  ( 0.1246719160104994284, -0.5511811023622046335, 0.09757992244046803654 ) ) ;
#19276 = CARTESIAN_POINT ( 'NONE',  ( 0.2362204724409456558, -0.1870078740157479769, 0.4822834645669291653 ) ) ;
#19278 = EDGE_CURVE ( 'NONE', #65199, #70928, #4282, .T. ) ;
#19277 = CARTESIAN_POINT ( 'NONE',  ( -1.397637795275589623, 0.1660481256975885056, 0.3530559997133364547 ) ) ;
#19279 = CARTESIAN_POINT ( 'NONE',  ( -0.7152230971128602510, -0.2845877964562159024, 0.3641732283464567677 ) ) ;
#19280 = CARTESIAN_POINT ( 'NONE',  ( 0.1938976377952755792, -0.1938976377952756069, 0.1574803149606299191 ) ) ;
#19281 = CARTESIAN_POINT ( 'NONE',  ( -0.3608923884514428360, 0.2952755905511811885, 0.1292274648535926551 ) ) ;
#19282 = CARTESIAN_POINT ( 'NONE',  ( -0.3460692066303960313, 0.1998031496062989965, -1.047900262467191590 ) ) ;
#19283 = CARTESIAN_POINT ( 'NONE',  ( 0.1049643490035304938, -0.3917322834645669549, -2.532152230971127960 ) ) ;
#19284 = CARTESIAN_POINT ( 'NONE',  ( 0.1574803149606306130, -0.1870078740157479769, 0.3641732283464567677 ) ) ;
#19285 = CARTESIAN_POINT ( 'NONE',  ( -0.5643044619422565855, -0.4281496062992124485, 0.4176697321401328655 ) ) ;
#19286 = CARTESIAN_POINT ( 'NONE',  ( -0.9776902887139098386, 0.2952755905511810774, -0.1292274648535930714 ) ) ;
#19287 = CARTESIAN_POINT ( 'NONE',  ( -1.299212598425196097, 0.1771653543307087630, 0.000000000000000000 ) ) ;
#19288 = CARTESIAN_POINT ( 'NONE',  ( -3.931479177127797264, 1.111134681805650004, -0.2105673636452098652 ) ) ;
#19289 = CARTESIAN_POINT ( 'NONE',  ( -0.3674540682414689785, 0.2306618581243848609, 0.2411417322834645549 ) ) ;
#19290 = ADVANCED_FACE ( 'NONE', ( #60700 ), #15274, .F. ) ;
#19291 = CARTESIAN_POINT ( 'NONE',  ( -0.8070866141732276899, 0.07958543189024071263, -0.2665933059059888421 ) ) ;
#19292 = CARTESIAN_POINT ( 'NONE',  ( -1.476377952755905110, -0.4536011799217368745, -0.2665933059059886201 ) ) ;
#19293 = CARTESIAN_POINT ( 'NONE',  ( 1.135170603674541256, 0.2952755905511811885, 0.1292274648535926551 ) ) ;
#19294 = CARTESIAN_POINT ( 'NONE',  ( -0.1938976377952756625, -0.1938976377952756625, 0.07874015748031495954 ) ) ;
#19295 = CARTESIAN_POINT ( 'NONE',  ( -0.1049643490035307158, 0.3917322834645670104, -2.050544250165041493 ) ) ;
#19296 = EDGE_LOOP ( 'NONE', ( #33020, #19179, #73610, #63352 ) ) ;
#19297 = EDGE_CURVE ( 'NONE', #4124, #34136, #61076, .T. ) ;
#19298 = CARTESIAN_POINT ( 'NONE',  ( -0.7478466213799878082, 1.968503937007873850, 0.5309055118110236338 ) ) ;
#19299 = CARTESIAN_POINT ( 'NONE',  ( -1.548556430446193399, 0.2306618581243848609, 0.2411417322834645549 ) ) ;
#19300 = CARTESIAN_POINT ( 'NONE',  ( -0.7677165354330699465, 0.1660481256975885056, 0.3530559997133364547 ) ) ;
#19301 = CARTESIAN_POINT ( 'NONE',  ( -1.430446194225720724, 0.05413385826771626580, -0.4176697321401330321 ) ) ;
#19302 = CARTESIAN_POINT ( 'NONE',  ( -0.3392501089628019995, 0.1958661417322832277, -2.158136482939632561 ) ) ;
#19303 = CARTESIAN_POINT ( 'NONE',  ( 1.450131233595801428, -0.5511811023622048555, -0.09757992244046775898 ) ) ;
#19304 = CARTESIAN_POINT ( 'NONE',  ( 0.5446194225721792126, -0.3162353388693405765, 0.4822834645669290543 ) ) ;
#19305 = CARTESIAN_POINT ( 'NONE',  ( 0.1443569553805781891, 0.05413385826771626580, -0.4176697321401330321 ) ) ;
#19306 = CARTESIAN_POINT ( 'NONE',  ( -0.3264567959345324177, -3.773335473449285555E-15, -0.3791475997938234532 ) ) ;
#19307 = CARTESIAN_POINT ( 'NONE',  ( -0.1998031496062994405, 0.3460692066303957537, -2.609580052493438274 ) ) ;
#19308 = CARTESIAN_POINT ( 'NONE',  ( 1.154855643044620184, 0.1283753931104746893, -0.1820866141732285504 ) ) ;
#19309 = CARTESIAN_POINT ( 'NONE',  ( -0.3996062992125986035, -0.1070741851644056997, -1.305774278215223072 ) ) ;
#19310 = ORIENTED_EDGE ( 'NONE', *, *, #25809, .F. ) ;
#19311 = CARTESIAN_POINT ( 'NONE',  ( -9.594673741351313045E-17, 0.3917322834645670659, 0.003261524113173961108 ) ) ;
#19312 = ORIENTED_EDGE ( 'NONE', *, *, #2159, .F. ) ;
#19313 = CARTESIAN_POINT ( 'NONE',  ( -0.06561679790026180015, -0.4281496062992127816, -0.4176697321401328100 ) ) ;
#19314 = CARTESIAN_POINT ( 'NONE',  ( -0.9448818897637790704, -0.1870078740157479769, 0.4822834645669291653 ) ) ;
#19315 = CARTESIAN_POINT ( 'NONE',  ( -1.443569553805773564, 0.2306618581243847221, -0.2411417322834647770 ) ) ;
#19316 = CARTESIAN_POINT ( 'NONE',  ( 0.7020997375328090762, -0.3162353388693405765, 0.4822834645669290543 ) ) ;
#19317 = CONICAL_SURFACE ( 'NONE', #71786, 65.61679790026244063, 1.030376826524312284 ) ;
#19318 = CARTESIAN_POINT ( 'NONE',  ( 1.686351706036745890, 0.2952755905511811885, 0.1292274648535926551 ) ) ;
#19319 = CARTESIAN_POINT ( 'NONE',  ( 1.279527559055118724, 0.1660481256975885056, 0.3530559997133364547 ) ) ;
#19320 = CARTESIAN_POINT ( 'NONE',  ( -0.3477690288713902178, 0.2952755905511810774, -0.1292274648535930714 ) ) ;
#19321 = CARTESIAN_POINT ( 'NONE',  ( 0.6233595800524939223, -0.3162353388693405765, 0.4822834645669290543 ) ) ;
#19322 = CARTESIAN_POINT ( 'NONE',  ( -1.555118110236219930, -0.5400638737290845981, -0.3530559997133363437 ) ) ;
#19323 = CARTESIAN_POINT ( 'NONE',  ( 1.259842519685040019, -0.1870078740157479769, 0.4822834645669291653 ) ) ;
#19324 = ADVANCED_FACE ( 'NONE', ( #73768, #9364 ), #67442, .F. ) ;
#19325 = CARTESIAN_POINT ( 'NONE',  ( 1.463254593175853824, -0.6692913385826771977, 0.1292274648535927661 ) ) ;
#19326 = CARTESIAN_POINT ( 'NONE',  ( -0.2362204724409442680, -0.1870078740157480879, -0.4822834645669291653 ) ) ;
#19327 = CARTESIAN_POINT ( 'NONE',  ( -0.1958661417322836718, 0.3392501089628017219, -0.3202099737532808077 ) ) ;
#19328 = CARTESIAN_POINT ( 'NONE',  ( 0.6233595800524942554, -0.08942795157528024563, -0.3641732283464568787 ) ) ;
#19329 = ORIENTED_EDGE ( 'NONE', *, *, #41924, .T. ) ;
#19330 = CARTESIAN_POINT ( 'NONE',  ( -0.1974969037888706647, 0.3420746716998658843, -0.6430446194225721834 ) ) ;
#19331 = ORIENTED_EDGE ( 'NONE', *, *, #69939, .T. ) ;
#19332 = CARTESIAN_POINT ( 'NONE',  ( -0.4724409448818890911, -0.1870078740157479769, 0.3641732283464567677 ) ) ;
#19333 = CARTESIAN_POINT ( 'NONE',  ( -0.4091458600556405756, 0.2362204724409446288, -0.1837270341207349056 ) ) ;
#19334 = CARTESIAN_POINT ( 'NONE',  ( 0.3083989501312343062, -0.3162353388693405765, 0.4822834645669290543 ) ) ;
#19335 = CARTESIAN_POINT ( 'NONE',  ( 0.02624671916010564918, 0.2306618581243848609, 0.2411417322834645549 ) ) ;
#19336 = CARTESIAN_POINT ( 'NONE',  ( -1.161417322834644716, -0.5400638737290845981, -0.3530559997133363437 ) ) ;
#19337 = EDGE_CURVE ( 'NONE', #40450, #39419, #80908, .T. ) ;
#19338 = VECTOR ( 'NONE', #4301, 39.37007874015748143 ) ;
#19339 = CARTESIAN_POINT ( 'NONE',  ( -0.2867679344610365444, -0.2867679344610367664, -1.788077058563991795 ) ) ;
#19340 = CARTESIAN_POINT ( 'NONE',  ( -1.187664041994749731, -0.3162353388693405765, 0.4822834645669290543 ) ) ;
#19341 = CARTESIAN_POINT ( 'NONE',  ( -0.1474713956048439301, -2.191421614605370878E-15, 0.4445507791589071167 ) ) ;
#19342 = CARTESIAN_POINT ( 'NONE',  ( 0.9776902887139113929, 0.1771653543307087630, 0.09757992244046791164 ) ) ;
#19343 = CARTESIAN_POINT ( 'NONE',  ( 0.5380577427821529035, -0.4281496062992124485, 0.4176697321401328655 ) ) ;
#19344 = CARTESIAN_POINT ( 'NONE',  ( 0.8989501312335964611, 0.2952755905511811885, 0.1292274648535926551 ) ) ;
#19345 = CARTESIAN_POINT ( 'NONE',  ( -0.3460692066303958092, -0.1998031496062994683, -1.154855643044619518 ) ) ;
#19346 = CARTESIAN_POINT ( 'NONE',  ( -1.404199475065615932, 0.05413385826771666132, 0.4176697321401328100 ) ) ;
#19347 = CARTESIAN_POINT ( 'NONE',  ( 4.893765752498283308E-17, -0.3996062992125985480, -0.7854330708661416693 ) ) ;
#19348 = CARTESIAN_POINT ( 'NONE',  ( -0.1998031496062994405, 0.3460692066303957537, -0.2473753280839895152 ) ) ;
#19349 = CARTESIAN_POINT ( 'NONE',  ( -0.1443569553805768291, 0.05413385826771666132, 0.4176697321401328100 ) ) ;
#19350 = CARTESIAN_POINT ( 'NONE',  ( -9.787531504996567848E-17, 0.3996062992125986035, -2.519685039370078705 ) ) ;
#19351 = EDGE_CURVE ( 'NONE', #16864, #62412, #54118, .T. ) ;
#19352 = CARTESIAN_POINT ( 'NONE',  ( -0.3392501089628019995, 0.1958661417322832277, -1.685695538057742970 ) ) ;
#19353 = CARTESIAN_POINT ( 'NONE',  ( -1.161417322834644716, 0.07958543189024085140, 0.2665933059059887866 ) ) ;
#19354 = CARTESIAN_POINT ( 'NONE',  ( 1.391076115485564868, -0.6046776061558807314, 0.2411417322834647770 ) ) ;
#19355 = CARTESIAN_POINT ( 'NONE',  ( 1.528871391076116026, 0.2952755905511811885, 0.1292274648535926551 ) ) ;
#19356 = CARTESIAN_POINT ( 'NONE',  ( 0.01312335958005323398, -0.3690944881889765550, -0.3153832671262227771 ) ) ;
#19357 = CARTESIAN_POINT ( 'NONE',  ( 0.3543307086614179147, 0.2952755905511811885, 0.000000000000000000 ) ) ;
#19358 = CARTESIAN_POINT ( 'NONE',  ( 0.3458507752293908943, 0.3458507752293908943, -1.631889763779527325 ) ) ;
#19359 = CARTESIAN_POINT ( 'NONE',  ( 0.3740157480314966754, -0.4536011799217367080, 0.2665933059059888421 ) ) ;
#19360 = CARTESIAN_POINT ( 'NONE',  ( 0.4790026246719167324, -0.05778040916215522460, 0.4822834645669289988 ) ) ;
#19361 = CARTESIAN_POINT ( 'NONE',  ( 0.3949938075777409408, -0.1058382717557499186, -0.8182414698162731037 ) ) ;
#19362 = CARTESIAN_POINT ( 'NONE',  ( -1.141732283464566011, -0.6692913385826771977, 8.415575281601705876E-17 ) ) ;
#19363 = CARTESIAN_POINT ( 'NONE',  ( 0.3083989501312343062, -0.2845877964562159024, 0.3641732283464567677 ) ) ;
#19364 = CARTESIAN_POINT ( 'NONE',  ( 0.3273801728231982566, 0.000000000000000000, 0.3464511005275205946 ) ) ;
#19365 = CARTESIAN_POINT ( 'NONE',  ( -0.4790026246719154557, -0.3162353388693405765, 0.4822834645669290543 ) ) ;
#19366 = CARTESIAN_POINT ( 'NONE',  ( -0.1968503937007867743, 0.1771653543307087630, 0.000000000000000000 ) ) ;
#19367 = LINE ( 'NONE', #76620, #60112 ) ;
#19368 = CARTESIAN_POINT ( 'NONE',  ( -0.2230971128608915943, -0.4281496062992127816, -0.4176697321401328100 ) ) ;
#19369 = CARTESIAN_POINT ( 'NONE',  ( 0.1902887139107617975, 0.1771653543307087630, 0.09757992244046791164 ) ) ;
#19370 = CARTESIAN_POINT ( 'NONE',  ( 0.3460692066303958092, 0.1998031496062993018, -2.097769028871391050 ) ) ;
#19371 = CARTESIAN_POINT ( 'NONE',  ( -0.03937007874015669567, 0.2952755905511811885, 0.000000000000000000 ) ) ;
#19372 = CARTESIAN_POINT ( 'NONE',  ( 0.1049643490035304522, -0.3917322834645668994, -1.740138164533121756 ) ) ;
#19373 = CARTESIAN_POINT ( 'NONE',  ( 1.332020997375329197, -0.2845877964562159024, 0.3641732283464567677 ) ) ;
#19374 = CARTESIAN_POINT ( 'NONE',  ( 0.4848604877838280647, 0.000000000000000000, 0.3464511005275205946 ) ) ;
#19375 = CARTESIAN_POINT ( 'NONE',  ( -0.9120734908136475250, 0.1771653543307087630, 0.09757992244046791164 ) ) ;
#19376 = CARTESIAN_POINT ( 'NONE',  ( -0.8989501312335946848, 0.1771653543307087075, -0.09757992244046823083 ) ) ;
#19377 = CARTESIAN_POINT ( 'NONE',  ( -0.8267716535433065062, 0.2952755905511811885, 0.000000000000000000 ) ) ;
#19378 = CARTESIAN_POINT ( 'NONE',  ( -0.1115485564304456306, 0.2952755905511810774, -0.1292274648535930714 ) ) ;
#19379 = CARTESIAN_POINT ( 'NONE',  ( 0.7611548556430454138, 0.1283753931104746893, -0.1820866141732285504 ) ) ;
#19380 = CARTESIAN_POINT ( 'NONE',  ( -0.2596916824146293656, 0.1407161764240515978, 5.810203857714900444 ) ) ;
#19381 = CARTESIAN_POINT ( 'NONE',  ( 1.049868766404200127, -0.5023911411419708095, -0.1820866141732282451 ) ) ;
#19382 = AXIS2_PLACEMENT_3D ( 'NONE', #10391, #73948, #67633 ) ;
#19383 = CARTESIAN_POINT ( 'NONE',  ( 0.8792650918635177559, 0.05413385826771666132, 0.4176697321401328100 ) ) ;
#19384 = CARTESIAN_POINT ( 'NONE',  ( -0.1070741851644051862, -0.3996062992125986590, 0.008530183727034111943 ) ) ;
#19385 = CARTESIAN_POINT ( 'NONE',  ( -0.3018372703412066094, 0.05413385826771666132, 0.4176697321401328100 ) ) ;
#19386 = CARTESIAN_POINT ( 'NONE',  ( -0.1049643490035302024, -0.3917322834645671215, -0.9442257217847768169 ) ) ;
#19387 = CARTESIAN_POINT ( 'NONE',  ( -1.732283464566928277, -0.1870078740157479769, 0.4822834645669291653 ) ) ;
#19388 = CARTESIAN_POINT ( 'NONE',  ( 0.7742782152230979209, 0.05413385826771626580, -0.4176697321401330321 ) ) ;
#19389 = CARTESIAN_POINT ( 'NONE',  ( -0.05249343832020911260, 0.2306618581243848609, 0.2411417322834645549 ) ) ;
#19390 = PLANE ( 'NONE',  #73652 ) ;
#19391 = CARTESIAN_POINT ( 'NONE',  ( 0.3871391076115493490, -0.2845877964562159024, 0.3641732283464567677 ) ) ;
#19392 = CARTESIAN_POINT ( 'NONE',  ( 0.7677165354330716118, 0.1660481256975883668, -0.3530559997133364547 ) ) ;
#19393 = EDGE_CURVE ( 'NONE', #9282, #36478, #36270, .T. ) ;
#19394 = CARTESIAN_POINT ( 'NONE',  ( -0.3018372703412066094, -0.004921259842519576551, 0.3153832671262227771 ) ) ;
#19395 = CARTESIAN_POINT ( 'NONE',  ( -0.7742782152230962556, -0.4281496062992127816, -0.4176697321401328100 ) ) ;
#19396 = DIRECTION ( 'NONE',  ( -0.8660254037844433705, 0.000000000000000000, 0.4999999999999920064 ) ) ;
#19397 = CARTESIAN_POINT ( 'NONE',  ( 0.1837270341207354329, 0.2306618581243848609, 0.2411417322834645549 ) ) ;
#19398 = CARTESIAN_POINT ( 'NONE',  ( -1.377952755905511140, -0.6692913385826771977, 8.415575281601705876E-17 ) ) ;
#19399 = CARTESIAN_POINT ( 'NONE',  ( -0.8464566929133852113, -0.4536011799217368745, -0.2665933059059886201 ) ) ;
#19400 = CARTESIAN_POINT ( 'NONE',  ( 0.3805774278215230400, 0.05413385826771626580, -0.4176697321401330321 ) ) ;
#19401 = CARTESIAN_POINT ( 'NONE',  ( -1.082677165354329896, 0.1660481256975885056, 0.3530559997133364547 ) ) ;
#19402 = CARTESIAN_POINT ( 'NONE',  ( -0.4396325459317577122, -0.6692913385826773087, -0.1292274648535924053 ) ) ;
#19403 =( BOUNDED_SURFACE ( )  B_SPLINE_SURFACE ( 1, 2, ( 
 ( #13675, #19138, #38913, #64593, #71327, #65013, #7348, #20398, #1051, #14097, #26705, #46050, #71744, #53192, #10169, #49272, #14517, #1875, #59518, #74144, #72575, #40582, #36239, #7777, #67830, #27535, #27117, #78905, #16489, #3434, #14922, #78490, #40170, #29508, #35418, #39749, #22784, #33854, #1461, #52781, #29913, #68248, #48861, #65854, #23190, #42135, #80472, #48444, #8187, #80878, #10582, #35834, #20813, #74975, #74561, #54768, #46881, #21226, #61501, #66263, #16907, #29096, #8603, #61083, #42545, #59105, #4251, #81287, #61909, #46468, #3848, #55577, #23603, #55169, #72162, #65445, #33445, #12635, #49683, #68642, #37058, #82109, #18539, #11401, #57644, #76610, #70282, #10981, #5487, #36641, #31148, #69052, #25245, #7, #24015, #24422, #25659, #38294, #81705, #51321, #43350, #37473, #75375, #50909, #6307, #37884, #42948, #5893, #63971, #50092, #18940, #56814, #18130, #17724, #30327, #44588, #62742, #82513, #4654, #75788, #17320, #43763, #69468, #11821, #57223, #24829, #62317, #55993, #5078, #30747, #63146, #56410, #50498, #76201, #31984, #44182, #69874, #63559, #82924, #12227, #31565, #26919, #14321, #52995, #58059, #13892, #40387, #77444, #26508, #52579, #52162, #58486, #78288, #77866, #51741, #77024, #851, #59322, #13469, #425, #71966, #72385, #33659, #20619, #58912, #66070, #65669, #39551, #46692, #64390, #59737, #45006, #14735, #26081, #70706, #39126, #20195, #46271, #71126, #34073, #78708, #8406, #13058, #65240, #38712, #7578, #45431, #1678, #2091, #19777, #45846, #27756, #19357, #64807, #6726, #7146, #33250, #32819, #27335, #32396, #39979, #71545, #7995, #1271, #21032, #3748, #9651, #54245, #53828, #66483, #55071, #73211, #67316, #40798, #2925, #53420, #79962, #22275, #28589, #10066, #41627, #36143, #21446, #47103, #4155, #47935, #72792, #35320, #79542, #48762, #34495, #60983, #74043, #35729, #3333, #60574, #28997, #16390, #29412, #60160, #73638, #16808, #21855, #15980, #54663, #80374, #34911, #22687, #48346, #28171, #79129, #42037, #61399, #15561, #2512, #67731, #74461, #80779, #23095, #42445, #68144, #10489, #61815, #15142, #8818, #47519, #41221, #66908, #9239, #69376, #11729, #4564, #69786, #57131, #31056, #68549, #63872, #63465, #43673, #36967, #75286, #37385, #17629, #5799, #18039, #43261, #55899, #31469, #49176, #76519, #70185, #25150, #36550, #68958, #12131, #37788, #81610, #18450, #50001, #10890, #24741, #50818, #44092, #18848, #44494, #12538, #11308, #82828, #62646, #38197, #5394, #63056, #29820, #62226, #17224, #55482, #81191, #30235, #56725, #4988, #30655, #82422, #23508, #74880, #42856, #23925, #49591, #50409, #56319, #76109, #82017, #24331, #75698, #32298, #52061, #19674, #71028, #46171, #31887, #20099, #57958, #51226, #326, #77767, #7049, #45333, #19252, #12957, #65138, #39025, #6211, #45750, #25980, #76924, #44904, #65564, #58814, #7474, #13372, #70602, #71867, #57547, #38614, #746, #64292, #33145, #6626, #71445, #51638, #33559, #1171, #20519, #26822, #13793, #39877, #77343, #64709, #7898, #32718, #58385, #52480, #78188, #39450, #26407, #14217, #83238, #25559, #59611, #13344, #45722, #65945, #20070, #7020, #78582, #79003, #40262, #33533, #65538, #72669, #72260, #46145, #53291, #27629, #8281, #717, #33947, #59196, #39847, #7869, #58355, #1966, #21322, #1555, #38998, #34368, #46975, #14190, #7445, #71419, #27209, #13766, #15018, #71840, #39423, #33115, #65107, #52872, #58785, #40674, #20908, #1143, #26375, #66359, #19645, #8697, #296, #25952, #32688, #26793, #51610, #77315, #52035, #71001, #45306, #64681, #77739, #52450, #78160, #20491, #46561, #14608, #54121, #17101, #36025, #29702, #53703, #48230, #79412, #73926, #28460, #68022, #42736, #66784, #67195, #68432, #55365, #41096, #10772, #2801, #80253, #9119, #10365, #49054, #80663, #2389, #48642, #81070, #9526, #61697, #16268, #60859, #60449, #73085, #4037, #79835, #41913, #47394, #35198, #60033, #3213, #28875, #54538, #16683, #67607, #28045, #21731, #15435, #34790, #22570, #22152, #9938, #47811, #23386, #73513, #35610, #22975, #42322, #61273, #3626, #29294, #74336 ),
 ( #74753, #54956, #15862, #41510, #43142, #62518, #81896, #82704, #75985, #82301, #4857, #12415, #17918, #5270, #37261, #63339, #43554, #31342, #75165, #30531, #50287, #11185, #24620, #18327, #69255, #11602, #38073, #63749, #44369, #36846, #18727, #12007, #43967, #69664, #56195, #76395, #6088, #37661, #17510, #70476, #70061, #5674, #62937, #24207, #57008, #49878, #31763, #25024, #75578, #30934, #57424, #55775, #83118, #76799, #25436, #68839, #56601, #51102, #19130, #50697, #23799, #44779, #4448, #36432, #62105, #30113, #81483, #49472, #14092, #6922, #53185, #72157, #65849, #6508, #1045, #32178, #26699, #64585, #20807, #78900, #19546, #19975, #21221, #8182, #77217, #46876, #38905, #33010, #45205, #46463, #1868, #33440, #38491, #1455, #33848, #45626, #14512, #52354, #13669, #13256, #25853, #40165, #32593, #78061, #201, #71320, #12833, #39321, #65006, #7342, #52775, #20391, #64174, #57833, #51513, #70905, #58680, #58256, #46043, #621, #59514, #26277, #71737, #59100, #78483, #39744, #65440, #7773, #27112, #27530, #51939, #77643, #35929, #72982, #22049, #48129, #47709, #54021, #73826, #21633, #48537, #2285, #34689, #54859, #9016, #79314, #67502, #67921, #29192, #22469, #54438, #61596, #61172, #35093, #42226, #41409, #73405, #16164, #79732, #9837, #27947, #15334, #3111, #47293, #60760, #28776, #15756, #67093, #74237, #10259, #53606, #28359, #80149, #34269, #9424, #60352, #3524, #41810, #40999, #35508, #3942, #80564, #29601, #55262, #80972, #2699, #22875, #16581, #23285, #72570, #14917, #40577, #66679, #59929, #66258, #8597, #4343, #50188, #24109, #4752, #5173, #37977, #82608, #83017, #10676, #68337, #37155, #62414, #18226, #57321, #23696, #11081, #68739, #82204, #81798, #49778, #44275, #16998, #75885, #36738, #36332, #30426, #24522, #11501, #75478, #30010, #49369, #37566, #43452, #48955, #30837, #43043, #62007, #55673, #63652, #63240, #11912, #17819, #81382, #18631, #74656, #42640, #62839, #75065, #43863, #17413, #56502, #56093, #5991, #5580, #24926, #31246, #69564, #69965, #69150, #56912, #31662, #50593, #76302, #12319, #7677, #52260, #71227, #19452, #51002, #8092, #26608, #13994, #32078, #25755, #33348, #13571, #71643, #77966, #57739, #51417, #70807, #39651, #64910, #39225, #77119, #1365, #6825, #13159, #65342, #45529, #6408, #20296, #20717, #59010, #72062, #14420, #65759, #38810, #27017, #32494, #78386, #952, #58585, #52678, #101, #12732, #46368, #25340, #64069, #45945, #526, #64487, #7247, #40072, #33756, #60566, #70377, #44681, #32919, #58158, #76701, #19034, #45103, #26179, #51841, #38391, #77546, #19880, #81599, #54237, #29811, #22679, #73630, #48338, #36133, #48753, #61391, #41619, #3325, #74871, #80771, #2917, #68135, #80366, #47925, #15972, #75277, #17214, #49165, #3740, #67308, #55888, #28580, #79954, #74452, #9643, #81182, #35312, #10480, #54655, #17620, #42847, #62217, #68540, #61806, #23916, #60974, #29404, #43252, #28989, #10058, #10880, #36541, #55472, #16798, #74035, #22267, #68949, #4146, #4555, #16382, #42028, #30225, #42435, #49581, #23499, #67722, #35721, #55063, #11299, #36958, #23086, #5385, #38606, #44083, #31460, #63455, #6201, #69777, #57539, #18030, #31046, #76510, #37376, #25140, #18839, #12121, #37779, #64284, #318, #43664, #18441, #44484, #24321, #5790, #12948, #70176, #57122, #24732, #12528, #50400, #6619, #50809, #76097, #56715, #32290, #82007, #25971, #19663, #57950, #69366, #82816, #44895, #70594, #82413, #49992, #45325, #30645, #51630, #11720, #56310, #38189, #63864, #31879, #83230, #71020, #77334, #13364, #75689, #25551, #63046, #51218, #76915, #62635, #4979, #19244, #46164, #21747, #8713, #20092, #79428, #65130, #59214, #71438, #46994, #28063, #59629, #64701, #27647, #34384, #71860, #72687, #78602, #39866, #39442, #52054, #40690, #58805, #52890, #26396, #14210, #39017, #65557, #7889, #33552, #79022, #27230, #47412, #7041, #32710, #73101, #1575, #58376, #20926, #7465, #60049, #45742, #46581, #1984, #21341, #72279, #14626, #40281, #53309, #15035, #13786, #65963, #2405, #33135, #8299, #33967, #66376, #20511, #53720, #1163 ) ),
 .UNSPECIFIED., .F., .F., .F. ) 
 B_SPLINE_SURFACE_WITH_KNOTS ( ( 2, 2 ),
 ( 3, 2, 2, 2, 2, 2, 2, 2, 2, 2, 2, 2, 2, 2, 2, 2, 2, 2, 2, 2, 2, 2, 2, 2, 2, 2, 2, 2, 2, 2, 2, 2, 2, 2, 2, 2, 2, 2, 2, 2, 2, 2, 2, 2, 2, 2, 2, 2, 2, 2, 2, 2, 2, 2, 2, 2, 2, 2, 2, 2, 2, 2, 2, 2, 2, 2, 2, 2, 2, 2, 2, 2, 2, 2, 2, 2, 2, 2, 2, 2, 2, 2, 2, 2, 2, 2, 2, 2, 2, 2, 2, 2, 2, 2, 2, 2, 2, 2, 2, 2, 2, 2, 2, 2, 2, 2, 2, 2, 2, 2, 2, 2, 2, 2, 2, 2, 2, 2, 2, 2, 2, 2, 2, 2, 2, 2, 2, 2, 2, 2, 2, 2, 2, 2, 2, 2, 2, 2, 2, 2, 2, 2, 2, 2, 2, 2, 2, 2, 2, 2, 2, 2, 2, 2, 2, 2, 2, 2, 2, 2, 2, 2, 2, 2, 2, 2, 2, 2, 2, 2, 2, 2, 2, 2, 2, 2, 2, 2, 2, 2, 2, 2, 2, 2, 2, 2, 2, 2, 2, 2, 2, 2, 2, 2, 2, 2, 2, 2, 2, 2, 2, 2, 2, 2, 2, 2, 2, 2, 2, 2, 2, 2, 2, 2, 2, 2, 2, 2, 2, 2, 2, 2, 2, 2, 2, 2, 2, 2, 2, 2, 2, 2, 2, 2, 2, 2, 2, 2, 2, 2, 2, 2, 2, 2, 2, 2, 2, 2, 2, 2, 2, 2, 2, 2, 2, 3 ),
 ( 0.000000000000000000, 1.000000000000000000 ),
 ( 0.000000000000000000, 0.003787878787878787984, 0.007575757575757575968, 0.01136363636363636395, 0.01515151515151515194, 0.01893939393939393992, 0.02272727272727272790, 0.02651515151515151589, 0.03030303030303030387, 0.03409090909090908839, 0.03787878787878787984, 0.04166666666666666435, 0.04545454545454545581, 0.04924242424242424032, 0.05303030303030303177, 0.05681818181818181629, 0.06060606060606060774, 0.06439393939393939226, 0.06818181818181817677, 0.07196969696969697516, 0.07575757575757575968, 0.07954545454545454419, 0.08333333333333332871, 0.08712121212121212710, 0.09090909090909091161, 0.09469696969696969613, 0.09848484848484848064, 0.1022727272727272790, 0.1060606060606060635, 0.1098484848484848481, 0.1136363636363636326, 0.1174242424242424310, 0.1212121212121212155, 0.1250000000000000000, 0.1287878787878787845, 0.1325757575757575690, 0.1363636363636363535, 0.1401515151515151381, 0.1439393939393939503, 0.1477272727272727348, 0.1515151515151515194, 0.1553030303030303039, 0.1590909090909090884, 0.1628787878787878729, 0.1666666666666666574, 0.1704545454545454419, 0.1742424242424242542, 0.1780303030303030387, 0.1818181818181818232, 0.1856060606060606077, 0.1893939393939393923, 0.1931818181818181768, 0.1969696969696969613, 0.2007575757575757458, 0.2045454545454545581, 0.2083333333333333426, 0.2121212121212121271, 0.2159090909090909116, 0.2196969696969696961, 0.2234848484848484806, 0.2272727272727272652, 0.2310606060606060497, 0.2348484848484848619, 0.2386363636363636465, 0.2424242424242424310, 0.2462121212121212155, 0.2500000000000000000, 0.2537878787878787845, 0.2575757575757575690, 0.2613636363636363535, 0.2651515151515151381, 0.2689393939393939226, 0.2727272727272727071, 0.2765151515151514916, 0.2803030303030302761, 0.2840909090909091161, 0.2878787878787879007, 0.2916666666666666852, 0.2954545454545454697, 0.2992424242424242542, 0.3030303030303030387, 0.3068181818181818232, 0.3106060606060606077, 0.3143939393939393923, 0.3181818181818181768, 0.3219696969696969613, 0.3257575757575757458, 0.3295454545454545303, 0.3333333333333333148, 0.3371212121212120993, 0.3409090909090908839, 0.3446969696969697239, 0.3484848484848485084, 0.3522727272727272929, 0.3560606060606060774, 0.3598484848484848619, 0.3636363636363636465, 0.3674242424242424310, 0.3712121212121212155, 0.3750000000000000000, 0.3787878787878787845, 0.3825757575757575690, 0.3863636363636363535, 0.3901515151515151381, 0.3939393939393939226, 0.3977272727272727071, 0.4015151515151514916, 0.4053030303030302761, 0.4090909090909091161, 0.4128787878787879007, 0.4166666666666666852, 0.4204545454545454697, 0.4242424242424242542, 0.4280303030303030387, 0.4318181818181818232, 0.4356060606060606077, 0.4393939393939393923, 0.4431818181818181768, 0.4469696969696969613, 0.4507575757575757458, 0.4545454545454545303, 0.4583333333333333148, 0.4621212121212120993, 0.4659090909090908839, 0.4696969696969697239, 0.4734848484848485084, 0.4772727272727272929, 0.4810606060606060774, 0.4848484848484848619, 0.4886363636363636465, 0.4924242424242424310, 0.4962121212121212155, 0.5000000000000000000, 0.5037878787878787845, 0.5075757575757575690, 0.5113636363636363535, 0.5151515151515151381, 0.5189393939393939226, 0.5227272727272727071, 0.5265151515151514916, 0.5303030303030302761, 0.5340909090909090606, 0.5378787878787878451, 0.5416666666666666297, 0.5454545454545454142, 0.5492424242424241987, 0.5530303030303029832, 0.5568181818181817677, 0.5606060606060605522, 0.5643939393939394478, 0.5681818181818182323, 0.5719696969696970168, 0.5757575757575758013, 0.5795454545454545858, 0.5833333333333333703, 0.5871212121212121549, 0.5909090909090909394, 0.5946969696969697239, 0.5984848484848485084, 0.6022727272727272929, 0.6060606060606060774, 0.6098484848484848619, 0.6136363636363636465, 0.6174242424242424310, 0.6212121212121212155, 0.6250000000000000000, 0.6287878787878787845, 0.6325757575757575690, 0.6363636363636363535, 0.6401515151515151381, 0.6439393939393939226, 0.6477272727272727071, 0.6515151515151514916, 0.6553030303030302761, 0.6590909090909090606, 0.6628787878787878451, 0.6666666666666666297, 0.6704545454545454142, 0.6742424242424241987, 0.6780303030303029832, 0.6818181818181817677, 0.6856060606060605522, 0.6893939393939394478, 0.6931818181818182323, 0.6969696969696970168, 0.7007575757575758013, 0.7045454545454545858, 0.7083333333333333703, 0.7121212121212121549, 0.7159090909090909394, 0.7196969696969697239, 0.7234848484848485084, 0.7272727272727272929, 0.7310606060606060774, 0.7348484848484848619, 0.7386363636363636465, 0.7424242424242424310, 0.7462121212121212155, 0.7500000000000000000, 0.7537878787878787845, 0.7575757575757575690, 0.7613636363636363535, 0.7651515151515151381, 0.7689393939393939226, 0.7727272727272727071, 0.7765151515151514916, 0.7803030303030302761, 0.7840909090909090606, 0.7878787878787878451, 0.7916666666666666297, 0.7954545454545454142, 0.7992424242424241987, 0.8030303030303029832, 0.8068181818181817677, 0.8106060606060605522, 0.8143939393939394478, 0.8181818181818182323, 0.8219696969696970168, 0.8257575757575758013, 0.8295454545454545858, 0.8333333333333333703, 0.8371212121212121549, 0.8409090909090909394, 0.8446969696969697239, 0.8484848484848485084, 0.8522727272727272929, 0.8560606060606060774, 0.8598484848484848619, 0.8636363636363636465, 0.8674242424242424310, 0.8712121212121212155, 0.8750000000000000000, 0.8787878787878787845, 0.8825757575757575690, 0.8863636363636363535, 0.8901515151515151381, 0.8939393939393939226, 0.8977272727272727071, 0.9015151515151514916, 0.9053030303030302761, 0.9090909090909090606, 0.9128787878787878451, 0.9166666666666666297, 0.9204545454545454142, 0.9242424242424241987, 0.9280303030303029832, 0.9318181818181817677, 0.9356060606060605522, 0.9393939393939394478, 0.9431818181818182323, 0.9469696969696970168, 0.9507575757575758013, 0.9545454545454545858, 0.9583333333333333703, 0.9621212121212121549, 0.9659090909090909394 ),
 .UNSPECIFIED. ) 
 GEOMETRIC_REPRESENTATION_ITEM ( )  RATIONAL_B_SPLINE_SURFACE ( (
 ( 1.000000000000000000, 0.9659258262890683122, 1.000000000000000000, 0.9659258262890683122, 1.000000000000000000, 0.9659258262890683122, 1.000000000000000000, 0.9659258262890683122, 1.000000000000000000, 0.9659258262890683122, 1.000000000000000000, 0.9659258262890683122, 1.000000000000000000, 0.9659258262890683122, 1.000000000000000000, 0.9659258262890683122, 1.000000000000000000, 0.9659258262890683122, 1.000000000000000000, 0.9659258262890683122, 1.000000000000000000, 0.9659258262890683122, 1.000000000000000000, 0.9659258262890683122, 1.000000000000000000, 0.9659258262890683122, 1.000000000000000000, 0.9659258262890683122, 1.000000000000000000, 0.9659258262890683122, 1.000000000000000000, 0.9659258262890683122, 1.000000000000000000, 0.9659258262890683122, 1.000000000000000000, 0.9659258262890683122, 1.000000000000000000, 0.9659258262890683122, 1.000000000000000000, 0.9659258262890683122, 1.000000000000000000, 0.9659258262890683122, 1.000000000000000000, 0.9659258262890683122, 1.000000000000000000, 0.9659258262890683122, 1.000000000000000000, 0.9659258262890683122, 1.000000000000000000, 0.9659258262890683122, 1.000000000000000000, 0.9659258262890683122, 1.000000000000000000, 0.9659258262890683122, 1.000000000000000000, 0.9659258262890683122, 1.000000000000000000, 0.9659258262890683122, 1.000000000000000000, 0.9659258262890683122, 1.000000000000000000, 0.9659258262890683122, 1.000000000000000000, 0.9659258262890683122, 1.000000000000000000, 0.9659258262890683122, 1.000000000000000000, 0.9659258262890683122, 1.000000000000000000, 0.9659258262890683122, 1.000000000000000000, 0.9659258262890683122, 1.000000000000000000, 0.9659258262890683122, 1.000000000000000000, 0.9659258262890683122, 1.000000000000000000, 0.9659258262890683122, 1.000000000000000000, 0.9659258262890683122, 1.000000000000000000, 0.9659258262890683122, 1.000000000000000000, 0.9659258262890683122, 1.000000000000000000, 0.9659258262890683122, 1.000000000000000000, 0.9659258262890683122, 1.000000000000000000, 0.9659258262890683122, 1.000000000000000000, 0.9659258262890683122, 1.000000000000000000, 0.9659258262890683122, 1.000000000000000000, 0.9659258262890683122, 1.000000000000000000, 0.9659258262890683122, 1.000000000000000000, 0.9659258262890683122, 1.000000000000000000, 0.9659258262890683122, 1.000000000000000000, 0.9659258262890683122, 1.000000000000000000, 0.9659258262890683122, 1.000000000000000000, 0.9659258262890683122, 1.000000000000000000, 0.9659258262890683122, 1.000000000000000000, 0.9659258262890683122, 1.000000000000000000, 0.9659258262890683122, 1.000000000000000000, 0.9659258262890683122, 1.000000000000000000, 0.9659258262890683122, 1.000000000000000000, 0.9659258262890683122, 1.000000000000000000, 0.9659258262890683122, 1.000000000000000000, 0.9659258262890683122, 1.000000000000000000, 0.9659258262890683122, 1.000000000000000000, 0.9659258262890683122, 1.000000000000000000, 0.9659258262890683122, 1.000000000000000000, 0.9659258262890683122, 1.000000000000000000, 0.9659258262890683122, 1.000000000000000000, 0.9659258262890683122, 1.000000000000000000, 0.9659258262890683122, 1.000000000000000000, 0.9659258262890683122, 1.000000000000000000, 0.9659258262890683122, 1.000000000000000000, 0.9659258262890683122, 1.000000000000000000, 0.9659258262890683122, 1.000000000000000000, 0.9659258262890683122, 1.000000000000000000, 0.9659258262890683122, 1.000000000000000000, 0.9659258262890683122, 1.000000000000000000, 0.9659258262890683122, 1.000000000000000000, 0.9659258262890683122, 1.000000000000000000, 0.9659258262890683122, 1.000000000000000000, 0.9659258262890683122, 1.000000000000000000, 0.9659258262890683122, 1.000000000000000000, 0.9659258262890683122, 1.000000000000000000, 0.9659258262890683122, 1.000000000000000000, 0.9659258262890683122, 1.000000000000000000, 0.9659258262890683122, 1.000000000000000000, 0.9659258262890683122, 1.000000000000000000, 0.9659258262890683122, 1.000000000000000000, 0.9659258262890683122, 1.000000000000000000, 0.9659258262890683122, 1.000000000000000000, 0.9659258262890683122, 1.000000000000000000, 0.9659258262890683122, 1.000000000000000000, 0.9659258262890683122, 1.000000000000000000, 0.9659258262890683122, 1.000000000000000000, 0.9659258262890683122, 1.000000000000000000, 0.9659258262890683122, 1.000000000000000000, 0.9659258262890683122, 1.000000000000000000, 0.9659258262890683122, 1.000000000000000000, 0.9659258262890683122, 1.000000000000000000, 0.9659258262890683122, 1.000000000000000000, 0.9659258262890683122, 1.000000000000000000, 0.9659258262890683122, 1.000000000000000000, 0.9659258262890683122, 1.000000000000000000, 0.9659258262890683122, 1.000000000000000000, 0.9659258262890683122, 1.000000000000000000, 0.9659258262890683122, 1.000000000000000000, 0.9659258262890683122, 1.000000000000000000, 0.9659258262890683122, 1.000000000000000000, 0.9659258262890683122, 1.000000000000000000, 0.9659258262890683122, 1.000000000000000000, 0.9659258262890683122, 1.000000000000000000, 0.9659258262890683122, 1.000000000000000000, 0.9659258262890683122, 1.000000000000000000, 0.9659258262890683122, 1.000000000000000000, 0.9659258262890683122, 1.000000000000000000, 0.9659258262890683122, 1.000000000000000000, 0.9659258262890683122, 1.000000000000000000, 0.9659258262890683122, 1.000000000000000000, 0.9659258262890683122, 1.000000000000000000, 0.9659258262890683122, 1.000000000000000000, 0.9659258262890683122, 1.000000000000000000, 0.9659258262890683122, 1.000000000000000000, 0.9659258262890683122, 1.000000000000000000, 0.9659258262890683122, 1.000000000000000000, 0.9659258262890683122, 1.000000000000000000, 0.9659258262890683122, 1.000000000000000000, 0.9659258262890683122, 1.000000000000000000, 0.9659258262890683122, 1.000000000000000000, 0.9659258262890683122, 1.000000000000000000, 0.9659258262890683122, 1.000000000000000000, 0.9659258262890683122, 1.000000000000000000, 0.9659258262890683122, 1.000000000000000000, 0.9659258262890683122, 1.000000000000000000, 0.9659258262890683122, 1.000000000000000000, 0.9659258262890683122, 1.000000000000000000, 0.9659258262890683122, 1.000000000000000000, 0.9659258262890683122, 1.000000000000000000, 0.9659258262890683122, 1.000000000000000000, 0.9659258262890683122, 1.000000000000000000, 0.9659258262890683122, 1.000000000000000000, 0.9659258262890683122, 1.000000000000000000, 0.9659258262890683122, 1.000000000000000000, 0.9659258262890683122, 1.000000000000000000, 0.9659258262890683122, 1.000000000000000000, 0.9659258262890683122, 1.000000000000000000, 0.9659258262890683122, 1.000000000000000000, 0.9659258262890683122, 1.000000000000000000, 0.9659258262890683122, 1.000000000000000000, 0.9659258262890683122, 1.000000000000000000, 0.9659258262890683122, 1.000000000000000000, 0.9659258262890683122, 1.000000000000000000, 0.9659258262890683122, 1.000000000000000000, 0.9659258262890683122, 1.000000000000000000, 0.9659258262890683122, 1.000000000000000000, 0.9659258262890683122, 1.000000000000000000, 0.9659258262890683122, 1.000000000000000000, 0.9659258262890683122, 1.000000000000000000, 0.9659258262890683122, 1.000000000000000000, 0.9659258262890683122, 1.000000000000000000, 0.9659258262890683122, 1.000000000000000000, 0.9659258262890683122, 1.000000000000000000, 0.9659258262890683122, 1.000000000000000000, 0.9659258262890683122, 1.000000000000000000, 0.9659258262890683122, 1.000000000000000000, 0.9659258262890683122, 1.000000000000000000, 0.9659258262890683122, 1.000000000000000000, 0.9659258262890683122, 1.000000000000000000, 0.9659258262890683122, 1.000000000000000000, 0.9659258262890683122, 1.000000000000000000, 0.9659258262890683122, 1.000000000000000000, 0.9659258262890683122, 1.000000000000000000, 0.9659258262890683122, 1.000000000000000000, 0.9659258262890683122, 1.000000000000000000, 0.9659258262890683122, 1.000000000000000000, 0.9659258262890683122, 1.000000000000000000, 0.9659258262890683122, 1.000000000000000000, 0.9659258262890683122, 1.000000000000000000, 0.9659258262890683122, 1.000000000000000000, 0.9659258262890683122, 1.000000000000000000, 0.9659258262890683122, 1.000000000000000000, 0.9659258262890683122, 1.000000000000000000, 0.9659258262890683122, 1.000000000000000000, 0.9659258262890683122, 1.000000000000000000, 0.9659258262890683122, 1.000000000000000000, 0.9659258262890683122, 1.000000000000000000, 0.9659258262890683122, 1.000000000000000000, 0.9659258262890683122, 1.000000000000000000, 0.9659258262890683122, 1.000000000000000000, 0.9659258262890683122, 1.000000000000000000, 0.9659258262890683122, 1.000000000000000000, 0.9659258262890683122, 1.000000000000000000, 0.9659258262890683122, 1.000000000000000000, 0.9659258262890683122, 1.000000000000000000, 0.9659258262890683122, 1.000000000000000000, 0.9659258262890683122, 1.000000000000000000, 0.9659258262890683122, 1.000000000000000000, 0.9659258262890683122, 1.000000000000000000, 0.9659258262890683122, 1.000000000000000000, 0.9659258262890683122, 1.000000000000000000, 0.9659258262890683122, 1.000000000000000000, 0.9659258262890683122, 1.000000000000000000, 0.9659258262890683122, 1.000000000000000000, 0.9659258262890683122, 1.000000000000000000, 0.9659258262890683122, 1.000000000000000000, 0.9659258262890683122, 1.000000000000000000, 0.9659258262890683122, 1.000000000000000000, 0.9659258262890683122, 1.000000000000000000, 0.9659258262890683122, 1.000000000000000000, 0.9659258262890683122, 1.000000000000000000, 0.9659258262890683122, 1.000000000000000000, 0.9659258262890683122, 1.000000000000000000, 0.9659258262890683122, 1.000000000000000000, 0.9659258262890683122, 1.000000000000000000, 0.9659258262890683122, 1.000000000000000000, 0.9659258262890683122, 1.000000000000000000, 0.9659258262890683122, 1.000000000000000000, 0.9659258262890683122, 1.000000000000000000, 0.9659258262890683122, 1.000000000000000000, 0.9659258262890683122, 1.000000000000000000, 0.9659258262890683122, 1.000000000000000000, 0.9659258262890683122, 1.000000000000000000, 0.9659258262890683122, 1.000000000000000000, 0.9659258262890683122, 1.000000000000000000, 0.9659258262890683122, 1.000000000000000000, 0.9659258262890683122, 1.000000000000000000, 0.9659258262890683122, 1.000000000000000000, 0.9659258262890683122, 1.000000000000000000, 0.9659258262890683122, 1.000000000000000000, 0.9659258262890683122, 1.000000000000000000, 0.9659258262890683122, 1.000000000000000000, 0.9659258262890683122, 1.000000000000000000, 0.9659258262890683122, 1.000000000000000000, 0.9659258262890683122, 1.000000000000000000, 0.9659258262890683122, 1.000000000000000000, 0.9659258262890683122, 1.000000000000000000, 0.9659258262890683122, 1.000000000000000000, 0.9659258262890683122, 1.000000000000000000, 0.9659258262890683122, 1.000000000000000000, 0.9659258262890683122, 1.000000000000000000, 0.9659258262890683122, 1.000000000000000000, 0.9659258262890683122, 1.000000000000000000, 0.9659258262890683122, 1.000000000000000000, 0.9659258262890683122, 1.000000000000000000, 0.9659258262890683122, 1.000000000000000000, 0.9659258262890683122, 1.000000000000000000, 0.9659258262890683122, 1.000000000000000000, 0.9659258262890683122, 1.000000000000000000, 0.9659258262890683122, 1.000000000000000000, 0.9659258262890683122, 1.000000000000000000, 0.9659258262890683122, 1.000000000000000000, 0.9659258262890683122, 1.000000000000000000, 0.9659258262890683122, 1.000000000000000000, 0.9659258262890683122, 1.000000000000000000, 0.9659258262890683122, 1.000000000000000000, 0.9659258262890683122, 1.000000000000000000, 0.9659258262890683122, 1.000000000000000000),
 ( 1.000000000000000000, 0.9659258262890683122, 1.000000000000000000, 0.9659258262890683122, 1.000000000000000000, 0.9659258262890683122, 1.000000000000000000, 0.9659258262890683122, 1.000000000000000000, 0.9659258262890683122, 1.000000000000000000, 0.9659258262890683122, 1.000000000000000000, 0.9659258262890683122, 1.000000000000000000, 0.9659258262890683122, 1.000000000000000000, 0.9659258262890683122, 1.000000000000000000, 0.9659258262890683122, 1.000000000000000000, 0.9659258262890683122, 1.000000000000000000, 0.9659258262890683122, 1.000000000000000000, 0.9659258262890683122, 1.000000000000000000, 0.9659258262890683122, 1.000000000000000000, 0.9659258262890683122, 1.000000000000000000, 0.9659258262890683122, 1.000000000000000000, 0.9659258262890683122, 1.000000000000000000, 0.9659258262890683122, 1.000000000000000000, 0.9659258262890683122, 1.000000000000000000, 0.9659258262890683122, 1.000000000000000000, 0.9659258262890683122, 1.000000000000000000, 0.9659258262890683122, 1.000000000000000000, 0.9659258262890683122, 1.000000000000000000, 0.9659258262890683122, 1.000000000000000000, 0.9659258262890683122, 1.000000000000000000, 0.9659258262890683122, 1.000000000000000000, 0.9659258262890683122, 1.000000000000000000, 0.9659258262890683122, 1.000000000000000000, 0.9659258262890683122, 1.000000000000000000, 0.9659258262890683122, 1.000000000000000000, 0.9659258262890683122, 1.000000000000000000, 0.9659258262890683122, 1.000000000000000000, 0.9659258262890683122, 1.000000000000000000, 0.9659258262890683122, 1.000000000000000000, 0.9659258262890683122, 1.000000000000000000, 0.9659258262890683122, 1.000000000000000000, 0.9659258262890683122, 1.000000000000000000, 0.9659258262890683122, 1.000000000000000000, 0.9659258262890683122, 1.000000000000000000, 0.9659258262890683122, 1.000000000000000000, 0.9659258262890683122, 1.000000000000000000, 0.9659258262890683122, 1.000000000000000000, 0.9659258262890683122, 1.000000000000000000, 0.9659258262890683122, 1.000000000000000000, 0.9659258262890683122, 1.000000000000000000, 0.9659258262890683122, 1.000000000000000000, 0.9659258262890683122, 1.000000000000000000, 0.9659258262890683122, 1.000000000000000000, 0.9659258262890683122, 1.000000000000000000, 0.9659258262890683122, 1.000000000000000000, 0.9659258262890683122, 1.000000000000000000, 0.9659258262890683122, 1.000000000000000000, 0.9659258262890683122, 1.000000000000000000, 0.9659258262890683122, 1.000000000000000000, 0.9659258262890683122, 1.000000000000000000, 0.9659258262890683122, 1.000000000000000000, 0.9659258262890683122, 1.000000000000000000, 0.9659258262890683122, 1.000000000000000000, 0.9659258262890683122, 1.000000000000000000, 0.9659258262890683122, 1.000000000000000000, 0.9659258262890683122, 1.000000000000000000, 0.9659258262890683122, 1.000000000000000000, 0.9659258262890683122, 1.000000000000000000, 0.9659258262890683122, 1.000000000000000000, 0.9659258262890683122, 1.000000000000000000, 0.9659258262890683122, 1.000000000000000000, 0.9659258262890683122, 1.000000000000000000, 0.9659258262890683122, 1.000000000000000000, 0.9659258262890683122, 1.000000000000000000, 0.9659258262890683122, 1.000000000000000000, 0.9659258262890683122, 1.000000000000000000, 0.9659258262890683122, 1.000000000000000000, 0.9659258262890683122, 1.000000000000000000, 0.9659258262890683122, 1.000000000000000000, 0.9659258262890683122, 1.000000000000000000, 0.9659258262890683122, 1.000000000000000000, 0.9659258262890683122, 1.000000000000000000, 0.9659258262890683122, 1.000000000000000000, 0.9659258262890683122, 1.000000000000000000, 0.9659258262890683122, 1.000000000000000000, 0.9659258262890683122, 1.000000000000000000, 0.9659258262890683122, 1.000000000000000000, 0.9659258262890683122, 1.000000000000000000, 0.9659258262890683122, 1.000000000000000000, 0.9659258262890683122, 1.000000000000000000, 0.9659258262890683122, 1.000000000000000000, 0.9659258262890683122, 1.000000000000000000, 0.9659258262890683122, 1.000000000000000000, 0.9659258262890683122, 1.000000000000000000, 0.9659258262890683122, 1.000000000000000000, 0.9659258262890683122, 1.000000000000000000, 0.9659258262890683122, 1.000000000000000000, 0.9659258262890683122, 1.000000000000000000, 0.9659258262890683122, 1.000000000000000000, 0.9659258262890683122, 1.000000000000000000, 0.9659258262890683122, 1.000000000000000000, 0.9659258262890683122, 1.000000000000000000, 0.9659258262890683122, 1.000000000000000000, 0.9659258262890683122, 1.000000000000000000, 0.9659258262890683122, 1.000000000000000000, 0.9659258262890683122, 1.000000000000000000, 0.9659258262890683122, 1.000000000000000000, 0.9659258262890683122, 1.000000000000000000, 0.9659258262890683122, 1.000000000000000000, 0.9659258262890683122, 1.000000000000000000, 0.9659258262890683122, 1.000000000000000000, 0.9659258262890683122, 1.000000000000000000, 0.9659258262890683122, 1.000000000000000000, 0.9659258262890683122, 1.000000000000000000, 0.9659258262890683122, 1.000000000000000000, 0.9659258262890683122, 1.000000000000000000, 0.9659258262890683122, 1.000000000000000000, 0.9659258262890683122, 1.000000000000000000, 0.9659258262890683122, 1.000000000000000000, 0.9659258262890683122, 1.000000000000000000, 0.9659258262890683122, 1.000000000000000000, 0.9659258262890683122, 1.000000000000000000, 0.9659258262890683122, 1.000000000000000000, 0.9659258262890683122, 1.000000000000000000, 0.9659258262890683122, 1.000000000000000000, 0.9659258262890683122, 1.000000000000000000, 0.9659258262890683122, 1.000000000000000000, 0.9659258262890683122, 1.000000000000000000, 0.9659258262890683122, 1.000000000000000000, 0.9659258262890683122, 1.000000000000000000, 0.9659258262890683122, 1.000000000000000000, 0.9659258262890683122, 1.000000000000000000, 0.9659258262890683122, 1.000000000000000000, 0.9659258262890683122, 1.000000000000000000, 0.9659258262890683122, 1.000000000000000000, 0.9659258262890683122, 1.000000000000000000, 0.9659258262890683122, 1.000000000000000000, 0.9659258262890683122, 1.000000000000000000, 0.9659258262890683122, 1.000000000000000000, 0.9659258262890683122, 1.000000000000000000, 0.9659258262890683122, 1.000000000000000000, 0.9659258262890683122, 1.000000000000000000, 0.9659258262890683122, 1.000000000000000000, 0.9659258262890683122, 1.000000000000000000, 0.9659258262890683122, 1.000000000000000000, 0.9659258262890683122, 1.000000000000000000, 0.9659258262890683122, 1.000000000000000000, 0.9659258262890683122, 1.000000000000000000, 0.9659258262890683122, 1.000000000000000000, 0.9659258262890683122, 1.000000000000000000, 0.9659258262890683122, 1.000000000000000000, 0.9659258262890683122, 1.000000000000000000, 0.9659258262890683122, 1.000000000000000000, 0.9659258262890683122, 1.000000000000000000, 0.9659258262890683122, 1.000000000000000000, 0.9659258262890683122, 1.000000000000000000, 0.9659258262890683122, 1.000000000000000000, 0.9659258262890683122, 1.000000000000000000, 0.9659258262890683122, 1.000000000000000000, 0.9659258262890683122, 1.000000000000000000, 0.9659258262890683122, 1.000000000000000000, 0.9659258262890683122, 1.000000000000000000, 0.9659258262890683122, 1.000000000000000000, 0.9659258262890683122, 1.000000000000000000, 0.9659258262890683122, 1.000000000000000000, 0.9659258262890683122, 1.000000000000000000, 0.9659258262890683122, 1.000000000000000000, 0.9659258262890683122, 1.000000000000000000, 0.9659258262890683122, 1.000000000000000000, 0.9659258262890683122, 1.000000000000000000, 0.9659258262890683122, 1.000000000000000000, 0.9659258262890683122, 1.000000000000000000, 0.9659258262890683122, 1.000000000000000000, 0.9659258262890683122, 1.000000000000000000, 0.9659258262890683122, 1.000000000000000000, 0.9659258262890683122, 1.000000000000000000, 0.9659258262890683122, 1.000000000000000000, 0.9659258262890683122, 1.000000000000000000, 0.9659258262890683122, 1.000000000000000000, 0.9659258262890683122, 1.000000000000000000, 0.9659258262890683122, 1.000000000000000000, 0.9659258262890683122, 1.000000000000000000, 0.9659258262890683122, 1.000000000000000000, 0.9659258262890683122, 1.000000000000000000, 0.9659258262890683122, 1.000000000000000000, 0.9659258262890683122, 1.000000000000000000, 0.9659258262890683122, 1.000000000000000000, 0.9659258262890683122, 1.000000000000000000, 0.9659258262890683122, 1.000000000000000000, 0.9659258262890683122, 1.000000000000000000, 0.9659258262890683122, 1.000000000000000000, 0.9659258262890683122, 1.000000000000000000, 0.9659258262890683122, 1.000000000000000000, 0.9659258262890683122, 1.000000000000000000, 0.9659258262890683122, 1.000000000000000000, 0.9659258262890683122, 1.000000000000000000, 0.9659258262890683122, 1.000000000000000000, 0.9659258262890683122, 1.000000000000000000, 0.9659258262890683122, 1.000000000000000000, 0.9659258262890683122, 1.000000000000000000, 0.9659258262890683122, 1.000000000000000000, 0.9659258262890683122, 1.000000000000000000, 0.9659258262890683122, 1.000000000000000000, 0.9659258262890683122, 1.000000000000000000, 0.9659258262890683122, 1.000000000000000000, 0.9659258262890683122, 1.000000000000000000, 0.9659258262890683122, 1.000000000000000000, 0.9659258262890683122, 1.000000000000000000, 0.9659258262890683122, 1.000000000000000000, 0.9659258262890683122, 1.000000000000000000, 0.9659258262890683122, 1.000000000000000000, 0.9659258262890683122, 1.000000000000000000, 0.9659258262890683122, 1.000000000000000000, 0.9659258262890683122, 1.000000000000000000, 0.9659258262890683122, 1.000000000000000000, 0.9659258262890683122, 1.000000000000000000, 0.9659258262890683122, 1.000000000000000000, 0.9659258262890683122, 1.000000000000000000, 0.9659258262890683122, 1.000000000000000000, 0.9659258262890683122, 1.000000000000000000, 0.9659258262890683122, 1.000000000000000000, 0.9659258262890683122, 1.000000000000000000, 0.9659258262890683122, 1.000000000000000000, 0.9659258262890683122, 1.000000000000000000, 0.9659258262890683122, 1.000000000000000000, 0.9659258262890683122, 1.000000000000000000, 0.9659258262890683122, 1.000000000000000000, 0.9659258262890683122, 1.000000000000000000, 0.9659258262890683122, 1.000000000000000000, 0.9659258262890683122, 1.000000000000000000, 0.9659258262890683122, 1.000000000000000000, 0.9659258262890683122, 1.000000000000000000, 0.9659258262890683122, 1.000000000000000000, 0.9659258262890683122, 1.000000000000000000, 0.9659258262890683122, 1.000000000000000000, 0.9659258262890683122, 1.000000000000000000, 0.9659258262890683122, 1.000000000000000000, 0.9659258262890683122, 1.000000000000000000, 0.9659258262890683122, 1.000000000000000000, 0.9659258262890683122, 1.000000000000000000, 0.9659258262890683122, 1.000000000000000000, 0.9659258262890683122, 1.000000000000000000, 0.9659258262890683122, 1.000000000000000000, 0.9659258262890683122, 1.000000000000000000, 0.9659258262890683122, 1.000000000000000000, 0.9659258262890683122, 1.000000000000000000, 0.9659258262890683122, 1.000000000000000000, 0.9659258262890683122, 1.000000000000000000, 0.9659258262890683122, 1.000000000000000000, 0.9659258262890683122, 1.000000000000000000, 0.9659258262890683122, 1.000000000000000000, 0.9659258262890683122, 1.000000000000000000, 0.9659258262890683122, 1.000000000000000000, 0.9659258262890683122, 1.000000000000000000, 0.9659258262890683122, 1.000000000000000000, 0.9659258262890683122, 1.000000000000000000, 0.9659258262890683122, 1.000000000000000000, 0.9659258262890683122, 1.000000000000000000, 0.9659258262890683122, 1.000000000000000000, 0.9659258262890683122, 1.000000000000000000) ) ) 
 REPRESENTATION_ITEM ( '' )  SURFACE ( )  );
#19405 = CARTESIAN_POINT ( 'NONE',  ( 1.476377952755906220, 0.1660481256975883668, -0.3530559997133364547 ) ) ;
#19404 = DIRECTION ( 'NONE',  ( 0.7071067811865472397, 0.000000000000000000, 0.7071067811865476838 ) ) ;
#19406 = CARTESIAN_POINT ( 'NONE',  ( 1.377952755905512472, 0.2952755905511811885, 0.000000000000000000 ) ) ;
#19407 = CARTESIAN_POINT ( 'NONE',  ( 0.3917322834645669549, 0.1049643490035304660, -2.636482939632545541 ) ) ;
#19408 = CARTESIAN_POINT ( 'NONE',  ( -1.568241469816272105, -0.3162353388693409650, -0.4822834645669289433 ) ) ;
#19409 = CARTESIAN_POINT ( 'NONE',  ( -1.017060367454067249, -0.3162353388693409650, -0.4822834645669289433 ) ) ;
#19410 = CARTESIAN_POINT ( 'NONE',  ( 0.4091458600556403535, 0.2362204724409449896, -0.6036745406824146620 ) ) ;
#19411 = CARTESIAN_POINT ( 'NONE',  ( -0.2925321140481932924, 0.2925321140481931814, 0.1377952755905511584 ) ) ;
#19412 = ORIENTED_EDGE ( 'NONE', *, *, #153, .F. ) ;
#19413 = CARTESIAN_POINT ( 'NONE',  ( -0.09186351706036663400, -0.3690944881889763329, 0.3153832671262228327 ) ) ;
#19414 = CARTESIAN_POINT ( 'NONE',  ( 0.1958661417322836440, -0.3392501089628017219, -1.973753280839895208 ) ) ;
#19415 = VERTEX_POINT ( 'NONE', #47233 ) ;
#19416 = CARTESIAN_POINT ( 'NONE',  ( 0.1771653543307093182, 0.1660481256975885056, 0.3530559997133364547 ) ) ;
#19417 = CARTESIAN_POINT ( 'NONE',  ( 0.5052493438320215802, 0.2952755905511811885, 0.1292274648535926551 ) ) ;
#19418 = CARTESIAN_POINT ( 'NONE',  ( -0.1938976377952756625, 0.1938976377952755792, 0.07874015748031495954 ) ) ;
#19419 = CARTESIAN_POINT ( 'NONE',  ( 3.924389226575468737, 2.559055118110236560, 0.3149606299212599492 ) ) ;
#19420 = CARTESIAN_POINT ( 'NONE',  ( -0.2559055118110227234, -0.4536011799217367080, 0.2665933059059888421 ) ) ;
#19421 = CARTESIAN_POINT ( 'NONE',  ( 0.7152230971128616943, -0.05778040916215522460, 0.4822834645669289988 ) ) ;
#19422 = CARTESIAN_POINT ( 'NONE',  ( 1.017060367454068581, -0.08942795157528024563, -0.3641732283464568787 ) ) ;
#19423 = CARTESIAN_POINT ( 'NONE',  ( 0.1574803149606306130, -0.1870078740157480879, -0.4822834645669291653 ) ) ;
#19424 = CARTESIAN_POINT ( 'NONE',  ( -0.3917322834645668994, -0.1049643490035306742, -1.070846825950444448 ) ) ;
#19425 = CARTESIAN_POINT ( 'NONE',  ( -0.7742782152230962556, -0.4281496062992127816, -0.4176697321401328100 ) ) ;
#19426 = CARTESIAN_POINT ( 'NONE',  ( -1.443569553805773564, -0.5023911411419708095, 0.1820866141732285504 ) ) ;
#19427 = CARTESIAN_POINT ( 'NONE',  ( -0.6430446194225716283, -0.4281496062992124485, 0.4176697321401328655 ) ) ;
#19428 = CARTESIAN_POINT ( 'NONE',  ( 0.000000000000000000, 0.4374015748031496176, 0.000000000000000000 ) ) ;
#19429 = CARTESIAN_POINT ( 'NONE',  ( 0.2726377952755905665, -0.1133856558944469489, 0.1574803149606299191 ) ) ;
#19430 = ORIENTED_EDGE ( 'NONE', *, *, #9579, .T. ) ;
#19431 = CARTESIAN_POINT ( 'NONE',  ( 0.3392501089628018329, 0.1958661417322835607, -2.332696481136169453 ) ) ;
#19432 = CARTESIAN_POINT ( 'NONE',  ( -0.1574803149606292529, -0.1870078740157480879, -0.4822834645669291653 ) ) ;
#19433 = ORIENTED_EDGE ( 'NONE', *, *, #28964, .F. ) ;
#19434 = CARTESIAN_POINT ( 'NONE',  ( -0.5839895013123351797, 0.2952755905511810774, -0.1292274648535930714 ) ) ;
#19435 = CARTESIAN_POINT ( 'NONE',  ( 1.305774278215223960, 0.2952755905511810774, -0.1292274648535930714 ) ) ;
#19436 = CARTESIAN_POINT ( 'NONE',  ( 1.082677165354331228, -0.5400638737290844871, 0.3530559997133364547 ) ) ;
#19437 = CARTESIAN_POINT ( 'NONE',  ( 0.6364829396325465405, -0.05778040916215522460, 0.4822834645669289988 ) ) ;
#19438 = CARTESIAN_POINT ( 'NONE',  ( 0.1902887139107617975, -0.6692913385826773087, -0.1292274648535924053 ) ) ;
#19439 = CARTESIAN_POINT ( 'NONE',  ( 0.2867679344610365999, -0.2867679344610365444, -1.442913385826771755 ) ) ;
#19440 = CARTESIAN_POINT ( 'NONE',  ( -1.174540682414697335, -0.3162353388693409650, -0.4822834645669289433 ) ) ;
#19441 = CARTESIAN_POINT ( 'NONE',  ( -0.2755905511811015396, -0.6692913385826771977, 8.415575281601705876E-17 ) ) ;
#19442 = CIRCLE ( 'NONE', #11347, 0.1771653543307088186 ) ;
#19443 = CARTESIAN_POINT ( 'NONE',  ( 0.08530183727034192087, -0.08942795157527998196, 0.3641732283464567121 ) ) ;
#19444 = CARTESIAN_POINT ( 'NONE',  ( -0.2597269936800725709, -0.1406511682536830121, 5.810287953473523892 ) ) ;
#19445 = CARTESIAN_POINT ( 'NONE',  ( -0.1377952755905504645, 0.1660481256975885056, 0.3530559997133364547 ) ) ;
#19446 = CARTESIAN_POINT ( 'NONE',  ( 3.910259856776663767, 1.664469867010863746, -0.4581933108574676172 ) ) ;
#19447 = CARTESIAN_POINT ( 'NONE',  ( 1.030183727034121421, -0.3162353388693409650, -0.4822834645669289433 ) ) ;
#19448 = CARTESIAN_POINT ( 'NONE',  ( 0.5183727034120741983, 0.2066929133858267098, -0.1054918080437494132 ) ) ;
#19449 = ORIENTED_EDGE ( 'NONE', *, *, #14771, .F. ) ;
#19450 = VERTEX_POINT ( 'NONE', #72922 ) ;
#19451 = CARTESIAN_POINT ( 'NONE',  ( 0.3740157480314966754, -0.5400638737290844871, 0.3530559997133364547 ) ) ;
#19452 = CARTESIAN_POINT ( 'NONE',  ( -0.1115485564304456306, 0.1771653543307087075, -0.09757992244046823083 ) ) ;
#19454 = CARTESIAN_POINT ( 'NONE',  ( -0.06680712611108347021, -4.070224344450961593E-15, 0.3627989612356168347 ) ) ;
#19453 = CARTESIAN_POINT ( 'NONE',  ( 1.318897637795276356, -0.4536011799217367080, 0.2665933059059888421 ) ) ;
#19455 = CARTESIAN_POINT ( 'NONE',  ( 0.1958661417322834775, 0.3392501089628018884, -1.016404199475065662 ) ) ;
#19456 = CARTESIAN_POINT ( 'NONE',  ( 0.3458507752293908943, -0.3458507752293908943, -0.3326771653543306728 ) ) ;
#19457 = CARTESIAN_POINT ( 'NONE',  ( 1.679790026246720025, 0.1283753931104748280, 0.1820866141732283561 ) ) ;
#19458 = CARTESIAN_POINT ( 'NONE',  ( -1.437007874015747477, 0.1660481256975883668, -0.3530559997133364547 ) ) ;
#19459 = CONICAL_SURFACE ( 'NONE', #6055, 3.543307086614173151, 0.7853981633974691512 ) ;
#19460 = CARTESIAN_POINT ( 'NONE',  ( -0.3460692066303957537, -0.1998031496062994405, -2.648950131233595684 ) ) ;
#19461 = CARTESIAN_POINT ( 'NONE',  ( 0.1312335958005255154, -0.6046776061558807314, 0.2411417322834647770 ) ) ;
#19462 = CARTESIAN_POINT ( 'NONE',  ( -1.174540682414697335, -0.05778040916215522460, 0.4822834645669289988 ) ) ;
#19463 = CARTESIAN_POINT ( 'NONE',  ( -1.187664041994750175, -0.05778040916215560624, -0.4822834645669293319 ) ) ;
#19464 = CARTESIAN_POINT ( 'NONE',  ( 0.2427821522309716595, -0.3162353388693409650, -0.4822834645669289433 ) ) ;
#19465 = CARTESIAN_POINT ( 'NONE',  ( 0.1974969037888704704, 0.3420746716998660508, 0.09383202099737533719 ) ) ;
#19466 = CARTESIAN_POINT ( 'NONE',  ( 1.660104986876641320, -0.05778040916215522460, 0.4822834645669289988 ) ) ;
#19467 = CARTESIAN_POINT ( 'NONE',  ( 0.7611548556430451917, -0.6046776061558807314, 0.2411417322834647770 ) ) ;
#19468 = CARTESIAN_POINT ( 'NONE',  ( 1.010498687664042716, -0.3690944881889763329, 0.3153832671262228327 ) ) ;
#19469 = CARTESIAN_POINT ( 'NONE',  ( 0.7998211177050879028, 0.000000000000000000, 0.3464511005275205946 ) ) ;
#19470 = CARTESIAN_POINT ( 'NONE',  ( 0.8398950131233602345, -0.5023911411419708095, 0.1820866141732285504 ) ) ;
#19471 = CARTESIAN_POINT ( 'NONE',  ( -1.128608923884513837, 0.2306618581243847221, -0.2411417322834647770 ) ) ;
#19472 = CARTESIAN_POINT ( 'NONE',  ( -0.1070741851644056997, 0.3996062992125984925, -0.7132545931758530466 ) ) ;
#19473 = CARTESIAN_POINT ( 'NONE',  ( 1.036745406824147731, 0.05413385826771666132, 0.4176697321401328100 ) ) ;
#19474 = CARTESIAN_POINT ( 'NONE',  ( -0.2867679344610365999, 0.2867679344610364889, -0.6417322834645668994 ) ) ;
#19476 = CARTESIAN_POINT ( 'NONE',  ( 0.000000000000000000, 0.000000000000000000, -2.755905511811024056 ) ) ;
#19475 = CARTESIAN_POINT ( 'NONE',  ( 0.5314960629921267055, -0.5400638737290844871, 0.3530559997133364547 ) ) ;
#19477 = CARTESIAN_POINT ( 'NONE',  ( -1.646981627296586703, -0.2845877964562161244, -0.3641732283464567121 ) ) ;
#19478 = CARTESIAN_POINT ( 'NONE',  ( 0.09186351706036827158, 0.05413385826771666132, 0.4176697321401328100 ) ) ;
#19479 = CARTESIAN_POINT ( 'NONE',  ( 0.5839895013123367340, -0.5511811023622048555, -0.09757992244046775898 ) ) ;
#19480 = CARTESIAN_POINT ( 'NONE',  ( 0.6627296587926517768, -0.6692913385826773087, -0.1292274648535924053 ) ) ;
#19481 = CARTESIAN_POINT ( 'NONE',  ( 0.7611548556430454138, 0.1539470093639521697, -0.1968503937007875793 ) ) ;
#19482 = CARTESIAN_POINT ( 'NONE',  ( -0.9908136482939626788, -0.5511811023622048555, -0.09757992244046775898 ) ) ;
#19483 = CARTESIAN_POINT ( 'NONE',  ( -0.5511811023622041894, -0.1870078740157480879, -0.4822834645669291653 ) ) ;
#19484 = CARTESIAN_POINT ( 'NONE',  ( 1.633858267716535639, -0.5400638737290844871, 0.3530559997133364547 ) ) ;
#19485 = CARTESIAN_POINT ( 'NONE',  ( -1.194225721784776262, 0.05413385826771626580, -0.4176697321401330321 ) ) ;
#19486 = CARTESIAN_POINT ( 'NONE',  ( 1.135170603674541256, -0.6692913385826773087, -0.1292274648535924053 ) ) ;
#19487 = CARTESIAN_POINT ( 'NONE',  ( -1.384514435695537005, -0.5511811023622048555, -0.09757992244046775898 ) ) ;
#19488 = CARTESIAN_POINT ( 'NONE',  ( -0.7478466213799872531, 1.968503937007873850, -0.5309055118110235227 ) ) ;
#19489 = CARTESIAN_POINT ( 'NONE',  ( 1.161417322834646271, 0.1660481256975883668, -0.3530559997133364547 ) ) ;
#19490 = CARTESIAN_POINT ( 'NONE',  ( -0.4724409448818899238, 0.1265901696524986686, -2.314304461942256808 ) ) ;
#19491 = CARTESIAN_POINT ( 'NONE',  ( -1.594488188976377563, -0.5400638737290844871, 0.3530559997133364547 ) ) ;
#19492 = CARTESIAN_POINT ( 'NONE',  ( -1.561679790026246017, -0.3690944881889765550, -0.3153832671262227771 ) ) ;
#19493 = CARTESIAN_POINT ( 'NONE',  ( -0.9580052493438311334, -0.3690944881889763329, 0.3153832671262228327 ) ) ;
#19494 = CARTESIAN_POINT ( 'NONE',  ( -1.948818897637795367, 0.000000000000000000, 5.701968306260621233 ) ) ;
#19495 = CARTESIAN_POINT ( 'NONE',  ( -0.2296587926509179312, -0.05778040916215522460, 0.4822834645669289988 ) ) ;
#19496 = CARTESIAN_POINT ( 'NONE',  ( -0.4330708661417315697, -0.5511811023622047445, 6.969142054262312111E-17 ) ) ;
#19497 = CARTESIAN_POINT ( 'NONE',  ( -1.607611548556429737, -0.5511811023622046335, 0.09757992244046803654 ) ) ;
#19498 = CARTESIAN_POINT ( 'NONE',  ( 0.8070866141732288002, 0.07958543189024085140, 0.2665933059059887866 ) ) ;
#19499 = CARTESIAN_POINT ( 'NONE',  ( 0.3674540682414705883, -0.6046776061558807314, 0.2411417322834647770 ) ) ;
#19500 = CARTESIAN_POINT ( 'NONE',  ( 1.338582677165355062, -0.1870078740157480879, -0.4822834645669291653 ) ) ;
#19501 = CARTESIAN_POINT ( 'NONE',  ( 0.3346456692913393205, -0.5400638737290845981, -0.3530559997133363437 ) ) ;
#19502 = CARTESIAN_POINT ( 'NONE',  ( 0.4396325459317590445, -0.5511811023622046335, 0.09757992244046803654 ) ) ;
#19503 = CARTESIAN_POINT ( 'NONE',  ( 1.476377952755906220, 0.1660481256975883668, -0.3530559997133364547 ) ) ;
#19504 = CARTESIAN_POINT ( 'NONE',  ( -1.148293963254592542, 0.2952755905511811885, 0.1292274648535926551 ) ) ;
#19505 = CARTESIAN_POINT ( 'NONE',  ( -0.6167979002624665030, 0.05413385826771666132, 0.4176697321401328100 ) ) ;
#19506 = CARTESIAN_POINT ( 'NONE',  ( -0.1070741851644057135, 0.3996062992125985480, -0.3215223097112860917 ) ) ;
#19507 = CARTESIAN_POINT ( 'NONE',  ( 0.2952755905511810774, 0.000000000000000000, -1.220472440944881942 ) ) ;
#19508 = CARTESIAN_POINT ( 'NONE',  ( -0.05905511811023545637, -0.5400638737290845981, -0.3530559997133363437 ) ) ;
#19509 = CARTESIAN_POINT ( 'NONE',  ( 1.135170603674541256, 0.1771653543307087630, 0.09757992244046791164 ) ) ;
#19510 = CARTESIAN_POINT ( 'NONE',  ( -0.5971128608923877978, -0.6692913385826773087, -0.1292274648535924053 ) ) ;
#19511 = CARTESIAN_POINT ( 'NONE',  ( 0.2165354330708668673, 0.1660481256975883668, -0.3530559997133364547 ) ) ;
#19512 = CARTESIAN_POINT ( 'NONE',  ( 0.3996062992125986590, -0.1070741851644053111, -2.158792650918635037 ) ) ;
#19513 = CIRCLE ( 'NONE', #15515, 0.3937007874015748254 ) ;
#19514 = CARTESIAN_POINT ( 'NONE',  ( -9.674558042662121740E-17, 0.3949938075777409963, -2.047244094488188892 ) ) ;
#19515 = CARTESIAN_POINT ( 'NONE',  ( -0.1958661417322836718, 0.3392501089628017219, -0.4776902887139107268 ) ) ;
#19516 = CARTESIAN_POINT ( 'NONE',  ( 0.2445414048442311472, -0.1655124888405462846, 5.638514421976807078 ) ) ;
#19517 = CARTESIAN_POINT ( 'NONE',  ( 0.3392501089628018884, -0.1958661417322834220, -1.041994750656167756 ) ) ;
#19518 = CARTESIAN_POINT ( 'NONE',  ( -0.9120734908136475250, 0.1771653543307087630, 0.09757992244046791164 ) ) ;
#19519 = CARTESIAN_POINT ( 'NONE',  ( -1.318897637795274802, -0.5400638737290845981, -0.3530559997133363437 ) ) ;
#19520 = CARTESIAN_POINT ( 'NONE',  ( 0.3949938075777409963, 2.418639510665530743E-17, -2.714566929133857887 ) ) ;
#19521 = CARTESIAN_POINT ( 'NONE',  ( 0.2952755905511819101, 0.1660481256975883668, -0.3530559997133364547 ) ) ;
#19522 = CARTESIAN_POINT ( 'NONE',  ( 1.161417322834646271, 0.1660481256975883668, -0.3530559997133364547 ) ) ;
#19523 = CARTESIAN_POINT ( 'NONE',  ( 0.6364829396325465405, -0.05778040916215522460, 0.4822834645669289988 ) ) ;
#19524 = CARTESIAN_POINT ( 'NONE',  ( 5.785732909357575061E-17, -0.4724409448818898682, -2.913385826771653697 ) ) ;
#19525 = CARTESIAN_POINT ( 'NONE',  ( -0.1998031496062994683, 0.3460692066303958092, -2.532808398950130879 ) ) ;
#19526 = CARTESIAN_POINT ( 'NONE',  ( -0.1049643490035307158, 0.3917322834645670104, -0.7907017304800020296 ) ) ;
#19527 = CARTESIAN_POINT ( 'NONE',  ( 0.3215223097112867578, -0.05778040916215522460, 0.4822834645669289988 ) ) ;
#19528 = CARTESIAN_POINT ( 'NONE',  ( 0.03937007874015806264, 0.2952755905511811885, 0.000000000000000000 ) ) ;
#19529 = CARTESIAN_POINT ( 'NONE',  ( 0.9448818897637802916, -0.1870078740157479769, 0.3641732283464567677 ) ) ;
#19530 = CARTESIAN_POINT ( 'NONE',  ( 1.469816272965879911, -0.6046776061558807314, 0.2411417322834647770 ) ) ;
#19531 = CARTESIAN_POINT ( 'NONE',  ( -0.3917322834645669549, -0.1049643490035306603, 0.02690288713910752097 ) ) ;
#19532 = CARTESIAN_POINT ( 'NONE',  ( 0.3412073490813655186, 0.2306618581243848609, 0.2411417322834645549 ) ) ;
#19533 = CARTESIAN_POINT ( 'NONE',  ( 1.174540682414699111, -0.3162353388693405765, 0.4822834645669290543 ) ) ;
#19534 = CARTESIAN_POINT ( 'NONE',  ( 0.5708661417322842269, 0.1660481256975885056, 0.3530559997133364547 ) ) ;
#19535 = CARTESIAN_POINT ( 'NONE',  ( 1.095800524934383846, -0.08942795157528024563, -0.3641732283464568787 ) ) ;
#19536 = CARTESIAN_POINT ( 'NONE',  ( -1.082677165354329896, 0.1660481256975885056, 0.3530559997133364547 ) ) ;
#19537 = CARTESIAN_POINT ( 'NONE',  ( -0.9186351706036736120, 0.2306618581243848609, 0.2411417322834645549 ) ) ;
#19538 = CARTESIAN_POINT ( 'NONE',  ( 1.332020997375328974, -0.05778040916215560624, -0.4822834645669293319 ) ) ;
#19539 = CARTESIAN_POINT ( 'NONE',  ( 0.2867679344610365999, 0.2867679344610365999, -0.6948818897637795144 ) ) ;
#19540 = CARTESIAN_POINT ( 'NONE',  ( -0.2867679344610365999, 0.2867679344610364889, -2.059055118110236116 ) ) ;
#19541 = CARTESIAN_POINT ( 'NONE',  ( -0.1958661417322834220, -0.3392501089628018884, -2.892388451443569153 ) ) ;
#19542 = VERTEX_POINT ( 'NONE', #40935 ) ;
#19543 = CARTESIAN_POINT ( 'NONE',  ( 0.3460692066303959757, -0.1998031496062991907, 0.05249343832020995915 ) ) ;
#19544 = ORIENTED_EDGE ( 'NONE', *, *, #24864, .F. ) ;
#19545 = CARTESIAN_POINT ( 'NONE',  ( 1.437007874015748810, -0.5400638737290845981, -0.3530559997133363437 ) ) ;
#19546 = CARTESIAN_POINT ( 'NONE',  ( 1.089238845144357537, -0.3690944881889763329, 0.3153832671262228327 ) ) ;
#19547 = CARTESIAN_POINT ( 'NONE',  ( 0.1998031496062992740, 0.3460692066303959757, -1.404199475065616820 ) ) ;
#19548 = CARTESIAN_POINT ( 'NONE',  ( 1.187664041994751285, -0.08942795157527998196, 0.3641732283464567121 ) ) ;
#19549 = CARTESIAN_POINT ( 'NONE',  ( 0.4724409448818898682, 2.892866454678787531E-17, -0.2755905511811023723 ) ) ;
#19550 = CARTESIAN_POINT ( 'NONE',  ( -0.1656158939409619058, 1.092528437896311155, 2.846760252546623793 ) ) ;
#19551 = DIRECTION ( 'NONE',  ( 0.000000000000000000, -0.6427876096865364763, -0.7660444431189804559 ) ) ;
#19552 = CARTESIAN_POINT ( 'NONE',  ( -0.1958661417322836718, 0.3392501089628017219, -1.042650918635170676 ) ) ;
#19553 = CARTESIAN_POINT ( 'NONE',  ( -1.154855643044618851, 0.1283753931104748280, 0.1820866141732283561 ) ) ;
#19554 = CARTESIAN_POINT ( 'NONE',  ( -1.673228346456691717, 0.07958543189024071263, -0.2665933059059888421 ) ) ;
#19555 = CARTESIAN_POINT ( 'NONE',  ( -1.246719160104985846, -0.4281496062992127816, -0.4176697321401328100 ) ) ;
#19556 = CARTESIAN_POINT ( 'NONE',  ( -0.09842519685039295696, 0.1660481256975883668, -0.3530559997133364547 ) ) ;
#19557 = CARTESIAN_POINT ( 'NONE',  ( 1.509186351706037543, -0.4281496062992127816, -0.4176697321401328100 ) ) ;
#19558 = ORIENTED_EDGE ( 'NONE', *, *, #67626, .T. ) ;
#19559 = CARTESIAN_POINT ( 'NONE',  ( -1.028297472258253853, 1.383492524721027017, -0.4490203305827997204 ) ) ;
#19560 = SHAPE_REPRESENTATION_RELATIONSHIP ( 'NONE' , 'NONE' ,  #61632, #56452 ) ;
#19561 = CARTESIAN_POINT ( 'NONE',  ( 5.785732909357575061E-17, -0.4724409448818898682, -2.125984251968504157 ) ) ;
#19562 = CARTESIAN_POINT ( 'NONE',  ( -1.157146581871515012E-16, 0.4724409448818898682, -2.677165354330708347 ) ) ;
#19563 = CARTESIAN_POINT ( 'NONE',  ( -0.3049517105654738214, -2.191421614605370878E-15, 0.4445507791589071167 ) ) ;
#19564 = CARTESIAN_POINT ( 'NONE',  ( -1.095800524934382292, -0.2845877964562161244, -0.3641732283464567121 ) ) ;
#19565 = CARTESIAN_POINT ( 'NONE',  ( -1.325459317585300889, 0.05413385826771666132, 0.4176697321401328100 ) ) ;
#19566 = CARTESIAN_POINT ( 'NONE',  ( 0.7808398950131241190, -0.05778040916215560624, -0.4822834645669293319 ) ) ;
#19567 = AXIS2_PLACEMENT_3D ( 'NONE', #70735, #26539, #78737 ) ;
#19568 = EDGE_LOOP ( 'NONE', ( #43040, #31007, #55469, #65926, #12910, #911, #19142, #49775, #52868, #26137, #56373, #37975, #49891, #28631, #35273, #59296, #55935, #68851, #12924 ) ) ;
#19570 = CARTESIAN_POINT ( 'NONE',  ( -0.4724409448818880364, -0.1265901696525023323, -2.642388451443570485 ) ) ;
#19569 = CARTESIAN_POINT ( 'NONE',  ( 0.000000000000000000, 0.000000000000000000, 2.362204724409448620 ) ) ;
#19571 = CARTESIAN_POINT ( 'NONE',  ( 1.233595800524935227, 0.2306618581243847221, -0.2411417322834647770 ) ) ;
#19572 = CARTESIAN_POINT ( 'NONE',  ( -1.456692913385826182, -0.6692913385826771977, 8.415575281601705876E-17 ) ) ;
#19573 = CARTESIAN_POINT ( 'NONE',  ( 0.3917322834645668994, -0.1049643490035303134, -0.8215029939294470340 ) ) ;
#19574 = CARTESIAN_POINT ( 'NONE',  ( -0.3937007874015740483, -0.1870078740157480601, -0.3641732283464567677 ) ) ;
#19575 = CARTESIAN_POINT ( 'NONE',  ( -1.272965879265091305, -0.004921259842519870586, -0.3153832671262229437 ) ) ;
#19576 = CARTESIAN_POINT ( 'NONE',  ( 0.3917322834645670104, -0.1049643490035303273, -1.141076115485564202 ) ) ;
#19577 = CARTESIAN_POINT ( 'NONE',  ( -0.4002624671916004129, -0.2845877964562159024, 0.3641732283464567677 ) ) ;
#19578 = CARTESIAN_POINT ( 'NONE',  ( 0.2887139107611556010, -0.5023911411419708095, 0.1820866141732285504 ) ) ;
#19579 = CARTESIAN_POINT ( 'NONE',  ( 0.03937007874015806264, 0.2952755905511811885, 0.000000000000000000 ) ) ;
#19580 = CARTESIAN_POINT ( 'NONE',  ( -0.9973753280839886548, 0.1283753931104748280, 0.1820866141732283561 ) ) ;
#19581 = CARTESIAN_POINT ( 'NONE',  ( -0.3917322834645670104, -7.196005306013484475E-17, -2.551181102362204633 ) ) ;
#19582 = CARTESIAN_POINT ( 'NONE',  ( 1.154855643044620184, 0.2306618581243847221, -0.2411417322834647770 ) ) ;
#19583 = EDGE_CURVE ( 'NONE', #32176, #44890, #16904, .T. ) ;
#19584 = CARTESIAN_POINT ( 'NONE',  ( -1.482939632545930975, 0.05413385826771666132, 0.4176697321401328100 ) ) ;
#19585 = CARTESIAN_POINT ( 'NONE',  ( 0.3458507752293908943, -0.3458507752293908943, -1.277559055118109965 ) ) ;
#19586 = CARTESIAN_POINT ( 'NONE',  ( -0.2362204724409442680, -0.1870078740157480879, -0.4822834645669291653 ) ) ;
#19587 = CARTESIAN_POINT ( 'NONE',  ( -1.056430446194224881, -0.6692913385826771977, 0.1292274648535927661 ) ) ;
#19588 = CARTESIAN_POINT ( 'NONE',  ( 0.9448818897637802916, -0.1870078740157480601, -0.3641732283464567677 ) ) ;
#19589 = CARTESIAN_POINT ( 'NONE',  ( -0.5118110236220466680, -0.5511811023622047445, 6.969142054262312111E-17 ) ) ;
#19590 = CARTESIAN_POINT ( 'NONE',  ( -0.5839895013123351797, 0.2952755905511810774, -0.1292274648535930714 ) ) ;
#19591 = CARTESIAN_POINT ( 'NONE',  ( -1.522309711286088607, -0.6046776061558807314, 0.2411417322834647770 ) ) ;
#19592 = DIRECTION ( 'NONE',  ( 0.000000000000000000, 0.000000000000000000, -1.000000000000000000 ) ) ;
#19593 = CARTESIAN_POINT ( 'NONE',  ( 1.469816272965879911, -0.5023911411419708095, 0.1820866141732285504 ) ) ;
#19594 = CARTESIAN_POINT ( 'NONE',  ( -0.4593175853018364174, -0.4281496062992127816, -0.4176697321401328100 ) ) ;
#19595 = CARTESIAN_POINT ( 'NONE',  ( -1.325459317585300889, -0.4281496062992127816, -0.4176697321401328100 ) ) ;
#19596 = EDGE_LOOP ( 'NONE', ( #72255, #62103 ) ) ;
#19597 = CARTESIAN_POINT ( 'NONE',  ( 0.3460692066303958092, 0.1998031496062993018, -2.255249343832020692 ) ) ;
#19598 = CARTESIAN_POINT ( 'NONE',  ( -0.7742782152230962556, -0.3690944881889765550, -0.3153832671262227771 ) ) ;
#19599 = CARTESIAN_POINT ( 'NONE',  ( 0.6889763779527563470, 0.1660481256975883668, -0.3530559997133364547 ) ) ;
#19600 = CARTESIAN_POINT ( 'NONE',  ( -1.043307086614172707, 0.07958543189024071263, -0.2665933059059888421 ) ) ;
#19601 = CARTESIAN_POINT ( 'NONE',  ( -0.2925321140481930149, -0.2925321140481933480, -1.395669291338582640 ) ) ;
#19602 = CARTESIAN_POINT ( 'NONE',  ( -1.056430446194224881, 0.2952755905511810774, -0.1292274648535930714 ) ) ;
#19603 = AXIS2_PLACEMENT_3D ( 'NONE', #78352, #77931, #13124 ) ;
#19604 = CARTESIAN_POINT ( 'NONE',  ( 0.8136482939632553313, -0.6046776061558809534, -0.2411417322834644161 ) ) ;
#19605 = CARTESIAN_POINT ( 'NONE',  ( 0.5314960629921267055, -0.5400638737290844871, 0.3530559997133364547 ) ) ;
#19606 = LINE ( 'NONE', #70964, #14353 ) ;
#19607 = CARTESIAN_POINT ( 'NONE',  ( -1.384514435695537005, 0.1771653543307087630, 0.09757992244046791164 ) ) ;
#19608 = CARTESIAN_POINT ( 'NONE',  ( 0.1998031496062994128, -0.3460692066303957537, -0.7985564304461942875 ) ) ;
#19609 = CARTESIAN_POINT ( 'NONE',  ( 0.3996062992125986590, -0.1070741851644053111, -0.7414698162729659314 ) ) ;
#19610 = CARTESIAN_POINT ( 'NONE',  ( -0.3949938075777409408, -0.1058382717557502933, -0.8333333333333334814 ) ) ;
#19611 = CARTESIAN_POINT ( 'NONE',  ( 0.2656293764155540083, 1.144263613740634566, -1.650922135227781418 ) ) ;
#19612 = CARTESIAN_POINT ( 'NONE',  ( 1.082677165354331228, 0.07958543189024071263, -0.2665933059059888421 ) ) ;
#19613 = EDGE_CURVE ( 'NONE', #38994, #33309, #69185, .T. ) ;
#19614 = CARTESIAN_POINT ( 'NONE',  ( 0.2952755905511816326, -0.4536011799217367080, 0.2665933059059888421 ) ) ;
#19615 = CARTESIAN_POINT ( 'NONE',  ( -0.01968503937007793844, -0.5400638737290844871, 0.3530559997133364547 ) ) ;
#19616 = CARTESIAN_POINT ( 'NONE',  ( 1.371391076115485719, -0.6692913385826773087, -0.1292274648535924053 ) ) ;
#19617 = CARTESIAN_POINT ( 'NONE',  ( -0.1058382717557497660, -0.3949938075777411073, -1.251312335958005173 ) ) ;
#19618 = CARTESIAN_POINT ( 'NONE',  ( 0.3871391076115493490, -0.2845877964562159024, 0.3641732283464567677 ) ) ;
#19619 = CARTESIAN_POINT ( 'NONE',  ( -0.5577427821522301654, -0.3162353388693405765, 0.4822834645669290543 ) ) ;
#19620 = CARTESIAN_POINT ( 'NONE',  ( -1.220472440944881054, -0.6692913385826771977, 8.415575281601705876E-17 ) ) ;
#19621 = CARTESIAN_POINT ( 'NONE',  ( 0.8989501312335964611, 0.2952755905511811885, 0.1292274648535926551 ) ) ;
#19622 = CARTESIAN_POINT ( 'NONE',  ( 0.1265901696524989462, 0.4724409448818897572, -1.568241469816272993 ) ) ;
#19623 = CARTESIAN_POINT ( 'NONE',  ( 0.3460692066303959757, -0.1998031496062991907, -2.624671916010498762 ) ) ;
#19624 = AXIS2_PLACEMENT_3D ( 'NONE', #38908, #65007, #64588 ) ;
#19625 = EDGE_LOOP ( 'NONE', ( #35685, #17522 ) ) ;
#19626 = ORIENTED_EDGE ( 'NONE', *, *, #6477, .F. ) ;
#19627 = CARTESIAN_POINT ( 'NONE',  ( -1.371391076115484831, 0.2952755905511810774, -0.1292274648535930714 ) ) ;
#19628 = CARTESIAN_POINT ( 'NONE',  ( -0.4396325459317577122, -0.6692913385826773087, -0.1292274648535924053 ) ) ;
#19630 = CARTESIAN_POINT ( 'NONE',  ( -0.8792650918635160906, -0.4281496062992124485, 0.4176697321401328655 ) ) ;
#19629 = CARTESIAN_POINT ( 'NONE',  ( -0.6824146981627288167, 0.1283753931104748280, 0.1820866141732283561 ) ) ;
#19631 = CARTESIAN_POINT ( 'NONE',  ( 0.1958661417322834497, 0.3392501089628018329, -1.956673597603987957 ) ) ;
#19632 = CARTESIAN_POINT ( 'NONE',  ( 0.2925321140481932369, -0.2925321140481931814, -2.852362204724409711 ) ) ;
#19633 = CARTESIAN_POINT ( 'NONE',  ( -1.646981627296586703, -0.08942795157527998196, 0.3641732283464567121 ) ) ;
#19634 = CARTESIAN_POINT ( 'NONE',  ( -1.364829396325458521, 0.2306618581243847221, -0.2411417322834647770 ) ) ;
#19635 = CARTESIAN_POINT ( 'NONE',  ( 0.2165354330708668673, 0.1660481256975883668, -0.3530559997133364547 ) ) ;
#19636 = CARTESIAN_POINT ( 'NONE',  ( -0.7611548556430438595, -0.6046776061558809534, -0.2411417322834644161 ) ) ;
#19637 = B_SPLINE_CURVE_WITH_KNOTS ( 'NONE', 3,
 ( #56542, #5211, #30875, #53130, #27891, #78841, #40525, #79259, #989, #52715, #21167, #40108, #19919, #78004, #58622, #39263, #53962, #52298, #21574, #32955, #65380, #2226, #65795, #66204, #46823 ),
 .UNSPECIFIED., .F., .F.,
 ( 4, 2, 2, 2, 2, 2, 2, 2, 2, 1, 2, 2, 4 ),
 ( 0.000000000000000000, 0.002357302890897380095, 0.003535954336346069926, 0.004714605781794759323, 0.007071908672692136383, 0.008250560118140825780, 0.009429211563589516912, 0.01178651445448690438, 0.01296516589993559551, 0.01414381734538429011, 0.01532246879083298124, 0.01650112023628167238, 0.01885842312717905811 ),
 .UNSPECIFIED. ) ;
#19638 = EDGE_CURVE ( 'NONE', #78367, #43096, #500, .T. ) ;
#19639 = CARTESIAN_POINT ( 'NONE',  ( 0.1958661417322836440, -0.3392501089628017219, -1.658792650918635259 ) ) ;
#19640 = CARTESIAN_POINT ( 'NONE',  ( -1.010498687664041384, -0.004921259842519576551, 0.3153832671262227771 ) ) ;
#19641 = VERTEX_POINT ( 'NONE', #11847 ) ;
#19642 = CARTESIAN_POINT ( 'NONE',  ( 0.3949938075777409963, 2.418639510665530435E-17, -2.007874015748031482 ) ) ;
#19643 = VERTEX_POINT ( 'NONE', #29944 ) ;
#19644 = DIRECTION ( 'NONE',  ( -0.8050726085550657940, -2.493067783899223597E-16, -0.5931762764594871173 ) ) ;
#19645 = CARTESIAN_POINT ( 'NONE',  ( -1.227034120734907585, 0.2952755905511811885, 0.1292274648535926551 ) ) ;
#19646 = CARTESIAN_POINT ( 'NONE',  ( -0.7086614173228339419, -0.1870078740157479769, 0.4822834645669291653 ) ) ;
#19647 = CARTESIAN_POINT ( 'NONE',  ( 0.3460692066303959202, 0.1998031496062993295, -0.2887139107611548794 ) ) ;
#19648 = CARTESIAN_POINT ( 'NONE',  ( -1.056430446194224881, 0.2952755905511810774, -0.1292274648535930714 ) ) ;
#19649 = CARTESIAN_POINT ( 'NONE',  ( -1.049868766404198794, 0.2306618581243847221, -0.2411417322834647770 ) ) ;
#19650 = CARTESIAN_POINT ( 'NONE',  ( -9.594673741351313045E-17, 0.3917322834645670104, 0.2303149606299211838 ) ) ;
#19651 = CARTESIAN_POINT ( 'NONE',  ( -0.006561679790025524116, -0.08942795157528024563, -0.3641732283464568787 ) ) ;
#19652 = CARTESIAN_POINT ( 'NONE',  ( -0.02282215444009891639, 1.063505409135067525, -1.439960907823146119 ) ) ;
#19653 = CARTESIAN_POINT ( 'NONE',  ( 0.2867679344610365999, 0.2867679344610365999, -0.2224409448818898127 ) ) ;
#19654 = CARTESIAN_POINT ( 'NONE',  ( -0.3477690288713905509, -0.5511811023622046335, 0.09757992244046803654 ) ) ;
#19655 = CARTESIAN_POINT ( 'NONE',  ( -0.7349081364829387342, -0.6046776061558807314, 0.2411417322834647770 ) ) ;
#19656 = CARTESIAN_POINT ( 'NONE',  ( 1.377952755905512472, -0.6692913385826771977, 8.415575281601705876E-17 ) ) ;
#19657 = CARTESIAN_POINT ( 'NONE',  ( -0.5774278215223089816, -0.6046776061558807314, 0.2411417322834647770 ) ) ;
#19658 = VERTEX_POINT ( 'NONE', #37910 ) ;
#19659 = ORIENTED_EDGE ( 'NONE', *, *, #4484, .T. ) ;
#19660 = CARTESIAN_POINT ( 'NONE',  ( 0.3460692066303959202, -0.1998031496062991630, -2.071522309711285814 ) ) ;
#19661 = CARTESIAN_POINT ( 'NONE',  ( -1.141732283464566011, 0.2952755905511811885, 0.000000000000000000 ) ) ;
#19662 = CARTESIAN_POINT ( 'NONE',  ( 1.292650918635171564, 0.2952755905511811885, 0.1292274648535926551 ) ) ;
#19663 = CARTESIAN_POINT ( 'NONE',  ( -1.167979002624671470, -0.3690944881889765550, -0.3153832671262227771 ) ) ;
#19664 = CARTESIAN_POINT ( 'NONE',  ( -1.272965879265091305, -0.4281496062992124485, 0.4176697321401328655 ) ) ;
#19665 = CARTESIAN_POINT ( 'NONE',  ( 0.4724409448818898682, 2.892866454678787531E-17, -0.7480314960629921295 ) ) ;
#19666 = CARTESIAN_POINT ( 'NONE',  ( -0.3307086614173228023, -0.3647102339900947787, 0.000000000000000000 ) ) ;
#19667 = CARTESIAN_POINT ( 'NONE',  ( -0.3917322834645670104, -7.196005306013484475E-17, -0.3464566929133857665 ) ) ;
#19668 = AXIS2_PLACEMENT_3D ( 'NONE', #7793, #66279, #8619 ) ;
#19669 = CARTESIAN_POINT ( 'NONE',  ( 0.1958661417322834775, 0.3392501089628018884, -1.961286089238845287 ) ) ;
#19670 = CARTESIAN_POINT ( 'NONE',  ( -0.05249343832020911260, 0.2306618581243848609, 0.2411417322834645549 ) ) ;
#19671 = CARTESIAN_POINT ( 'NONE',  ( -1.174540682414697335, -0.08942795157527998196, 0.3641732283464567121 ) ) ;
#19672 = AXIS2_PLACEMENT_3D ( 'NONE', #1196, #14243, #60498 ) ;
#19673 = AXIS2_PLACEMENT_3D ( 'NONE', #57179, #82881, #73589 ) ;
#19674 = CARTESIAN_POINT ( 'NONE',  ( -0.5839895013123351797, 0.2952755905511810774, -0.1292274648535930714 ) ) ;
#19675 = CARTESIAN_POINT ( 'NONE',  ( 0.4724409448818898682, 2.892866454678787531E-17, -2.557086614173228689 ) ) ;
#19676 = CARTESIAN_POINT ( 'NONE',  ( -1.161417322834644716, -0.5400638737290845981, -0.3530559997133363437 ) ) ;
#19677 = CARTESIAN_POINT ( 'NONE',  ( -1.036745406824146176, 0.05413385826771626580, -0.4176697321401330321 ) ) ;
#19678 = CARTESIAN_POINT ( 'NONE',  ( -0.1706036745406816491, -0.4281496062992124485, 0.4176697321401328655 ) ) ;
#19679 = CARTESIAN_POINT ( 'NONE',  ( -0.3949938075777408852, -0.1058382717557502933, -2.484908136482939955 ) ) ;
#19680 = CARTESIAN_POINT ( 'NONE',  ( 0.7677165354330716118, -0.4536011799217367080, 0.2665933059059888421 ) ) ;
#19681 =( REPRESENTATION_RELATIONSHIP ('NONE','NONE', #79348, #48103 ) REPRESENTATION_RELATIONSHIP_WITH_TRANSFORMATION ( #31259 )SHAPE_REPRESENTATION_RELATIONSHIP( ) );
#19682 = CARTESIAN_POINT ( 'NONE',  ( -0.8530183727034112984, -0.3690944881889765550, -0.3153832671262227771 ) ) ;
#19683 = CARTESIAN_POINT ( 'NONE',  ( -0.03998971805478993002, 1.064647760289955114, -1.632685650884892370 ) ) ;
#19684 = CARTESIAN_POINT ( 'NONE',  ( 0.6824146981627303710, -0.5023911411419708095, 0.1820866141732285504 ) ) ;
#19685 = CARTESIAN_POINT ( 'NONE',  ( 1.476377952755906220, 0.07958543189024071263, -0.2665933059059888421 ) ) ;
#19686 = CARTESIAN_POINT ( 'NONE',  ( 1.391076115485564868, -0.6046776061558807314, 0.2411417322834647770 ) ) ;
#19687 = CARTESIAN_POINT ( 'NONE',  ( -0.08530183727034056085, -0.2845877964562159024, 0.3641732283464567677 ) ) ;
#19688 = CARTESIAN_POINT ( 'NONE',  ( 0.1049643490035304938, -0.3917322834645669549, -1.337270341207349000 ) ) ;
#19689 = CARTESIAN_POINT ( 'NONE',  ( -0.6758530183727028406, 0.2952755905511811885, 0.1292274648535926551 ) ) ;
#19690 = CARTESIAN_POINT ( 'NONE',  ( 1.423884514435696191, -0.05778040916215522460, 0.4822834645669289988 ) ) ;
#19691 = AXIS2_PLACEMENT_3D ( 'NONE', #73943, #28479, #41527 ) ;
#19692 = CARTESIAN_POINT ( 'NONE',  ( -0.3458507752293909498, 0.3458507752293907833, -0.09645669291338582196 ) ) ;
#19693 = CARTESIAN_POINT ( 'NONE',  ( -0.3871391076115476282, -0.08942795157527998196, 0.3641732283464567121 ) ) ;
#19694 = CARTESIAN_POINT ( 'NONE',  ( -0.4068241469816267775, 0.05413385826771626580, -0.4176697321401330321 ) ) ;
#19695 = CARTESIAN_POINT ( 'NONE',  ( 0.5314960629921267055, -0.5400638737290844871, 0.3530559997133364547 ) ) ;
#19696 = CARTESIAN_POINT ( 'NONE',  ( 0.4724409448818898682, 2.892866454678787531E-17, -0.6673228346456693272 ) ) ;
#19697 = CARTESIAN_POINT ( 'NONE',  ( 0.7874015748031503170, -0.1870078740157479769, 0.3641732283464567677 ) ) ;
#19698 = CARTESIAN_POINT ( 'NONE',  ( -0.01312335958005186876, -0.3690944881889763329, 0.3153832671262228327 ) ) ;
#19699 = CARTESIAN_POINT ( 'NONE',  ( -0.5052493438320203589, 0.2952755905511810774, -0.1292274648535930714 ) ) ;
#19700 = CARTESIAN_POINT ( 'NONE',  ( -1.437007874015747477, -0.5400638737290844871, 0.3530559997133364547 ) ) ;
#19701 = CARTESIAN_POINT ( 'NONE',  ( -0.5314960629921250401, 0.07958543189024085140, 0.2665933059059887866 ) ) ;
#19702 = PLANE ( 'NONE',  #20663 ) ;
#19703 = CARTESIAN_POINT ( 'NONE',  ( -1.023622047244093558, -0.1870078740157479769, 0.4822834645669291653 ) ) ;
#19704 = CARTESIAN_POINT ( 'NONE',  ( -0.1070741851644051862, -0.3996062992125986590, -0.9363517060367454459 ) ) ;
#19705 = CARTESIAN_POINT ( 'NONE',  ( -0.3917322834645669549, -0.1049643490035306603, -2.650262467191601079 ) ) ;
#19706 = CARTESIAN_POINT ( 'NONE',  ( 0.02624671916010564918, 0.1283753931104748280, 0.1820866141732283561 ) ) ;
#19707 = CARTESIAN_POINT ( 'NONE',  ( -0.6627296587926501115, 0.2952755905511810774, -0.1292274648535930714 ) ) ;
#19708 = CARTESIAN_POINT ( 'NONE',  ( -1.233595800524933894, -0.6046776061558809534, -0.2411417322834644161 ) ) ;
#19709 = CARTESIAN_POINT ( 'NONE',  ( -1.410761154855641575, -0.2845877964562161244, -0.3641732283464567121 ) ) ;
#19710 = CARTESIAN_POINT ( 'NONE',  ( -3.913926014577544521, 1.327547550174811741, -0.4257567319240657122 ) ) ;
#19711 = CARTESIAN_POINT ( 'NONE',  ( -0.8333333333333323711, 0.1771653543307087630, 0.09757992244046791164 ) ) ;
#19712 = CARTESIAN_POINT ( 'NONE',  ( -1.732283464566928277, -0.1870078740157479769, 0.3641732283464567677 ) ) ;
#19713 = CARTESIAN_POINT ( 'NONE',  ( 1.338582677165355062, -0.1870078740157480879, -0.4822834645669291653 ) ) ;
#19714 = CARTESIAN_POINT ( 'NONE',  ( -0.3996062992125986035, -0.1070741851644056997, 0.1115485564304461580 ) ) ;
#19715 = CARTESIAN_POINT ( 'NONE',  ( 0.2867679344610366554, 0.2867679344610366554, -2.024297531004936701 ) ) ;
#19716 = ORIENTED_EDGE ( 'NONE', *, *, #44509, .T. ) ;
#19717 = LINE ( 'NONE', #63505, #75424 ) ;
#19718 = EDGE_CURVE ( 'NONE', #5025, #18348, #69085, .T. ) ;
#19719 = CARTESIAN_POINT ( 'NONE',  ( 1.528871391076116026, -0.5511811023622048555, -0.09757992244046775898 ) ) ;
#19720 = CARTESIAN_POINT ( 'NONE',  ( -1.325459317585300889, -0.4281496062992127816, -0.4176697321401328100 ) ) ;
#19721 = CARTESIAN_POINT ( 'NONE',  ( 1.410761154855643795, -0.3162353388693405765, 0.4822834645669290543 ) ) ;
#19722 = CARTESIAN_POINT ( 'NONE',  ( 0.3917322834645670104, 2.398668435337828261E-17, -1.777559055118110409 ) ) ;
#19723 = CARTESIAN_POINT ( 'NONE',  ( 1.535433070866142558, 0.1771653543307087630, 0.000000000000000000 ) ) ;
#19724 = ADVANCED_FACE ( 'NONE', ( #11433 ), #11015, .F. ) ;
#19725 = CARTESIAN_POINT ( 'NONE',  ( 0.7086614173228353852, -0.1870078740157479769, 0.4822834645669291653 ) ) ;
#19726 = CARTESIAN_POINT ( 'NONE',  ( -0.1443569553805765515, -0.4281496062992127816, -0.4176697321401328100 ) ) ;
#19727 = DIRECTION ( 'NONE',  ( -1.000000000000000000, -3.050063254464715781E-16, 0.000000000000000000 ) ) ;
#19728 = CIRCLE ( 'NONE', #65415, 0.2952755905511810774 ) ;
#19730 = DIRECTION ( 'NONE',  ( 0.000000000000000000, 0.000000000000000000, -1.000000000000000000 ) ) ;
#19729 = AXIS2_PLACEMENT_3D ( 'NONE', #30080, #15829, #9905 ) ;
#19731 = CARTESIAN_POINT ( 'NONE',  ( 0.6627296587926515548, 0.1771653543307087630, 0.09757992244046791164 ) ) ;
#19732 = CARTESIAN_POINT ( 'NONE',  ( -0.1070741851644051862, -0.3996062992125987146, -1.174540682414698001 ) ) ;
#19733 = ORIENTED_EDGE ( 'NONE', *, *, #18308, .T. ) ;
#19734 = CARTESIAN_POINT ( 'NONE',  ( 0.2867679344610365999, -0.2867679344610365444, -2.925196850393700920 ) ) ;
#19735 = ORIENTED_EDGE ( 'NONE', *, *, #20396, .F. ) ;
#19736 = CARTESIAN_POINT ( 'NONE',  ( -0.1377952755905504645, 0.1660481256975885056, 0.3530559997133364547 ) ) ;
#19737 = PRODUCT_DEFINITION_SHAPE ( 'NONE', 'NONE',  #83323 ) ;
#19738 = CARTESIAN_POINT ( 'NONE',  ( -1.450131233595799651, 0.2952755905511810774, -0.1292274648535930714 ) ) ;
#19739 = CARTESIAN_POINT ( 'NONE',  ( 0.4527559055118117182, 0.1660481256975883668, -0.3530559997133364547 ) ) ;
#19740 = CARTESIAN_POINT ( 'NONE',  ( 1.135170603674541256, -0.6692913385826773087, -0.1292274648535924053 ) ) ;
#19741 = CARTESIAN_POINT ( 'NONE',  ( 1.482939632545932307, 0.05413385826771626580, -0.4176697321401330321 ) ) ;
#19742 = CARTESIAN_POINT ( 'NONE',  ( -0.4527559055118102749, -0.5400638737290845981, -0.3530559997133363437 ) ) ;
#19743 = CARTESIAN_POINT ( 'NONE',  ( -0.1312335958005241554, 0.2306618581243848609, 0.2411417322834645549 ) ) ;
#19744 = CARTESIAN_POINT ( 'NONE',  ( 1.502624671916010790, -0.3162353388693409650, -0.4822834645669289433 ) ) ;
#19745 = CARTESIAN_POINT ( 'NONE',  ( 1.345144356955381593, -0.3162353388693409650, -0.4822834645669289433 ) ) ;
#19746 = CARTESIAN_POINT ( 'NONE',  ( 1.056430446194226658, 0.2952755905511811885, 0.1292274648535926551 ) ) ;
#19747 = CARTESIAN_POINT ( 'NONE',  ( -0.07874015748031421014, -0.1870078740157480879, -0.4822834645669291653 ) ) ;
#19748 = ADVANCED_FACE ( 'NONE', ( #76232 ), #57160, .T. ) ;
#19749 = CARTESIAN_POINT ( 'NONE',  ( -0.3917322834645669549, -0.1049643490035306603, -0.3530183727034120755 ) ) ;
#19750 = CARTESIAN_POINT ( 'NONE',  ( 0.5446194225721792126, -0.2845877964562159024, 0.3641732283464567677 ) ) ;
#19751 = ORIENTED_EDGE ( 'NONE', *, *, #7379, .T. ) ;
#19752 = CARTESIAN_POINT ( 'NONE',  ( 0.1974969037888706369, -0.3420746716998659953, -0.7217847769028871152 ) ) ;
#19753 = ORIENTED_EDGE ( 'NONE', *, *, #48374, .T. ) ;
#19754 = CARTESIAN_POINT ( 'NONE',  ( -0.2493438320209966919, -0.004921259842519870586, -0.3153832671262229437 ) ) ;
#19755 = CARTESIAN_POINT ( 'NONE',  ( 2.704370107879210838, 1.253873987468413498, -0.3814095263789911150 ) ) ;
#19756 = CARTESIAN_POINT ( 'NONE',  ( 0.08530183727034192087, -0.3162353388693409650, -0.4822834645669289433 ) ) ;
#19757 = CARTESIAN_POINT ( 'NONE',  ( -0.05249343832020938322, -0.6046776061558809534, -0.2411417322834644161 ) ) ;
#19758 = EDGE_CURVE ( 'NONE', #15966, #33945, #43792, .T. ) ;
#19759 = CARTESIAN_POINT ( 'NONE',  ( -0.9776902887139098386, -0.6692913385826771977, 0.1292274648535927661 ) ) ;
#19760 = CARTESIAN_POINT ( 'NONE',  ( -0.1958661417322833942, -0.3392501089628018884, -1.479678108432757933 ) ) ;
#19761 = CARTESIAN_POINT ( 'NONE',  ( -1.587926509186350810, 0.05413385826771626580, -0.4176697321401330321 ) ) ;
#19762 = CARTESIAN_POINT ( 'NONE',  ( -1.595398199321656385, 1.564277624879635509, -0.1559797534342483583 ) ) ;
#19763 = CARTESIAN_POINT ( 'NONE',  ( 0.8136482939632553313, 0.1283753931104748280, 0.1820866141732283561 ) ) ;
#19764 = CARTESIAN_POINT ( 'NONE',  ( 0.4396325459317593221, 0.2952755905511810774, -0.1292274648535930714 ) ) ;
#19765 = CARTESIAN_POINT ( 'NONE',  ( 0.8595800524934390507, -0.3162353388693405765, 0.4822834645669290543 ) ) ;
#19766 = CARTESIAN_POINT ( 'NONE',  ( -0.2925321140481932924, 0.2925321140481931814, -1.122047244094488194 ) ) ;
#19767 = CARTESIAN_POINT ( 'NONE',  ( -1.660104986876639543, -0.05778040916215560624, -0.4822834645669293319 ) ) ;
#19768 = CARTESIAN_POINT ( 'NONE',  ( 0.1998031496062994128, -0.3460692066303957537, -0.7985564304461942875 ) ) ;
#19769 = CARTESIAN_POINT ( 'NONE',  ( 0.3996062992125984925, 0.1070741851644054637, -0.04396325459317587669 ) ) ;
#19770 = CARTESIAN_POINT ( 'NONE',  ( 0.01968503937007930540, 0.1660481256975885056, 0.3530559997133364547 ) ) ;
#19771 = CARTESIAN_POINT ( 'NONE',  ( 0.1070741851644054915, -0.3996062992125986035, -2.762467191601049255 ) ) ;
#19772 = CARTESIAN_POINT ( 'NONE',  ( 0.3917322834645670104, -0.1049643490035303411, -1.928477690288713742 ) ) ;
#19773 = CARTESIAN_POINT ( 'NONE',  ( -1.397637795275589623, -0.4536011799217368745, -0.2665933059059886201 ) ) ;
#19774 = CARTESIAN_POINT ( 'NONE',  ( 1.174540682414699111, -0.05778040916215560624, -0.4822834645669293319 ) ) ;
#19775 = CARTESIAN_POINT ( 'NONE',  ( 1.502624671916010790, -0.05778040916215522460, 0.4822834645669289988 ) ) ;
#19776 = CARTESIAN_POINT ( 'NONE',  ( 0.2887139107611556010, 0.1283753931104746893, -0.1820866141732285504 ) ) ;
#19777 = CARTESIAN_POINT ( 'NONE',  ( 0.3740157480314966754, 0.1660481256975883668, -0.3530559997133364547 ) ) ;
#19778 = CARTESIAN_POINT ( 'NONE',  ( 0.2362204724409449064, 0.4091458600556404646, -1.323490813648294129 ) ) ;
#19779 = CARTESIAN_POINT ( 'NONE',  ( 0.4790026246719168435, -0.2845877964562161244, -0.3641732283464567121 ) ) ;
#19780 =( BOUNDED_CURVE ( )  B_SPLINE_CURVE ( 2, ( #42983, #68678, #3053, #16526, #61537, #35039, #28719, #54382, #36676, #48069, #74597, #16940, #80505 ),
 .UNSPECIFIED., .F., .F. ) 
 B_SPLINE_CURVE_WITH_KNOTS ( ( 3, 2, 2, 2, 2, 2, 3 ),
 ( 0.1625000000000000056, 0.1666666666666666574, 0.1708333333333333370, 0.1749999999999999889, 0.1791666666666666685, 0.1833333333333333204, 0.1875000000000000000 ),
 .UNSPECIFIED. ) 
 CURVE ( )  GEOMETRIC_REPRESENTATION_ITEM ( )  RATIONAL_B_SPLINE_CURVE ( ( 1.000000000000000000, 0.9659258262890683122, 1.000000000000000000, 0.9659258262890683122, 1.000000000000000000, 0.9659258262890683122, 1.000000000000000000, 0.9659258262890683122, 1.000000000000000000, 0.9659258262890683122, 1.000000000000000000, 0.9659258262890683122, 1.000000000000000000 ) ) 
 REPRESENTATION_ITEM ( '' )  );
#19781 = CARTESIAN_POINT ( 'NONE',  ( -0.02624671916010428221, -0.6046776061558807314, 0.2411417322834647770 ) ) ;
#19782 = CARTESIAN_POINT ( 'NONE',  ( -0.2891555358219909388, -0.2891555358219912164, -1.395669291338582418 ) ) ;
#19783 = CARTESIAN_POINT ( 'NONE',  ( -1.391076115485563758, 0.2306618581243848609, 0.2411417322834645549 ) ) ;
#19784 = CARTESIAN_POINT ( 'NONE',  ( 0.5905511811023629321, -0.5511811023622047445, 6.969142054262312111E-17 ) ) ;
#19785 = ADVANCED_FACE ( 'NONE', ( #62348 ), #76635, .F. ) ;
#19786 = LINE ( 'NONE', #858, #74909 ) ;
#19787 = CARTESIAN_POINT ( 'NONE',  ( -0.5577427821522301654, -0.05778040916215560624, -0.4822834645669293319 ) ) ;
#19788 = CARTESIAN_POINT ( 'NONE',  ( -0.3346456692913377662, 0.07958543189024071263, -0.2665933059059888421 ) ) ;
#19789 = DIRECTION ( 'NONE',  ( 0.000000000000000000, 0.000000000000000000, 1.000000000000000000 ) ) ;
#19790 = CARTESIAN_POINT ( 'NONE',  ( -0.7611548556430438595, 0.2306618581243848609, 0.2411417322834645549 ) ) ;
#19791 = CARTESIAN_POINT ( 'NONE',  ( -0.1640419947506553400, -0.05778040916215560624, -0.4822834645669293319 ) ) ;
#19792 = CARTESIAN_POINT ( 'NONE',  ( 0.1968503937007881344, 0.1771653543307087630, 0.000000000000000000 ) ) ;
#19793 = AXIS2_PLACEMENT_3D ( 'NONE', #68704, #69529, #5546 ) ;
#19794 = CARTESIAN_POINT ( 'NONE',  ( -0.2925321140481932369, 0.2925321140481931259, -2.301181102362204633 ) ) ;
#19795 = CARTESIAN_POINT ( 'NONE',  ( 8.195543980992789655E-16, -0.1870078740157480879, -0.4822834645669291653 ) ) ;
#19796 = VECTOR ( 'NONE', #79265, 39.37007874015748143 ) ;
#19798 = CARTESIAN_POINT ( 'NONE',  ( -0.2867679344610366554, 0.2867679344610365444, -2.146962311514748478 ) ) ;
#19797 = AXIS2_PLACEMENT_3D ( 'NONE', #23157, #16873, #61876 ) ;
#19799 = CARTESIAN_POINT ( 'NONE',  ( 0.9055118110236227702, 0.1771653543307087630, 0.000000000000000000 ) ) ;
#19800 = CARTESIAN_POINT ( 'NONE',  ( 1.279527559055118724, 0.1660481256975885056, 0.3530559997133364547 ) ) ;
#19801 = CARTESIAN_POINT ( 'NONE',  ( -0.6299212598425188991, -0.1870078740157479769, 0.3641732283464567677 ) ) ;
#19802 = CARTESIAN_POINT ( 'NONE',  ( -1.318897637795274802, -0.4536011799217368745, -0.2665933059059886201 ) ) ;
#19803 = CARTESIAN_POINT ( 'NONE',  ( -0.7020997375328074108, -0.05778040916215522460, 0.4822834645669289988 ) ) ;
#19804 = CARTESIAN_POINT ( 'NONE',  ( -0.02624671916010428221, -0.6046776061558807314, 0.2411417322834647770 ) ) ;
#19805 = CARTESIAN_POINT ( 'NONE',  ( 0.6364829396325465405, -0.2845877964562161244, -0.3641732283464567121 ) ) ;
#19806 = CARTESIAN_POINT ( 'NONE',  ( -0.2362204724409451284, 0.4091458600556402425, -2.375328083989501238 ) ) ;
#19807 = CARTESIAN_POINT ( 'NONE',  ( 1.030183727034121421, -0.2845877964562161244, -0.3641732283464567121 ) ) ;
#19808 = EDGE_CURVE ( 'NONE', #33309, #68837, #66219, .T. ) ;
#19809 = CARTESIAN_POINT ( 'NONE',  ( 0.1312335958005257930, 0.2306618581243847221, -0.2411417322834647770 ) ) ;
#19810 = CARTESIAN_POINT ( 'NONE',  ( -0.3996062992125986590, 0.1070741851644051723, 0.04790026246719158304 ) ) ;
#19811 = CARTESIAN_POINT ( 'NONE',  ( -0.3346456692913377662, -0.5400638737290844871, 0.3530559997133364547 ) ) ;
#19812 = CARTESIAN_POINT ( 'NONE',  ( -0.1958661417322834220, -0.3392501089628018884, -1.410104986876640654 ) ) ;
#19813 = CARTESIAN_POINT ( 'NONE',  ( 1.581364829396326277, -0.08942795157527998196, 0.3641732283464567121 ) ) ;
#19814 = CARTESIAN_POINT ( 'NONE',  ( 0.2755905511811031494, 0.2952755905511811885, 0.000000000000000000 ) ) ;
#19815 = CARTESIAN_POINT ( 'NONE',  ( 0.2887139107611556010, 0.2306618581243847221, -0.2411417322834647770 ) ) ;
#19816 = CARTESIAN_POINT ( 'NONE',  ( 0.5905511811023628210, 0.2066929133858268208, 0.000000000000000000 ) ) ;
#19817 = CARTESIAN_POINT ( 'NONE',  ( -0.09186351706036663400, -0.3690944881889763329, 0.3153832671262228327 ) ) ;
#19818 = CARTESIAN_POINT ( 'NONE',  ( 0.6364829396325465405, -0.3162353388693409650, -0.4822834645669289433 ) ) ;
#19819 = CARTESIAN_POINT ( 'NONE',  ( -0.5249343832020990641, -0.5023911411419708095, -0.1820866141732282451 ) ) ;
#19820 = CARTESIAN_POINT ( 'NONE',  ( -0.7283464566929126471, -0.5400638737290844871, 0.3530559997133364547 ) ) ;
#19821 = LINE ( 'NONE', #45047, #44729 ) ;
#19822 = CARTESIAN_POINT ( 'NONE',  ( 0.02624671916010564918, 0.2306618581243848609, 0.2411417322834645549 ) ) ;
#19823 = CARTESIAN_POINT ( 'NONE',  ( -1.122047244094487306, 0.1660481256975883668, -0.3530559997133364547 ) ) ;
#19824 = CARTESIAN_POINT ( 'NONE',  ( -0.8989501312335946848, 0.1771653543307087075, -0.09757992244046823083 ) ) ;
#19825 = CARTESIAN_POINT ( 'NONE',  ( 0.3346456692913390985, 0.1660481256975885056, 0.3530559997133364547 ) ) ;
#19826 = CARTESIAN_POINT ( 'NONE',  ( -1.200787401574802349, 0.1660481256975883668, -0.3530559997133364547 ) ) ;
#19827 = CARTESIAN_POINT ( 'NONE',  ( -0.2887139107611542133, -0.6046776061558809534, -0.2411417322834644161 ) ) ;
#19828 = EDGE_CURVE ( 'NONE', #64046, #79730, #21048, .T. ) ;
#19829 = CARTESIAN_POINT ( 'NONE',  ( 1.141392835773559211, 0.3937007874015747699, 1.141392835773562764 ) ) ;
#19831 = CARTESIAN_POINT ( 'NONE',  ( 1.496062992125984703, -0.1870078740157480879, -0.4822834645669291653 ) ) ;
#19830 = CARTESIAN_POINT ( 'NONE',  ( -0.9055118110236215490, 0.2952755905511811885, 0.000000000000000000 ) ) ;
#19832 = CARTESIAN_POINT ( 'NONE',  ( 1.463254593175853824, -0.6692913385826771977, 0.1292274648535927661 ) ) ;
#19833 = CARTESIAN_POINT ( 'NONE',  ( -0.1049643490035301885, -0.3917322834645671215, -2.269028871391076230 ) ) ;
#19834 = CARTESIAN_POINT ( 'NONE',  ( -0.4359958488159583201, 1.724409448818897905, -3.912791665790201101 ) ) ;
#19835 = CARTESIAN_POINT ( 'NONE',  ( -1.397637795275589623, 0.1660481256975885056, 0.3530559997133364547 ) ) ;
#19836 = CARTESIAN_POINT ( 'NONE',  ( 0.4091458600556403535, 0.2362204724409449896, -0.9186351706036745002 ) ) ;
#19837 = CARTESIAN_POINT ( 'NONE',  ( -9.787531504996567848E-17, 0.3996062992125986035, -1.920830620545185230E-17 ) ) ;
#19838 = VERTEX_POINT ( 'NONE', #71157 ) ;
#19839 = CARTESIAN_POINT ( 'NONE',  ( -0.1443569553805765515, -0.3690944881889765550, -0.3153832671262227771 ) ) ;
#19840 = CARTESIAN_POINT ( 'NONE',  ( -0.3917322834645670104, -7.196005306013484475E-17, -1.763779527559055094 ) ) ;
#19841 = ORIENTED_EDGE ( 'NONE', *, *, #65161, .T. ) ;
#19842 = CARTESIAN_POINT ( 'NONE',  ( 0.4330708661417329575, -0.6692913385826771977, 8.415575281601705876E-17 ) ) ;
#19843 = CARTESIAN_POINT ( 'NONE',  ( 0.4724409448818904789, -0.1870078740157479769, 0.4822834645669291653 ) ) ;
#19844 = CARTESIAN_POINT ( 'NONE',  ( -0.3458507752293906723, -0.3458507752293910609, -2.893700787401574992 ) ) ;
#19845 = CARTESIAN_POINT ( 'NONE',  ( -0.5396849562100385356, -4.992347309556208597E-15, 0.3791483426435189319 ) ) ;
#19846 = CARTESIAN_POINT ( 'NONE',  ( -0.3346456692913377662, 0.07958543189024071263, -0.2665933059059888421 ) ) ;
#19847 = CARTESIAN_POINT ( 'NONE',  ( 0.4965823425844641537, 1.491030243332470917, -0.5309055118110237448 ) ) ;
#19848 = CARTESIAN_POINT ( 'NONE',  ( 0.7217847769028878924, 0.05413385826771666132, 0.4176697321401328100 ) ) ;
#19849 = CARTESIAN_POINT ( 'NONE',  ( 0.9317585301837276734, -0.3690944881889763329, 0.3153832671262228327 ) ) ;
#19850 = CARTESIAN_POINT ( 'NONE',  ( -0.2362204724409440182, -0.1870078740157479769, 0.4822834645669291653 ) ) ;
#19851 = CARTESIAN_POINT ( 'NONE',  ( 0.2867679344610365999, -0.2867679344610365999, -1.280820579231284340 ) ) ;
#19852 = CARTESIAN_POINT ( 'NONE',  ( -0.8858267716535425107, -0.5400638737290844871, 0.3530559997133364547 ) ) ;
#19853 = CARTESIAN_POINT ( 'NONE',  ( -1.482939632545930975, -0.3690944881889765550, -0.3153832671262227771 ) ) ;
#19854 = CARTESIAN_POINT ( 'NONE',  ( -0.8333333333333323711, -0.6692913385826773087, -0.1292274648535924053 ) ) ;
#19855 = CARTESIAN_POINT ( 'NONE',  ( 1.384514435695538559, 0.2952755905511810774, -0.1292274648535930714 ) ) ;
#19856 = CARTESIAN_POINT ( 'NONE',  ( 1.679790026246720025, 0.1283753931104748280, 0.1820866141732283561 ) ) ;
#19857 = ORIENTED_EDGE ( 'NONE', *, *, #21817, .T. ) ;
#19858 = CARTESIAN_POINT ( 'NONE',  ( 0.1049643490035304799, -0.3917322834645670104, -2.286764722605985956 ) ) ;
#19859 = CARTESIAN_POINT ( 'NONE',  ( -0.07874015748031421014, -0.1870078740157479769, 0.4822834645669291653 ) ) ;
#19860 = VERTEX_POINT ( 'NONE', #64838 ) ;
#19861 = AXIS2_PLACEMENT_3D ( 'NONE', #37915, #69090, #56441 ) ;
#19862 = CARTESIAN_POINT ( 'NONE',  ( -0.6299212598425188991, -0.1870078740157479769, 0.4822834645669291653 ) ) ;
#19863 = CARTESIAN_POINT ( 'NONE',  ( 1.253280839895013710, -0.3162353388693405765, 0.4822834645669290543 ) ) ;
#19864 = CARTESIAN_POINT ( 'NONE',  ( 1.437007874015748810, 0.1660481256975885056, 0.3530559997133364547 ) ) ;
#19865 = CARTESIAN_POINT ( 'NONE',  ( 0.2296587926509192634, -0.05778040916215560624, -0.4822834645669293319 ) ) ;
#19866 = CARTESIAN_POINT ( 'NONE',  ( -0.01968503937007793844, 0.1660481256975883668, -0.3530559997133364547 ) ) ;
#19867 = CARTESIAN_POINT ( 'NONE',  ( 0.3917322834645670104, 2.398668435337828261E-17, -1.620078740157480324 ) ) ;
#19868 = CARTESIAN_POINT ( 'NONE',  ( -1.108923884514435132, -0.3162353388693405765, 0.4822834645669290543 ) ) ;
#19869 = CARTESIAN_POINT ( 'NONE',  ( -0.3805774278215216522, 0.05413385826771666132, 0.4176697321401328100 ) ) ;
#19870 = CARTESIAN_POINT ( 'NONE',  ( -0.02624671916010428221, 0.1283753931104746893, -0.1820866141732285504 ) ) ;
#19871 = FACE_OUTER_BOUND ( 'NONE', #52135, .T. ) ;
#19872 = CARTESIAN_POINT ( 'NONE',  ( 1.312335958005250269, -0.6046776061558807314, 0.2411417322834647770 ) ) ;
#19873 = CARTESIAN_POINT ( 'NONE',  ( -0.5511811023622041894, -0.1870078740157480879, -0.4822834645669291653 ) ) ;
#19874 = CARTESIAN_POINT ( 'NONE',  ( 0.2821522309711291809, 0.2066929133858267098, -0.1054918080437494132 ) ) ;
#19875 = CARTESIAN_POINT ( 'NONE',  ( 1.062992125984252745, -0.6692913385826771977, 8.415575281601705876E-17 ) ) ;
#19876 = CARTESIAN_POINT ( 'NONE',  ( 1.348312163386739426, 0.2755905511811023723, 0.7386866130305692613 ) ) ;
#19877 = ORIENTED_EDGE ( 'NONE', *, *, #47629, .F. ) ;
#19878 = VERTEX_POINT ( 'NONE', #32425 ) ;
#19879 = CARTESIAN_POINT ( 'NONE',  ( 0.2362204724409456558, -0.1870078740157479769, 0.4822834645669291653 ) ) ;
#19880 = CARTESIAN_POINT ( 'NONE',  ( -0.5052493438320203589, -0.5511811023622046335, 0.09757992244046803654 ) ) ;
#19882 = CARTESIAN_POINT ( 'NONE',  ( -0.2362204724409447953, -0.4091458600556404646, -0.3805774278215223183 ) ) ;
#19881 = CARTESIAN_POINT ( 'NONE',  ( 1.587926509186352586, -0.3690944881889765550, -0.3153832671262227771 ) ) ;
#19883 = CARTESIAN_POINT ( 'NONE',  ( -0.4091458600556405756, 0.2362204724409446288, -0.2604986876640419946 ) ) ;
#19884 = DIRECTION ( 'NONE',  ( 1.000000000000000000, 0.000000000000000000, 0.000000000000000000 ) ) ;
#19885 = ADVANCED_FACE ( 'NONE', ( #7606 ), #65695, .F. ) ;
#19886 = CARTESIAN_POINT ( 'NONE',  ( 1.200787401574803681, -0.5400638737290845981, -0.3530559997133363437 ) ) ;
#19887 = CARTESIAN_POINT ( 'NONE',  ( 0.2891555358219910499, -0.2891555358219909944, -0.3326771653543307283 ) ) ;
#19888 = CARTESIAN_POINT ( 'NONE',  ( 0.03280839895013198948, 0.2952755905511811885, 0.1292274648535926551 ) ) ;
#19889 = CARTESIAN_POINT ( 'NONE',  ( -1.306827173596998737, 0.000000000000000000, 0.4445507791589060065 ) ) ;
#19890 = CARTESIAN_POINT ( 'NONE',  ( -1.614173228346456268, -0.6692913385826771977, 8.415575281601705876E-17 ) ) ;
#19891 = CARTESIAN_POINT ( 'NONE',  ( -0.3215223097112853146, -0.3162353388693405765, 0.4822834645669290543 ) ) ;
#19892 = ADVANCED_FACE ( 'NONE', ( #64418 ), #48907, .T. ) ;
#19893 = CARTESIAN_POINT ( 'NONE',  ( -0.1974969037888706924, 0.3420746716998658843, -0.08989501312335958227 ) ) ;
#19894 = CARTESIAN_POINT ( 'NONE',  ( -1.574803149606298192, -0.1870078740157480601, -0.3641732283464567677 ) ) ;
#19895 = CARTESIAN_POINT ( 'NONE',  ( 0.3412073490813655186, 0.2306618581243848609, 0.2411417322834645549 ) ) ;
#19896 = CARTESIAN_POINT ( 'NONE',  ( 0.9383202099737538715, -0.08942795157528024563, -0.3641732283464568787 ) ) ;
#19897 = CARTESIAN_POINT ( 'NONE',  ( -0.03937007874015669567, 0.2952755905511811885, 0.000000000000000000 ) ) ;
#19898 = CARTESIAN_POINT ( 'NONE',  ( 0.6430446194225729606, -0.3690944881889765550, -0.3153832671262227771 ) ) ;
#19899 = CARTESIAN_POINT ( 'NONE',  ( -1.259842519685038686, -0.1870078740157480879, -0.4822834645669291653 ) ) ;
#19900 = CARTESIAN_POINT ( 'NONE',  ( -0.2925321140481932369, 0.2925321140481931259, -0.8838582677165351953 ) ) ;
#19901 = CARTESIAN_POINT ( 'NONE',  ( 1.148293963254593875, -0.6692913385826771977, 0.1292274648535927661 ) ) ;
#19902 = CARTESIAN_POINT ( 'NONE',  ( 0.3917322834645670104, -0.1049643490035303411, -0.7335958005249343383 ) ) ;
#19903 = CARTESIAN_POINT ( 'NONE',  ( 0.8792650918635177559, 0.05413385826771666132, 0.4176697321401328100 ) ) ;
#19904 = CARTESIAN_POINT ( 'NONE',  ( -0.3492006680983059108, 0.3045572308828553565, -0.01849200668098333403 ) ) ;
#19905 = CARTESIAN_POINT ( 'NONE',  ( 0.4790026246719167324, -0.08942795157527998196, 0.3641732283464567121 ) ) ;
#19906 = CARTESIAN_POINT ( 'NONE',  ( 0.7020997375328090762, -0.3162353388693405765, 0.4822834645669290543 ) ) ;
#19907 = CARTESIAN_POINT ( 'NONE',  ( -0.4562095852119795736, 1.668416680336018976, 2.129998074986525047 ) ) ;
#19908 = CARTESIAN_POINT ( 'NONE',  ( -0.9448818897637790704, -0.1870078740157479769, 0.3641732283464567677 ) ) ;
#19909 = CARTESIAN_POINT ( 'NONE',  ( -1.161417322834644716, -0.5400638737290845981, -0.3530559997133363437 ) ) ;
#19910 = CARTESIAN_POINT ( 'NONE',  ( 1.220472440944882608, 0.2952755905511811885, 0.000000000000000000 ) ) ;
#19911 = CARTESIAN_POINT ( 'NONE',  ( -0.9711286089238838626, -0.6046776061558807314, 0.2411417322834647770 ) ) ;
#19912 = CARTESIAN_POINT ( 'NONE',  ( 0.7480314960629927956, 0.2952755905511811885, 0.000000000000000000 ) ) ;
#19913 = CARTESIAN_POINT ( 'NONE',  ( -1.299212598425196097, 0.1771653543307087630, 0.000000000000000000 ) ) ;
#19914 =( BOUNDED_CURVE ( )  B_SPLINE_CURVE ( 2, ( #21653, #59121, #46065, #34289, #34709, #79333, #72591, #21242, #52796, #14112, #33869, #78506, #8204 ),
 .UNSPECIFIED., .F., .F. ) 
 B_SPLINE_CURVE_WITH_KNOTS ( ( 3, 2, 2, 2, 2, 2, 3 ),
 ( 0.3672150842069599186, 0.3674242424242424310, 0.3712121212121212155, 0.3750000000000000000, 0.3787878787878787845, 0.3825757575757575690, 0.3827849157930400814 ),
 .UNSPECIFIED. ) 
 CURVE ( )  GEOMETRIC_REPRESENTATION_ITEM ( )  RATIONAL_B_SPLINE_CURVE ( ( 0.9964447847208419695, 0.9981185001348091834, 1.000000000000000000, 0.9659258262890683122, 1.000000000000000000, 0.9659258262890683122, 1.000000000000000000, 0.9659258262890683122, 1.000000000000000000, 0.9659258262890683122, 1.000000000000000000, 0.9981185001348091834, 0.9964447847208420805 ) ) 
 REPRESENTATION_ITEM ( '' )  );
#19915 = CARTESIAN_POINT ( 'NONE',  ( -0.3948371832379763968, -0.006307039255732561391, -1.220472440944884163 ) ) ;
#19916 = CARTESIAN_POINT ( 'NONE',  ( 1.122047244094488860, 0.1660481256975885056, 0.3530559997133364547 ) ) ;
#19917 = VECTOR ( 'NONE', #74179, 39.37007874015748143 ) ;
#19918 = CARTESIAN_POINT ( 'NONE',  ( 5.785732909357575061E-17, -0.4724409448818898682, -2.517716535433071279 ) ) ;
#19919 = CARTESIAN_POINT ( 'NONE',  ( 0.3462686196234177061, 1.212745639448218116, 3.921766127980873762 ) ) ;
#19920 = CARTESIAN_POINT ( 'NONE',  ( 1.200787401574803681, 0.1660481256975885056, 0.3530559997133364547 ) ) ;
#19921 = CARTESIAN_POINT ( 'NONE',  ( -1.141732283464566011, -0.5511811023622047445, 6.969142054262312111E-17 ) ) ;
#19922 = CARTESIAN_POINT ( 'NONE',  ( 1.463254593175853824, -0.5511811023622046335, 0.09757992244046803654 ) ) ;
#19923 = CARTESIAN_POINT ( 'NONE',  ( -1.410761154855641575, -0.2845877964562161244, -0.3641732283464567121 ) ) ;
#19924 = CARTESIAN_POINT ( 'NONE',  ( -0.3937007874015740483, -0.1870078740157479769, 0.3641732283464567677 ) ) ;
#19925 = CARTESIAN_POINT ( 'NONE',  ( -1.476377952755905110, -0.4536011799217368745, -0.2665933059059886201 ) ) ;
#19926 = CARTESIAN_POINT ( 'NONE',  ( 1.056430446194226436, -0.5511811023622048555, -0.09757992244046775898 ) ) ;
#19927 = CARTESIAN_POINT ( 'NONE',  ( 0.6430446194225729606, -0.4281496062992127816, -0.4176697321401328100 ) ) ;
#19928 = CARTESIAN_POINT ( 'NONE',  ( 1.207349081364829990, -0.6046776061558809534, -0.2411417322834644161 ) ) ;
#19929 = CARTESIAN_POINT ( 'NONE',  ( 0.2362204724409456558, -0.1870078740157479769, 0.4822834645669291653 ) ) ;
#19930 = CARTESIAN_POINT ( 'NONE',  ( 0.5774278215223103139, -0.5023911411419708095, -0.1820866141732282451 ) ) ;
#19931 = B_SPLINE_CURVE_WITH_KNOTS ( 'NONE', 3,
 ( #14860, #33791, #52711, #59043, #7282, #19915, #1397, #26641, #20751, #46401, #72094, #64942, #78001, #64523, #8540, #20329, #14453, #45981 ),
 .UNSPECIFIED., .F., .F.,
 ( 4, 2, 2, 2, 2, 2, 2, 2, 4 ),
 ( 7.070062332036847214E-17, 0.001588476978679775799, 0.002382715468019628354, 0.002779834712689554631, 0.002978394335024517336, 0.003077674146191998906, 0.003127314051775739474, 0.003152134004567610191, 0.003176953957359480041 ),
 .UNSPECIFIED. ) ;
#19932 = CARTESIAN_POINT ( 'NONE',  ( 1.522309711286089939, -0.6046776061558809534, -0.2411417322834644161 ) ) ;
#19933 = FACE_OUTER_BOUND ( 'NONE', #16882, .T. ) ;
#19934 = CARTESIAN_POINT ( 'NONE',  ( -0.6299212598425188991, -0.1870078740157479769, 0.4822834645669291653 ) ) ;
#19935 = CARTESIAN_POINT ( 'NONE',  ( 0.3460692066303959202, 0.1998031496062993295, -0.4461942257217847430 ) ) ;
#19936 = CARTESIAN_POINT ( 'NONE',  ( 0.01277272433825663370, 0.004960608223778963273, 0.3437734562760189072 ) ) ;
#19937 = CARTESIAN_POINT ( 'NONE',  ( 0.1837270341207354329, 0.2306618581243848609, 0.2411417322834645549 ) ) ;
#19938 = CARTESIAN_POINT ( 'NONE',  ( -0.2559055118110227234, -0.5400638737290844871, 0.3530559997133364547 ) ) ;
#19939 = CARTESIAN_POINT ( 'NONE',  ( 0.09186351706036799403, -0.4281496062992127816, -0.4176697321401328100 ) ) ;
#19940 = CARTESIAN_POINT ( 'NONE',  ( -9.787531504996567848E-17, 0.3996062992125986035, -2.519685039370078705 ) ) ;
#19941 = CARTESIAN_POINT ( 'NONE',  ( -0.1974969037888703871, -0.3420746716998661063, -1.955380577427821454 ) ) ;
#19942 = CARTESIAN_POINT ( 'NONE',  ( -0.3917322834645671215, 0.1049643490035301469, -0.6548556430446192955 ) ) ;
#19943 = CARTESIAN_POINT ( 'NONE',  ( 0.1698998578625684763, 0.000000000000000000, 0.3464511005275205946 ) ) ;
#19944 = CARTESIAN_POINT ( 'NONE',  ( 4.797336870675656522E-17, -0.3917322834645670104, -0.8582677165354329896 ) ) ;
#19945 = CARTESIAN_POINT ( 'NONE',  ( -1.102362204724408601, -0.1870078740157479769, 0.3641732283464567677 ) ) ;
#19946 = CARTESIAN_POINT ( 'NONE',  ( 0.3917322834645669549, 0.1049643490035304660, -1.061679790026246462 ) ) ;
#19947 = CARTESIAN_POINT ( 'NONE',  ( -1.181102362204723644, -0.1870078740157480879, -0.4822834645669291653 ) ) ;
#19948 = CARTESIAN_POINT ( 'NONE',  ( -0.1049643490035306742, 0.3917322834645668994, 0.07088545751412257678 ) ) ;
#19949 = CARTESIAN_POINT ( 'NONE',  ( 0.2821522309711292364, 0.2952755905511810774, -0.1292274648535930714 ) ) ;
#19950 = CARTESIAN_POINT ( 'NONE',  ( 0.02624671916010564918, 0.1283753931104748280, 0.1820866141732283561 ) ) ;
#19951 = CARTESIAN_POINT ( 'NONE',  ( 1.108923884514436242, -0.05778040916215522460, 0.4822834645669289988 ) ) ;
#19952 = CARTESIAN_POINT ( 'NONE',  ( 0.2887139107611556010, -0.6046776061558807314, 0.2411417322834647770 ) ) ;
#19953 = CARTESIAN_POINT ( 'NONE',  ( -0.1265901696524993347, 0.4724409448818896462, -0.08333333333333334259 ) ) ;
#19954 = CARTESIAN_POINT ( 'NONE',  ( -9.787531504996567848E-17, 0.3996062992125986035, -2.677165354330708347 ) ) ;
#19955 = CARTESIAN_POINT ( 'NONE',  ( 0.3917322834645670659, 2.398668435337828261E-17, -1.374691231792337653 ) ) ;
#19956 = CARTESIAN_POINT ( 'NONE',  ( 1.417322834645670104, -0.1870078740157480879, -0.4822834645669291653 ) ) ;
#19957 = CARTESIAN_POINT ( 'NONE',  ( 0.6955380577427828781, 0.05413385826771626580, -0.4176697321401330321 ) ) ;
#19958 = CARTESIAN_POINT ( 'NONE',  ( 0.1509186351706042484, -0.3162353388693405765, 0.4822834645669290543 ) ) ;
#19959 = CARTESIAN_POINT ( 'NONE',  ( 1.233595800524935227, 0.2306618581243847221, -0.2411417322834647770 ) ) ;
#19960 = CARTESIAN_POINT ( 'NONE',  ( -0.1049643490035307020, 0.3917322834645669549, -0.7211286089238846397 ) ) ;
#19961 = CARTESIAN_POINT ( 'NONE',  ( 0.006561679790026889343, -0.05778040916215522460, 0.4822834645669289988 ) ) ;
#19962 = CARTESIAN_POINT ( 'NONE',  ( 0.9055118110236227702, 0.2952755905511811885, 0.000000000000000000 ) ) ;
#19963 = CARTESIAN_POINT ( 'NONE',  ( 0.4986876640419954376, -0.6046776061558809534, -0.2411417322834644161 ) ) ;
#19964 = CARTESIAN_POINT ( 'NONE',  ( 1.023622047244095334, -0.1870078740157479769, 0.3641732283464567677 ) ) ;
#19965 = CARTESIAN_POINT ( 'NONE',  ( -0.8727034120734901146, -0.05778040916215560624, -0.4822834645669293319 ) ) ;
#19966 = CARTESIAN_POINT ( 'NONE',  ( -1.266404199475064773, -0.3162353388693405765, 0.4822834645669290543 ) ) ;
#19967 = CARTESIAN_POINT ( 'NONE',  ( 0.7611548556430451917, -0.6046776061558807314, 0.2411417322834647770 ) ) ;
#19968 = CARTESIAN_POINT ( 'NONE',  ( -0.006303098002812318121, -0.3922539627124579931, -1.929133858267716883 ) ) ;
#19969 = CARTESIAN_POINT ( 'NONE',  ( 0.1958661417322834775, 0.3392501089628018884, -1.868766404199474929 ) ) ;
#19970 = CARTESIAN_POINT ( 'NONE',  ( 1.541994750656168645, 0.2952755905511810774, -0.1292274648535930714 ) ) ;
#19971 = VERTEX_POINT ( 'NONE', #2075 ) ;
#19972 = CARTESIAN_POINT ( 'NONE',  ( 0.3420746716998660508, -0.1974969037888703871, -2.939632545931758489 ) ) ;
#19973 = VERTEX_POINT ( 'NONE', #72370 ) ;
#19974 = CARTESIAN_POINT ( 'NONE',  ( 1.391076115485564868, 0.2306618581243847221, -0.2411417322834647770 ) ) ;
#19975 = CARTESIAN_POINT ( 'NONE',  ( 1.082677165354331228, -0.4536011799217367080, 0.2665933059059888421 ) ) ;
#19976 = CARTESIAN_POINT ( 'NONE',  ( 0.7974104941589355011, -4.927456884911482678E-16, 0.4445507791589062840 ) ) ;
#19977 = CARTESIAN_POINT ( 'NONE',  ( -0.2642730939577113136, 1.143123705106231736, 2.800754169703324692 ) ) ;
#19978 = CARTESIAN_POINT ( 'NONE',  ( -0.4359958488159755841, 1.724409448818897905, 1.033875059083675163 ) ) ;
#19979 = CARTESIAN_POINT ( 'NONE',  ( -0.2867679344610365999, 0.2867679344610364889, -0.7342519685039372579 ) ) ;
#19980 = EDGE_CURVE ( 'NONE', #39843, #75063, #15994, .T. ) ;
#19981 = CARTESIAN_POINT ( 'NONE',  ( -1.266404199475064773, -0.08942795157528024563, -0.3641732283464568787 ) ) ;
#19982 = CARTESIAN_POINT ( 'NONE',  ( -1.719160104986876103, -0.004921259842519576551, 0.3153832671262227771 ) ) ;
#19983 = FACE_OUTER_BOUND ( 'NONE', #37685, .T. ) ;
#19984 = CARTESIAN_POINT ( 'NONE',  ( -0.3018372703412066094, 0.05413385826771666132, 0.4176697321401328100 ) ) ;
#19985 = CARTESIAN_POINT ( 'NONE',  ( -1.601049868766403650, 0.2306618581243847221, -0.2411417322834647770 ) ) ;
#19986 = ORIENTED_EDGE ( 'NONE', *, *, #63016, .F. ) ;
#19987 = CARTESIAN_POINT ( 'NONE',  ( 0.000000000000000000, 0.4374015748031496176, 0.000000000000000000 ) ) ;
#19988 = CARTESIAN_POINT ( 'NONE',  ( 0.3149606299212484029, 2.559055118110236560, 1.076935383196061080 ) ) ;
#19989 = CARTESIAN_POINT ( 'NONE',  ( 0.8561328129276796206, 8.471767977567108961E-16, -0.4445507791589058955 ) ) ;
#19990 = CARTESIAN_POINT ( 'NONE',  ( -1.122047244094487306, 0.07958543189024071263, -0.2665933059059888421 ) ) ;
#19991 = CARTESIAN_POINT ( 'NONE',  ( -1.482939632545930975, 0.05413385826771666132, 0.4176697321401328100 ) ) ;
#19992 = CARTESIAN_POINT ( 'NONE',  ( 0.5249343832021005074, -0.6046776061558807314, 0.2411417322834647770 ) ) ;
#19993 = VERTEX_POINT ( 'NONE', #7562 ) ;
#19995 = CARTESIAN_POINT ( 'NONE',  ( 0.4724409448818898682, 2.892866454678787531E-17, -2.480314960629921295 ) ) ;
#19994 = CARTESIAN_POINT ( 'NONE',  ( -0.3458507752293906723, -0.3458507752293910609, -2.498031496062992574 ) ) ;
#19996 = CARTESIAN_POINT ( 'NONE',  ( 1.213910761154856299, 0.2952755905511811885, 0.1292274648535926551 ) ) ;
#19997 = CARTESIAN_POINT ( 'NONE',  ( 1.581364829396326277, -0.08942795157527998196, 0.3641732283464567121 ) ) ;
#19998 = CARTESIAN_POINT ( 'NONE',  ( -0.3392501089628018329, -0.1958661417322836440, -0.7624478758192109185 ) ) ;
#19999 = CARTESIAN_POINT ( 'NONE',  ( -0.2755905511811018171, 0.1771653543307087630, 0.000000000000000000 ) ) ;
#20000 = CARTESIAN_POINT ( 'NONE',  ( -1.528871391076114250, -0.5511811023622046335, 0.09757992244046803654 ) ) ;
#20001 = CARTESIAN_POINT ( 'NONE',  ( 1.614173228346457156, 1.929133858267716661, 0.5309055118110233007 ) ) ;
#20002 = CARTESIAN_POINT ( 'NONE',  ( 0.3215223097112867578, -0.05778040916215522460, 0.4822834645669289988 ) ) ;
#20003 = CARTESIAN_POINT ( 'NONE',  ( -0.3280839895013117347, -0.004921259842519870586, -0.3153832671262229437 ) ) ;
#20004 = CARTESIAN_POINT ( 'NONE',  ( 0.1509186351706042484, -0.2845877964562159024, 0.3641732283464567677 ) ) ;
#20005 = CARTESIAN_POINT ( 'NONE',  ( -0.08530183727034056085, -0.05778040916215560624, -0.4822834645669293319 ) ) ;
#20006 = CARTESIAN_POINT ( 'NONE',  ( -1.213910761154854745, -0.5511811023622046335, 0.09757992244046803654 ) ) ;
#20007 = CARTESIAN_POINT ( 'NONE',  ( -0.3917322834645670104, -0.1049643490035307020, 0.1148100805436201299 ) ) ;
#20008 = CARTESIAN_POINT ( 'NONE',  ( 0.8530183727034126306, 0.05413385826771626580, -0.4176697321401330321 ) ) ;
#20009 = CARTESIAN_POINT ( 'NONE',  ( -1.574803149606298192, -0.1870078740157480879, -0.4822834645669291653 ) ) ;
#20010 = CARTESIAN_POINT ( 'NONE',  ( -0.4091458600556402980, -0.2362204724409451284, -1.074146981627296604 ) ) ;
#20011 = CARTESIAN_POINT ( 'NONE',  ( -0.4461942257217840213, 0.2306618581243848609, 0.2411417322834645549 ) ) ;
#20012 = CARTESIAN_POINT ( 'NONE',  ( 0.2821522309711292364, -0.5511811023622046335, 0.09757992244046803654 ) ) ;
#20013 = CARTESIAN_POINT ( 'NONE',  ( -1.043307086614172041, -0.5400638737290844871, 0.3530559997133364547 ) ) ;
#20014 = CARTESIAN_POINT ( 'NONE',  ( 0.7677165354330716118, 0.07958543189024071263, -0.2665933059059888421 ) ) ;
#20015 = CARTESIAN_POINT ( 'NONE',  ( -0.1509186351706028884, -0.08942795157527998196, 0.3641732283464567121 ) ) ;
#20016 = CARTESIAN_POINT ( 'NONE',  ( -0.7283464566929126471, 0.1660481256975883668, -0.3530559997133364547 ) ) ;
#20017 = CARTESIAN_POINT ( 'NONE',  ( -1.456692913385826182, 0.2952755905511811885, 0.000000000000000000 ) ) ;
#20018 = CARTESIAN_POINT ( 'NONE',  ( -0.5314960629921194890, 2.716535433070866645, -1.854472803289054283 ) ) ;
#20019 = CARTESIAN_POINT ( 'NONE',  ( 1.194225721784777594, -0.004921259842519576551, 0.3153832671262227771 ) ) ;
#20020 = CARTESIAN_POINT ( 'NONE',  ( 0.3805774278215230400, -0.4281496062992124485, 0.4176697321401328655 ) ) ;
#20021 = CARTESIAN_POINT ( 'NONE',  ( -1.601049868766403650, 0.2306618581243847221, -0.2411417322834647770 ) ) ;
#20022 = CARTESIAN_POINT ( 'NONE',  ( -1.332020997375327642, -0.3162353388693409650, -0.4822834645669289433 ) ) ;
#20023 = ORIENTED_EDGE ( 'NONE', *, *, #35324, .T. ) ;
#20024 = CARTESIAN_POINT ( 'NONE',  ( 0.1998031496062992463, 0.3460692066303959202, -2.583333333333333481 ) ) ;
#20025 = CARTESIAN_POINT ( 'NONE',  ( -0.9120734908136475250, -0.5511811023622048555, -0.09757992244046775898 ) ) ;
#20026 = CARTESIAN_POINT ( 'NONE',  ( 0.5839895013123367340, -0.6692913385826773087, -0.1292274648535924053 ) ) ;
#20027 = CARTESIAN_POINT ( 'NONE',  ( -0.9514435695538050464, -0.2845877964562159024, 0.3641732283464567677 ) ) ;
#20028 = CARTESIAN_POINT ( 'NONE',  ( 0.3996062992125986035, -0.1070741851644052972, -1.920603674540682260 ) ) ;
#20029 = CARTESIAN_POINT ( 'NONE',  ( -1.194225721784776262, 0.05413385826771626580, -0.4176697321401330321 ) ) ;
#20030 = CARTESIAN_POINT ( 'NONE',  ( 0.9120734908136490793, 0.2952755905511810774, -0.1292274648535930714 ) ) ;
#20031 = CARTESIAN_POINT ( 'NONE',  ( 0.3280839895013130669, -0.4281496062992127816, -0.4176697321401328100 ) ) ;
#20032 = CARTESIAN_POINT ( 'NONE',  ( 1.469816272965879911, 0.2306618581243847221, -0.2411417322834647770 ) ) ;
#20033 = CARTESIAN_POINT ( 'NONE',  ( -1.679790026246718693, 0.1283753931104746893, -0.1820866141732285504 ) ) ;
#20034 = CARTESIAN_POINT ( 'NONE',  ( 0.3460692066303958092, 0.1998031496062993018, -0.9954068241469815614 ) ) ;
#20035 = CARTESIAN_POINT ( 'NONE',  ( 0.3996062992125986590, -0.1070741851644053111, -1.213910761154855189 ) ) ;
#20036 = CARTESIAN_POINT ( 'NONE',  ( 0.1974969037888704704, 0.3420746716998660508, -0.6167979002624671692 ) ) ;
#20037 = CARTESIAN_POINT ( 'NONE',  ( 0.2538623822092395677, 1.136619844641765242, -1.626743363757151117 ) ) ;
#20038 = CARTESIAN_POINT ( 'NONE',  ( 0.6692913385826778638, -0.5511811023622047445, 6.969142054262312111E-17 ) ) ;
#20039 = CARTESIAN_POINT ( 'NONE',  ( 0.3477690288713918276, 0.1771653543307087630, 0.09757992244046791164 ) ) ;
#20040 = CARTESIAN_POINT ( 'NONE',  ( -0.09842519685039295696, 0.1660481256975883668, -0.3530559997133364547 ) ) ;
#20041 = CARTESIAN_POINT ( 'NONE',  ( 1.148293963254593653, 0.2952755905511810774, -0.1292274648535930714 ) ) ;
#20042 = CARTESIAN_POINT ( 'NONE',  ( -0.1974969037888706924, 0.3420746716998658843, -1.664698162729658870 ) ) ;
#20043 = CARTESIAN_POINT ( 'NONE',  ( 0.2559055118110243332, 0.07958543189024085140, 0.2665933059059887866 ) ) ;
#20044 = CARTESIAN_POINT ( 'NONE',  ( -0.7086614173228339419, -0.1870078740157479769, 0.4822834645669291653 ) ) ;
#20045 = CARTESIAN_POINT ( 'NONE',  ( -1.358267716535432434, -0.5400638737290844871, 0.3530559997133364547 ) ) ;
#20046 = CARTESIAN_POINT ( 'NONE',  ( 1.017060367454068803, -0.3162353388693405765, 0.4822834645669290543 ) ) ;
#20047 = CARTESIAN_POINT ( 'NONE',  ( -0.4091458600556405756, 0.2362204724409446288, -1.758530183727034180 ) ) ;
#20048 = CARTESIAN_POINT ( 'NONE',  ( 0.3165741174738966324, 0.2316922116739144610, -2.755905511811024944 ) ) ;
#20049 = EDGE_LOOP ( 'NONE', ( #39373, #60628, #5446, #56356 ) ) ;
#20050 = ORIENTED_EDGE ( 'NONE', *, *, #77818, .T. ) ;
#20051 = CARTESIAN_POINT ( 'NONE',  ( -1.410761154855642463, -0.05778040916215522460, 0.4822834645669289988 ) ) ;
#20052 = CARTESIAN_POINT ( 'NONE',  ( -0.4461942257217840213, -0.6046776061558809534, -0.2411417322834644161 ) ) ;
#20054 = CARTESIAN_POINT ( 'NONE',  ( -0.9580052493438311334, 0.05413385826771626580, -0.4176697321401330321 ) ) ;
#20053 = CARTESIAN_POINT ( 'NONE',  ( -0.6167979002624665030, -0.3690944881889765550, -0.3153832671262227771 ) ) ;
#20055 = CARTESIAN_POINT ( 'NONE',  ( 0.2867679344610365999, 0.2867679344610365999, -1.792631602853332007 ) ) ;
#20056 = CARTESIAN_POINT ( 'NONE',  ( -0.4613432605871728986, -1.429000049448402363E-15, 0.3954974714151491821 ) ) ;
#20057 = CARTESIAN_POINT ( 'NONE',  ( 1.633858267716535639, -0.5400638737290844871, 0.3530559997133364547 ) ) ;
#20058 = CARTESIAN_POINT ( 'NONE',  ( -1.325459317585300889, -0.4281496062992127816, -0.4176697321401328100 ) ) ;
#20059 = CARTESIAN_POINT ( 'NONE',  ( 0.4265091863517067039, -0.6692913385826773087, -0.1292274648535924053 ) ) ;
#20060 = CARTESIAN_POINT ( 'NONE',  ( -0.8989501312335946848, -0.6692913385826771977, 0.1292274648535927661 ) ) ;
#20061 = CARTESIAN_POINT ( 'NONE',  ( -0.1049643490035307020, 0.3917322834645669549, 0.06627296587926499727 ) ) ;
#20062 = EDGE_CURVE ( 'NONE', #82183, #54857, #62175, .T. ) ;
#20063 = CARTESIAN_POINT ( 'NONE',  ( 0.6561679790026253567, 0.2306618581243848609, 0.2411417322834645549 ) ) ;
#20064 = CARTESIAN_POINT ( 'NONE',  ( 4.797336870675656522E-17, -0.3917322834645670104, -1.488188976377952777 ) ) ;
#20065 = CARTESIAN_POINT ( 'NONE',  ( -0.7611548556430438595, -0.5023911411419708095, -0.1820866141732282451 ) ) ;
#20066 = ORIENTED_EDGE ( 'NONE', *, *, #16700, .T. ) ;
#20067 = CARTESIAN_POINT ( 'NONE',  ( -0.3949938075777411628, 0.1058382717557497937, -1.922572178477690130 ) ) ;
#20068 = VERTEX_POINT ( 'NONE', #71951 ) ;
#20069 = CARTESIAN_POINT ( 'NONE',  ( -1.660104986876639543, -0.08942795157528024563, -0.3641732283464568787 ) ) ;
#20070 = CARTESIAN_POINT ( 'NONE',  ( -0.9514435695538050464, -0.3162353388693405765, 0.4822834645669290543 ) ) ;
#20071 = CARTESIAN_POINT ( 'NONE',  ( -1.227034120734907141, -0.6692913385826773087, -0.1292274648535924053 ) ) ;
#20072 = CARTESIAN_POINT ( 'NONE',  ( 0.1998031496062992740, 0.3460692066303959757, -0.6167979002624671692 ) ) ;
#20073 = CARTESIAN_POINT ( 'NONE',  ( -1.141732283464566011, -0.6692913385826771977, 8.415575281601705876E-17 ) ) ;
#20074 = CARTESIAN_POINT ( 'NONE',  ( -1.456692913385826182, -0.6692913385826771977, 8.415575281601705876E-17 ) ) ;
#20075 = VECTOR ( 'NONE', #49151, 39.37007874015748143 ) ;
#20076 = CARTESIAN_POINT ( 'NONE',  ( -1.358267716535432434, -0.5400638737290844871, 0.3530559997133364547 ) ) ;
#20077 = CARTESIAN_POINT ( 'NONE',  ( -1.948818897637795367, 1.928577636452520604E-17, 5.859448621221250875 ) ) ;
#20078 = CARTESIAN_POINT ( 'NONE',  ( 0.1698998578625684763, 0.000000000000000000, 0.3464511005275205946 ) ) ;
#20079 = ADVANCED_FACE ( 'NONE', ( #65224 ), #43702, .T. ) ;
#20080 = CARTESIAN_POINT ( 'NONE',  ( 0.2559055118110243332, 0.07958543189024085140, 0.2665933059059887866 ) ) ;
#20081 = DIRECTION ( 'NONE',  ( 0.000000000000000000, 1.000000000000000000, 0.000000000000000000 ) ) ;
#20082 = CARTESIAN_POINT ( 'NONE',  ( -0.3392501089628019995, 0.1958661417322832277, -0.2683727034120735877 ) ) ;
#20083 = CARTESIAN_POINT ( 'NONE',  ( -0.3608923884514428360, -0.5511811023622048555, -0.09757992244046775898 ) ) ;
#20084 = CARTESIAN_POINT ( 'NONE',  ( -0.8398950131233585692, 0.2306618581243848609, 0.2411417322834645549 ) ) ;
#20085 = CARTESIAN_POINT ( 'NONE',  ( 0.7545931758530188826, -0.6692913385826771977, 0.1292274648535927661 ) ) ;
#20086 = CARTESIAN_POINT ( 'NONE',  ( -0.3018372703412066094, -0.4281496062992127816, -0.4176697321401328100 ) ) ;
#20087 = ORIENTED_EDGE ( 'NONE', *, *, #80969, .F. ) ;
#20088 = ORIENTED_EDGE ( 'NONE', *, *, #48534, .T. ) ;
#20089 = CARTESIAN_POINT ( 'NONE',  ( 0.2925321140481932369, -0.2925321140481931814, -1.907480314960629197 ) ) ;
#20090 = CARTESIAN_POINT ( 'NONE',  ( -1.115485564304461219, 0.05413385826771626580, -0.4176697321401330321 ) ) ;
#20091 = CARTESIAN_POINT ( 'NONE',  ( 1.266404199475066328, -0.05778040916215522460, 0.4822834645669289988 ) ) ;
#20092 = CARTESIAN_POINT ( 'NONE',  ( -1.371391076115484831, 0.1771653543307087075, -0.09757992244046823083 ) ) ;
#20093 = CARTESIAN_POINT ( 'NONE',  ( 0.4091458600556403535, 0.2362204724409449896, -0.7611548556430446366 ) ) ;
#20094 = CARTESIAN_POINT ( 'NONE',  ( 1.901964908973707402, 1.119136672863562776, 0.2244172274865111338 ) ) ;
#20095 = CARTESIAN_POINT ( 'NONE',  ( 0.3917322834645670104, 2.398668435337828261E-17, -0.4251968503937007537 ) ) ;
#20096 = LINE ( 'NONE', #38611, #11637 ) ;
#20097 = CARTESIAN_POINT ( 'NONE',  ( -0.3215223097112853146, -0.05778040916215560624, -0.4822834645669293319 ) ) ;
#20098 = CARTESIAN_POINT ( 'NONE',  ( -1.601049868766403650, 0.1283753931104746893, -0.1820866141732285504 ) ) ;
#20099 = CARTESIAN_POINT ( 'NONE',  ( -0.6102362204724400829, 0.1660481256975885056, 0.3530559997133364547 ) ) ;
#20100 = CARTESIAN_POINT ( 'NONE',  ( -0.3996062992125986590, 0.1070741851644051723, 0.2053805774278214813 ) ) ;
#20102 = CARTESIAN_POINT ( 'NONE',  ( 0.000000000000000000, 2.716535433070866645, 0.000000000000000000 ) ) ;
#20101 = CARTESIAN_POINT ( 'NONE',  ( -1.397637795275589623, 0.1660481256975885056, 0.3530559997133364547 ) ) ;
#20103 = CARTESIAN_POINT ( 'NONE',  ( -1.115485564304461219, -0.4281496062992124485, 0.4176697321401328655 ) ) ;
#20104 = CARTESIAN_POINT ( 'NONE',  ( -0.3477690288713905509, -0.6692913385826771977, 0.1292274648535927661 ) ) ;
#20106 = B_SPLINE_CURVE_WITH_KNOTS ( 'NONE', 3,
 ( #48749, #74448, #34900, #42431 ),
 .UNSPECIFIED., .F., .F.,
 ( 4, 4 ),
 ( 0.07469576999304926301, 0.07612553241189917719 ),
 .UNSPECIFIED. ) ;
#20105 = CARTESIAN_POINT ( 'NONE',  ( 4.837279021331061486E-17, -0.3949938075777409963, -2.832677165354331006 ) ) ;
#20107 = CARTESIAN_POINT ( 'NONE',  ( 0.8858267716535438430, -0.4536011799217368745, -0.2665933059059886201 ) ) ;
#20108 = CARTESIAN_POINT ( 'NONE',  ( 0.2867679344610366554, -0.2867679344610365444, -0.02559055118110245552 ) ) ;
#20109 = CARTESIAN_POINT ( 'NONE',  ( 0.8661417322834653598, -0.1870078740157479769, 0.3641732283464567677 ) ) ;
#20110 = CARTESIAN_POINT ( 'NONE',  ( 1.561679790026247350, -0.3690944881889763329, 0.3153832671262228327 ) ) ;
#20111 = CARTESIAN_POINT ( 'NONE',  ( 1.233595800524935227, -0.6046776061558807314, 0.2411417322834647770 ) ) ;
#20112 = UNCERTAINTY_MEASURE_WITH_UNIT (LENGTH_MEASURE( 1.000000000000000082E-05 ), #1164, 'distance_accuracy_value', 'NONE');
#20113 = CARTESIAN_POINT ( 'NONE',  ( 0.05249343832021075018, -0.5023911411419708095, 0.1820866141732285504 ) ) ;
#20114 = CARTESIAN_POINT ( 'NONE',  ( -0.3917322834645669549, -0.1049643490035306603, -1.612860892388451539 ) ) ;
#20115 = CARTESIAN_POINT ( 'NONE',  ( -0.7742782152230962556, -0.4281496062992127816, -0.4176697321401328100 ) ) ;
#20116 = CARTESIAN_POINT ( 'NONE',  ( 1.108923884514436242, -0.05778040916215522460, 0.4822834645669289988 ) ) ;
#20117 = CARTESIAN_POINT ( 'NONE',  ( -0.4724409448818895907, -0.1265901696524993070, 0.03477690288713909672 ) ) ;
#20118 = CARTESIAN_POINT ( 'NONE',  ( -0.6758530183727028406, 0.1771653543307087630, 0.09757992244046791164 ) ) ;
#20119 = CARTESIAN_POINT ( 'NONE',  ( -0.4724409448818898682, -8.678599364036362592E-17, -1.061023622047243986 ) ) ;
#20120 = CARTESIAN_POINT ( 'NONE',  ( 0.2821522309711292364, 0.2952755905511810774, -0.1292274648535930714 ) ) ;
#20121 = CARTESIAN_POINT ( 'NONE',  ( -0.2362204724409451284, 0.4091458600556402425, -0.7198162729658792447 ) ) ;
#20122 = CARTESIAN_POINT ( 'NONE',  ( 0.9251968503937015864, -0.4536011799217367080, 0.2665933059059888421 ) ) ;
#20123 = CARTESIAN_POINT ( 'NONE',  ( -0.03280839895013062252, -0.5511811023622046335, 0.09757992244046803654 ) ) ;
#20124 = CARTESIAN_POINT ( 'NONE',  ( -0.2755905511811015396, -0.6692913385826771977, 8.415575281601705876E-17 ) ) ;
#20125 = CARTESIAN_POINT ( 'NONE',  ( -1.187664041994750175, -0.05778040916215560624, -0.4822834645669293319 ) ) ;
#20126 = CARTESIAN_POINT ( 'NONE',  ( -0.6167979002624665030, -0.3690944881889765550, -0.3153832671262227771 ) ) ;
#20127 = PLANE ( 'NONE',  #5856 ) ;
#20128 = CARTESIAN_POINT ( 'NONE',  ( 0.7217847769028878924, 0.05413385826771666132, 0.4176697321401328100 ) ) ;
#20129 = CARTESIAN_POINT ( 'NONE',  ( -1.049868766404198794, -0.6046776061558807314, 0.2411417322834647770 ) ) ;
#20130 = CARTESIAN_POINT ( 'NONE',  ( 0.3996062992125985480, 2.446882876249141654E-17, -1.139763779527559029 ) ) ;
#20131 = CARTESIAN_POINT ( 'NONE',  ( 0.1958661417322834775, 0.3392501089628018884, -2.748687664041994605 ) ) ;
#20132 = CARTESIAN_POINT ( 'NONE',  ( 0.2427821522309716595, -0.2845877964562161244, -0.3641732283464567121 ) ) ;
#20133 = CARTESIAN_POINT ( 'NONE',  ( -0.8989501312335946848, -0.6692913385826771977, 0.1292274648535927661 ) ) ;
#20134 = CARTESIAN_POINT ( 'NONE',  ( -1.010498687664041384, 0.05413385826771666132, 0.4176697321401328100 ) ) ;
#20135 = CARTESIAN_POINT ( 'NONE',  ( -1.240157480314959759, -0.4536011799217368745, -0.2665933059059886201 ) ) ;
#20136 = CARTESIAN_POINT ( 'NONE',  ( 1.660104986876641320, -0.05778040916215522460, 0.4822834645669289988 ) ) ;
#20137 = CARTESIAN_POINT ( 'NONE',  ( -1.030183727034119867, -0.2845877964562159024, 0.3641732283464567677 ) ) ;
#20138 = CARTESIAN_POINT ( 'NONE',  ( -0.7611548556430438595, 0.1539470093639523085, 0.1968503937007873850 ) ) ;
#20139 = CARTESIAN_POINT ( 'NONE',  ( 1.332020997375328974, -0.05778040916215560624, -0.4822834645669293319 ) ) ;
#20140 = CARTESIAN_POINT ( 'NONE',  ( -0.3917322834645670104, -0.1049643490035307020, -2.562355273787088716 ) ) ;
#20141 = EDGE_CURVE ( 'NONE', #69851, #50773, #38013, .T. ) ;
#20142 = EDGE_LOOP ( 'NONE', ( #30006, #31811, #64028, #70677 ) ) ;
#20143 = CARTESIAN_POINT ( 'NONE',  ( 0.01150853369506186011, -0.3951562584566668535, -5.613290098372280880E-13 ) ) ;
#20144 = CARTESIAN_POINT ( 'NONE',  ( 1.561679790026247350, -0.3690944881889763329, 0.3153832671262228327 ) ) ;
#20145 = CARTESIAN_POINT ( 'NONE',  ( -1.095800524934382292, -0.05778040916215522460, 0.4822834645669289988 ) ) ;
#20146 = CARTESIAN_POINT ( 'NONE',  ( 1.148293963254593653, 0.2952755905511810774, -0.1292274648535930714 ) ) ;
#20147 = CARTESIAN_POINT ( 'NONE',  ( 0.2867679344610365999, 0.2867679344610365999, -2.112204724409449064 ) ) ;
#20148 = CARTESIAN_POINT ( 'NONE',  ( 1.646981627296588035, -0.2845877964562159024, 0.3641732283464567677 ) ) ;
#20149 = CARTESIAN_POINT ( 'NONE',  ( 0.6233595800524942554, -0.05778040916215560624, -0.4822834645669293319 ) ) ;
#20150 = CARTESIAN_POINT ( 'NONE',  ( 0.1049868766404206816, 0.2306618581243848609, 0.2411417322834645549 ) ) ;
#20151 = CARTESIAN_POINT ( 'NONE',  ( 0.2895944160946348211, 1.160344800674453003, -3.926428547179232620 ) ) ;
#20152 = CARTESIAN_POINT ( 'NONE',  ( 0.3996062992125985480, -0.1070741851644052972, -2.708005249343832244 ) ) ;
#20153 = CARTESIAN_POINT ( 'NONE',  ( 0.6496062992125991586, 0.07958543189024085140, 0.2665933059059887866 ) ) ;
#20154 = CARTESIAN_POINT ( 'NONE',  ( -0.1998031496062994683, 0.3460692066303958092, -1.272965879265091749 ) ) ;
#20155 = ORIENTED_EDGE ( 'NONE', *, *, #76274, .F. ) ;
#20156 = CARTESIAN_POINT ( 'NONE',  ( 0.3392501089628018884, -0.1958661417322834220, -2.931758530183726563 ) ) ;
#20157 = EDGE_LOOP ( 'NONE', ( #20087, #58886, #37034, #50984 ) ) ;
#20158 = CARTESIAN_POINT ( 'NONE',  ( 0.06561679790026316017, 0.05413385826771626580, -0.4176697321401330321 ) ) ;
#20159 = CARTESIAN_POINT ( 'NONE',  ( 1.528871391076116026, -0.6692913385826773087, -0.1292274648535924053 ) ) ;
#20160 = CARTESIAN_POINT ( 'NONE',  ( 0.5774278215223104249, 0.2306618581243848609, 0.2411417322834645549 ) ) ;
#20161 = CARTESIAN_POINT ( 'NONE',  ( 1.069553805774278832, 0.2952755905511810774, -0.1292274648535930714 ) ) ;
#20162 = CARTESIAN_POINT ( 'NONE',  ( -0.3608923884514428360, 0.2952755905511811885, 0.1292274648535926551 ) ) ;
#20163 = CARTESIAN_POINT ( 'NONE',  ( 0.02624671916010564918, 0.2306618581243848609, 0.2411417322834645549 ) ) ;
#20164 = CARTESIAN_POINT ( 'NONE',  ( 1.561679790026247350, -0.4281496062992124485, 0.4176697321401328655 ) ) ;
#20165 = CARTESIAN_POINT ( 'NONE',  ( 1.397637795275591177, -0.5400638737290844871, 0.3530559997133364547 ) ) ;
#20166 = CARTESIAN_POINT ( 'NONE',  ( 1.128608923884515169, -0.6046776061558809534, -0.2411417322834644161 ) ) ;
#20167 = CARTESIAN_POINT ( 'NONE',  ( 0.1049643490035304938, -0.3917322834645669549, -0.07742782152230966164 ) ) ;
#20168 = CARTESIAN_POINT ( 'NONE',  ( 0.6430446194225729606, -0.3690944881889765550, -0.3153832671262227771 ) ) ;
#20169 = ORIENTED_EDGE ( 'NONE', *, *, #15774, .F. ) ;
#20170 = CARTESIAN_POINT ( 'NONE',  ( 0.3949938075777409408, 0.1058382717557500574, -0.4396325459317587114 ) ) ;
#20171 = ORIENTED_EDGE ( 'NONE', *, *, #65042, .F. ) ;
#20172 = CARTESIAN_POINT ( 'NONE',  ( -0.3083989501312330295, -0.08942795157527998196, 0.3641732283464567121 ) ) ;
#20173 = CARTESIAN_POINT ( 'NONE',  ( -0.03280839895013062252, 0.2952755905511810774, -0.1292274648535930714 ) ) ;
#20174 = CARTESIAN_POINT ( 'NONE',  ( 2.723203318070475998, 1.231544801320231919, -0.3638227417423834931 ) ) ;
#20175 = CARTESIAN_POINT ( 'NONE',  ( 0.2034120734908142214, 0.2952755905511810774, -0.1292274648535930714 ) ) ;
#20176 = CARTESIAN_POINT ( 'NONE',  ( 0.1509186351706042484, -0.3162353388693405765, 0.4822834645669290543 ) ) ;
#20177 = CARTESIAN_POINT ( 'NONE',  ( -0.8202099737532801971, -0.6692913385826771977, 0.1292274648535927661 ) ) ;
#20178 = CARTESIAN_POINT ( 'NONE',  ( 1.450131233595801428, -0.5511811023622048555, -0.09757992244046775898 ) ) ;
#20179 = CARTESIAN_POINT ( 'NONE',  ( -1.633858267716534529, 0.1660481256975885056, 0.3530559997133364547 ) ) ;
#20180 = DIRECTION ( 'NONE',  ( -0.000000000000000000, 1.000000000000000000, -0.000000000000000000 ) ) ;
#20181 = CARTESIAN_POINT ( 'NONE',  ( 0.8398950131233602345, 0.1283753931104746893, -0.1820866141732285504 ) ) ;
#20182 = CARTESIAN_POINT ( 'NONE',  ( 0.6233595800524942554, -0.05778040916215560624, -0.4822834645669293319 ) ) ;
#20183 = CARTESIAN_POINT ( 'NONE',  ( 0.7086614173228353852, -0.1870078740157479769, 0.4822834645669291653 ) ) ;
#20184 = CARTESIAN_POINT ( 'NONE',  ( -0.3460692066303960868, 0.1998031496062990242, -1.443569553805774230 ) ) ;
#20185 = CARTESIAN_POINT ( 'NONE',  ( -1.581364829396324945, -0.3162353388693405765, 0.4822834645669290543 ) ) ;
#20186 = CARTESIAN_POINT ( 'NONE',  ( -0.1998031496062994405, 0.3460692066303957537, -0.5623359580052492701 ) ) ;
#20187 = CARTESIAN_POINT ( 'NONE',  ( -0.3996062992125984925, -0.1070741851644056858, -0.1227034120734908501 ) ) ;
#20188 = CARTESIAN_POINT ( 'NONE',  ( -0.07874015748031421014, -0.1870078740157480879, -0.4822834645669291653 ) ) ;
#20189 = CARTESIAN_POINT ( 'NONE',  ( 4.893765752498283924E-17, -0.3996062992125986035, -2.598425196850393970 ) ) ;
#20190 = CARTESIAN_POINT ( 'NONE',  ( 0.3392501089628018884, -0.1958661417322834220, -2.079396325459317740 ) ) ;
#20191 = CARTESIAN_POINT ( 'NONE',  ( -1.135170603674539924, 0.1771653543307087075, -0.09757992244046823083 ) ) ;
#20192 = CARTESIAN_POINT ( 'NONE',  ( 1.450131233595801428, 0.2952755905511811885, 0.1292274648535926551 ) ) ;
#20193 = CARTESIAN_POINT ( 'NONE',  ( 1.443569553805774897, -0.6046776061558809534, -0.2411417322834644161 ) ) ;
#20194 = CARTESIAN_POINT ( 'NONE',  ( -0.09842519685039295696, -0.4536011799217367080, 0.2665933059059888421 ) ) ;
#20195 = CARTESIAN_POINT ( 'NONE',  ( 0.4593175853018379162, -0.4281496062992124485, 0.4176697321401328655 ) ) ;
#20196 = CARTESIAN_POINT ( 'NONE',  ( 0.4724409448818898682, 2.892866454678787531E-17, -1.454724409448818756 ) ) ;
#20197 = CARTESIAN_POINT ( 'NONE',  ( 0.2362204724409456558, -0.1870078740157479769, 0.3641732283464567677 ) ) ;
#20198 = CARTESIAN_POINT ( 'NONE',  ( 5.463695987328526437E-16, -0.1870078740157479769, 0.4822834645669291653 ) ) ;
#20200 = CONICAL_SURFACE ( 'NONE', #79528, 1.220472440944881942, 0.7853981633974621568 ) ;
#20199 = CARTESIAN_POINT ( 'NONE',  ( -0.1058382717557497660, -0.3949938075777411073, -1.251312335958005173 ) ) ;
#20201 = CARTESIAN_POINT ( 'NONE',  ( -1.135170603674539924, -0.6692913385826771977, 0.1292274648535927661 ) ) ;
#20202 = CARTESIAN_POINT ( 'NONE',  ( 0.4068241469816279987, -0.3690944881889765550, -0.3153832671262227771 ) ) ;
#20203 = CARTESIAN_POINT ( 'NONE',  ( 0.3740157480314966754, 0.1012011053420775880, -0.2882089793578257453 ) ) ;
#20205 = EDGE_CURVE ( 'NONE', #49832, #34363, #9111, .T. ) ;
#20204 = CARTESIAN_POINT ( 'NONE',  ( -0.8464566929133852113, -0.5400638737290845981, -0.3530559997133363437 ) ) ;
#20206 = CARTESIAN_POINT ( 'NONE',  ( -0.4855643044619415427, -0.004921259842519870586, -0.3153832671262229437 ) ) ;
#20207 = DIRECTION ( 'NONE',  ( 0.000000000000000000, -0.6427876096865389188, -0.7660444431189783465 ) ) ;
#20208 = CARTESIAN_POINT ( 'NONE',  ( -0.6364829396325453192, -0.3162353388693405765, 0.4822834645669290543 ) ) ;
#20209 = CARTESIAN_POINT ( 'NONE',  ( -0.3871391076115476282, -0.05778040916215522460, 0.4822834645669289988 ) ) ;
#20210 = CARTESIAN_POINT ( 'NONE',  ( 0.3543307086614179147, 0.1771653543307087630, 0.000000000000000000 ) ) ;
#20211 = CARTESIAN_POINT ( 'NONE',  ( -9.787531504996566615E-17, 0.3996062992125985480, -2.281496062992125928 ) ) ;
#20212 = CARTESIAN_POINT ( 'NONE',  ( -0.09186351706036663400, -0.4281496062992124485, 0.4176697321401328655 ) ) ;
#20213 = EDGE_CURVE ( 'NONE', #9504, #76474, #4934, .T. ) ;
#20214 = CARTESIAN_POINT ( 'NONE',  ( -9.594673741351310580E-17, 0.3917322834645669549, -2.127277272144670217 ) ) ;
#20215 = CARTESIAN_POINT ( 'NONE',  ( -1.660104986876639543, -0.08942795157528024563, -0.3641732283464568787 ) ) ;
#20216 = CARTESIAN_POINT ( 'NONE',  ( 0.6167979002624679463, -0.004921259842519870586, -0.3153832671262229437 ) ) ;
#20217 = CARTESIAN_POINT ( 'NONE',  ( 1.463254593175853824, 0.2952755905511810774, -0.1292274648535930714 ) ) ;
#20218 = CARTESIAN_POINT ( 'NONE',  ( -0.6627296587926503335, -0.5511811023622046335, 0.09757992244046803654 ) ) ;
#20219 = CARTESIAN_POINT ( 'NONE',  ( -0.9514435695538050464, -0.2845877964562159024, 0.3641732283464567677 ) ) ;
#20220 = CARTESIAN_POINT ( 'NONE',  ( -0.7283464566929126471, -0.5400638737290844871, 0.3530559997133364547 ) ) ;
#20221 = CARTESIAN_POINT ( 'NONE',  ( 0.01968503937007930540, 0.1660481256975885056, 0.3530559997133364547 ) ) ;
#20222 = CARTESIAN_POINT ( 'NONE',  ( 0.4724409448818904789, -0.1870078740157480601, -0.3641732283464567677 ) ) ;
#20223 = CARTESIAN_POINT ( 'NONE',  ( -0.2896728340831399851, 0.05829427551933642065, 5.869670624399383030 ) ) ;
#20224 = CARTESIAN_POINT ( 'NONE',  ( 0.8923884514435701520, -0.5023911411419708095, -0.1820866141732282451 ) ) ;
#20225 = CARTESIAN_POINT ( 'NONE',  ( 0.2099737532808405305, -0.6046776061558807314, 0.2411417322834647770 ) ) ;
#20226 = EDGE_CURVE ( 'NONE', #69770, #31420, #77851, .T. ) ;
#20227 = CARTESIAN_POINT ( 'NONE',  ( 0.3996062992125984925, 0.1070741851644054637, -0.04396325459317586282 ) ) ;
#20228 = CARTESIAN_POINT ( 'NONE',  ( -0.6233595800524928121, -0.05778040916215522460, 0.4822834645669289988 ) ) ;
#20229 = CARTESIAN_POINT ( 'NONE',  ( -0.1049643490035302024, -0.3917322834645671215, -1.259186351706037099 ) ) ;
#20230 = CARTESIAN_POINT ( 'NONE',  ( 1.404199475065617264, -0.3690944881889763329, 0.3153832671262228327 ) ) ;
#20231 = CARTESIAN_POINT ( 'NONE',  ( 0.4330708661417329575, 0.2952755905511811885, 0.000000000000000000 ) ) ;
#20232 = CARTESIAN_POINT ( 'NONE',  ( 0.05905511811023709395, -0.5400638737290844871, 0.3530559997133364547 ) ) ;
#20233 = CARTESIAN_POINT ( 'NONE',  ( 1.604771003085129211, 1.002618919725273061, 0.1466069496707753106 ) ) ;
#20234 = CARTESIAN_POINT ( 'NONE',  ( -0.06561679790026180015, -0.004921259842519576551, 0.3153832671262227771 ) ) ;
#20235 = CARTESIAN_POINT ( 'NONE',  ( 0.8202099737532814183, -0.6692913385826773087, -0.1292274648535924053 ) ) ;
#20236 = CARTESIAN_POINT ( 'NONE',  ( -0.2559055118110230564, 0.07958543189024071263, -0.2665933059059888421 ) ) ;
#20237 = CARTESIAN_POINT ( 'NONE',  ( -0.8398950131233585692, 0.2306618581243848609, 0.2411417322834645549 ) ) ;
#20238 = FACE_OUTER_BOUND ( 'NONE', #38152, .T. ) ;
#20239 = CARTESIAN_POINT ( 'NONE',  ( -0.2952755905511804668, 0.1660481256975885056, 0.3530559997133364547 ) ) ;
#20240 = ORIENTED_EDGE ( 'NONE', *, *, #42687, .F. ) ;
#20241 = CARTESIAN_POINT ( 'NONE',  ( -1.338582677165353729, -0.1870078740157479769, 0.4822834645669291653 ) ) ;
#20242 = CARTESIAN_POINT ( 'NONE',  ( -0.5774278215223089816, 0.1283753931104746893, -0.1820866141732285504 ) ) ;
#20243 = CARTESIAN_POINT ( 'NONE',  ( -0.01968503937007793844, -0.5400638737290844871, 0.3530559997133364547 ) ) ;
#20244 = CARTESIAN_POINT ( 'NONE',  ( -1.174540682414697335, -0.3162353388693409650, -0.4822834645669289433 ) ) ;
#20245 = CARTESIAN_POINT ( 'NONE',  ( -0.8661417322834640276, -0.1870078740157479769, 0.4822834645669291653 ) ) ;
#20246 = CARTESIAN_POINT ( 'NONE',  ( -3.937007874015748143, 2.755905511811024056, -0.5314960629921260393 ) ) ;
#20248 = CARTESIAN_POINT ( 'NONE',  ( 0.7677165354330716118, -0.5400638737290844871, 0.3530559997133364547 ) ) ;
#20247 = CARTESIAN_POINT ( 'NONE',  ( 0.4531182788721080934, 1.535433070866141447, -0.5309055118110237448 ) ) ;
#20249 = CARTESIAN_POINT ( 'NONE',  ( 1.095800524934383846, -0.05778040916215560624, -0.4822834645669293319 ) ) ;
#20250 = CARTESIAN_POINT ( 'NONE',  ( -0.1049643490035307020, 0.3917322834645669549, -2.675853018372703396 ) ) ;
#20251 = CARTESIAN_POINT ( 'NONE',  ( -1.509186351706035767, -0.4281496062992124485, 0.4176697321401328655 ) ) ;
#20252 = CARTESIAN_POINT ( 'NONE',  ( -1.430446194225721390, -0.4281496062992124485, 0.4176697321401328655 ) ) ;
#20253 = CARTESIAN_POINT ( 'NONE',  ( 0.4724409448818898682, 2.892866454678787531E-17, -0.7480314960629921295 ) ) ;
#20254 = CARTESIAN_POINT ( 'NONE',  ( -0.3460692066303958092, -0.1998031496062994683, 0.1049868766404199322 ) ) ;
#20255 = ORIENTED_EDGE ( 'NONE', *, *, #29420, .F. ) ;
#20256 = CARTESIAN_POINT ( 'NONE',  ( -0.01312335958005186876, -0.004921259842519870586, -0.3153832671262229437 ) ) ;
#20257 = CARTESIAN_POINT ( 'NONE',  ( -0.1958661417322836718, 0.3392501089628017219, -1.737532808398950079 ) ) ;
#20258 = EDGE_LOOP ( 'NONE', ( #24520, #62297, #2814, #24886 ) ) ;
#20259 = CARTESIAN_POINT ( 'NONE',  ( 0.09186351706036799403, -0.4281496062992127816, -0.4176697321401328100 ) ) ;
#20260 = CARTESIAN_POINT ( 'NONE',  ( -0.1049868766404193215, 0.2306618581243847221, -0.2411417322834647770 ) ) ;
#20261 = CARTESIAN_POINT ( 'NONE',  ( 0.07128922432405689069, 0.3857547143408421864, -2.755905511811022279 ) ) ;
#20262 = CARTESIAN_POINT ( 'NONE',  ( -0.9055118110236215490, -0.5511811023622047445, 6.969142054262312111E-17 ) ) ;
#20263 =( LENGTH_UNIT ( ) NAMED_UNIT ( * ) SI_UNIT ( $, .METRE. ) );
#20264 = CARTESIAN_POINT ( 'NONE',  ( 0.8923884514435703741, 0.2306618581243848609, 0.2411417322834645549 ) ) ;
#20265 = CARTESIAN_POINT ( 'NONE',  ( 0.9711286089238851948, 0.1283753931104748280, 0.1820866141732283561 ) ) ;
#20266 = CARTESIAN_POINT ( 'NONE',  ( -0.4396325459317577122, -0.6692913385826773087, -0.1292274648535924053 ) ) ;
#20267 = CARTESIAN_POINT ( 'NONE',  ( 0.1049643490035303689, 0.3917322834645668994, -1.018353387630234419 ) ) ;
#20268 = CARTESIAN_POINT ( 'NONE',  ( -0.7611548556430438595, -0.6046776061558809534, -0.2411417322834644161 ) ) ;
#20269 = CARTESIAN_POINT ( 'NONE',  ( -1.620734908136482577, -0.5511811023622048555, -0.09757992244046775898 ) ) ;
#20270 = CARTESIAN_POINT ( 'NONE',  ( 1.148293963254593875, -0.6692913385826771977, 0.1292274648535927661 ) ) ;
#20271 = CARTESIAN_POINT ( 'NONE',  ( 1.568241469816273659, -0.08942795157528024563, -0.3641732283464568787 ) ) ;
#20272 = ORIENTED_EDGE ( 'NONE', *, *, #75879, .F. ) ;
#20273 = CARTESIAN_POINT ( 'NONE',  ( 0.3392501089628018884, -0.1958661417322833942, -2.621410391897324832 ) ) ;
#20274 = CARTESIAN_POINT ( 'NONE',  ( 0.05249343832021075018, -0.6046776061558807314, 0.2411417322834647770 ) ) ;
#20275 = ORIENTED_EDGE ( 'NONE', *, *, #55345, .T. ) ;
#20276 = CARTESIAN_POINT ( 'NONE',  ( -0.8005249343832013809, -0.4281496062992124485, 0.4176697321401328655 ) ) ;
#20277 = CARTESIAN_POINT ( 'NONE',  ( 1.371391076115485719, -0.6692913385826773087, -0.1292274648535924053 ) ) ;
#20278 = CARTESIAN_POINT ( 'NONE',  ( 1.397637795275591177, -0.5400638737290844871, 0.3530559997133364547 ) ) ;
#20279 =( BOUNDED_CURVE ( )  B_SPLINE_CURVE ( 2, ( #75878, #77961, #20711, #65336, #45096, #19874, #520, #64480, #79220, #77539, #21124, #58151, #7240 ),
 .UNSPECIFIED., .F., .F. ) 
 B_SPLINE_CURVE_WITH_KNOTS ( ( 3, 2, 2, 2, 2, 2, 3 ),
 ( 0.4013059932978690347, 0.4015151515151514916, 0.4053030303030302761, 0.4090909090909091161, 0.4128787878787879007, 0.4166666666666666852, 0.4168758248839491420 ),
 .UNSPECIFIED. ) 
 CURVE ( )  GEOMETRIC_REPRESENTATION_ITEM ( )  RATIONAL_B_SPLINE_CURVE ( ( 0.9964447847208428577, 0.9981185001348096275, 1.000000000000000000, 0.9659258262890683122, 1.000000000000000000, 0.9659258262890683122, 1.000000000000000000, 0.9659258262890683122, 1.000000000000000000, 0.9659258262890683122, 1.000000000000000000, 0.9981185001348097385, 0.9964447847208430797 ) ) 
 REPRESENTATION_ITEM ( '' )  );
#20280 = CARTESIAN_POINT ( 'NONE',  ( 0.2362204724409456558, -0.1870078740157480879, -0.4822834645669291653 ) ) ;
#20281 = CARTESIAN_POINT ( 'NONE',  ( -0.1771653543307080136, 0.1660481256975883668, -0.3530559997133364547 ) ) ;
#20282 = CARTESIAN_POINT ( 'NONE',  ( 0.3392501089628018329, 0.1958661417322835607, -1.790682414698162805 ) ) ;
#20283 = CARTESIAN_POINT ( 'NONE',  ( -1.089238845144356427, 0.05413385826771666132, 0.4176697321401328100 ) ) ;
#20284 = CARTESIAN_POINT ( 'NONE',  ( -0.1312335958005241554, -0.6046776061558809534, -0.2411417322834644161 ) ) ;
#20285 = CARTESIAN_POINT ( 'NONE',  ( -0.3083989501312330295, -0.2845877964562161244, -0.3641732283464567121 ) ) ;
#20286 = CARTESIAN_POINT ( 'NONE',  ( 1.141392835773559211, 1.299212598425196985, 0.9642274814428540841 ) ) ;
#20287 = AXIS2_PLACEMENT_3D ( 'NONE', #76563, #37834, #18891 ) ;
#20288 = CARTESIAN_POINT ( 'NONE',  ( 1.305774278215223960, -0.6692913385826771977, 0.1292274648535927661 ) ) ;
#20289 = CARTESIAN_POINT ( 'NONE',  ( -0.5118110236220466680, -0.6692913385826771977, 8.415575281601705876E-17 ) ) ;
#20290 = CARTESIAN_POINT ( 'NONE',  ( 0.4359958488159816348, 1.724409448818897905, -2.630268417803909298 ) ) ;
#20291 = EDGE_CURVE ( 'NONE', #23282, #4461, #58471, .T. ) ;
#20292 = CARTESIAN_POINT ( 'NONE',  ( 1.272965879265092637, 0.05413385826771666132, 0.4176697321401328100 ) ) ;
#20293 = CARTESIAN_POINT ( 'NONE',  ( 3.912467585512841239, 1.355617292003078012, -0.4390143889087900209 ) ) ;
#20294 = ORIENTED_EDGE ( 'NONE', *, *, #60874, .T. ) ;
#20295 = CARTESIAN_POINT ( 'NONE',  ( 0.1902887139107617975, -0.6692913385826773087, -0.1292274648535924053 ) ) ;
#20296 = CARTESIAN_POINT ( 'NONE',  ( -0.2690288713910754526, 0.1771653543307087075, -0.09757992244046823083 ) ) ;
#20298 = DIRECTION ( 'NONE',  ( 1.000000000000000000, -0.000000000000000000, -0.000000000000000000 ) ) ;
#20297 = CARTESIAN_POINT ( 'NONE',  ( 0.9580052493438327987, -0.3690944881889765550, -0.3153832671262227771 ) ) ;
#20299 = CARTESIAN_POINT ( 'NONE',  ( 0.3458507752293908943, 0.3458507752293908943, -0.3720472440944882497 ) ) ;
#20300 = CARTESIAN_POINT ( 'NONE',  ( 1.653543307086614789, -0.1870078740157479769, 0.3641732283464567677 ) ) ;
#20301 = CARTESIAN_POINT ( 'NONE',  ( 1.430446194225722500, 0.05413385826771666132, 0.4176697321401328100 ) ) ;
#20302 = CARTESIAN_POINT ( 'NONE',  ( 0.3949938075777409408, -0.1058382717557499186, -0.03083989501312336609 ) ) ;
#20303 = CARTESIAN_POINT ( 'NONE',  ( 0.1509186351706042484, -0.3162353388693405765, 0.4822834645669290543 ) ) ;
#20304 = CARTESIAN_POINT ( 'NONE',  ( -1.607611548556429737, 0.2952755905511810774, -0.1292274648535930714 ) ) ;
#20305 = CARTESIAN_POINT ( 'NONE',  ( 1.581364829396326277, -0.08942795157527998196, 0.3641732283464567121 ) ) ;
#20306 = CARTESIAN_POINT ( 'NONE',  ( -0.07217847769028813698, -0.3162353388693409650, -0.4822834645669289433 ) ) ;
#20307 = CARTESIAN_POINT ( 'NONE',  ( 0.3949938075777409408, -0.1058382717557499186, -0.03083989501312336609 ) ) ;
#20308 = CARTESIAN_POINT ( 'NONE',  ( -1.601049868766403650, 0.1283753931104746893, -0.1820866141732285504 ) ) ;
#20309 = CARTESIAN_POINT ( 'NONE',  ( 0.5905511811023629321, -0.6692913385826771977, 8.415575281601705876E-17 ) ) ;
#20310 = CARTESIAN_POINT ( 'NONE',  ( 1.076115485564305141, 0.1283753931104746893, -0.1820866141732285504 ) ) ;
#20311 = CARTESIAN_POINT ( 'NONE',  ( -0.01312335958005186876, 0.05413385826771626580, -0.4176697321401330321 ) ) ;
#20312 = CARTESIAN_POINT ( 'NONE',  ( 0.7808398950131241190, -0.08942795157528024563, -0.3641732283464568787 ) ) ;
#20313 = CARTESIAN_POINT ( 'NONE',  ( -1.364829396325458521, -0.6046776061558807314, 0.2411417322834647770 ) ) ;
#20314 = CARTESIAN_POINT ( 'NONE',  ( 0.1070741851644053388, 0.3996062992125986035, -0.7001312335958002064 ) ) ;
#20315 = CARTESIAN_POINT ( 'NONE',  ( 1.043307086614173818, 0.1660481256975885056, 0.3530559997133364547 ) ) ;
#20316 = CARTESIAN_POINT ( 'NONE',  ( -0.3917322834645669549, -0.1049643490035306603, -0.8254593175853015552 ) ) ;
#20318 = CARTESIAN_POINT ( 'NONE',  ( 0.9251968503937014754, 0.1660481256975883391, -0.3530559997133364547 ) ) ;
#20317 = CARTESIAN_POINT ( 'NONE',  ( 0.8989501312335964611, 0.2952755905511811885, 0.1292274648535926551 ) ) ;
#20319 = CARTESIAN_POINT ( 'NONE',  ( -0.3477690288713902178, 0.2066929133858267098, -0.1054918080437494132 ) ) ;
#20320 = CARTESIAN_POINT ( 'NONE',  ( 0.4658792650918640033, -0.2845877964562159024, 0.3641732283464567677 ) ) ;
#20321 = CARTESIAN_POINT ( 'NONE',  ( 0.6430446194225729606, -0.4281496062992127816, -0.4176697321401328100 ) ) ;
#20322 = CARTESIAN_POINT ( 'NONE',  ( -0.2491186766705762723, 0.1588297147721999536, 0.1541304905092664712 ) ) ;
#20323 = CARTESIAN_POINT ( 'NONE',  ( -0.8923884514435688198, 0.1283753931104746893, -0.1820866141732285504 ) ) ;
#20324 = CARTESIAN_POINT ( 'NONE',  ( -1.167979002624671470, -0.4281496062992127816, -0.4176697321401328100 ) ) ;
#20325 = CARTESIAN_POINT ( 'NONE',  ( -1.561679790026246017, 0.05413385826771666132, 0.4176697321401328100 ) ) ;
#20326 = VECTOR ( 'NONE', #13001, 39.37007874015748143 ) ;
#20327 = CARTESIAN_POINT ( 'NONE',  ( 1.148293963254593875, -0.6692913385826771977, 0.1292274648535927661 ) ) ;
#20328 = CARTESIAN_POINT ( 'NONE',  ( -1.646981627296586703, -0.08942795157527998196, 0.3641732283464567121 ) ) ;
#20329 = CARTESIAN_POINT ( 'NONE',  ( -0.3977953519386773773, -0.03143970413924696006, -1.220472440944937897 ) ) ;
#20330 = CARTESIAN_POINT ( 'NONE',  ( 0.8202099737532813073, 0.2952755905511811885, 0.1292274648535926551 ) ) ;
#20331 = CARTESIAN_POINT ( 'NONE',  ( 0.2925321140481932369, -0.2925321140481931814, 0.1397637795275590289 ) ) ;
#20332 = CARTESIAN_POINT ( 'NONE',  ( 1.692913385826772421, 0.2952755905511811885, 0.000000000000000000 ) ) ;
#20333 = CARTESIAN_POINT ( 'NONE',  ( 1.417322834645670104, -0.1870078740157480879, -0.4822834645669291653 ) ) ;
#20334 = CARTESIAN_POINT ( 'NONE',  ( -1.312335958005248715, -0.5023911411419708095, -0.1820866141732282451 ) ) ;
#20335 = CARTESIAN_POINT ( 'NONE',  ( 1.207349081364829990, 0.1283753931104748280, 0.1820866141732283561 ) ) ;
#20336 = CARTESIAN_POINT ( 'NONE',  ( -1.194225721784776262, -0.3690944881889763329, 0.3153832671262228327 ) ) ;
#20337 = CARTESIAN_POINT ( 'NONE',  ( -0.3412073490813641308, 0.1283753931104746893, -0.1820866141732285504 ) ) ;
#20338 = PLANE ( 'NONE',  #54696 ) ;
#20339 = CARTESIAN_POINT ( 'NONE',  ( 1.108923884514436242, -0.08942795157527998196, 0.3641732283464567121 ) ) ;
#20340 = CARTESIAN_POINT ( 'NONE',  ( 0.7152230971128616943, -0.05778040916215522460, 0.4822834645669289988 ) ) ;
#20341 = CARTESIAN_POINT ( 'NONE',  ( 1.154855643044620184, 0.2306618581243847221, -0.2411417322834647770 ) ) ;
#20342 = CARTESIAN_POINT ( 'NONE',  ( -0.1181102362204717315, -0.6692913385826771977, 8.415575281601705876E-17 ) ) ;
#20343 = VECTOR ( 'NONE', #40496, 39.37007874015748143 ) ;
#20344 = CARTESIAN_POINT ( 'NONE',  ( 0.6430446194225728496, -0.004921259842519576551, 0.3153832671262227771 ) ) ;
#20345 = CARTESIAN_POINT ( 'NONE',  ( 1.240157480314961314, -0.5400638737290844871, 0.3530559997133364547 ) ) ;
#20346 = CARTESIAN_POINT ( 'NONE',  ( -1.640419947506561060, 0.05413385826771666132, 0.4176697321401328100 ) ) ;
#20347 = CARTESIAN_POINT ( 'NONE',  ( -0.5052493438320203589, -0.6692913385826771977, 0.1292274648535927661 ) ) ;
#20348 = CARTESIAN_POINT ( 'NONE',  ( 0.3460692066303959757, -0.1998031496062991907, -0.5774278215223097588 ) ) ;
#20349 = CARTESIAN_POINT ( 'NONE',  ( -0.4724409448818917001, 0.1265901696524956710, -1.211942257217847985 ) ) ;
#20350 = CARTESIAN_POINT ( 'NONE',  ( 0.02624671916010564918, 0.2306618581243848609, 0.2411417322834645549 ) ) ;
#20351 = CARTESIAN_POINT ( 'NONE',  ( -0.4461942257217840213, -0.6046776061558809534, -0.2411417322834644161 ) ) ;
#20352 = CARTESIAN_POINT ( 'NONE',  ( 0.1115485564304467270, -0.6692913385826773087, -0.1292274648535924053 ) ) ;
#20353 = EDGE_CURVE ( 'NONE', #49008, #14378, #70690, .T. ) ;
#20354 = CARTESIAN_POINT ( 'NONE',  ( 0.3996062992125986035, 0.1070741851644054776, -2.486876640419947382 ) ) ;
#20355 = CARTESIAN_POINT ( 'NONE',  ( -0.1058382717557497937, -0.3949938075777411628, -1.961942257217847763 ) ) ;
#20356 = CARTESIAN_POINT ( 'NONE',  ( -0.1958661417322834220, -0.3392501089628018884, -0.6876640419947506189 ) ) ;
#20357 = CARTESIAN_POINT ( 'NONE',  ( 0.2371566215357294449, -0.1759343135753352327, 5.725906639596368919 ) ) ;
#20358 = CARTESIAN_POINT ( 'NONE',  ( -0.3917322834645670104, -7.196005306013484475E-17, -1.133858267716535195 ) ) ;
#20359 = EDGE_CURVE ( 'NONE', #45388, #70359, #33234, .T. ) ;
#20360 = CARTESIAN_POINT ( 'NONE',  ( -0.7611548556430438595, 0.1283753931104748280, 0.1820866141732283561 ) ) ;
#20361 = CARTESIAN_POINT ( 'NONE',  ( 0.2867679344610365999, -0.2867679344610365444, -1.192913385826771755 ) ) ;
#20362 = CARTESIAN_POINT ( 'NONE',  ( -1.345144356955379816, -0.05778040916215560624, -0.4822834645669293319 ) ) ;
#20363 = CARTESIAN_POINT ( 'NONE',  ( -9.594673741351310580E-17, 0.3917322834645669549, 0.2349274522647787078 ) ) ;
#20364 = CARTESIAN_POINT ( 'NONE',  ( 0.4527559055118117182, 0.1660481256975883668, -0.3530559997133364547 ) ) ;
#20365 = CARTESIAN_POINT ( 'NONE',  ( -0.5905511811023615998, 0.1771653543307087630, 0.000000000000000000 ) ) ;
#20366 = CARTESIAN_POINT ( 'NONE',  ( 1.102362204724410155, -0.1870078740157479769, 0.4822834645669291653 ) ) ;
#20367 = CARTESIAN_POINT ( 'NONE',  ( 0.3608923884514443348, 0.2952755905511810774, -0.1292274648535930714 ) ) ;
#20368 = CARTESIAN_POINT ( 'NONE',  ( 0.4620977091643874712, 1.428887118379093435, 1.022480879491282968 ) ) ;
#20369 = CARTESIAN_POINT ( 'NONE',  ( -0.1070741851644051862, -0.3996062992125987146, -2.591863517060367439 ) ) ;
#20370 = CARTESIAN_POINT ( 'NONE',  ( 0.3917322834645670659, -0.1049643490035303273, -1.368129552002311788 ) ) ;
#20371 = CARTESIAN_POINT ( 'NONE',  ( 1.266404199475066328, -0.3162353388693409650, -0.4822834645669289433 ) ) ;
#20372 = CARTESIAN_POINT ( 'NONE',  ( 0.2887139107611556010, -0.6046776061558807314, 0.2411417322834647770 ) ) ;
#20373 = CARTESIAN_POINT ( 'NONE',  ( 0.05905511811023681640, 0.1660481256975883668, -0.3530559997133364547 ) ) ;
#20374 = CARTESIAN_POINT ( 'NONE',  ( -1.646981627296586703, -0.05778040916215522460, 0.4822834645669289988 ) ) ;
#20375 = CARTESIAN_POINT ( 'NONE',  ( 0.7677165354330716118, 0.1660481256975883668, -0.3530559997133364547 ) ) ;
#20376 = CARTESIAN_POINT ( 'NONE',  ( 0.3917322834645670104, -0.1049643490035303411, -0.6686351706036747222 ) ) ;
#20377 = CARTESIAN_POINT ( 'NONE',  ( -0.01968503937007793844, -0.5400638737290844871, 0.3530559997133364547 ) ) ;
#20378 = CARTESIAN_POINT ( 'NONE',  ( 1.089238845144357759, 0.05413385826771626580, -0.4176697321401330321 ) ) ;
#20379 = CARTESIAN_POINT ( 'NONE',  ( 0.5249343832021005074, -0.6046776061558807314, 0.2411417322834647770 ) ) ;
#20380 = CARTESIAN_POINT ( 'NONE',  ( 0.9711286089238851948, -0.5023911411419708095, -0.1820866141732282451 ) ) ;
#20381 = CARTESIAN_POINT ( 'NONE',  ( -0.9317585301837263412, 0.05413385826771666132, 0.4176697321401328100 ) ) ;
#20382 = CARTESIAN_POINT ( 'NONE',  ( -1.437007874015747477, -0.5400638737290844871, 0.3530559997133364547 ) ) ;
#20383 = AXIS2_PLACEMENT_3D ( 'NONE', #23804, #12012, #70066 ) ;
#20384 = CARTESIAN_POINT ( 'NONE',  ( 0.7808398950131240079, -0.3162353388693405765, 0.4822834645669290543 ) ) ;
#20385 = DIRECTION ( 'NONE',  ( 0.000000000000000000, 0.000000000000000000, -1.000000000000000000 ) ) ;
#20386 = CARTESIAN_POINT ( 'NONE',  ( -0.3392501089628019995, 0.1958661417322832277, -2.065616797900262647 ) ) ;
#20387 = ORIENTED_EDGE ( 'NONE', *, *, #53209, .T. ) ;
#20388 = CARTESIAN_POINT ( 'NONE',  ( -9.787531504996567848E-17, 0.3996062992125986035, -0.1574803149606299746 ) ) ;
#20389 = ORIENTED_EDGE ( 'NONE', *, *, #53708, .T. ) ;
#20390 = CARTESIAN_POINT ( 'NONE',  ( 1.568241469816273659, -0.05778040916215560624, -0.4822834645669293319 ) ) ;
#20391 = CARTESIAN_POINT ( 'NONE',  ( 0.8858267716535438430, -0.4536011799217368745, -0.2665933059059886201 ) ) ;
#20392 = LINE ( 'NONE', #33849, #7510 ) ;
#20393 = CARTESIAN_POINT ( 'NONE',  ( -0.1179898944395515598, 1.077592634160693841, 2.860510421453457575 ) ) ;
#20394 = DIRECTION ( 'NONE',  ( 0.000000000000000000, 0.000000000000000000, 1.000000000000000000 ) ) ;
#20395 = CARTESIAN_POINT ( 'NONE',  ( 0.3392501089628018329, 0.1958661417322835607, -0.8458005249343831800 ) ) ;
#20396 = EDGE_CURVE ( 'NONE', #31638, #7519, #45830, .T. ) ;
#20397 = CARTESIAN_POINT ( 'NONE',  ( -1.036745406824146176, -0.3690944881889763329, 0.3153832671262228327 ) ) ;
#20398 = CARTESIAN_POINT ( 'NONE',  ( 1.568241469816273437, -0.3162353388693405765, 0.4822834645669290543 ) ) ;
#20399 = CARTESIAN_POINT ( 'NONE',  ( -1.541994750656167090, -0.6692913385826773087, -0.1292274648535924053 ) ) ;
#20400 = CARTESIAN_POINT ( 'NONE',  ( -0.3083989501312330295, -0.05778040916215522460, 0.4822834645669289988 ) ) ;
#20401 = CARTESIAN_POINT ( 'NONE',  ( 1.122047244094488860, 0.1660481256975885056, 0.3530559997133364547 ) ) ;
#20402 = VERTEX_POINT ( 'NONE', #58896 ) ;
#20403 = CARTESIAN_POINT ( 'NONE',  ( -1.410761154855642463, -0.05778040916215522460, 0.4822834645669289988 ) ) ;
#20404 = CARTESIAN_POINT ( 'NONE',  ( 0.4849061582275022153, 1.568468489416427580, 0.4921425059946342717 ) ) ;
#20405 = DIRECTION ( 'NONE',  ( 0.000000000000000000, 0.000000000000000000, 1.000000000000000000 ) ) ;
#20406 = DIRECTION ( 'NONE',  ( -0.000000000000000000, -1.000000000000000000, -0.000000000000000000 ) ) ;
#20407 = CARTESIAN_POINT ( 'NONE',  ( 1.603475055217291612, 1.267857067133554061, -0.04573490813648243419 ) ) ;
#20408 = CARTESIAN_POINT ( 'NONE',  ( -0.7414698162729651543, -0.5511811023622046335, 0.09757992244046803654 ) ) ;
#20409 =( BOUNDED_SURFACE ( )  B_SPLINE_SURFACE ( 1, 2, ( 
 ( #74889, #36559, #10901, #62236, #31479, #76529, #71457, #19263, #26833, #13384, #1182, #39463, #57140, #52491, #39037, #63881, #83248, #38207, #78200, #33156, #50827, #25571, #757, #13805, #77354, #32730, #6220, #64721, #31896, #25159, #12549, #26418, #12968, #58397, #19686, #18857, #38625, #63474, #52071, #82837, #20530, #5809, #14228, #58825, #57971, #77778, #44505, #46182, #337, #71879, #70194, #57557, #51236, #7061, #76935, #44916, #70613, #64303, #20111, #45759, #65150, #6637, #32309, #71040, #25992, #51650, #45344, #7486, #41542, #15053, #60070, #52907, #33570, #2425, #22187, #59647, #46602, #34826, #35231, #79870, #73121, #21766, #53331, #14644, #34402, #79040, #15472, #47429, #53739, #2003, #40709, #27248, #54573, #21359, #60483, #47012, #65575, #41129, #66820, #28081, #33985, #7909, #2834, #54155, #47844, #60895, #72706, #9561, #3246, #80287, #67231, #28495, #9153, #27665, #1593, #78621, #66394, #8732, #48261, #28910, #73957, #73550, #79447, #20944, #15893, #22600, #39888, #59232, #72298, #40300, #65981, #8319, #3663, #82333, #75609, #69286, #74371, #74785, #5306, #80695, #9975, #24651, #4476, #17540, #37293, #30146, #81102, #4890, #55807, #50319, #30965, #29326, #81928, #62136, #62555, #43172, #23008, #42355, #61729, #30565, #48675, #49503, #56230, #11633, #24239, #16715, #4066, #11217, #49912, #62968, #41946, #17948, #16304, #68053, #54987, #42768, #49085, #17136, #43585, #56632, #81514, #23835, #67642, #75196, #10400, #68464, #35645, #68868, #36877, #36462, #61305, #36057, #29733, #55395, #23419, #10802, #63370, #234, #57041, #58287, #39354, #45656, #26730, #70092, #6539, #57868, #1077, #76428, #652, #13284, #12446, #5704, #82735, #58712, #25054, #32209, #25886, #44400, #51546, #13698, #70507, #33043, #38105, #12865, #31792, #51134, #38522, #38936, #31376, #71352, #64205, #65038, #76016, #69695, #12038, #77250, #50729, #18358, #44002, #37695, #19579, #64617, #51967, #18756, #63781, #45239, #6120, #57455, #76829, #7375, #77675, #19161, #70939, #83148, #25468, #6954, #26309, #44811, #32624, #20005, #47740, #9046, #2318, #34301, #65880, #27142, #46908, #8216, #27978, #59962, #66291, #14545, #27562, #39776, #67124, #33880, #47324, #59546, #78093, #53637, #3144, #2730, #8630, #1901, #46077, #53221, #66713, #78931, #35127, #54050, #52806, #9454, #79344, #73015, #78516, #20424, #59131, #40197, #34721, #60381, #15788, #14123, #21254, #72603, #33469, #28391, #15366, #1489, #60791, #79764, #7804, #14950, #20840, #22081, #71770, #65470, #73438, #40608, #41440, #21665, #52384, #46492, #72188, #41027, #4376, #29224, #48572, #3559, #17850, #81830, #16198, #74269, #49402, #62448, #42671, #81415, #54891, #30044, #80596, #73857, #61202, #75096, #61629, #23731, #68370, #41845, #3971, #28807, #17444, #80184, #75511, #54471, #62868, #24140, #11531, #9872, #10708, #62039, #22904, #55706, #49810, #23318, #69180, #16613, #48988, #67950, #29634, #43074, #74686, #42255, #22499, #68771, #11115, #36772, #43484, #10293, #37188, #48162, #67535, #30461, #4784, #36364, #35960, #35541, #55295, #81004, #17032, #56124, #51873, #39257, #38424, #57353, #69595, #83049, #19911, #76331, #57771, #12767, #70842, #63269, #25372, #75917, #71257, #64519, #58190, #5610, #63685, #77579, #11942, #82236, #13603, #76735, #6441, #26211, #19066, #69996, #77153, #44714, #5204, #45561, #18256, #13191, #51035, #51450, #32113, #37596, #31278, #50626, #19485, #56943, #64106, #45138, #558, #38840, #82640, #18661, #133, #6856, #30868, #56533, #32526, #24555, #24953, #43898, #31694, #38007, #6023, #50221, #44306, #70411, #25789, #12351, #46817, #65374, #65789, #35753, #78835, #34203, #1804, #23117, #64939, #29433, #55091, #48785, #78420, #52292, #72508, #45978, #48367, #80800, #61419, #16829, #59040, #21161, #14857, #74482, #7709, #74066, #2219, #1394, #77997, #71674, #27885, #27048, #20325, #14025, #7279, #39682, #40518, #66198, #33376, #8536, #3769, #59451, #32949, #52708, #27466, #20748, #40101, #59866, #53124, #46398, #58615, #53545, #79253, #21568, #982, #72091, #26638, #14450, #8122 ),
 ( #33787, #16412, #42059, #67754, #10088, #24757, #17245, #62665, #29839, #25169, #18467, #12149, #42874, #17647, #31488, #23526, #36161, #50838, #30675, #43690, #63484, #56336, #23941, #31074, #82035, #76538, #57149, #55503, #50425, #5005, #5412, #69395, #49196, #68567, #4582, #56742, #74897, #75717, #82440, #37806, #76125, #10909, #30253, #37403, #44110, #5818, #68165, #69802, #42465, #36567, #81211, #68978, #75303, #43279, #82848, #10508, #24349, #50018, #61835, #18057, #62245, #11326, #4175, #11747, #63075, #55917, #81630, #49608, #36986, #7919, #59243, #32320, #6230, #26429, #83259, #1193, #65586, #71889, #52918, #12979, #32741, #767, #27258, #19274, #26842, #33580, #1602, #20542, #13816, #52080, #38635, #63892, #31906, #26004, #57982, #18866, #44515, #70202, #77789, #71051, #25581, #13395, #12559, #6647, #71468, #20122, #52501, #76947, #39048, #57567, #38217, #78210, #14240, #44926, #77365, #51245, #70623, #64313, #347, #7071, #45769, #39898, #58408, #51661, #7498, #39475, #19697, #45354, #64733, #46194, #65162, #33167, #58835, #2014, #21370, #40720, #41552, #59658, #28508, #67240, #48270, #3257, #27678, #66406, #73559, #60905, #73968, #20956, #28918, #78632, #47025, #8330, #21777, #28094, #53750, #80296, #16313, #34835, #60495, #9571, #2844, #79053, #79460, #41958, #9163, #47854, #15483, #35654, #46614, #67651, #9988, #61317, #8743, #65992, #54165, #53343, #54586, #3672, #29335, #72309, #72717, #79880, #22197, #14656, #15064, #22610, #15903, #34414, #33996, #60082, #40313, #2436, #35241, #47439, #73133, #41140, #66830, #49512, #12048, #17145, #75205, #10811, #30155, #56240, #17549, #49094, #80704, #49921, #69296, #11645, #76026, #36471, #24660, #37303, #62977, #18371, #62146, #50329, #44011, #37706, #56641, #75619, #36888, #74798, #16725, #42366, #4487, #68473, #63379, #69705, #5715, #4903, #23845, #36066, #43181, #54996, #42777, #24248, #62564, #5316, #29742, #68878, #68065, #23018, #30974, #48685, #55406, #55817, #74382, #61738, #10409, #4075, #11227, #81937, #81112, #30574, #81525, #43594, #17957, #23430, #82342, #44409, #13710, #77260, #77685, #58298, #38116, #57464, #76838, #20015, #12455, #64628, #45666, #1088, #39364, #63791, #19172, #26319, #65049, #26740, #57051, #7387, #31385, #83158, #70103, #57877, #64214, #6548, #33054, #52394, #70948, #13293, #71362, #38945, #31804, #32219, #78103, #45251, #664, #51556, #71780, #82744, #20434, #46088, #14135, #44820, #18766, #6964, #6129, #58725, #39787, #65482, #25065, #25477, #32635, #51980, #50739, #51144, #76437, #70518, #12874, #38533, #244, #25896, #19589, #21675, #41038, #59556, #66723, #28818, #2332, #48173, #53231, #27988, #46920, #66301, #9060, #53648, #1911, #33480, #2743, #34732, #14556, #7814, #41856, #52816, #60392, #28403, #67136, #72203, #27574, #15376, #40208, #46503, #8640, #22512, #9465, #34312, #79356, #20851, #1500, #47336, #73451, #78947, #65891, #54061, #3155, #47753, #79776, #73026, #21265, #8226, #22092, #72613, #15801, #41452, #35139, #14961, #59973, #78527, #73869, #40618, #60801, #54483, #59142, #80194, #27152, #16209, #33890, #74699, #61215, #17044, #81843, #10721, #50234, #69196, #67964, #82249, #49417, #62462, #10306, #9883, #74281, #29647, #49824, #75524, #30881, #29237, #55309, #42684, #48584, #17863, #4797, #16625, #75930, #43498, #22917, #68382, #42267, #11545, #35552, #80607, #37201, #23330, #56548, #17457, #5217, #62882, #3570, #24567, #43087, #35972, #3983, #61642, #18271, #67548, #54901, #81017, #30474, #49000, #81429, #36786, #36378, #68784, #62052, #4390, #30058, #56138, #55719, #24154, #23744, #75111, #11128, #43911, #64532, #11955, #7291, #69609, #78010, #39269, #38437, #6869, #82653, #13615, #64120, #64951, #37610, #63285, #5625, #77165, #32538, #19925, #24968, #38022, #51463, #50640, #76344, #44727, #58628, #45575, #19079, #6455, #56956, #31291, #32125, #26223, #63698, #18674, #38852, #32961, #570, #19497, #25802, #57369, #44319, #57783, #83064, #45151, #70854, #147, #6037, #70424, #70009, #996, #25385, #58202, #51048, #12364, #13205, #31709, #77591 ) ),
 .UNSPECIFIED., .F., .F., .F. ) 
 B_SPLINE_SURFACE_WITH_KNOTS ( ( 2, 2 ),
 ( 3, 2, 2, 2, 2, 2, 2, 2, 2, 2, 2, 2, 2, 2, 2, 2, 2, 2, 2, 2, 2, 2, 2, 2, 2, 2, 2, 2, 2, 2, 2, 2, 2, 2, 2, 2, 2, 2, 2, 2, 2, 2, 2, 2, 2, 2, 2, 2, 2, 2, 2, 2, 2, 2, 2, 2, 2, 2, 2, 2, 2, 2, 2, 2, 2, 2, 2, 2, 2, 2, 2, 2, 2, 2, 2, 2, 2, 2, 2, 2, 2, 2, 2, 2, 2, 2, 2, 2, 2, 2, 2, 2, 2, 2, 2, 2, 2, 2, 2, 2, 2, 2, 2, 2, 2, 2, 2, 2, 2, 2, 2, 2, 2, 2, 2, 2, 2, 2, 2, 2, 2, 2, 2, 2, 2, 2, 2, 2, 2, 2, 2, 2, 2, 2, 2, 2, 2, 2, 2, 2, 2, 2, 2, 2, 2, 2, 2, 2, 2, 2, 2, 2, 2, 2, 2, 2, 2, 2, 2, 2, 2, 2, 2, 2, 2, 2, 2, 2, 2, 2, 2, 2, 2, 2, 2, 2, 2, 2, 2, 2, 2, 2, 2, 2, 2, 2, 2, 2, 2, 2, 2, 2, 2, 2, 2, 2, 2, 2, 2, 2, 2, 2, 2, 2, 2, 2, 2, 2, 2, 2, 2, 2, 2, 2, 2, 2, 2, 2, 2, 2, 2, 2, 2, 2, 2, 2, 2, 2, 2, 2, 2, 2, 2, 2, 2, 2, 2, 2, 2, 2, 2, 2, 2, 2, 2, 2, 2, 2, 2, 2, 2, 2, 2, 2, 2, 3 ),
 ( 0.000000000000000000, 1.000000000000000000 ),
 ( 0.000000000000000000, 0.003787878787878787984, 0.007575757575757575968, 0.01136363636363636395, 0.01515151515151515194, 0.01893939393939393992, 0.02272727272727272790, 0.02651515151515151589, 0.03030303030303030387, 0.03409090909090908839, 0.03787878787878787984, 0.04166666666666666435, 0.04545454545454545581, 0.04924242424242424032, 0.05303030303030303177, 0.05681818181818181629, 0.06060606060606060774, 0.06439393939393939226, 0.06818181818181817677, 0.07196969696969697516, 0.07575757575757575968, 0.07954545454545454419, 0.08333333333333332871, 0.08712121212121212710, 0.09090909090909091161, 0.09469696969696969613, 0.09848484848484848064, 0.1022727272727272790, 0.1060606060606060635, 0.1098484848484848481, 0.1136363636363636326, 0.1174242424242424310, 0.1212121212121212155, 0.1250000000000000000, 0.1287878787878787845, 0.1325757575757575690, 0.1363636363636363535, 0.1401515151515151381, 0.1439393939393939503, 0.1477272727272727348, 0.1515151515151515194, 0.1553030303030303039, 0.1590909090909090884, 0.1628787878787878729, 0.1666666666666666574, 0.1704545454545454419, 0.1742424242424242542, 0.1780303030303030387, 0.1818181818181818232, 0.1856060606060606077, 0.1893939393939393923, 0.1931818181818181768, 0.1969696969696969613, 0.2007575757575757458, 0.2045454545454545581, 0.2083333333333333426, 0.2121212121212121271, 0.2159090909090909116, 0.2196969696969696961, 0.2234848484848484806, 0.2272727272727272652, 0.2310606060606060497, 0.2348484848484848619, 0.2386363636363636465, 0.2424242424242424310, 0.2462121212121212155, 0.2500000000000000000, 0.2537878787878787845, 0.2575757575757575690, 0.2613636363636363535, 0.2651515151515151381, 0.2689393939393939226, 0.2727272727272727071, 0.2765151515151514916, 0.2803030303030302761, 0.2840909090909091161, 0.2878787878787879007, 0.2916666666666666852, 0.2954545454545454697, 0.2992424242424242542, 0.3030303030303030387, 0.3068181818181818232, 0.3106060606060606077, 0.3143939393939393923, 0.3181818181818181768, 0.3219696969696969613, 0.3257575757575757458, 0.3295454545454545303, 0.3333333333333333148, 0.3371212121212120993, 0.3409090909090908839, 0.3446969696969697239, 0.3484848484848485084, 0.3522727272727272929, 0.3560606060606060774, 0.3598484848484848619, 0.3636363636363636465, 0.3674242424242424310, 0.3712121212121212155, 0.3750000000000000000, 0.3787878787878787845, 0.3825757575757575690, 0.3863636363636363535, 0.3901515151515151381, 0.3939393939393939226, 0.3977272727272727071, 0.4015151515151514916, 0.4053030303030302761, 0.4090909090909091161, 0.4128787878787879007, 0.4166666666666666852, 0.4204545454545454697, 0.4242424242424242542, 0.4280303030303030387, 0.4318181818181818232, 0.4356060606060606077, 0.4393939393939393923, 0.4431818181818181768, 0.4469696969696969613, 0.4507575757575757458, 0.4545454545454545303, 0.4583333333333333148, 0.4621212121212120993, 0.4659090909090908839, 0.4696969696969697239, 0.4734848484848485084, 0.4772727272727272929, 0.4810606060606060774, 0.4848484848484848619, 0.4886363636363636465, 0.4924242424242424310, 0.4962121212121212155, 0.5000000000000000000, 0.5037878787878787845, 0.5075757575757575690, 0.5113636363636363535, 0.5151515151515151381, 0.5189393939393939226, 0.5227272727272727071, 0.5265151515151514916, 0.5303030303030302761, 0.5340909090909090606, 0.5378787878787878451, 0.5416666666666666297, 0.5454545454545454142, 0.5492424242424241987, 0.5530303030303029832, 0.5568181818181817677, 0.5606060606060605522, 0.5643939393939394478, 0.5681818181818182323, 0.5719696969696970168, 0.5757575757575758013, 0.5795454545454545858, 0.5833333333333333703, 0.5871212121212121549, 0.5909090909090909394, 0.5946969696969697239, 0.5984848484848485084, 0.6022727272727272929, 0.6060606060606060774, 0.6098484848484848619, 0.6136363636363636465, 0.6174242424242424310, 0.6212121212121212155, 0.6250000000000000000, 0.6287878787878787845, 0.6325757575757575690, 0.6363636363636363535, 0.6401515151515151381, 0.6439393939393939226, 0.6477272727272727071, 0.6515151515151514916, 0.6553030303030302761, 0.6590909090909090606, 0.6628787878787878451, 0.6666666666666666297, 0.6704545454545454142, 0.6742424242424241987, 0.6780303030303029832, 0.6818181818181817677, 0.6856060606060605522, 0.6893939393939394478, 0.6931818181818182323, 0.6969696969696970168, 0.7007575757575758013, 0.7045454545454545858, 0.7083333333333333703, 0.7121212121212121549, 0.7159090909090909394, 0.7196969696969697239, 0.7234848484848485084, 0.7272727272727272929, 0.7310606060606060774, 0.7348484848484848619, 0.7386363636363636465, 0.7424242424242424310, 0.7462121212121212155, 0.7500000000000000000, 0.7537878787878787845, 0.7575757575757575690, 0.7613636363636363535, 0.7651515151515151381, 0.7689393939393939226, 0.7727272727272727071, 0.7765151515151514916, 0.7803030303030302761, 0.7840909090909090606, 0.7878787878787878451, 0.7916666666666666297, 0.7954545454545454142, 0.7992424242424241987, 0.8030303030303029832, 0.8068181818181817677, 0.8106060606060605522, 0.8143939393939394478, 0.8181818181818182323, 0.8219696969696970168, 0.8257575757575758013, 0.8295454545454545858, 0.8333333333333333703, 0.8371212121212121549, 0.8409090909090909394, 0.8446969696969697239, 0.8484848484848485084, 0.8522727272727272929, 0.8560606060606060774, 0.8598484848484848619, 0.8636363636363636465, 0.8674242424242424310, 0.8712121212121212155, 0.8750000000000000000, 0.8787878787878787845, 0.8825757575757575690, 0.8863636363636363535, 0.8901515151515151381, 0.8939393939393939226, 0.8977272727272727071, 0.9015151515151514916, 0.9053030303030302761, 0.9090909090909090606, 0.9128787878787878451, 0.9166666666666666297, 0.9204545454545454142, 0.9242424242424241987, 0.9280303030303029832, 0.9318181818181817677, 0.9356060606060605522, 0.9393939393939394478, 0.9431818181818182323, 0.9469696969696970168, 0.9507575757575758013, 0.9545454545454545858, 0.9583333333333333703, 0.9621212121212121549, 0.9659090909090909394 ),
 .UNSPECIFIED. ) 
 GEOMETRIC_REPRESENTATION_ITEM ( )  RATIONAL_B_SPLINE_SURFACE ( (
 ( 1.000000000000000000, 0.9659258262890683122, 1.000000000000000000, 0.9659258262890683122, 1.000000000000000000, 0.9659258262890683122, 1.000000000000000000, 0.9659258262890683122, 1.000000000000000000, 0.9659258262890683122, 1.000000000000000000, 0.9659258262890683122, 1.000000000000000000, 0.9659258262890683122, 1.000000000000000000, 0.9659258262890683122, 1.000000000000000000, 0.9659258262890683122, 1.000000000000000000, 0.9659258262890683122, 1.000000000000000000, 0.9659258262890683122, 1.000000000000000000, 0.9659258262890683122, 1.000000000000000000, 0.9659258262890683122, 1.000000000000000000, 0.9659258262890683122, 1.000000000000000000, 0.9659258262890683122, 1.000000000000000000, 0.9659258262890683122, 1.000000000000000000, 0.9659258262890683122, 1.000000000000000000, 0.9659258262890683122, 1.000000000000000000, 0.9659258262890683122, 1.000000000000000000, 0.9659258262890683122, 1.000000000000000000, 0.9659258262890683122, 1.000000000000000000, 0.9659258262890683122, 1.000000000000000000, 0.9659258262890683122, 1.000000000000000000, 0.9659258262890683122, 1.000000000000000000, 0.9659258262890683122, 1.000000000000000000, 0.9659258262890683122, 1.000000000000000000, 0.9659258262890683122, 1.000000000000000000, 0.9659258262890683122, 1.000000000000000000, 0.9659258262890683122, 1.000000000000000000, 0.9659258262890683122, 1.000000000000000000, 0.9659258262890683122, 1.000000000000000000, 0.9659258262890683122, 1.000000000000000000, 0.9659258262890683122, 1.000000000000000000, 0.9659258262890683122, 1.000000000000000000, 0.9659258262890683122, 1.000000000000000000, 0.9659258262890683122, 1.000000000000000000, 0.9659258262890683122, 1.000000000000000000, 0.9659258262890683122, 1.000000000000000000, 0.9659258262890683122, 1.000000000000000000, 0.9659258262890683122, 1.000000000000000000, 0.9659258262890683122, 1.000000000000000000, 0.9659258262890683122, 1.000000000000000000, 0.9659258262890683122, 1.000000000000000000, 0.9659258262890683122, 1.000000000000000000, 0.9659258262890683122, 1.000000000000000000, 0.9659258262890683122, 1.000000000000000000, 0.9659258262890683122, 1.000000000000000000, 0.9659258262890683122, 1.000000000000000000, 0.9659258262890683122, 1.000000000000000000, 0.9659258262890683122, 1.000000000000000000, 0.9659258262890683122, 1.000000000000000000, 0.9659258262890683122, 1.000000000000000000, 0.9659258262890683122, 1.000000000000000000, 0.9659258262890683122, 1.000000000000000000, 0.9659258262890683122, 1.000000000000000000, 0.9659258262890683122, 1.000000000000000000, 0.9659258262890683122, 1.000000000000000000, 0.9659258262890683122, 1.000000000000000000, 0.9659258262890683122, 1.000000000000000000, 0.9659258262890683122, 1.000000000000000000, 0.9659258262890683122, 1.000000000000000000, 0.9659258262890683122, 1.000000000000000000, 0.9659258262890683122, 1.000000000000000000, 0.9659258262890683122, 1.000000000000000000, 0.9659258262890683122, 1.000000000000000000, 0.9659258262890683122, 1.000000000000000000, 0.9659258262890683122, 1.000000000000000000, 0.9659258262890683122, 1.000000000000000000, 0.9659258262890683122, 1.000000000000000000, 0.9659258262890683122, 1.000000000000000000, 0.9659258262890683122, 1.000000000000000000, 0.9659258262890683122, 1.000000000000000000, 0.9659258262890683122, 1.000000000000000000, 0.9659258262890683122, 1.000000000000000000, 0.9659258262890683122, 1.000000000000000000, 0.9659258262890683122, 1.000000000000000000, 0.9659258262890683122, 1.000000000000000000, 0.9659258262890683122, 1.000000000000000000, 0.9659258262890683122, 1.000000000000000000, 0.9659258262890683122, 1.000000000000000000, 0.9659258262890683122, 1.000000000000000000, 0.9659258262890683122, 1.000000000000000000, 0.9659258262890683122, 1.000000000000000000, 0.9659258262890683122, 1.000000000000000000, 0.9659258262890683122, 1.000000000000000000, 0.9659258262890683122, 1.000000000000000000, 0.9659258262890683122, 1.000000000000000000, 0.9659258262890683122, 1.000000000000000000, 0.9659258262890683122, 1.000000000000000000, 0.9659258262890683122, 1.000000000000000000, 0.9659258262890683122, 1.000000000000000000, 0.9659258262890683122, 1.000000000000000000, 0.9659258262890683122, 1.000000000000000000, 0.9659258262890683122, 1.000000000000000000, 0.9659258262890683122, 1.000000000000000000, 0.9659258262890683122, 1.000000000000000000, 0.9659258262890683122, 1.000000000000000000, 0.9659258262890683122, 1.000000000000000000, 0.9659258262890683122, 1.000000000000000000, 0.9659258262890683122, 1.000000000000000000, 0.9659258262890683122, 1.000000000000000000, 0.9659258262890683122, 1.000000000000000000, 0.9659258262890683122, 1.000000000000000000, 0.9659258262890683122, 1.000000000000000000, 0.9659258262890683122, 1.000000000000000000, 0.9659258262890683122, 1.000000000000000000, 0.9659258262890683122, 1.000000000000000000, 0.9659258262890683122, 1.000000000000000000, 0.9659258262890683122, 1.000000000000000000, 0.9659258262890683122, 1.000000000000000000, 0.9659258262890683122, 1.000000000000000000, 0.9659258262890683122, 1.000000000000000000, 0.9659258262890683122, 1.000000000000000000, 0.9659258262890683122, 1.000000000000000000, 0.9659258262890683122, 1.000000000000000000, 0.9659258262890683122, 1.000000000000000000, 0.9659258262890683122, 1.000000000000000000, 0.9659258262890683122, 1.000000000000000000, 0.9659258262890683122, 1.000000000000000000, 0.9659258262890683122, 1.000000000000000000, 0.9659258262890683122, 1.000000000000000000, 0.9659258262890683122, 1.000000000000000000, 0.9659258262890683122, 1.000000000000000000, 0.9659258262890683122, 1.000000000000000000, 0.9659258262890683122, 1.000000000000000000, 0.9659258262890683122, 1.000000000000000000, 0.9659258262890683122, 1.000000000000000000, 0.9659258262890683122, 1.000000000000000000, 0.9659258262890683122, 1.000000000000000000, 0.9659258262890683122, 1.000000000000000000, 0.9659258262890683122, 1.000000000000000000, 0.9659258262890683122, 1.000000000000000000, 0.9659258262890683122, 1.000000000000000000, 0.9659258262890683122, 1.000000000000000000, 0.9659258262890683122, 1.000000000000000000, 0.9659258262890683122, 1.000000000000000000, 0.9659258262890683122, 1.000000000000000000, 0.9659258262890683122, 1.000000000000000000, 0.9659258262890683122, 1.000000000000000000, 0.9659258262890683122, 1.000000000000000000, 0.9659258262890683122, 1.000000000000000000, 0.9659258262890683122, 1.000000000000000000, 0.9659258262890683122, 1.000000000000000000, 0.9659258262890683122, 1.000000000000000000, 0.9659258262890683122, 1.000000000000000000, 0.9659258262890683122, 1.000000000000000000, 0.9659258262890683122, 1.000000000000000000, 0.9659258262890683122, 1.000000000000000000, 0.9659258262890683122, 1.000000000000000000, 0.9659258262890683122, 1.000000000000000000, 0.9659258262890683122, 1.000000000000000000, 0.9659258262890683122, 1.000000000000000000, 0.9659258262890683122, 1.000000000000000000, 0.9659258262890683122, 1.000000000000000000, 0.9659258262890683122, 1.000000000000000000, 0.9659258262890683122, 1.000000000000000000, 0.9659258262890683122, 1.000000000000000000, 0.9659258262890683122, 1.000000000000000000, 0.9659258262890683122, 1.000000000000000000, 0.9659258262890683122, 1.000000000000000000, 0.9659258262890683122, 1.000000000000000000, 0.9659258262890683122, 1.000000000000000000, 0.9659258262890683122, 1.000000000000000000, 0.9659258262890683122, 1.000000000000000000, 0.9659258262890683122, 1.000000000000000000, 0.9659258262890683122, 1.000000000000000000, 0.9659258262890683122, 1.000000000000000000, 0.9659258262890683122, 1.000000000000000000, 0.9659258262890683122, 1.000000000000000000, 0.9659258262890683122, 1.000000000000000000, 0.9659258262890683122, 1.000000000000000000, 0.9659258262890683122, 1.000000000000000000, 0.9659258262890683122, 1.000000000000000000, 0.9659258262890683122, 1.000000000000000000, 0.9659258262890683122, 1.000000000000000000, 0.9659258262890683122, 1.000000000000000000, 0.9659258262890683122, 1.000000000000000000, 0.9659258262890683122, 1.000000000000000000, 0.9659258262890683122, 1.000000000000000000, 0.9659258262890683122, 1.000000000000000000, 0.9659258262890683122, 1.000000000000000000, 0.9659258262890683122, 1.000000000000000000, 0.9659258262890683122, 1.000000000000000000, 0.9659258262890683122, 1.000000000000000000, 0.9659258262890683122, 1.000000000000000000, 0.9659258262890683122, 1.000000000000000000, 0.9659258262890683122, 1.000000000000000000, 0.9659258262890683122, 1.000000000000000000, 0.9659258262890683122, 1.000000000000000000, 0.9659258262890683122, 1.000000000000000000, 0.9659258262890683122, 1.000000000000000000, 0.9659258262890683122, 1.000000000000000000, 0.9659258262890683122, 1.000000000000000000, 0.9659258262890683122, 1.000000000000000000, 0.9659258262890683122, 1.000000000000000000, 0.9659258262890683122, 1.000000000000000000, 0.9659258262890683122, 1.000000000000000000, 0.9659258262890683122, 1.000000000000000000, 0.9659258262890683122, 1.000000000000000000, 0.9659258262890683122, 1.000000000000000000, 0.9659258262890683122, 1.000000000000000000, 0.9659258262890683122, 1.000000000000000000, 0.9659258262890683122, 1.000000000000000000, 0.9659258262890683122, 1.000000000000000000, 0.9659258262890683122, 1.000000000000000000, 0.9659258262890683122, 1.000000000000000000, 0.9659258262890683122, 1.000000000000000000, 0.9659258262890683122, 1.000000000000000000, 0.9659258262890683122, 1.000000000000000000, 0.9659258262890683122, 1.000000000000000000, 0.9659258262890683122, 1.000000000000000000, 0.9659258262890683122, 1.000000000000000000, 0.9659258262890683122, 1.000000000000000000, 0.9659258262890683122, 1.000000000000000000, 0.9659258262890683122, 1.000000000000000000, 0.9659258262890683122, 1.000000000000000000, 0.9659258262890683122, 1.000000000000000000, 0.9659258262890683122, 1.000000000000000000, 0.9659258262890683122, 1.000000000000000000, 0.9659258262890683122, 1.000000000000000000, 0.9659258262890683122, 1.000000000000000000, 0.9659258262890683122, 1.000000000000000000, 0.9659258262890683122, 1.000000000000000000, 0.9659258262890683122, 1.000000000000000000, 0.9659258262890683122, 1.000000000000000000, 0.9659258262890683122, 1.000000000000000000, 0.9659258262890683122, 1.000000000000000000, 0.9659258262890683122, 1.000000000000000000, 0.9659258262890683122, 1.000000000000000000, 0.9659258262890683122, 1.000000000000000000, 0.9659258262890683122, 1.000000000000000000, 0.9659258262890683122, 1.000000000000000000, 0.9659258262890683122, 1.000000000000000000, 0.9659258262890683122, 1.000000000000000000, 0.9659258262890683122, 1.000000000000000000, 0.9659258262890683122, 1.000000000000000000, 0.9659258262890683122, 1.000000000000000000, 0.9659258262890683122, 1.000000000000000000, 0.9659258262890683122, 1.000000000000000000, 0.9659258262890683122, 1.000000000000000000, 0.9659258262890683122, 1.000000000000000000, 0.9659258262890683122, 1.000000000000000000, 0.9659258262890683122, 1.000000000000000000, 0.9659258262890683122, 1.000000000000000000, 0.9659258262890683122, 1.000000000000000000, 0.9659258262890683122, 1.000000000000000000, 0.9659258262890683122, 1.000000000000000000, 0.9659258262890683122, 1.000000000000000000, 0.9659258262890683122, 1.000000000000000000, 0.9659258262890683122, 1.000000000000000000, 0.9659258262890683122, 1.000000000000000000, 0.9659258262890683122, 1.000000000000000000, 0.9659258262890683122, 1.000000000000000000, 0.9659258262890683122, 1.000000000000000000, 0.9659258262890683122, 1.000000000000000000),
 ( 1.000000000000000000, 0.9659258262890683122, 1.000000000000000000, 0.9659258262890683122, 1.000000000000000000, 0.9659258262890683122, 1.000000000000000000, 0.9659258262890683122, 1.000000000000000000, 0.9659258262890683122, 1.000000000000000000, 0.9659258262890683122, 1.000000000000000000, 0.9659258262890683122, 1.000000000000000000, 0.9659258262890683122, 1.000000000000000000, 0.9659258262890683122, 1.000000000000000000, 0.9659258262890683122, 1.000000000000000000, 0.9659258262890683122, 1.000000000000000000, 0.9659258262890683122, 1.000000000000000000, 0.9659258262890683122, 1.000000000000000000, 0.9659258262890683122, 1.000000000000000000, 0.9659258262890683122, 1.000000000000000000, 0.9659258262890683122, 1.000000000000000000, 0.9659258262890683122, 1.000000000000000000, 0.9659258262890683122, 1.000000000000000000, 0.9659258262890683122, 1.000000000000000000, 0.9659258262890683122, 1.000000000000000000, 0.9659258262890683122, 1.000000000000000000, 0.9659258262890683122, 1.000000000000000000, 0.9659258262890683122, 1.000000000000000000, 0.9659258262890683122, 1.000000000000000000, 0.9659258262890683122, 1.000000000000000000, 0.9659258262890683122, 1.000000000000000000, 0.9659258262890683122, 1.000000000000000000, 0.9659258262890683122, 1.000000000000000000, 0.9659258262890683122, 1.000000000000000000, 0.9659258262890683122, 1.000000000000000000, 0.9659258262890683122, 1.000000000000000000, 0.9659258262890683122, 1.000000000000000000, 0.9659258262890683122, 1.000000000000000000, 0.9659258262890683122, 1.000000000000000000, 0.9659258262890683122, 1.000000000000000000, 0.9659258262890683122, 1.000000000000000000, 0.9659258262890683122, 1.000000000000000000, 0.9659258262890683122, 1.000000000000000000, 0.9659258262890683122, 1.000000000000000000, 0.9659258262890683122, 1.000000000000000000, 0.9659258262890683122, 1.000000000000000000, 0.9659258262890683122, 1.000000000000000000, 0.9659258262890683122, 1.000000000000000000, 0.9659258262890683122, 1.000000000000000000, 0.9659258262890683122, 1.000000000000000000, 0.9659258262890683122, 1.000000000000000000, 0.9659258262890683122, 1.000000000000000000, 0.9659258262890683122, 1.000000000000000000, 0.9659258262890683122, 1.000000000000000000, 0.9659258262890683122, 1.000000000000000000, 0.9659258262890683122, 1.000000000000000000, 0.9659258262890683122, 1.000000000000000000, 0.9659258262890683122, 1.000000000000000000, 0.9659258262890683122, 1.000000000000000000, 0.9659258262890683122, 1.000000000000000000, 0.9659258262890683122, 1.000000000000000000, 0.9659258262890683122, 1.000000000000000000, 0.9659258262890683122, 1.000000000000000000, 0.9659258262890683122, 1.000000000000000000, 0.9659258262890683122, 1.000000000000000000, 0.9659258262890683122, 1.000000000000000000, 0.9659258262890683122, 1.000000000000000000, 0.9659258262890683122, 1.000000000000000000, 0.9659258262890683122, 1.000000000000000000, 0.9659258262890683122, 1.000000000000000000, 0.9659258262890683122, 1.000000000000000000, 0.9659258262890683122, 1.000000000000000000, 0.9659258262890683122, 1.000000000000000000, 0.9659258262890683122, 1.000000000000000000, 0.9659258262890683122, 1.000000000000000000, 0.9659258262890683122, 1.000000000000000000, 0.9659258262890683122, 1.000000000000000000, 0.9659258262890683122, 1.000000000000000000, 0.9659258262890683122, 1.000000000000000000, 0.9659258262890683122, 1.000000000000000000, 0.9659258262890683122, 1.000000000000000000, 0.9659258262890683122, 1.000000000000000000, 0.9659258262890683122, 1.000000000000000000, 0.9659258262890683122, 1.000000000000000000, 0.9659258262890683122, 1.000000000000000000, 0.9659258262890683122, 1.000000000000000000, 0.9659258262890683122, 1.000000000000000000, 0.9659258262890683122, 1.000000000000000000, 0.9659258262890683122, 1.000000000000000000, 0.9659258262890683122, 1.000000000000000000, 0.9659258262890683122, 1.000000000000000000, 0.9659258262890683122, 1.000000000000000000, 0.9659258262890683122, 1.000000000000000000, 0.9659258262890683122, 1.000000000000000000, 0.9659258262890683122, 1.000000000000000000, 0.9659258262890683122, 1.000000000000000000, 0.9659258262890683122, 1.000000000000000000, 0.9659258262890683122, 1.000000000000000000, 0.9659258262890683122, 1.000000000000000000, 0.9659258262890683122, 1.000000000000000000, 0.9659258262890683122, 1.000000000000000000, 0.9659258262890683122, 1.000000000000000000, 0.9659258262890683122, 1.000000000000000000, 0.9659258262890683122, 1.000000000000000000, 0.9659258262890683122, 1.000000000000000000, 0.9659258262890683122, 1.000000000000000000, 0.9659258262890683122, 1.000000000000000000, 0.9659258262890683122, 1.000000000000000000, 0.9659258262890683122, 1.000000000000000000, 0.9659258262890683122, 1.000000000000000000, 0.9659258262890683122, 1.000000000000000000, 0.9659258262890683122, 1.000000000000000000, 0.9659258262890683122, 1.000000000000000000, 0.9659258262890683122, 1.000000000000000000, 0.9659258262890683122, 1.000000000000000000, 0.9659258262890683122, 1.000000000000000000, 0.9659258262890683122, 1.000000000000000000, 0.9659258262890683122, 1.000000000000000000, 0.9659258262890683122, 1.000000000000000000, 0.9659258262890683122, 1.000000000000000000, 0.9659258262890683122, 1.000000000000000000, 0.9659258262890683122, 1.000000000000000000, 0.9659258262890683122, 1.000000000000000000, 0.9659258262890683122, 1.000000000000000000, 0.9659258262890683122, 1.000000000000000000, 0.9659258262890683122, 1.000000000000000000, 0.9659258262890683122, 1.000000000000000000, 0.9659258262890683122, 1.000000000000000000, 0.9659258262890683122, 1.000000000000000000, 0.9659258262890683122, 1.000000000000000000, 0.9659258262890683122, 1.000000000000000000, 0.9659258262890683122, 1.000000000000000000, 0.9659258262890683122, 1.000000000000000000, 0.9659258262890683122, 1.000000000000000000, 0.9659258262890683122, 1.000000000000000000, 0.9659258262890683122, 1.000000000000000000, 0.9659258262890683122, 1.000000000000000000, 0.9659258262890683122, 1.000000000000000000, 0.9659258262890683122, 1.000000000000000000, 0.9659258262890683122, 1.000000000000000000, 0.9659258262890683122, 1.000000000000000000, 0.9659258262890683122, 1.000000000000000000, 0.9659258262890683122, 1.000000000000000000, 0.9659258262890683122, 1.000000000000000000, 0.9659258262890683122, 1.000000000000000000, 0.9659258262890683122, 1.000000000000000000, 0.9659258262890683122, 1.000000000000000000, 0.9659258262890683122, 1.000000000000000000, 0.9659258262890683122, 1.000000000000000000, 0.9659258262890683122, 1.000000000000000000, 0.9659258262890683122, 1.000000000000000000, 0.9659258262890683122, 1.000000000000000000, 0.9659258262890683122, 1.000000000000000000, 0.9659258262890683122, 1.000000000000000000, 0.9659258262890683122, 1.000000000000000000, 0.9659258262890683122, 1.000000000000000000, 0.9659258262890683122, 1.000000000000000000, 0.9659258262890683122, 1.000000000000000000, 0.9659258262890683122, 1.000000000000000000, 0.9659258262890683122, 1.000000000000000000, 0.9659258262890683122, 1.000000000000000000, 0.9659258262890683122, 1.000000000000000000, 0.9659258262890683122, 1.000000000000000000, 0.9659258262890683122, 1.000000000000000000, 0.9659258262890683122, 1.000000000000000000, 0.9659258262890683122, 1.000000000000000000, 0.9659258262890683122, 1.000000000000000000, 0.9659258262890683122, 1.000000000000000000, 0.9659258262890683122, 1.000000000000000000, 0.9659258262890683122, 1.000000000000000000, 0.9659258262890683122, 1.000000000000000000, 0.9659258262890683122, 1.000000000000000000, 0.9659258262890683122, 1.000000000000000000, 0.9659258262890683122, 1.000000000000000000, 0.9659258262890683122, 1.000000000000000000, 0.9659258262890683122, 1.000000000000000000, 0.9659258262890683122, 1.000000000000000000, 0.9659258262890683122, 1.000000000000000000, 0.9659258262890683122, 1.000000000000000000, 0.9659258262890683122, 1.000000000000000000, 0.9659258262890683122, 1.000000000000000000, 0.9659258262890683122, 1.000000000000000000, 0.9659258262890683122, 1.000000000000000000, 0.9659258262890683122, 1.000000000000000000, 0.9659258262890683122, 1.000000000000000000, 0.9659258262890683122, 1.000000000000000000, 0.9659258262890683122, 1.000000000000000000, 0.9659258262890683122, 1.000000000000000000, 0.9659258262890683122, 1.000000000000000000, 0.9659258262890683122, 1.000000000000000000, 0.9659258262890683122, 1.000000000000000000, 0.9659258262890683122, 1.000000000000000000, 0.9659258262890683122, 1.000000000000000000, 0.9659258262890683122, 1.000000000000000000, 0.9659258262890683122, 1.000000000000000000, 0.9659258262890683122, 1.000000000000000000, 0.9659258262890683122, 1.000000000000000000, 0.9659258262890683122, 1.000000000000000000, 0.9659258262890683122, 1.000000000000000000, 0.9659258262890683122, 1.000000000000000000, 0.9659258262890683122, 1.000000000000000000, 0.9659258262890683122, 1.000000000000000000, 0.9659258262890683122, 1.000000000000000000, 0.9659258262890683122, 1.000000000000000000, 0.9659258262890683122, 1.000000000000000000, 0.9659258262890683122, 1.000000000000000000, 0.9659258262890683122, 1.000000000000000000, 0.9659258262890683122, 1.000000000000000000, 0.9659258262890683122, 1.000000000000000000, 0.9659258262890683122, 1.000000000000000000, 0.9659258262890683122, 1.000000000000000000, 0.9659258262890683122, 1.000000000000000000, 0.9659258262890683122, 1.000000000000000000, 0.9659258262890683122, 1.000000000000000000, 0.9659258262890683122, 1.000000000000000000, 0.9659258262890683122, 1.000000000000000000, 0.9659258262890683122, 1.000000000000000000, 0.9659258262890683122, 1.000000000000000000, 0.9659258262890683122, 1.000000000000000000, 0.9659258262890683122, 1.000000000000000000, 0.9659258262890683122, 1.000000000000000000, 0.9659258262890683122, 1.000000000000000000, 0.9659258262890683122, 1.000000000000000000, 0.9659258262890683122, 1.000000000000000000, 0.9659258262890683122, 1.000000000000000000, 0.9659258262890683122, 1.000000000000000000, 0.9659258262890683122, 1.000000000000000000, 0.9659258262890683122, 1.000000000000000000, 0.9659258262890683122, 1.000000000000000000, 0.9659258262890683122, 1.000000000000000000, 0.9659258262890683122, 1.000000000000000000, 0.9659258262890683122, 1.000000000000000000, 0.9659258262890683122, 1.000000000000000000, 0.9659258262890683122, 1.000000000000000000, 0.9659258262890683122, 1.000000000000000000, 0.9659258262890683122, 1.000000000000000000, 0.9659258262890683122, 1.000000000000000000, 0.9659258262890683122, 1.000000000000000000, 0.9659258262890683122, 1.000000000000000000, 0.9659258262890683122, 1.000000000000000000, 0.9659258262890683122, 1.000000000000000000, 0.9659258262890683122, 1.000000000000000000, 0.9659258262890683122, 1.000000000000000000, 0.9659258262890683122, 1.000000000000000000, 0.9659258262890683122, 1.000000000000000000, 0.9659258262890683122, 1.000000000000000000, 0.9659258262890683122, 1.000000000000000000, 0.9659258262890683122, 1.000000000000000000, 0.9659258262890683122, 1.000000000000000000, 0.9659258262890683122, 1.000000000000000000, 0.9659258262890683122, 1.000000000000000000, 0.9659258262890683122, 1.000000000000000000, 0.9659258262890683122, 1.000000000000000000, 0.9659258262890683122, 1.000000000000000000, 0.9659258262890683122, 1.000000000000000000, 0.9659258262890683122, 1.000000000000000000, 0.9659258262890683122, 1.000000000000000000, 0.9659258262890683122, 1.000000000000000000, 0.9659258262890683122, 1.000000000000000000, 0.9659258262890683122, 1.000000000000000000) ) ) 
 REPRESENTATION_ITEM ( '' )  SURFACE ( )  );
#20410 = CARTESIAN_POINT ( 'NONE',  ( 0.9251968503937013644, 0.1012011053420775880, -0.2882089793578256898 ) ) ;
#20411 = CARTESIAN_POINT ( 'NONE',  ( 0.5183727034120741983, -0.6692913385826771977, 0.1292274648535927661 ) ) ;
#20412 = ORIENTED_EDGE ( 'NONE', *, *, #60997, .T. ) ;
#20414 = DIRECTION ( 'NONE',  ( 8.659560562354947649E-17, -0.7071067811865462405, 0.7071067811865486830 ) ) ;
#20413 = CARTESIAN_POINT ( 'NONE',  ( 1.614173228346457378, 0.9921945702958886448, -0.1372047244094476148 ) ) ;
#20415 = CARTESIAN_POINT ( 'NONE',  ( 1.115485564304462551, -0.4281496062992127816, -0.4176697321401328100 ) ) ;
#20416 = CARTESIAN_POINT ( 'NONE',  ( 1.515748031496063186, -0.4536011799217368745, -0.2665933059059886201 ) ) ;
#20417 = CARTESIAN_POINT ( 'NONE',  ( 0.1049643490035304522, -0.3917322834645668994, -0.7952562747693419087 ) ) ;
#20418 = CARTESIAN_POINT ( 'NONE',  ( -0.9711286089238838626, -0.5023911411419708095, 0.1820866141732285504 ) ) ;
#20419 = CARTESIAN_POINT ( 'NONE',  ( -1.601049868766403650, 0.1283753931104746893, -0.1820866141732285504 ) ) ;
#20420 = CARTESIAN_POINT ( 'NONE',  ( 0.4724409448818898682, 2.892866454678787531E-17, -0.7480314960629921295 ) ) ;
#20421 = CARTESIAN_POINT ( 'NONE',  ( 0.6561679790026253567, 0.2306618581243848609, 0.2411417322834645549 ) ) ;
#20422 = CARTESIAN_POINT ( 'NONE',  ( -0.9842519685039360366, 0.1771653543307087630, 0.000000000000000000 ) ) ;
#20423 = CARTESIAN_POINT ( 'NONE',  ( 0.2165354330708668673, 0.07958543189024071263, -0.2665933059059888421 ) ) ;
#20424 = CARTESIAN_POINT ( 'NONE',  ( -0.3215223097112853146, -0.3162353388693405765, 0.4822834645669290543 ) ) ;
#20425 = CARTESIAN_POINT ( 'NONE',  ( -1.279527559055116948, 0.07958543189024071263, -0.2665933059059888421 ) ) ;
#20426 = CARTESIAN_POINT ( 'NONE',  ( -0.3392501089628019995, 0.1958661417322831999, -0.1804655100075609198 ) ) ;
#20427 = CARTESIAN_POINT ( 'NONE',  ( 0.7283464566929140904, -0.5400638737290845981, -0.3530559997133363437 ) ) ;
#20428 = CARTESIAN_POINT ( 'NONE',  ( -1.404199475065615932, -0.4281496062992127816, -0.4176697321401328100 ) ) ;
#20429 = CARTESIAN_POINT ( 'NONE',  ( -0.3458507752293909498, 0.3458507752293907833, -1.041338582677165281 ) ) ;
#20430 = CARTESIAN_POINT ( 'NONE',  ( -0.8398950131233589023, -0.6046776061558809534, -0.2411417322834644161 ) ) ;
#20431 = CARTESIAN_POINT ( 'NONE',  ( -0.2165354330708654795, -0.4536011799217368745, -0.2665933059059886201 ) ) ;
#20432 = CARTESIAN_POINT ( 'NONE',  ( -1.384514435695537005, -0.6692913385826773087, -0.1292274648535924053 ) ) ;
#20433 = CARTESIAN_POINT ( 'NONE',  ( 0.8530183727034128527, -0.3690944881889763329, 0.3153832671262228327 ) ) ;
#20434 = CARTESIAN_POINT ( 'NONE',  ( -0.3674540682414692561, -0.5023911411419708095, -0.1820866141732282451 ) ) ;
#20435 = CARTESIAN_POINT ( 'NONE',  ( -0.9842519685039365918, -0.6692913385826771977, 8.415575281601705876E-17 ) ) ;
#20436 = CARTESIAN_POINT ( 'NONE',  ( -1.286089238845143479, -0.6046776061558807314, 0.2411417322834647770 ) ) ;
#20437 = CARTESIAN_POINT ( 'NONE',  ( -1.377952755905511140, -0.6692913385826771977, 8.415575281601705876E-17 ) ) ;
#20438 = DIRECTION ( 'NONE',  ( 0.000000000000000000, 0.000000000000000000, -1.000000000000000000 ) ) ;
#20439 = CARTESIAN_POINT ( 'NONE',  ( 1.207349081364829990, 0.1283753931104748280, 0.1820866141732283561 ) ) ;
#20440 = PRODUCT_DEFINITION_SHAPE ( 'NONE', 'NONE',  #83325 ) ;
#20441 = CARTESIAN_POINT ( 'NONE',  ( 0.6102362204724416372, 0.1660481256975883668, -0.3530559997133364547 ) ) ;
#20442 = CARTESIAN_POINT ( 'NONE',  ( -1.535433070866141225, -0.6692913385826771977, 8.415575281601705876E-17 ) ) ;
#20443 = CARTESIAN_POINT ( 'NONE',  ( -1.725721784776902190, -0.05778040916215522460, 0.4822834645669289988 ) ) ;
#20444 = VECTOR ( 'NONE', #63989, 39.37007874015748143 ) ;
#20445 = EDGE_LOOP ( 'NONE', ( #48127, #21810 ) ) ;
#20446 = CARTESIAN_POINT ( 'NONE',  ( -0.3996062992125984925, -0.1070741851644056858, -2.327427821522309426 ) ) ;
#20447 = CARTESIAN_POINT ( 'NONE',  ( -0.7414698162729651543, -0.5511811023622046335, 0.09757992244046803654 ) ) ;
#20448 = CARTESIAN_POINT ( 'NONE',  ( 0.5774278215223103139, -0.6046776061558809534, -0.2411417322834644161 ) ) ;
#20449 = CARTESIAN_POINT ( 'NONE',  ( -1.187664041994750175, -0.08942795157528024563, -0.3641732283464568787 ) ) ;
#20450 = CARTESIAN_POINT ( 'NONE',  ( 0.1998031496062992463, 0.3460692066303959202, -1.953412073490813805 ) ) ;
#20451 = CARTESIAN_POINT ( 'NONE',  ( -1.469816272965878357, -0.6046776061558809534, -0.2411417322834644161 ) ) ;
#20452 = CARTESIAN_POINT ( 'NONE',  ( 0.8202099737532814183, -0.6692913385826773087, -0.1292274648535924053 ) ) ;
#20453 = CARTESIAN_POINT ( 'NONE',  ( 0.3740157480314966754, -0.5400638737290844871, 0.3530559997133364547 ) ) ;
#20454 = CARTESIAN_POINT ( 'NONE',  ( 1.154855643044620184, 0.2306618581243847221, -0.2411417322834647770 ) ) ;
#20455 = CARTESIAN_POINT ( 'NONE',  ( -1.686351706036744558, 0.1771653543307087075, -0.09757992244046823083 ) ) ;
#20457 = EDGE_CURVE ( 'NONE', #15514, #13252, #27628, .T. ) ;
#20456 = CARTESIAN_POINT ( 'NONE',  ( -0.1070741851644057135, 0.3996062992125984925, -1.185695538057742748 ) ) ;
#20458 = CARTESIAN_POINT ( 'NONE',  ( 0.3460692066303959757, -0.1998031496062991907, -1.207349081364829324 ) ) ;
#20459 = CARTESIAN_POINT ( 'NONE',  ( -0.3420746716998661618, 0.1974969037888702206, -0.8136482939632546652 ) ) ;
#20460 = CARTESIAN_POINT ( 'NONE',  ( 0.3798529523383403772, 1.251889725672750142, -1.733216647067249427 ) ) ;
#20461 = CARTESIAN_POINT ( 'NONE',  ( 0.6758530183727039509, -0.5511811023622046335, 0.09757992244046803654 ) ) ;
#20462 = CARTESIAN_POINT ( 'NONE',  ( 0.1246719160104994284, -0.5511811023622046335, 0.09757992244046803654 ) ) ;
#20463 = CARTESIAN_POINT ( 'NONE',  ( -0.09186351706036689768, 0.05413385826771626580, -0.4176697321401330321 ) ) ;
#20464 = CARTESIAN_POINT ( 'NONE',  ( 1.312335958005249825, 0.2306618581243847221, -0.2411417322834647770 ) ) ;
#20465 = CARTESIAN_POINT ( 'NONE',  ( -0.3949938075777409963, -7.255918531996591613E-17, -1.533464566929133577 ) ) ;
#20466 = CARTESIAN_POINT ( 'NONE',  ( 0.1968503937007881344, -0.5511811023622047445, 6.969142054262312111E-17 ) ) ;
#20467 = CARTESIAN_POINT ( 'NONE',  ( -0.8136482939632537770, 0.2306618581243847221, -0.2411417322834647770 ) ) ;
#20468 = CARTESIAN_POINT ( 'NONE',  ( -1.522309711286088607, -0.6046776061558807314, 0.2411417322834647770 ) ) ;
#20469 = CARTESIAN_POINT ( 'NONE',  ( 1.036745406824147731, 0.05413385826771666132, 0.4176697321401328100 ) ) ;
#20470 = CARTESIAN_POINT ( 'NONE',  ( 0.4724409448818898682, 2.892866454678787531E-17, -1.850393700787401619 ) ) ;
#20471 = LINE ( 'NONE', #28022, #30428 ) ;
#20472 = ORIENTED_EDGE ( 'NONE', *, *, #28057, .T. ) ;
#20473 = EDGE_LOOP ( 'NONE', ( #16050, #3704, #48420, #36430 ) ) ;
#20474 = CARTESIAN_POINT ( 'NONE',  ( -1.213910761154854745, 0.2952755905511810774, -0.1292274648535930714 ) ) ;
#20476 = CARTESIAN_POINT ( 'NONE',  ( -1.266404199475064773, -0.05778040916215560624, -0.4822834645669293319 ) ) ;
#20475 = CARTESIAN_POINT ( 'NONE',  ( -0.8923884514435688198, -0.5023911411419708095, 0.1820866141732285504 ) ) ;
#20477 = CARTESIAN_POINT ( 'NONE',  ( -0.1958661417322834497, -0.3392501089628018884, -2.507854699966192147 ) ) ;
#20478 = CARTESIAN_POINT ( 'NONE',  ( -0.4605079024601024251, -1.150887559458346504E-15, 0.3627985898453527924 ) ) ;
#20479 = CARTESIAN_POINT ( 'NONE',  ( 1.476377952755906442, -0.5400638737290844871, 0.3530559997133364547 ) ) ;
#20480 = CARTESIAN_POINT ( 'NONE',  ( -1.279527559055116948, -0.5400638737290844871, 0.3530559997133364547 ) ) ;
#20481 = CARTESIAN_POINT ( 'NONE',  ( 0.2099737532808405305, 0.2306618581243847221, -0.2411417322834647770 ) ) ;
#20482 = CARTESIAN_POINT ( 'NONE',  ( -1.463254593175852492, 0.2952755905511811885, 0.1292274648535926551 ) ) ;
#20483 = CARTESIAN_POINT ( 'NONE',  ( 0.1049643490035304522, -0.3917322834645668994, -2.685020054296901382 ) ) ;
#20484 = CARTESIAN_POINT ( 'NONE',  ( 0.7086614173228352742, -0.1870078740157480879, -0.4822834645669291653 ) ) ;
#20485 = CARTESIAN_POINT ( 'NONE',  ( -0.2867679344610365999, 0.2867679344610364889, -1.744094488188976610 ) ) ;
#20486 = CARTESIAN_POINT ( 'NONE',  ( -0.9251968503937002541, -0.4536011799217368745, -0.2665933059059886201 ) ) ;
#20487 = ORIENTED_EDGE ( 'NONE', *, *, #26568, .F. ) ;
#20488 = CARTESIAN_POINT ( 'NONE',  ( -0.3949938075777409963, -7.255918531996591613E-17, -1.929133858267716439 ) ) ;
#20489 = VERTEX_POINT ( 'NONE', #68125 ) ;
#20490 = CARTESIAN_POINT ( 'NONE',  ( -1.568241469816272105, -0.08942795157527998196, 0.3641732283464567121 ) ) ;
#20491 = CARTESIAN_POINT ( 'NONE',  ( -1.325459317585300889, -0.4281496062992127816, -0.4176697321401328100 ) ) ;
#20492 = CARTESIAN_POINT ( 'NONE',  ( -1.463254593175852492, 0.2952755905511811885, 0.1292274648535926551 ) ) ;
#20493 = CARTESIAN_POINT ( 'NONE',  ( 0.3996062992125986035, 0.1070741851644054776, -0.5971128608923884640 ) ) ;
#20494 = CARTESIAN_POINT ( 'NONE',  ( -1.620734908136482577, -0.6692913385826773087, -0.1292274648535924053 ) ) ;
#20495 = CARTESIAN_POINT ( 'NONE',  ( -1.135170603674539924, -0.6692913385826771977, 0.1292274648535927661 ) ) ;
#20496 = CARTESIAN_POINT ( 'NONE',  ( -1.555118110236219930, -0.5400638737290845981, -0.3530559997133363437 ) ) ;
#20497 = DIRECTION ( 'NONE',  ( 1.000000000000000000, -0.000000000000000000, -0.000000000000000000 ) ) ;
#20498 = CARTESIAN_POINT ( 'NONE',  ( -0.7974104941589342799, -2.567464376874931580E-15, -0.4445507791589072832 ) ) ;
#20499 = CARTESIAN_POINT ( 'NONE',  ( 0.1181102362204730916, 0.1771653543307087630, 0.000000000000000000 ) ) ;
#20500 = CARTESIAN_POINT ( 'NONE',  ( 3.937007874015748143, 1.537401574803149984, 2.901595197523589142E-16 ) ) ;
#20501 = CARTESIAN_POINT ( 'NONE',  ( -0.1049643490035307020, 0.3917322834645669549, -0.5636482939632546652 ) ) ;
#20502 = CARTESIAN_POINT ( 'NONE',  ( -0.4921259842519677963, -0.4536011799217367080, 0.2665933059059888421 ) ) ;
#20503 = CARTESIAN_POINT ( 'NONE',  ( -0.9383202099737524282, -0.3162353388693409650, -0.4822834645669289433 ) ) ;
#20504 = CARTESIAN_POINT ( 'NONE',  ( 0.8202099737532813073, 0.2952755905511811885, 0.1292274648535926551 ) ) ;
#20505 = CARTESIAN_POINT ( 'NONE',  ( -1.076115485564303809, -0.6046776061558809534, -0.2411417322834644161 ) ) ;
#20506 = ORIENTED_EDGE ( 'NONE', *, *, #16133, .T. ) ;
#20507 = ORIENTED_EDGE ( 'NONE', *, *, #43446, .T. ) ;
#20509 = AXIS2_PLACEMENT_3D ( 'NONE', #22422, #3477, #29145 ) ;
#20508 = CARTESIAN_POINT ( 'NONE',  ( -1.069553805774277722, -0.6692913385826773087, -0.1292274648535924053 ) ) ;
#20510 = CARTESIAN_POINT ( 'NONE',  ( 1.030183727034121421, -0.3162353388693409650, -0.4822834645669289433 ) ) ;
#20511 = CARTESIAN_POINT ( 'NONE',  ( -1.719160104986876103, -0.004921259842519576551, 0.3153832671262227771 ) ) ;
#20512 = CARTESIAN_POINT ( 'NONE',  ( -1.640419947506561060, -0.4281496062992127816, -0.4176697321401328100 ) ) ;
#20513 = CARTESIAN_POINT ( 'NONE',  ( -0.4091458600556402980, -0.2362204724409451284, -1.154855643044619518 ) ) ;
#20514 = DIRECTION ( 'NONE',  ( -1.408710688920637755E-15, 1.000000000000000000, -4.918487082195260922E-30 ) ) ;
#20515 = CARTESIAN_POINT ( 'NONE',  ( -0.3917322834645669549, -0.1049643490035306603, -0.1955380577427821009 ) ) ;
#20516 = CARTESIAN_POINT ( 'NONE',  ( 0.1958661417322834775, 0.3392501089628018884, -2.591207349081364519 ) ) ;
#20517 = CARTESIAN_POINT ( 'NONE',  ( -0.1377952755905504645, -0.5400638737290845981, -0.3530559997133363437 ) ) ;
#20518 = CARTESIAN_POINT ( 'NONE',  ( -1.292650918635170010, 0.1771653543307087075, -0.09757992244046823083 ) ) ;
#20519 = CARTESIAN_POINT ( 'NONE',  ( -0.8202099737532801971, -0.6692913385826771977, 0.1292274648535927661 ) ) ;
#20520 = CARTESIAN_POINT ( 'NONE',  ( 0.2925321140481932369, 0.2925321140481932369, -0.05708661417322837689 ) ) ;
#20522 = CARTESIAN_POINT ( 'NONE',  ( -0.6824146981627288167, 0.1539470093639523085, 0.1968503937007873850 ) ) ;
#20521 = CARTESIAN_POINT ( 'NONE',  ( -1.312335958005248715, -0.6046776061558809534, -0.2411417322834644161 ) ) ;
#20523 = CARTESIAN_POINT ( 'NONE',  ( -0.8989501312335946848, 0.2952755905511810774, -0.1292274648535930714 ) ) ;
#20524 = CARTESIAN_POINT ( 'NONE',  ( -0.2624671916010490880, 0.2306618581243847221, -0.2411417322834647770 ) ) ;
#20525 = CARTESIAN_POINT ( 'NONE',  ( -0.3949938075777411073, 0.1058382717557497660, -2.629265091863516979 ) ) ;
#20526 = CARTESIAN_POINT ( 'NONE',  ( 0.7414698162729663755, -0.5511811023622048555, -0.09757992244046775898 ) ) ;
#20527 = CARTESIAN_POINT ( 'NONE',  ( -3.912791665790199769, 1.724409448818897905, -0.4359958488159722534 ) ) ;
#20528 = CARTESIAN_POINT ( 'NONE',  ( 0.3215223097112867578, -0.2845877964562161244, -0.3641732283464567121 ) ) ;
#20529 = CARTESIAN_POINT ( 'NONE',  ( 1.443569553805774897, 0.1283753931104748280, 0.1820866141732283561 ) ) ;
#20530 = CARTESIAN_POINT ( 'NONE',  ( 1.351706036745407458, -0.4281496062992127816, -0.4176697321401328100 ) ) ;
#20531 = CARTESIAN_POINT ( 'NONE',  ( 0.1181102362204730916, 0.1771653543307087630, 0.000000000000000000 ) ) ;
#20532 = CARTESIAN_POINT ( 'NONE',  ( 0.1049643490035304938, -0.3917322834645669549, -1.967191601049868899 ) ) ;
#20533 = CARTESIAN_POINT ( 'NONE',  ( -1.174540682414697335, -0.05778040916215522460, 0.4822834645669289988 ) ) ;
#20534 = CARTESIAN_POINT ( 'NONE',  ( 1.325459317585302665, 0.05413385826771626580, -0.4176697321401330321 ) ) ;
#20535 = B_SPLINE_CURVE_WITH_KNOTS ( 'NONE', 3,
 ( #3960, #17021, #36760, #29623 ),
 .UNSPECIFIED., .F., .F.,
 ( 4, 4 ),
 ( 1.734723475976806902E-18, 0.001357026659661017542 ),
 .UNSPECIFIED. ) ;
#20536 = CARTESIAN_POINT ( 'NONE',  ( -0.4091458600556402980, -0.2362204724409451284, 0.02821522309711285356 ) ) ;
#20537 = CARTESIAN_POINT ( 'NONE',  ( -0.5314960629921250401, 0.07958543189024085140, 0.2665933059059887866 ) ) ;
#20538 = CLOSED_SHELL ( 'NONE', ( #66492, #54205, #18121, #44866, #58939, #75378, #40034, #37271, #8055, #1081, #33939, #77308, #21751, #77471, #44868, #41341, #10079, #4724, #73865 ) ) ;
#20539 = CARTESIAN_POINT ( 'NONE',  ( -0.4608550785314876053, 0.02791078216816064370, 0.4328096321851915285 ) ) ;
#20540 = CARTESIAN_POINT ( 'NONE',  ( 0.2165354330708668673, -0.5400638737290844871, 0.3530559997133364547 ) ) ;
#20541 = CARTESIAN_POINT ( 'NONE',  ( 1.948818897637795367, 1.928577636452520604E-17, 5.859448621221250875 ) ) ;
#20542 = CARTESIAN_POINT ( 'NONE',  ( 1.043307086614173818, -0.4536011799217368745, -0.2665933059059886201 ) ) ;
#20543 = CARTESIAN_POINT ( 'NONE',  ( 0.3018372703412079971, -0.3690944881889763329, 0.3153832671262228327 ) ) ;
#20544 = CARTESIAN_POINT ( 'NONE',  ( -0.3477690288713902178, 0.2952755905511810774, -0.1292274648535930714 ) ) ;
#20545 = CARTESIAN_POINT ( 'NONE',  ( -1.706036745406823485, 0.2306618581243848609, 0.2411417322834645549 ) ) ;
#20546 = CARTESIAN_POINT ( 'NONE',  ( -0.5511811023622038563, -0.1870078740157479769, 0.3641732283464567677 ) ) ;
#20547 = FACE_OUTER_BOUND ( 'NONE', #46734, .T. ) ;
#20548 = CARTESIAN_POINT ( 'NONE',  ( 0.4068241469816281097, 0.05413385826771666132, 0.4176697321401328100 ) ) ;
#20549 = CARTESIAN_POINT ( 'NONE',  ( -0.8858267716535425107, -0.5400638737290844871, 0.3530559997133364547 ) ) ;
#20550 = CARTESIAN_POINT ( 'NONE',  ( 0.1070741851644054776, -0.3996062992125984925, -0.9494750656167976199 ) ) ;
#20551 = EDGE_CURVE ( 'NONE', #31839, #19838, #40124, .T. ) ;
#20552 = CARTESIAN_POINT ( 'NONE',  ( -0.3392501089628019995, 0.1958661417322832277, -2.630577427821522374 ) ) ;
#20553 = CARTESIAN_POINT ( 'NONE',  ( 0.05905511811023681640, 0.07958543189024071263, -0.2665933059059888421 ) ) ;
#20554 = CARTESIAN_POINT ( 'NONE',  ( -0.6102362204724400829, -0.5400638737290845981, -0.3530559997133363437 ) ) ;
#20555 = CARTESIAN_POINT ( 'NONE',  ( -1.049868766404198794, -0.6046776061558807314, 0.2411417322834647770 ) ) ;
#20556 = CARTESIAN_POINT ( 'NONE',  ( -1.233595800524933894, -0.5023911411419708095, -0.1820866141732282451 ) ) ;
#20557 = CARTESIAN_POINT ( 'NONE',  ( -3.908320185825792326, 1.537401574803149984, -0.4744094488188975722 ) ) ;
#20558 = CARTESIAN_POINT ( 'NONE',  ( -0.9448818897637790704, -0.1870078740157480601, -0.3641732283464567677 ) ) ;
#20559 = CARTESIAN_POINT ( 'NONE',  ( 0.4177787735907000921, 0.3937007874015748254, -1.244210979442979648 ) ) ;
#20560 = CARTESIAN_POINT ( 'NONE',  ( 1.325459317585302665, 0.05413385826771626580, -0.4176697321401330321 ) ) ;
#20561 = CARTESIAN_POINT ( 'NONE',  ( 0.2925321140481932369, 0.2925321140481932369, -0.1377952755905512139 ) ) ;
#20562 = AXIS2_PLACEMENT_3D ( 'NONE', #75180, #76812, #17524 ) ;
#20563 = CARTESIAN_POINT ( 'NONE',  ( 0.3917322834645670659, -0.1049643490035303273, -2.627972071687351363 ) ) ;
#20564 = EDGE_LOOP ( 'NONE', ( #79117, #3720, #49874, #65438 ) ) ;
#20565 = CARTESIAN_POINT ( 'NONE',  ( 0.4418045515502986298, 1.710866862483978679, -2.620820774047688317 ) ) ;
#20566 = CARTESIAN_POINT ( 'NONE',  ( 1.456692913385827515, 0.1771653543307087630, 0.000000000000000000 ) ) ;
#20567 = CARTESIAN_POINT ( 'NONE',  ( -1.410761154855642463, -0.05778040916215522460, 0.4822834645669289988 ) ) ;
#20568 = CARTESIAN_POINT ( 'NONE',  ( 1.253280839895013710, -0.3162353388693405765, 0.4822834645669290543 ) ) ;
#20569 = CARTESIAN_POINT ( 'NONE',  ( 0.1958661417322834775, 0.3392501089628018884, -2.433727034120734878 ) ) ;
#20570 = CARTESIAN_POINT ( 'NONE',  ( 1.555118110236221041, 0.07958543189024071263, -0.2665933059059888421 ) ) ;
#20571 = CARTESIAN_POINT ( 'NONE',  ( 0.5774278215223104249, 0.2306618581243848609, 0.2411417322834645549 ) ) ;
#20572 = CARTESIAN_POINT ( 'NONE',  ( -0.5249343832020990641, 0.2306618581243848609, 0.2411417322834645549 ) ) ;
#20573 = CARTESIAN_POINT ( 'NONE',  ( 0.3858746366555774188, 1.260986746289878502, -3.918061586339389724 ) ) ;
#20574 = CARTESIAN_POINT ( 'NONE',  ( 3.869764100875850765, 2.739927440807262471, 0.5314960629921260393 ) ) ;
#20575 = CARTESIAN_POINT ( 'NONE',  ( 0.7545931758530188826, -0.5511811023622046335, 0.09757992244046803654 ) ) ;
#20576 = CARTESIAN_POINT ( 'NONE',  ( -0.1070741851644051862, -0.3996062992125987146, -1.489501312335957950 ) ) ;
#20577 = EDGE_LOOP ( 'NONE', ( #53572, #56273, #19310, #7884 ) ) ;
#20578 = CARTESIAN_POINT ( 'NONE',  ( 0.3917322834645670104, 0.1049643490035304660, 0.03606992306330520509 ) ) ;
#20579 = ORIENTED_EDGE ( 'NONE', *, *, #64155, .F. ) ;
#20580 = CARTESIAN_POINT ( 'NONE',  ( 0.05249343832021075018, 0.2306618581243847221, -0.2411417322834647770 ) ) ;
#20581 = CARTESIAN_POINT ( 'NONE',  ( 1.384514435695538337, -0.6692913385826771977, 0.1292274648535927661 ) ) ;
#20582 = CARTESIAN_POINT ( 'NONE',  ( 0.3740157480314966754, -0.5400638737290844871, 0.3530559997133364547 ) ) ;
#20583 = CARTESIAN_POINT ( 'NONE',  ( 1.325459317585302665, -0.4281496062992124485, 0.4176697321401328655 ) ) ;
#20584 = CARTESIAN_POINT ( 'NONE',  ( -0.4133858267716528645, -0.5400638737290844871, 0.3530559997133364547 ) ) ;
#20585 = CARTESIAN_POINT ( 'NONE',  ( -0.1246719160104980823, 0.2952755905511811885, 0.1292274648535926551 ) ) ;
#20586 = CARTESIAN_POINT ( 'NONE',  ( 1.594488188976378673, 0.1660481256975885056, 0.3530559997133364547 ) ) ;
#20587 = CARTESIAN_POINT ( 'NONE',  ( 1.240157480314961314, -0.5400638737290844871, 0.3530559997133364547 ) ) ;
#20588 = CARTESIAN_POINT ( 'NONE',  ( 1.043307086614173818, 0.1660481256975885056, 0.3530559997133364547 ) ) ;
#20589 = CARTESIAN_POINT ( 'NONE',  ( 0.3392501089628018884, -0.1958661417322834220, -0.4120734908136482466 ) ) ;
#20590 = CARTESIAN_POINT ( 'NONE',  ( 0.6167979002624679463, -0.004921259842519870586, -0.3153832671262229437 ) ) ;
#20591 = EDGE_LOOP ( 'NONE', ( #39753, #28787, #77116, #28456 ) ) ;
#20592 = CARTESIAN_POINT ( 'NONE',  ( -0.3420746716998661618, 0.1974969037888702206, -0.4986876640419948270 ) ) ;
#20593 = ORIENTED_EDGE ( 'NONE', *, *, #42203, .F. ) ;
#20594 = CARTESIAN_POINT ( 'NONE',  ( -0.4330708661417315697, 0.1771653543307087630, 0.000000000000000000 ) ) ;
#20595 = CARTESIAN_POINT ( 'NONE',  ( -0.2034120734908128059, 0.2952755905511811885, 0.1292274648535926551 ) ) ;
#20596 = CARTESIAN_POINT ( 'NONE',  ( 2.554859668665111272, 1.520054044952884098, 0.4741688556381182251 ) ) ;
#20597 = CARTESIAN_POINT ( 'NONE',  ( 0.01968503937007930540, 0.1660481256975885056, 0.3530559997133364547 ) ) ;
#20598 = CARTESIAN_POINT ( 'NONE',  ( 0.03280839895013198948, 0.2952755905511811885, 0.1292274648535926551 ) ) ;
#20599 = CARTESIAN_POINT ( 'NONE',  ( -0.8398950131233585692, 0.2306618581243848609, 0.2411417322834645549 ) ) ;
#20600 = CARTESIAN_POINT ( 'NONE',  ( -1.148293963254592542, -0.6692913385826773087, -0.1292274648535924053 ) ) ;
#20601 = CARTESIAN_POINT ( 'NONE',  ( 1.187664041994751285, -0.08942795157527998196, 0.3641732283464567121 ) ) ;
#20602 = CARTESIAN_POINT ( 'NONE',  ( 0.000000000000000000, 0.000000000000000000, 0.000000000000000000 ) ) ;
#20603 = DIRECTION ( 'NONE',  ( 0.000000000000000000, 0.000000000000000000, -1.000000000000000000 ) ) ;
#20604 = CARTESIAN_POINT ( 'NONE',  ( 0.9580052493438326877, -0.004921259842519576551, 0.3153832671262227771 ) ) ;
#20605 = CONICAL_SURFACE ( 'NONE', #11172, 0.1190944881889763746, 0.8726646259971653219 ) ;
#20606 = CARTESIAN_POINT ( 'NONE',  ( 0.2821522309711292364, 0.2952755905511810774, -0.1292274648535930714 ) ) ;
#20607 = CARTESIAN_POINT ( 'NONE',  ( 0.8333333333333340365, -0.6692913385826771977, 0.1292274648535927661 ) ) ;
#20608 = CARTESIAN_POINT ( 'NONE',  ( -0.3996062992125987146, 0.1070741851644051862, -1.292650918635170454 ) ) ;
#20609 = CARTESIAN_POINT ( 'NONE',  ( -1.719160104986876103, 0.05413385826771666132, 0.4176697321401328100 ) ) ;
#20610 = CARTESIAN_POINT ( 'NONE',  ( -0.2925321140481930149, -0.2925321140481933480, -0.7657480314960628531 ) ) ;
#20611 = CARTESIAN_POINT ( 'NONE',  ( 0.1998031496062992463, 0.3460692066303959202, -0.5360892388451443669 ) ) ;
#20612 = CARTESIAN_POINT ( 'NONE',  ( -0.6758530183727028406, -0.6692913385826773087, -0.1292274648535924053 ) ) ;
#20613 = CARTESIAN_POINT ( 'NONE',  ( -0.4091458600556402980, -0.2362204724409451284, -0.2099737532808398921 ) ) ;
#20614 = CARTESIAN_POINT ( 'NONE',  ( 0.3917322834645670104, 2.398668435337828261E-17, -2.250000000000000000 ) ) ;
#20615 = CARTESIAN_POINT ( 'NONE',  ( -1.049868766404198794, -0.5023911411419708095, 0.1820866141732285504 ) ) ;
#20616 = CARTESIAN_POINT ( 'NONE',  ( 1.463254593175853824, 0.2952755905511810774, -0.1292274648535930714 ) ) ;
#20617 = CARTESIAN_POINT ( 'NONE',  ( 1.108923884514436686, -0.3162353388693409650, -0.4822834645669289433 ) ) ;
#20618 = CARTESIAN_POINT ( 'NONE',  ( -0.1181102362204717315, -0.5511811023622047445, 6.969142054262312111E-17 ) ) ;
#20619 = CARTESIAN_POINT ( 'NONE',  ( 0.5446194225721792126, -0.05778040916215560624, -0.4822834645669293319 ) ) ;
#20620 = CARTESIAN_POINT ( 'NONE',  ( 0.3458507752293908943, -0.3458507752293908943, -1.750000000000000222 ) ) ;
#20621 = CARTESIAN_POINT ( 'NONE',  ( -0.2362204724409440182, -0.1870078740157479769, 0.3641732283464567677 ) ) ;
#20622 = CARTESIAN_POINT ( 'NONE',  ( -0.1115485564304456306, 0.2952755905511810774, -0.1292274648535930714 ) ) ;
#20623 = VECTOR ( 'NONE', #44219, 39.37007874015748854 ) ;
#20624 = CARTESIAN_POINT ( 'NONE',  ( -0.3949938075777409963, -7.255918531996591613E-17, -1.533464566929133577 ) ) ;
#20625 = CARTESIAN_POINT ( 'NONE',  ( -1.181102362204723644, -0.1870078740157480879, -0.4822834645669291653 ) ) ;
#20626 = CARTESIAN_POINT ( 'NONE',  ( 0.6758530183727039509, 0.1771653543307087075, -0.09757992244046823083 ) ) ;
#20627 = LINE ( 'NONE', #45438, #6328 ) ;
#20628 = CARTESIAN_POINT ( 'NONE',  ( -0.7152230971128602510, -0.05778040916215560624, -0.4822834645669293319 ) ) ;
#20629 = CARTESIAN_POINT ( 'NONE',  ( -0.2952755905511803003, -0.4536011799217368745, -0.2665933059059886201 ) ) ;
#20630 = CARTESIAN_POINT ( 'NONE',  ( -1.595398199321657717, 0.4619154201552267414, -0.1559797534342468872 ) ) ;
#20631 = CARTESIAN_POINT ( 'NONE',  ( -0.8398950131233589023, -0.6046776061558809534, -0.2411417322834644161 ) ) ;
#20632 = CARTESIAN_POINT ( 'NONE',  ( -0.4527559055118102749, -0.5400638737290845981, -0.3530559997133363437 ) ) ;
#20633 = CARTESIAN_POINT ( 'NONE',  ( 0.01312335958005323398, -0.4281496062992127816, -0.4176697321401328100 ) ) ;
#20634 = CARTESIAN_POINT ( 'NONE',  ( 0.1998031496062994128, -0.3460692066303957537, -2.373359580052493367 ) ) ;
#20635 = CARTESIAN_POINT ( 'NONE',  ( -0.1049643490035301746, -0.3917322834645670659, -2.199455749834958951 ) ) ;
#20636 = DIRECTION ( 'NONE',  ( 0.000000000000000000, 0.000000000000000000, 1.000000000000000000 ) ) ;
#20637 = CARTESIAN_POINT ( 'NONE',  ( 0.8464566929133866546, -0.4536011799217367080, 0.2665933059059888421 ) ) ;
#20638 = CARTESIAN_POINT ( 'NONE',  ( 1.574803149606299746, -0.1870078740157479769, 0.4822834645669291653 ) ) ;
#20639 = CARTESIAN_POINT ( 'NONE',  ( -0.7152230971128602510, -0.08942795157528024563, -0.3641732283464568787 ) ) ;
#20640 = CARTESIAN_POINT ( 'NONE',  ( -1.010498687664041384, -0.3690944881889765550, -0.3153832671262227771 ) ) ;
#20641 = CARTESIAN_POINT ( 'NONE',  ( -0.7217847769028863381, -0.4281496062992124485, 0.4176697321401328655 ) ) ;
#20642 = CARTESIAN_POINT ( 'NONE',  ( -0.06561679790026180015, -0.4281496062992127816, -0.4176697321401328100 ) ) ;
#20643 = CARTESIAN_POINT ( 'NONE',  ( 0.6102362204724416372, 0.07958543189024071263, -0.2665933059059888421 ) ) ;
#20644 = CARTESIAN_POINT ( 'NONE',  ( -0.2362173824511233644, 0.1771694743175191988, 5.690029434716977974 ) ) ;
#20645 = CARTESIAN_POINT ( 'NONE',  ( 1.102362204724410155, -0.1870078740157479769, 0.3641732283464567677 ) ) ;
#20646 = CARTESIAN_POINT ( 'NONE',  ( 0.4855643044619430415, -0.4281496062992127816, -0.4176697321401328100 ) ) ;
#20647 = CARTESIAN_POINT ( 'NONE',  ( -9.787531504996566615E-17, 0.3996062992125985480, 0.08070866141732283006 ) ) ;
#20648 = ADVANCED_FACE ( 'NONE', ( #73620 ), #42018, .F. ) ;
#20649 = CARTESIAN_POINT ( 'NONE',  ( -0.6692913385826764205, -0.6692913385826771977, 8.415575281601705876E-17 ) ) ;
#20650 = CARTESIAN_POINT ( 'NONE',  ( 0.3392501089628018884, -0.1958661417322834220, -1.291994750656167978 ) ) ;
#20651 = CARTESIAN_POINT ( 'NONE',  ( 1.259842519685040019, -0.1870078740157479769, 0.3641732283464567677 ) ) ;
#20652 = CARTESIAN_POINT ( 'NONE',  ( 0.3149606299212606708, -0.1870078740157480879, -0.4822834645669291653 ) ) ;
#20653 = CARTESIAN_POINT ( 'NONE',  ( 0.01968503937007957949, -0.5400638737290845981, -0.3530559997133363437 ) ) ;
#20654 = CARTESIAN_POINT ( 'NONE',  ( -0.05905511811023545637, 0.07958543189024085140, 0.2665933059059887866 ) ) ;
#20655 = CARTESIAN_POINT ( 'NONE',  ( 1.114781747626347963, 3.405574981839577511E-16, 0.3464511005275203726 ) ) ;
#20656 = CARTESIAN_POINT ( 'NONE',  ( -0.1640419947506553400, -0.08942795157528024563, -0.3641732283464568787 ) ) ;
#20657 = CARTESIAN_POINT ( 'NONE',  ( 0.6430446194225729606, -0.4281496062992127816, -0.4176697321401328100 ) ) ;
#20658 = CARTESIAN_POINT ( 'NONE',  ( -0.9514435695538050464, -0.2845877964562159024, 0.3641732283464567677 ) ) ;
#20659 = CARTESIAN_POINT ( 'NONE',  ( -0.8792650918635160906, -0.4281496062992124485, 0.4176697321401328655 ) ) ;
#20660 = CARTESIAN_POINT ( 'NONE',  ( 0.1698998578625684763, 0.000000000000000000, 0.3464511005275205946 ) ) ;
#20661 = ORIENTED_EDGE ( 'NONE', *, *, #13568, .T. ) ;
#20662 = CARTESIAN_POINT ( 'NONE',  ( -1.207349081364828436, -0.6046776061558807314, 0.2411417322834647770 ) ) ;
#20663 = AXIS2_PLACEMENT_3D ( 'NONE', #57987, #7924, #63897 ) ;
#20664 = CARTESIAN_POINT ( 'NONE',  ( -1.318897637795274802, -0.4536011799217368745, -0.2665933059059886201 ) ) ;
#20665 = CARTESIAN_POINT ( 'NONE',  ( 0.03280839895013198948, 0.2952755905511811885, 0.1292274648535926551 ) ) ;
#20666 = CARTESIAN_POINT ( 'NONE',  ( -1.587926509186350810, -0.4281496062992124485, 0.4176697321401328655 ) ) ;
#20667 = CARTESIAN_POINT ( 'NONE',  ( -0.6167979002624665030, -0.4281496062992127816, -0.4176697321401328100 ) ) ;
#20668 = CARTESIAN_POINT ( 'NONE',  ( -0.4498537592782897998, 0.000000000000000000, -2.118110236220472675 ) ) ;
#20670 = CARTESIAN_POINT ( 'NONE',  ( 0.9383202099737536495, -0.3162353388693405765, 0.4822834645669290543 ) ) ;
#20669 = CARTESIAN_POINT ( 'NONE',  ( 1.692913385826772421, 0.2952755905511811885, 0.000000000000000000 ) ) ;
#20671 = CARTESIAN_POINT ( 'NONE',  ( 0.8398950131233602345, -0.6046776061558807314, 0.2411417322834647770 ) ) ;
#20672 = CARTESIAN_POINT ( 'NONE',  ( -0.2867679344610364334, -0.2867679344610367109, -2.570866141732283339 ) ) ;
#20673 = CARTESIAN_POINT ( 'NONE',  ( -1.614173228346457378, 1.330640075373402897, 0.1372047244094476981 ) ) ;
#20674 = CARTESIAN_POINT ( 'NONE',  ( -1.502624671916009680, -0.05778040916215560624, -0.4822834645669293319 ) ) ;
#20675 = CARTESIAN_POINT ( 'NONE',  ( -0.1070741851644051862, -0.3996062992125987146, -0.2296587926509186528 ) ) ;
#20676 = VERTEX_POINT ( 'NONE', #10470 ) ;
#20677 = CARTESIAN_POINT ( 'NONE',  ( -0.3805774278215216522, -0.004921259842519576551, 0.3153832671262227771 ) ) ;
#20679 = CARTESIAN_POINT ( 'NONE',  ( 0.1049643490035304938, -0.3917322834645669549, -1.809711286089239035 ) ) ;
#20678 = CONICAL_SURFACE ( 'NONE', #31405, 2.559055118110236560, 0.7853981633974500554 ) ;
#20680 = ORIENTED_EDGE ( 'NONE', *, *, #53659, .T. ) ;
#20681 = CARTESIAN_POINT ( 'NONE',  ( 0.4002624671916016896, -0.3162353388693409650, -0.4822834645669289433 ) ) ;
#20682 = CARTESIAN_POINT ( 'NONE',  ( -0.03280839895013062252, -0.6692913385826771977, 0.1292274648535927661 ) ) ;
#20683 = CARTESIAN_POINT ( 'NONE',  ( -0.5971128608923877978, -0.6692913385826773087, -0.1292274648535924053 ) ) ;
#20684 = CARTESIAN_POINT ( 'NONE',  ( 1.305774278215223960, -0.6692913385826771977, 0.1292274648535927661 ) ) ;
#20685 = CARTESIAN_POINT ( 'NONE',  ( -0.7480314960629914633, -0.5511811023622047445, 6.969142054262312111E-17 ) ) ;
#20686 = CARTESIAN_POINT ( 'NONE',  ( 0.5643044619422579178, 0.05413385826771666132, 0.4176697321401328100 ) ) ;
#20687 = EDGE_CURVE ( 'NONE', #29367, #82700, #38092, .T. ) ;
#20688 = CARTESIAN_POINT ( 'NONE',  ( 0.5774278215223103139, -0.5023911411419708095, -0.1820866141732282451 ) ) ;
#20689 = CARTESIAN_POINT ( 'NONE',  ( -0.5118110236220466680, 0.2952755905511811885, 0.000000000000000000 ) ) ;
#20690 = CARTESIAN_POINT ( 'NONE',  ( 0.1049643490035304522, -0.3917322834645668994, -0.9527365897299718833 ) ) ;
#20691 = CARTESIAN_POINT ( 'NONE',  ( -0.7808398950131222316, -0.3162353388693409650, -0.4822834645669289433 ) ) ;
#20692 = DIRECTION ( 'NONE',  ( 0.000000000000000000, 1.000000000000000000, -0.000000000000000000 ) ) ;
#20693 = CARTESIAN_POINT ( 'NONE',  ( 1.515748031496063408, 0.1660481256975885056, 0.3530559997133364547 ) ) ;
#20694 = CARTESIAN_POINT ( 'NONE',  ( 1.541994750656168645, 0.1771653543307087075, -0.09757992244046823083 ) ) ;
#20695 = ORIENTED_EDGE ( 'NONE', *, *, #65801, .T. ) ;
#20696 = CARTESIAN_POINT ( 'NONE',  ( 4.797336870675656522E-17, -0.3917322834645670659, -2.437683357776589510 ) ) ;
#20698 = B_SPLINE_CURVE_WITH_KNOTS ( 'NONE', 3,
 ( #27657, #79861, #21351, #47004, #22178, #72698, #17940, #29318, #49903, #23000, #10392, #9965 ),
 .UNSPECIFIED., .F., .F.,
 ( 4, 2, 2, 2, 2, 4 ),
 ( 0.05454303362711770270, 0.05585633982237129397, 0.05651299291999809654, 0.05716964601762489911, 0.05848295221287848344, 0.05979625840813206777 ),
 .UNSPECIFIED. ) ;
#20697 = CARTESIAN_POINT ( 'NONE',  ( 0.01312335958005323398, -0.4281496062992127816, -0.4176697321401328100 ) ) ;
#20699 = ORIENTED_EDGE ( 'NONE', *, *, #60494, .F. ) ;
#20700 = CARTESIAN_POINT ( 'NONE',  ( -1.338582677165353729, -0.1870078740157480879, -0.4822834645669291653 ) ) ;
#20701 = CARTESIAN_POINT ( 'NONE',  ( 1.240157480314961314, -0.5400638737290844871, 0.3530559997133364547 ) ) ;
#20702 = CARTESIAN_POINT ( 'NONE',  ( 1.135170603674541256, 0.2952755905511811885, 0.1292274648535926551 ) ) ;
#20703 = CARTESIAN_POINT ( 'NONE',  ( 0.2559055118110243332, -0.5400638737290845981, -0.3530559997133363437 ) ) ;
#20704 = CARTESIAN_POINT ( 'NONE',  ( -0.4002624671916004129, -0.3162353388693405765, 0.4822834645669290543 ) ) ;
#20705 = CARTESIAN_POINT ( 'NONE',  ( -0.1049643490035307020, 0.3917322834645669549, -1.666010498687664043 ) ) ;
#20706 = CARTESIAN_POINT ( 'NONE',  ( -1.194225721784776262, 0.05413385826771626580, -0.4176697321401330321 ) ) ;
#20707 = CARTESIAN_POINT ( 'NONE',  ( -0.7545931758530176614, -0.6692913385826773087, -0.1292274648535924053 ) ) ;
#20708 = CARTESIAN_POINT ( 'NONE',  ( -0.1115485564304453947, -0.5511811023622046335, 0.09757992244046803654 ) ) ;
#20709 = CARTESIAN_POINT ( 'NONE',  ( 1.541994750656168645, 0.2952755905511810774, -0.1292274648535930714 ) ) ;
#20710 = CARTESIAN_POINT ( 'NONE',  ( -0.5052493438320203589, -0.6692913385826771977, 0.1292274648535927661 ) ) ;
#20711 = CARTESIAN_POINT ( 'NONE',  ( 0.3018372703412079971, 0.009842519685039147898, -0.3409548833797004797 ) ) ;
#20712 = B_SPLINE_CURVE_WITH_KNOTS ( 'NONE', 3,
 ( #26859, #1209, #52518, #8757 ),
 .UNSPECIFIED., .F., .F.,
 ( 4, 4 ),
 ( 3.210432057665806998E-07, 0.001287787053612119391 ),
 .UNSPECIFIED. ) ;
#20713 = CARTESIAN_POINT ( 'NONE',  ( 0.6233595800524939223, -0.3162353388693405765, 0.4822834645669290543 ) ) ;
#20714 = CARTESIAN_POINT ( 'NONE',  ( 3.923605715242195480, 1.191231191135928791, -0.3247605523133955674 ) ) ;
#20715 = EDGE_CURVE ( 'NONE', #51820, #41668, #80338, .T. ) ;
#20716 = CARTESIAN_POINT ( 'NONE',  ( 0.03280839895013198948, -0.6692913385826773087, -0.1292274648535924053 ) ) ;
#20717 = CARTESIAN_POINT ( 'NONE',  ( -0.2755905511811018171, 0.1771653543307087630, 0.000000000000000000 ) ) ;
#20719 = CARTESIAN_POINT ( 'NONE',  ( -1.614173228346457378, 0.7794589730111968207, -0.1372047244094477536 ) ) ;
#20718 = CARTESIAN_POINT ( 'NONE',  ( 0.9120734908136490793, 0.1771653543307087075, -0.09757992244046823083 ) ) ;
#20720 = CARTESIAN_POINT ( 'NONE',  ( 0.4724409448818896462, 0.1265901696524990294, -0.3589238845144357426 ) ) ;
#20721 = CARTESIAN_POINT ( 'NONE',  ( 1.509186351706037543, -0.004921259842519576551, 0.3153832671262227771 ) ) ;
#20722 = CARTESIAN_POINT ( 'NONE',  ( 1.345144356955381593, -0.3162353388693409650, -0.4822834645669289433 ) ) ;
#20723 = CARTESIAN_POINT ( 'NONE',  ( 0.1974969037888704704, 0.3420746716998660508, -0.2211286089238845842 ) ) ;
#20724 = CARTESIAN_POINT ( 'NONE',  ( -0.03280839895013062252, -0.6692913385826771977, 0.1292274648535927661 ) ) ;
#20725 = CARTESIAN_POINT ( 'NONE',  ( -1.469816272965878357, 0.2306618581243848609, 0.2411417322834645549 ) ) ;
#20726 = VECTOR ( 'NONE', #64680, 39.37007874015748143 ) ;
#20727 = CARTESIAN_POINT ( 'NONE',  ( -1.568241469816272105, -0.05778040916215522460, 0.4822834645669289988 ) ) ;
#20728 = CARTESIAN_POINT ( 'NONE',  ( -0.1574803149606292529, -0.1870078740157479769, 0.4822834645669291653 ) ) ;
#20729 = CARTESIAN_POINT ( 'NONE',  ( -0.3949938075777409963, -7.255918531996591613E-17, -0.1161417322834646104 ) ) ;
#20730 = CARTESIAN_POINT ( 'NONE',  ( -1.620734908136482577, 0.1771653543307087630, 0.09757992244046791164 ) ) ;
#20731 = CARTESIAN_POINT ( 'NONE',  ( 0.4658792650918640033, -0.3162353388693405765, 0.4822834645669290543 ) ) ;
#20732 = CARTESIAN_POINT ( 'NONE',  ( 0.9055118110236227702, 0.1771653543307087630, 0.000000000000000000 ) ) ;
#20733 = CARTESIAN_POINT ( 'NONE',  ( 0.2527386706991758825, 1.111414106920971090, 0.1849575905693944811 ) ) ;
#20734 = CARTESIAN_POINT ( 'NONE',  ( 0.3805774278215230400, -0.3690944881889763329, 0.3153832671262228327 ) ) ;
#20735 = CARTESIAN_POINT ( 'NONE',  ( -1.377952755905511140, -0.6692913385826771977, 8.415575281601705876E-17 ) ) ;
#20736 = CARTESIAN_POINT ( 'NONE',  ( 0.1998031496062992463, 0.3460692066303959202, -0.8510498687664042050 ) ) ;
#20737 = CARTESIAN_POINT ( 'NONE',  ( 1.292650918635171564, -0.6692913385826773087, -0.1292274648535924053 ) ) ;
#20738 = CARTESIAN_POINT ( 'NONE',  ( 0.3917322834645670104, 2.398668435337828261E-17, -0.5826771653543306728 ) ) ;
#20740 = CARTESIAN_POINT ( 'NONE',  ( 1.374111565972423831E-16, 0.4374015748031496176, -1.122047244094488194 ) ) ;
#20739 = CARTESIAN_POINT ( 'NONE',  ( 0.2296587926509192634, -0.3162353388693405765, 0.4822834645669290543 ) ) ;
#20741 = PLANE ( 'NONE',  #18694 ) ;
#20742 = CARTESIAN_POINT ( 'NONE',  ( 0.4396325459317590445, -0.5511811023622046335, 0.09757992244046803654 ) ) ;
#20743 = CIRCLE ( 'NONE', #4567, 0.5118110236220472231 ) ;
#20744 = CARTESIAN_POINT ( 'NONE',  ( 0.4724409448818904789, -0.1870078740157480879, -0.4822834645669291653 ) ) ;
#20745 = CARTESIAN_POINT ( 'NONE',  ( -0.2544983382031791863, 0.1500752278769512393, 0.1555222293686583102 ) ) ;
#20746 = CARTESIAN_POINT ( 'NONE',  ( -0.9186351706036736120, 0.1283753931104748280, 0.1820866141732283561 ) ) ;
#20747 = CARTESIAN_POINT ( 'NONE',  ( -1.227034120734907585, 0.2952755905511811885, 0.1292274648535926551 ) ) ;
#20748 = CARTESIAN_POINT ( 'NONE',  ( -1.646981627296586703, -0.3162353388693409650, -0.4822834645669289433 ) ) ;
#20749 = CARTESIAN_POINT ( 'NONE',  ( 1.049868766404200349, 0.2306618581243848609, 0.2411417322834645549 ) ) ;
#20750 = CARTESIAN_POINT ( 'NONE',  ( 1.666666666666667185, 0.05413385826771666132, 0.4176697321401328100 ) ) ;
#20751 = CARTESIAN_POINT ( 'NONE',  ( -0.3959418824714271423, -0.02190130575838673821, -1.220472440944882386 ) ) ;
#20752 = CARTESIAN_POINT ( 'NONE',  ( 0.4855643044619428750, 0.05413385826771666132, 0.4176697321401328100 ) ) ;
#20753 = CARTESIAN_POINT ( 'NONE',  ( -0.1265901696524993347, 0.4724409448818895907, -2.760498687664041384 ) ) ;
#20754 = CARTESIAN_POINT ( 'NONE',  ( 1.627296587926509996, -0.6046776061558807314, 0.2411417322834647770 ) ) ;
#20755 = CARTESIAN_POINT ( 'NONE',  ( 1.561679790026247350, 0.05413385826771626580, -0.4176697321401330321 ) ) ;
#20756 = CARTESIAN_POINT ( 'NONE',  ( -1.568241469816272105, -0.08942795157527998196, 0.3641732283464567121 ) ) ;
#20757 = CARTESIAN_POINT ( 'NONE',  ( 1.076115485564305141, 0.1283753931104746893, -0.1820866141732285504 ) ) ;
#20758 = CARTESIAN_POINT ( 'NONE',  ( -1.148293963254592542, 0.1771653543307087630, 0.09757992244046791164 ) ) ;
#20759 = CARTESIAN_POINT ( 'NONE',  ( -0.2493438320209966919, -0.3690944881889763329, 0.3153832671262228327 ) ) ;
#20760 = CARTESIAN_POINT ( 'NONE',  ( -3.197598481144914739, 2.742783271388837374, 0.5314960629921260393 ) ) ;
#20761 = CARTESIAN_POINT ( 'NONE',  ( 0.4790026246719167324, -0.08942795157527998196, 0.3641732283464567121 ) ) ;
#20762 = CARTESIAN_POINT ( 'NONE',  ( 0.5511811023622055217, -0.1870078740157479769, 0.4822834645669291653 ) ) ;
#20763 = CARTESIAN_POINT ( 'NONE',  ( 1.056430446194226436, -0.6692913385826773087, -0.1292274648535924053 ) ) ;
#20764 = CARTESIAN_POINT ( 'NONE',  ( 0.07217847769028949700, -0.3162353388693405765, 0.4822834645669290543 ) ) ;
#20765 = CARTESIAN_POINT ( 'NONE',  ( -0.03280839895013062252, -0.5511811023622046335, 0.09757992244046803654 ) ) ;
#20766 = CARTESIAN_POINT ( 'NONE',  ( 1.135170603674541256, 0.2952755905511811885, 0.1292274648535926551 ) ) ;
#20767 = CARTESIAN_POINT ( 'NONE',  ( -0.9448818897637790704, -0.1870078740157479769, 0.4822834645669291653 ) ) ;
#20768 = CARTESIAN_POINT ( 'NONE',  ( -0.3996062992125986590, 0.1070741851644051862, -0.8202099737532806412 ) ) ;
#20769 = CARTESIAN_POINT ( 'NONE',  ( 0.1265901696524989184, 0.4724409448818898127, -1.172572178477690352 ) ) ;
#20770 = CARTESIAN_POINT ( 'NONE',  ( 0.03937007874015806264, 0.2952755905511811885, 0.000000000000000000 ) ) ;
#20771 = CARTESIAN_POINT ( 'NONE',  ( -0.6102362204724400829, -0.5400638737290845981, -0.3530559997133363437 ) ) ;
#20772 = CARTESIAN_POINT ( 'NONE',  ( -0.07874015748031421014, -0.1870078740157480879, -0.4822834645669291653 ) ) ;
#20773 = CARTESIAN_POINT ( 'NONE',  ( -0.1070741851644056997, 0.3996062992125986035, -2.683727034120735322 ) ) ;
#20774 = CARTESIAN_POINT ( 'NONE',  ( 0.1058382717557499880, 0.3949938075777411073, -1.883202099737532720 ) ) ;
#20775 = CARTESIAN_POINT ( 'NONE',  ( 0.2867679344610365999, -0.2867679344610365444, -0.7204724409448818312 ) ) ;
#20776 = CARTESIAN_POINT ( 'NONE',  ( 0.3392501089628018884, -0.1958661417322834220, -1.199475065616797842 ) ) ;
#20777 = CARTESIAN_POINT ( 'NONE',  ( -0.9645669291338575535, -0.4536011799217367080, 0.2665933059059888421 ) ) ;
#20778 = CARTESIAN_POINT ( 'NONE',  ( -0.3917322834645669549, -0.1049643490035306603, -1.297900262467191590 ) ) ;
#20779 = CARTESIAN_POINT ( 'NONE',  ( -1.679790026246718693, 0.2306618581243847221, -0.2411417322834647770 ) ) ;
#20780 = CARTESIAN_POINT ( 'NONE',  ( 0.1958661417322834497, 0.3392501089628018329, 0.09057049688420130973 ) ) ;
#20781 = CARTESIAN_POINT ( 'NONE',  ( 0.2887139107611556010, 0.2306618581243847221, -0.2411417322834647770 ) ) ;
#20782 = CARTESIAN_POINT ( 'NONE',  ( -0.6889763779527552368, -0.4536011799217368745, -0.2665933059059886201 ) ) ;
#20783 = CARTESIAN_POINT ( 'NONE',  ( 1.056430446194226436, -0.6692913385826773087, -0.1292274648535924053 ) ) ;
#20784 = CARTESIAN_POINT ( 'NONE',  ( 0.4790026246719167324, -0.05778040916215522460, 0.4822834645669289988 ) ) ;
#20785 = CARTESIAN_POINT ( 'NONE',  ( 0.3136779242486383290, 1.181160616066996294, 1.077380321234679084 ) ) ;
#20786 = CARTESIAN_POINT ( 'NONE',  ( 0.2925321140481932369, -0.2925321140481932369, -2.775590551181101429 ) ) ;
#20787 = CARTESIAN_POINT ( 'NONE',  ( 4.797336870675656522E-17, -0.3917322834645670659, -1.020360523130920738 ) ) ;
#20788 = CARTESIAN_POINT ( 'NONE',  ( 1.358267716535433323, 0.1660481256975885056, 0.3530559997133364547 ) ) ;
#20789 = CARTESIAN_POINT ( 'NONE',  ( 0.5708661417322841158, -0.5400638737290845981, -0.3530559997133363437 ) ) ;
#20790 = CARTESIAN_POINT ( 'NONE',  ( 0.2296587926509192634, -0.05778040916215560624, -0.4822834645669293319 ) ) ;
#20791 = CARTESIAN_POINT ( 'NONE',  ( 1.469816272965879911, 0.2306618581243847221, -0.2411417322834647770 ) ) ;
#20792 = CARTESIAN_POINT ( 'NONE',  ( 0.7283464566929143125, 0.1660481256975885056, 0.3530559997133364547 ) ) ;
#20793 = CARTESIAN_POINT ( 'NONE',  ( -0.1049643490035307020, 0.3917322834645669549, -0.4061679790026246351 ) ) ;
#20794 = CARTESIAN_POINT ( 'NONE',  ( 0.1443569553805781891, -0.4281496062992124485, 0.4176697321401328655 ) ) ;
#20795 = CARTESIAN_POINT ( 'NONE',  ( 1.003937007874016407, -0.5400638737290844871, 0.3530559997133364547 ) ) ;
#20796 = CARTESIAN_POINT ( 'NONE',  ( 0.5774278215223104249, 0.2306618581243848609, 0.2411417322834645549 ) ) ;
#20797 = CARTESIAN_POINT ( 'NONE',  ( 1.305774278215223960, -0.5511811023622046335, 0.09757992244046803654 ) ) ;
#20798 = CARTESIAN_POINT ( 'NONE',  ( -1.423884514435694859, -0.3162353388693405765, 0.4822834645669290543 ) ) ;
#20799 = CARTESIAN_POINT ( 'NONE',  ( -1.555118110236219930, 0.1660481256975885056, 0.3530559997133364547 ) ) ;
#20800 = CARTESIAN_POINT ( 'NONE',  ( 0.8530183727034126306, 0.05413385826771626580, -0.4176697321401330321 ) ) ;
#20801 = CARTESIAN_POINT ( 'NONE',  ( -0.7270051398050848546, 2.375327444609086402, -0.4916655823645590950 ) ) ;
#20802 = CARTESIAN_POINT ( 'NONE',  ( -0.2867679344610364334, -0.2867679344610367109, -1.940944881889763884 ) ) ;
#20803 = VERTEX_POINT ( 'NONE', #18430 ) ;
#20804 = CARTESIAN_POINT ( 'NONE',  ( 4.893765752498283924E-17, -0.3996062992125986035, -0.5511811023622047445 ) ) ;
#20805 = ORIENTED_EDGE ( 'NONE', *, *, #24322, .T. ) ;
#20806 = CARTESIAN_POINT ( 'NONE',  ( 1.095800524934383846, -0.05778040916215560624, -0.4822834645669293319 ) ) ;
#20807 = CARTESIAN_POINT ( 'NONE',  ( 1.102362204724410155, -0.1870078740157479769, 0.3641732283464567677 ) ) ;
#20808 = CARTESIAN_POINT ( 'NONE',  ( 1.586052503253845281, 0.4724409448818907564, -0.1653254495020589354 ) ) ;
#20809 = ADVANCED_FACE ( 'NONE', ( #50389 ), #17719, .T. ) ;
#20810 = CARTESIAN_POINT ( 'NONE',  ( -0.1807843743677566839, 1.098495470880701985, 2.841284648355170361 ) ) ;
#20811 = CARTESIAN_POINT ( 'NONE',  ( 5.785732909357575061E-17, -0.4724409448818898682, -1.181102362204724310 ) ) ;
#20812 = CARTESIAN_POINT ( 'NONE',  ( -0.2867679344610364334, -0.2867679344610367109, -1.246062992125984481 ) ) ;
#20813 = CARTESIAN_POINT ( 'NONE',  ( 1.272965879265092637, 0.05413385826771666132, 0.4176697321401328100 ) ) ;
#20814 = CARTESIAN_POINT ( 'NONE',  ( -1.509186351706035767, -0.4281496062992124485, 0.4176697321401328655 ) ) ;
#20815 = CARTESIAN_POINT ( 'NONE',  ( -0.3937007874015740483, -0.1870078740157480879, -0.4822834645669291653 ) ) ;
#20816 = CARTESIAN_POINT ( 'NONE',  ( 1.128608923884514947, 0.2306618581243848609, 0.2411417322834645549 ) ) ;
#20817 = EDGE_LOOP ( 'NONE', ( #5154, #83226, #4631, #63824 ) ) ;
#20818 = CARTESIAN_POINT ( 'NONE',  ( -1.699475065616797398, 0.2952755905511811885, 0.1292274648535926551 ) ) ;
#20819 = CARTESIAN_POINT ( 'NONE',  ( -1.077529977636055181, 1.180708531484368162, -0.3131643582486707267 ) ) ;
#20820 = DIRECTION ( 'NONE',  ( 5.551115123125781470E-17, 1.000000000000000000, 5.814484458649070979E-31 ) ) ;
#20821 = CARTESIAN_POINT ( 'NONE',  ( 1.509186351706037543, -0.004921259842519576551, 0.3153832671262227771 ) ) ;
#20822 = DIRECTION ( 'NONE',  ( 0.000000000000000000, 0.000000000000000000, 1.000000000000000000 ) ) ;
#20823 = CARTESIAN_POINT ( 'NONE',  ( -0.8267716535433065062, 0.1771653543307087630, 0.000000000000000000 ) ) ;
#20824 = CARTESIAN_POINT ( 'NONE',  ( -1.423884514435694859, -0.05778040916215560624, -0.4822834645669293319 ) ) ;
#20825 = CARTESIAN_POINT ( 'NONE',  ( 0.6430446194225729606, -0.4281496062992127816, -0.4176697321401328100 ) ) ;
#20826 = ORIENTED_EDGE ( 'NONE', *, *, #82082, .F. ) ;
#20828 = DIRECTION ( 'NONE',  ( 0.000000000000000000, 0.000000000000000000, -1.000000000000000000 ) ) ;
#20827 = DIRECTION ( 'NONE',  ( 0.000000000000000000, 0.000000000000000000, 1.000000000000000000 ) ) ;
#20829 = EDGE_CURVE ( 'NONE', #28560, #11553, #53510, .T. ) ;
#20830 = CARTESIAN_POINT ( 'NONE',  ( 0.8530183727034128527, -0.4281496062992124485, 0.4176697321401328655 ) ) ;
#20831 = CARTESIAN_POINT ( 'NONE',  ( -1.633858267716534529, -0.5400638737290845981, -0.3530559997133363437 ) ) ;
#20832 = CARTESIAN_POINT ( 'NONE',  ( 0.3917322834645668994, -0.1049643490035303134, -0.6640226789688171705 ) ) ;
#20833 = CARTESIAN_POINT ( 'NONE',  ( -0.6036745406824141069, 0.1283753931104748280, 0.1820866141732283561 ) ) ;
#20834 = CARTESIAN_POINT ( 'NONE',  ( -1.535433070866141225, -0.5511811023622047445, 6.969142054262312111E-17 ) ) ;
#20835 = CARTESIAN_POINT ( 'NONE',  ( -0.3808816823641234528, 0.09156050430092053938, -1.220472440944881942 ) ) ;
#20837 = EDGE_CURVE ( 'NONE', #2386, #71433, #59828, .T. ) ;
#20836 = CARTESIAN_POINT ( 'NONE',  ( 0.4265091863517067039, -0.6692913385826773087, -0.1292274648535924053 ) ) ;
#20838 = CARTESIAN_POINT ( 'NONE',  ( -0.8136482939632537770, 0.1283753931104746893, -0.1820866141732285504 ) ) ;
#20839 = CARTESIAN_POINT ( 'NONE',  ( 0.2296587926509192634, -0.08942795157528024563, -0.3641732283464568787 ) ) ;
#20840 = CARTESIAN_POINT ( 'NONE',  ( -0.4330708661417315697, 0.2952755905511811885, 0.000000000000000000 ) ) ;
#20841 = CARTESIAN_POINT ( 'NONE',  ( -1.003937007874014853, 0.07958543189024085140, 0.2665933059059887866 ) ) ;
#20842 = CARTESIAN_POINT ( 'NONE',  ( 0.3392501089628018884, -0.1958661417322833942, -0.2592056674878758793 ) ) ;
#20843 = CARTESIAN_POINT ( 'NONE',  ( 0.8070866141732288002, 0.1660481256975885056, 0.3530559997133364547 ) ) ;
#20844 = CARTESIAN_POINT ( 'NONE',  ( 2.503252890251015828, 2.755905511811024056, 0.5314960629921260393 ) ) ;
#20845 = CARTESIAN_POINT ( 'NONE',  ( 0.4724409448818896462, 0.1265901696524990294, -1.618766404199474929 ) ) ;
#20846 = CARTESIAN_POINT ( 'NONE',  ( -0.9448818897637790704, -0.1870078740157479769, 0.4822834645669291653 ) ) ;
#20847 = CARTESIAN_POINT ( 'NONE',  ( -0.3215223097112853146, -0.2845877964562159024, 0.3641732283464567677 ) ) ;
#20848 = CARTESIAN_POINT ( 'NONE',  ( -1.443569553805773564, 0.2306618581243847221, -0.2411417322834647770 ) ) ;
#20849 = CARTESIAN_POINT ( 'NONE',  ( 0.7283464566929143125, 0.07958543189024085140, 0.2665933059059887866 ) ) ;
#20850 = AXIS2_PLACEMENT_3D ( 'NONE', #82305, #50701, #12420 ) ;
#20851 = CARTESIAN_POINT ( 'NONE',  ( -0.7414698162729651543, 0.1771653543307087075, -0.09757992244046823083 ) ) ;
#20852 = CARTESIAN_POINT ( 'NONE',  ( -0.8989501312335946848, 0.2952755905511810774, -0.1292274648535930714 ) ) ;
#20853 = CARTESIAN_POINT ( 'NONE',  ( -1.076115485564303809, 0.2306618581243848609, 0.2411417322834645549 ) ) ;
#20854 = CARTESIAN_POINT ( 'NONE',  ( 1.633858267716535639, -0.5400638737290844871, 0.3530559997133364547 ) ) ;
#20855 = CARTESIAN_POINT ( 'NONE',  ( -1.157146581871515012E-16, 0.4724409448818898682, -2.124015748031495843 ) ) ;
#20856 = CARTESIAN_POINT ( 'NONE',  ( 0.7742782152230979209, -0.004921259842519870586, -0.3153832671262229437 ) ) ;
#20857 = CARTESIAN_POINT ( 'NONE',  ( 0.5249343832021005074, -0.6046776061558807314, 0.2411417322834647770 ) ) ;
#20858 = CARTESIAN_POINT ( 'NONE',  ( -1.607611548556429737, 0.2952755905511810774, -0.1292274648535930714 ) ) ;
#20859 = CARTESIAN_POINT ( 'NONE',  ( -1.404199475065615932, 0.05413385826771666132, 0.4176697321401328100 ) ) ;
#20860 = EDGE_LOOP ( 'NONE', ( #57915, #71415, #65518, #1553 ) ) ;
#20861 = B_SPLINE_CURVE_WITH_KNOTS ( 'NONE', 3,
 ( #51834, #64903, #32914, #40068, #65755, #71637, #26603, #1769, #13153, #8502, #59413, #8088, #27851, #70800, #945, #33752 ),
 .UNSPECIFIED., .F., .F.,
 ( 4, 2, 2, 2, 2, 2, 2, 4 ),
 ( 0.000000000000000000, 0.0003923911760484576224, 0.0007847823520969152448, 0.001177173528145373030, 0.001569564704193830490, 0.001961955880242287949, 0.002354347056290746060, 0.003139129408387677025 ),
 .UNSPECIFIED. ) ;
#20862 = EDGE_CURVE ( 'NONE', #38184, #24792, #42396, .T. ) ;
#20863 = CARTESIAN_POINT ( 'NONE',  ( 0.1998031496062994128, -0.3460692066303957537, -2.688320209973753538 ) ) ;
#20864 = CARTESIAN_POINT ( 'NONE',  ( -1.187664041994749731, -0.2845877964562159024, 0.3641732283464567677 ) ) ;
#20865 = CARTESIAN_POINT ( 'NONE',  ( -0.5183727034120726440, 0.2952755905511811885, 0.1292274648535926551 ) ) ;
#20866 = CARTESIAN_POINT ( 'NONE',  ( 0.8661417322834652488, -0.1870078740157480879, -0.4822834645669291653 ) ) ;
#20867 = CARTESIAN_POINT ( 'NONE',  ( -1.364829396325458521, 0.1283753931104746893, -0.1820866141732285504 ) ) ;
#20868 = CARTESIAN_POINT ( 'NONE',  ( 0.1070741851644054776, -0.3996062992125984925, -1.736876640419947826 ) ) ;
#20869 = CARTESIAN_POINT ( 'NONE',  ( -1.259842519685038686, -0.1870078740157479769, 0.4822834645669291653 ) ) ;
#20870 = CARTESIAN_POINT ( 'NONE',  ( 0.4921259842519691285, -0.5400638737290845981, -0.3530559997133363437 ) ) ;
#20871 = CARTESIAN_POINT ( 'NONE',  ( 0.3477690288713918276, -0.6692913385826773087, -0.1292274648535924053 ) ) ;
#20872 = CARTESIAN_POINT ( 'NONE',  ( 1.167979002624672580, 0.05413385826771626580, -0.4176697321401330321 ) ) ;
#20873 = CARTESIAN_POINT ( 'NONE',  ( 1.092343761084413556, 1.535433070866141447, -0.6033564923654646250 ) ) ;
#20875 = EDGE_CURVE ( 'NONE', #55882, #11181, #2601, .T. ) ;
#20874 = CARTESIAN_POINT ( 'NONE',  ( 0.3460692066303959202, 0.1998031496062993295, -1.233595800524934338 ) ) ;
#20876 = CARTESIAN_POINT ( 'NONE',  ( 0.2891555358219910499, -0.2891555358219909944, -0.7283464566929134243 ) ) ;
#20877 = CARTESIAN_POINT ( 'NONE',  ( 0.3025936627584911998, 1.171974003123068542, -1.693908891378735015 ) ) ;
#20878 = CARTESIAN_POINT ( 'NONE',  ( 0.2296587926509192634, -0.08942795157528024563, -0.3641732283464568787 ) ) ;
#20879 = CARTESIAN_POINT ( 'NONE',  ( 0.2362204724409456558, -0.1870078740157480879, -0.4822834645669291653 ) ) ;
#20880 = CARTESIAN_POINT ( 'NONE',  ( 1.469816272965879911, 0.2306618581243847221, -0.2411417322834647770 ) ) ;
#20881 = CARTESIAN_POINT ( 'NONE',  ( -0.1058382717557497660, -0.3949938075777411073, -1.566272965879265344 ) ) ;
#20882 = CARTESIAN_POINT ( 'NONE',  ( 0.3412073490813655186, -0.5023911411419708095, -0.1820866141732282451 ) ) ;
#20883 = ADVANCED_FACE ( 'NONE', ( #34585 ), #57493, .F. ) ;
#20884 = CARTESIAN_POINT ( 'NONE',  ( -0.6102362204724400829, -0.5400638737290845981, -0.3530559997133363437 ) ) ;
#20885 = CARTESIAN_POINT ( 'NONE',  ( -1.620734908136482577, 0.2952755905511811885, 0.1292274648535926551 ) ) ;
#20886 = CARTESIAN_POINT ( 'NONE',  ( 0.3937007874015754361, -0.1870078740157479769, 0.4822834645669291653 ) ) ;
#20887 = CARTESIAN_POINT ( 'NONE',  ( -1.157146581871515012E-16, 0.4724409448818898682, -2.204724409448818978 ) ) ;
#20888 = CARTESIAN_POINT ( 'NONE',  ( 0.2502216998114611402, -0.3021538998228294748, -2.755905511811026720 ) ) ;
#20889 = ORIENTED_EDGE ( 'NONE', *, *, #69043, .F. ) ;
#20890 = ORIENTED_EDGE ( 'NONE', *, *, #1215, .T. ) ;
#20891 = CARTESIAN_POINT ( 'NONE',  ( 1.489501312335958172, -0.08942795157528024563, -0.3641732283464568787 ) ) ;
#20893 = CARTESIAN_POINT ( 'NONE',  ( -1.305774278215222184, 0.2952755905511811885, 0.1292274648535926551 ) ) ;
#20892 = CARTESIAN_POINT ( 'NONE',  ( -1.174540682414697335, -0.08942795157527998196, 0.3641732283464567121 ) ) ;
#20894 = CARTESIAN_POINT ( 'NONE',  ( 0.2867679344610365999, -0.2867679344610365999, -2.383182783955693829 ) ) ;
#20895 = CARTESIAN_POINT ( 'NONE',  ( 0.3996062992125986035, -0.1070741851644052972, -2.865485564304462329 ) ) ;
#20896 = CARTESIAN_POINT ( 'NONE',  ( 1.594488188976378673, -0.5400638737290845981, -0.3530559997133363437 ) ) ;
#20897 = CARTESIAN_POINT ( 'NONE',  ( -1.351706036745406347, 0.05413385826771626580, -0.4176697321401330321 ) ) ;
#20898 = CARTESIAN_POINT ( 'NONE',  ( 0.4724409448818904789, -0.1870078740157479769, 0.4822834645669291653 ) ) ;
#20899 = CARTESIAN_POINT ( 'NONE',  ( -1.332020997375327642, -0.05778040916215522460, 0.4822834645669289988 ) ) ;
#20900 = CARTESIAN_POINT ( 'NONE',  ( -0.3917322834645670659, 0.1049643490035301607, -2.790006930937320995 ) ) ;
#20901 = CARTESIAN_POINT ( 'NONE',  ( 0.7217847769028878924, -0.4281496062992127816, -0.4176697321401328100 ) ) ;
#20902 = CARTESIAN_POINT ( 'NONE',  ( 0.2867679344610365999, -0.2867679344610365444, -1.822834645669291653 ) ) ;
#20903 = CARTESIAN_POINT ( 'NONE',  ( -1.089238845144356427, -0.3690944881889765550, -0.3153832671262227771 ) ) ;
#20904 = ORIENTED_EDGE ( 'NONE', *, *, #22304, .T. ) ;
#20905 = CARTESIAN_POINT ( 'NONE',  ( 0.1974969037888706369, -0.3420746716998659953, -2.139107611548556331 ) ) ;
#20906 = VERTEX_POINT ( 'NONE', #5299 ) ;
#20907 = CARTESIAN_POINT ( 'NONE',  ( -1.692913385826770645, 0.1771653543307087630, 0.000000000000000000 ) ) ;
#20908 = CARTESIAN_POINT ( 'NONE',  ( -1.200787401574802349, 0.1660481256975883668, -0.3530559997133364547 ) ) ;
#20909 = CARTESIAN_POINT ( 'NONE',  ( -1.397637795275589623, -0.5400638737290845981, -0.3530559997133363437 ) ) ;
#20910 = CARTESIAN_POINT ( 'NONE',  ( 0.3460692066303959202, 0.1998031496062993295, -0.4461942257217847430 ) ) ;
#20911 = CARTESIAN_POINT ( 'NONE',  ( -1.719160104986876103, 0.05413385826771666132, 0.4176697321401328100 ) ) ;
#20912 = CARTESIAN_POINT ( 'NONE',  ( -1.633858267716534529, -0.5400638737290845981, -0.3530559997133363437 ) ) ;
#20913 = CARTESIAN_POINT ( 'NONE',  ( -1.338582677165353729, -0.1870078740157479769, 0.4822834645669291653 ) ) ;
#20914 = CARTESIAN_POINT ( 'NONE',  ( -0.3830016109920609813, -4.992347309556208597E-15, 0.4118484887281982920 ) ) ;
#20915 = CARTESIAN_POINT ( 'NONE',  ( 0.2362204724409456558, -0.1870078740157479769, 0.3641732283464567677 ) ) ;
#20916 = CARTESIAN_POINT ( 'NONE',  ( 0.5314960629920847390, 2.755905511811024056, 3.937007874015794773 ) ) ;
#20917 = CARTESIAN_POINT ( 'NONE',  ( 0.1049643490035304938, -0.3917322834645669549, -0.3274278215223098143 ) ) ;
#20918 = CARTESIAN_POINT ( 'NONE',  ( -0.9842519685039365918, -0.5511811023622047445, 6.969142054262312111E-17 ) ) ;
#20919 = CARTESIAN_POINT ( 'NONE',  ( -0.8923884514435688198, -0.6046776061558807314, 0.2411417322834647770 ) ) ;
#20920 = CARTESIAN_POINT ( 'NONE',  ( 0.7808398950131240079, -0.3162353388693405765, 0.4822834645669290543 ) ) ;
#20921 = CARTESIAN_POINT ( 'NONE',  ( -0.7480314960629914633, -0.6692913385826771977, 8.415575281601705876E-17 ) ) ;
#20922 = ORIENTED_EDGE ( 'NONE', *, *, #2281, .T. ) ;
#20923 = VERTEX_POINT ( 'NONE', #48667 ) ;
#20924 = CARTESIAN_POINT ( 'NONE',  ( -1.148293963254592542, 0.2952755905511811885, 0.1292274648535926551 ) ) ;
#20925 = CARTESIAN_POINT ( 'NONE',  ( 0.6824146981627303710, 0.2306618581243847221, -0.2411417322834647770 ) ) ;
#20926 = CARTESIAN_POINT ( 'NONE',  ( -1.594488188976377563, -0.4536011799217367080, 0.2665933059059888421 ) ) ;
#20927 = CARTESIAN_POINT ( 'NONE',  ( -0.3458507752293909498, 0.3458507752293907833, -1.279527559055118058 ) ) ;
#20928 = DIRECTION ( 'NONE',  ( 1.000000000000000000, 1.460819769243627131E-15, 0.000000000000000000 ) ) ;
#20929 = CARTESIAN_POINT ( 'NONE',  ( 0.3392501089628018884, -0.1958661417322834220, -0.4120734908136482466 ) ) ;
#20930 = CARTESIAN_POINT ( 'NONE',  ( -0.3392501089628017219, -0.1958661417322836718, -2.341863517060367439 ) ) ;
#20931 = CARTESIAN_POINT ( 'NONE',  ( -0.4724409448818890911, -0.1870078740157480879, -0.4822834645669291653 ) ) ;
#20932 = CARTESIAN_POINT ( 'NONE',  ( -1.568241469816272105, -0.2845877964562161244, -0.3641732283464567121 ) ) ;
#20933 = CARTESIAN_POINT ( 'NONE',  ( 0.2925321140481932369, 0.2925321140481932369, 0.1003937007874015491 ) ) ;
#20935 = LINE ( 'NONE', #33562, #61310 ) ;
#20934 = CARTESIAN_POINT ( 'NONE',  ( -1.502624671916009680, -0.05778040916215560624, -0.4822834645669293319 ) ) ;
#20936 = EDGE_CURVE ( 'NONE', #27207, #9799, #74364, .T. ) ;
#20937 = CARTESIAN_POINT ( 'NONE',  ( -1.305774278215222184, -0.6692913385826773087, -0.1292274648535924053 ) ) ;
#20938 = CARTESIAN_POINT ( 'NONE',  ( -0.4527559055118102749, 0.1660481256975885056, 0.3530559997133364547 ) ) ;
#20939 = CARTESIAN_POINT ( 'NONE',  ( 0.3949938075777409408, -0.1058382717557499186, -2.865485564304462329 ) ) ;
#20940 = CARTESIAN_POINT ( 'NONE',  ( 0.6364829396325465405, -0.08942795157527998196, 0.3641732283464567121 ) ) ;
#20941 = CARTESIAN_POINT ( 'NONE',  ( 3.912791665790199769, 1.724409448818897905, -0.4359958488159719758 ) ) ;
#20942 = CARTESIAN_POINT ( 'NONE',  ( 0.5380577427821529035, -0.3690944881889763329, 0.3153832671262228327 ) ) ;
#20943 = CARTESIAN_POINT ( 'NONE',  ( 1.358267716535433323, -0.4536011799217368745, -0.2665933059059886201 ) ) ;
#20944 = CARTESIAN_POINT ( 'NONE',  ( 0.8070866141732288002, 0.1660481256975885056, 0.3530559997133364547 ) ) ;
#20945 = PRODUCT_DEFINITION_CONTEXT ( 'detailed design', #2497, 'design' ) ;
#20946 = CARTESIAN_POINT ( 'NONE',  ( 0.2755905511811031494, 0.1771653543307087630, 0.000000000000000000 ) ) ;
#20947 = CARTESIAN_POINT ( 'NONE',  ( 0.2867679344610365999, 0.2867679344610365999, -2.019685039370078261 ) ) ;
#20948 = CARTESIAN_POINT ( 'NONE',  ( -1.181102362204723644, -0.1870078740157479769, 0.4822834645669291653 ) ) ;
#20949 = CARTESIAN_POINT ( 'NONE',  ( -0.04593175853018302557, -0.5511811023622048555, -0.09757992244046775898 ) ) ;
#20950 = CARTESIAN_POINT ( 'NONE',  ( 0.3458507752293908943, -0.3458507752293908943, -0.1751968503937007537 ) ) ;
#20951 = VECTOR ( 'NONE', #14667, 39.37007874015748143 ) ;
#20952 = CARTESIAN_POINT ( 'NONE',  ( -0.7086614173228339419, -0.1870078740157479769, 0.3641732283464567677 ) ) ;
#20953 = DIRECTION ( 'NONE',  ( -1.000000000000000000, -3.469446951953613696E-16, 0.000000000000000000 ) ) ;
#20954 = CARTESIAN_POINT ( 'NONE',  ( -0.01312335958005186876, 0.05413385826771626580, -0.4176697321401330321 ) ) ;
#20955 = CARTESIAN_POINT ( 'NONE',  ( -1.586052503253845503, 2.125984251968505045, -0.1653254495020588799 ) ) ;
#20956 = CARTESIAN_POINT ( 'NONE',  ( 0.6496062992125991586, 0.07958543189024085140, 0.2665933059059887866 ) ) ;
#20957 = CARTESIAN_POINT ( 'NONE',  ( -0.3608923884514428360, -0.5511811023622048555, -0.09757992244046775898 ) ) ;
#20958 = CARTESIAN_POINT ( 'NONE',  ( -0.2099737532808391705, 0.2306618581243848609, 0.2411417322834645549 ) ) ;
#20959 = DIRECTION ( 'NONE',  ( 1.000000000000000000, 0.000000000000000000, 0.000000000000000000 ) ) ;
#20960 = CARTESIAN_POINT ( 'NONE',  ( -0.9514435695538050464, -0.08942795157528024563, -0.3641732283464568787 ) ) ;
#20961 = CARTESIAN_POINT ( 'NONE',  ( 0.6758530183727039509, -0.6692913385826771977, 0.1292274648535927661 ) ) ;
#20962 = CARTESIAN_POINT ( 'NONE',  ( -0.7349081364829387342, -0.6046776061558807314, 0.2411417322834647770 ) ) ;
#20963 = CARTESIAN_POINT ( 'NONE',  ( 0.3996062992125985480, 2.446882876249141654E-17, -1.612204724409448842 ) ) ;
#20964 = CARTESIAN_POINT ( 'NONE',  ( -0.3917322834645670104, -7.196005306013484475E-17, -2.643700787401574548 ) ) ;
#20965 = CARTESIAN_POINT ( 'NONE',  ( 0.3280839895013130669, -0.004921259842519576551, 0.3153832671262227771 ) ) ;
#20966 = CARTESIAN_POINT ( 'NONE',  ( -1.325459317585300889, 0.05413385826771666132, 0.4176697321401328100 ) ) ;
#20967 = CARTESIAN_POINT ( 'NONE',  ( -1.187664041994749731, -0.2845877964562159024, 0.3641732283464567677 ) ) ;
#20968 = CARTESIAN_POINT ( 'NONE',  ( 1.627296587926509996, -0.6046776061558807314, 0.2411417322834647770 ) ) ;
#20969 = CARTESIAN_POINT ( 'NONE',  ( -0.7677165354330699465, -0.4536011799217368745, -0.2665933059059886201 ) ) ;
#20970 = CARTESIAN_POINT ( 'NONE',  ( -0.7349081364829390672, 0.1539470093639521697, -0.1968503937007875793 ) ) ;
#20971 = CARTESIAN_POINT ( 'NONE',  ( 0.9908136482939640111, 0.2952755905511810774, -0.1292274648535930714 ) ) ;
#20972 = CARTESIAN_POINT ( 'NONE',  ( -0.1070741851644051862, -0.3996062992125987146, 0.08530183727034119923 ) ) ;
#20973 = CARTESIAN_POINT ( 'NONE',  ( -0.3392501089628019995, 0.1958661417322831999, -2.542670234417010011 ) ) ;
#20974 = DIRECTION ( 'NONE',  ( 0.000000000000000000, 1.000000000000000000, 0.000000000000000000 ) ) ;
#20975 = CARTESIAN_POINT ( 'NONE',  ( 1.555118110236221041, -0.4536011799217367080, 0.2665933059059888421 ) ) ;
#20976 = CARTESIAN_POINT ( 'NONE',  ( -1.489501312335957062, -0.3162353388693409650, -0.4822834645669289433 ) ) ;
#20977 = CARTESIAN_POINT ( 'NONE',  ( 1.450131233595801428, 0.2952755905511811885, 0.1292274648535926551 ) ) ;
#20978 = CARTESIAN_POINT ( 'NONE',  ( 0.3392501089628018884, -0.1958661417322834220, -2.394356955380577467 ) ) ;
#20979 = CARTESIAN_POINT ( 'NONE',  ( 0.3503937007874015630, -0.3733313776025732333, -0.01968503937007903132 ) ) ;
#20980 = CARTESIAN_POINT ( 'NONE',  ( 0.3477690288713918276, -0.6692913385826773087, -0.1292274648535924053 ) ) ;
#20981 = CARTESIAN_POINT ( 'NONE',  ( -0.4527559055118102749, -0.5400638737290845981, -0.3530559997133363437 ) ) ;
#20982 = CARTESIAN_POINT ( 'NONE',  ( 1.548556430446194954, 0.2306618581243847221, -0.2411417322834647770 ) ) ;
#20983 = CARTESIAN_POINT ( 'NONE',  ( 0.1070741851644053666, 0.3996062992125986035, -2.040682414698162361 ) ) ;
#20984 = CARTESIAN_POINT ( 'NONE',  ( 0.5708661417322841158, -0.4536011799217368745, -0.2665933059059886201 ) ) ;
#20985 = CARTESIAN_POINT ( 'NONE',  ( 0.3460692066303959202, 0.1998031496062993295, -1.863517060367454015 ) ) ;
#20986 = ORIENTED_EDGE ( 'NONE', *, *, #58958, .T. ) ;
#20987 = CARTESIAN_POINT ( 'NONE',  ( 0.1958661417322836718, -0.3392501089628017219, -0.4035626228684533467 ) ) ;
#20988 = ORIENTED_EDGE ( 'NONE', *, *, #72187, .F. ) ;
#20989 = B_SPLINE_CURVE_WITH_KNOTS ( 'NONE', 1,
 ( #62620, #75674 ),
 .UNSPECIFIED., .F., .F.,
 ( 2, 2 ),
 ( 0.000000000000000000, 0.001849999999999997480 ),
 .UNSPECIFIED. ) ;
#20990 = CARTESIAN_POINT ( 'NONE',  ( 0.02624671916010564918, 0.2306618581243848609, 0.2411417322834645549 ) ) ;
#20991 = CARTESIAN_POINT ( 'NONE',  ( 1.213910761154856299, -0.6692913385826773087, -0.1292274648535924053 ) ) ;
#20992 = CARTESIAN_POINT ( 'NONE',  ( 0.1706036745406830368, -0.4281496062992127816, -0.4176697321401328100 ) ) ;
#20993 = CARTESIAN_POINT ( 'NONE',  ( -0.3018372703412066094, -0.3690944881889765550, -0.3153832671262227771 ) ) ;
#20994 = CARTESIAN_POINT ( 'NONE',  ( 1.062992125984252745, 0.2952755905511811885, 0.000000000000000000 ) ) ;
#20995 = CARTESIAN_POINT ( 'NONE',  ( -0.6102362204724400829, -0.5400638737290845981, -0.3530559997133363437 ) ) ;
#20996 = CARTESIAN_POINT ( 'NONE',  ( 0.1706036745406830368, 0.05413385826771666132, 0.4176697321401328100 ) ) ;
#20997 = CARTESIAN_POINT ( 'NONE',  ( 1.587926509186352142, 0.05413385826771666132, 0.4176697321401328100 ) ) ;
#20998 = CARTESIAN_POINT ( 'NONE',  ( 0.6955380577427828781, 0.05413385826771626580, -0.4176697321401330321 ) ) ;
#20999 = CARTESIAN_POINT ( 'NONE',  ( 1.384514435695538559, 0.2952755905511810774, -0.1292274648535930714 ) ) ;
#21000 = CARTESIAN_POINT ( 'NONE',  ( -0.2867679344610365999, 0.2867679344610364889, -0.4842519685039369248 ) ) ;
#21001 = CARTESIAN_POINT ( 'NONE',  ( 0.07874015748031558404, -0.1870078740157479769, 0.3641732283464567677 ) ) ;
#21002 = EDGE_LOOP ( 'NONE', ( #25873, #77401 ) ) ;
#21003 = CARTESIAN_POINT ( 'NONE',  ( 0.1058382717557499880, 0.3949938075777411073, -0.6233595800524935893 ) ) ;
#21004 = AXIS2_PLACEMENT_3D ( 'NONE', #14938, #2718, #28378 ) ;
#21005 = VERTEX_POINT ( 'NONE', #43994 ) ;
#21006 = CARTESIAN_POINT ( 'NONE',  ( -0.4199475065616791736, 0.1283753931104746893, -0.1820866141732285504 ) ) ;
#21007 = AXIS2_PLACEMENT_3D ( 'NONE', #26002, #77364, #26428 ) ;
#21008 = CARTESIAN_POINT ( 'NONE',  ( 0.09842519685039434474, 0.1660481256975885056, 0.3530559997133364547 ) ) ;
#21009 = CARTESIAN_POINT ( 'NONE',  ( -1.413425744192504663, 1.183688739992415417, 0.3163780376571070363 ) ) ;
#21010 = CARTESIAN_POINT ( 'NONE',  ( -0.2952755905511804668, 0.1660481256975885056, 0.3530559997133364547 ) ) ;
#21011 = CARTESIAN_POINT ( 'NONE',  ( -0.3871391076115479057, -0.3162353388693409650, -0.4822834645669289433 ) ) ;
#21012 = CARTESIAN_POINT ( 'NONE',  ( -0.8464566929133852113, 0.1660481256975885056, 0.3530559997133364547 ) ) ;
#21013 = CARTESIAN_POINT ( 'NONE',  ( -0.9711286089238838626, -0.6046776061558807314, 0.2411417322834647770 ) ) ;
#21014 = CARTESIAN_POINT ( 'NONE',  ( 1.266404199475066328, -0.2845877964562161244, -0.3641732283464567121 ) ) ;
#21015 = CARTESIAN_POINT ( 'NONE',  ( -0.8478501267249328732, 2.401574803149606474, -0.8478501267249377582 ) ) ;
#21016 = CARTESIAN_POINT ( 'NONE',  ( -0.4091458600556402980, -0.2362204724409451284, -2.729658792650918375 ) ) ;
#21017 = CARTESIAN_POINT ( 'NONE',  ( 0.7480314960629927956, -0.5511811023622047445, 6.969142054262312111E-17 ) ) ;
#21018 = CARTESIAN_POINT ( 'NONE',  ( 0.4330708661417329575, 0.2952755905511811885, 0.000000000000000000 ) ) ;
#21019 = CARTESIAN_POINT ( 'NONE',  ( 0.3149606299212606708, -0.1870078740157480879, -0.4822834645669291653 ) ) ;
#21020 = CARTESIAN_POINT ( 'NONE',  ( 0.2925321140481932369, 0.2925321140481932369, -1.240157480314960647 ) ) ;
#21021 = CARTESIAN_POINT ( 'NONE',  ( -2.795275590551181466, 2.125984251968505045, 0.000000000000000000 ) ) ;
#21022 = CARTESIAN_POINT ( 'NONE',  ( -0.3996062992125986590, 0.1070741851644051723, -0.7395013123359580609 ) ) ;
#21023 = CARTESIAN_POINT ( 'NONE',  ( 0.3460692066303959202, -0.1998031496062991630, -0.6541994750656167090 ) ) ;
#21024 = CARTESIAN_POINT ( 'NONE',  ( -0.6102362204724400829, 0.1660481256975885056, 0.3530559997133364547 ) ) ;
#21025 = B_SPLINE_CURVE_WITH_KNOTS ( 'NONE', 3,
 ( #77221, #1457, #32596, #77645, #26279, #52356, #51940, #20393, #64178, #19550, #20810, #78063, #27114, #19134, #19977, #45628, #52777, #46465, #57837, #25858, #59102, #46046, #72159, #7775, #44783, #70480, #14514, #65851, #40167, #8184, #14094, #45209 ),
 .UNSPECIFIED., .F., .F.,
 ( 4, 2, 2, 2, 2, 2, 2, 2, 2, 2, 2, 2, 2, 2, 2, 4 ),
 ( 0.03390883336407149451, 0.03455365212229168786, 0.03519847088051188816, 0.03648810839695228181, 0.03777774591339266852, 0.03906738342983306217, 0.04035702094627344888, 0.04164665846271384253, 0.04422593349559461595, 0.04680520852847537550, 0.04938448356135614198, 0.05067412107779653563, 0.05196375859423692234, 0.05325339611067732293, 0.05389821486889750934, 0.05454303362711770270 ),
 .UNSPECIFIED. ) ;
#21026 = CARTESIAN_POINT ( 'NONE',  ( 0.4724409448818898682, 2.892866454678787531E-17, 0.03937007874015747977 ) ) ;
#21027 = CARTESIAN_POINT ( 'NONE',  ( -0.2867679344610364334, -0.2867679344610367109, -2.033464566929133355 ) ) ;
#21028 = CARTESIAN_POINT ( 'NONE',  ( -1.351706036745406347, -0.3690944881889763329, 0.3153832671262228327 ) ) ;
#21029 = CARTESIAN_POINT ( 'NONE',  ( 0.9120734908136489683, -0.6692913385826771977, 0.1292274648535927661 ) ) ;
#21030 = CARTESIAN_POINT ( 'NONE',  ( 1.102362204724410155, -0.1870078740157480879, -0.4822834645669291653 ) ) ;
#21031 = CARTESIAN_POINT ( 'NONE',  ( -0.3477690288713902178, 0.1771653543307087075, -0.09757992244046823083 ) ) ;
#21032 = CARTESIAN_POINT ( 'NONE',  ( 0.2755905511811031494, -0.6692913385826771977, 8.415575281601705876E-17 ) ) ;
#21033 = CARTESIAN_POINT ( 'NONE',  ( 5.785732909357575061E-17, -0.4724409448818898682, -1.887795275590550936 ) ) ;
#21034 = CARTESIAN_POINT ( 'NONE',  ( -0.2821522309711278487, -0.5511811023622048555, -0.09757992244046775898 ) ) ;
#21035 = CARTESIAN_POINT ( 'NONE',  ( 0.05249343832021075018, 0.2306618581243847221, -0.2411417322834647770 ) ) ;
#21036 = ADVANCED_FACE ( 'NONE', ( #30958 ), #28516, .F. ) ;
#21037 = CARTESIAN_POINT ( 'NONE',  ( -0.1058382717557497660, -0.3949938075777411073, -1.566272965879265344 ) ) ;
#21038 = CARTESIAN_POINT ( 'NONE',  ( -1.666666666666665853, 0.05413385826771626580, -0.4176697321401330321 ) ) ;
#21039 = CARTESIAN_POINT ( 'NONE',  ( 0.3543307086614179147, 0.1771653543307087630, 0.000000000000000000 ) ) ;
#21040 = CARTESIAN_POINT ( 'NONE',  ( 1.404199475065617708, -0.004921259842519870586, -0.3153832671262229437 ) ) ;
#21041 = CARTESIAN_POINT ( 'NONE',  ( -0.7545931758530177724, 0.2952755905511811885, 0.1292274648535926551 ) ) ;
#21042 = CARTESIAN_POINT ( 'NONE',  ( -0.6167979002624665030, -0.3690944881889765550, -0.3153832671262227771 ) ) ;
#21043 = CARTESIAN_POINT ( 'NONE',  ( 0.4724409448818898682, 2.892866454678787531E-17, -2.242125984251968518 ) ) ;
#21044 = CARTESIAN_POINT ( 'NONE',  ( -0.6167979002624665030, 0.05413385826771666132, 0.4176697321401328100 ) ) ;
#21045 = CARTESIAN_POINT ( 'NONE',  ( -0.6824146981627288167, 0.2306618581243848609, 0.2411417322834645549 ) ) ;
#21046 = CARTESIAN_POINT ( 'NONE',  ( -0.1181102362204717315, -0.6692913385826771977, 8.415575281601705876E-17 ) ) ;
#21047 = CARTESIAN_POINT ( 'NONE',  ( 4.893765752498283308E-17, -0.3996062992125985480, -2.517716535433071279 ) ) ;
#21048 = B_SPLINE_CURVE_WITH_KNOTS ( 'NONE', 3,
 ( #81734, #82139, #82953, #69498, #50526, #75819, #38325, #55608, #18966, #44615, #63998, #43384, #17351, #37500, #4686, #5922, #81319, #25271, #49303, #24043, #69899, #68674, #31594, #17754, #57250, #75004, #42979, #14348, #45459, #53023 ),
 .UNSPECIFIED., .F., .F.,
 ( 4, 2, 2, 2, 2, 2, 2, 2, 2, 2, 2, 2, 2, 2, 4 ),
 ( 0.005313729678161706153, 0.005969797177609010609, 0.006625864677056315065, 0.007937999675950898823, 0.009250134674845481714, 0.01056226967374006634, 0.01318653967152924947, 0.01581080966931843260, 0.01712294466821301375, 0.01843507966710759144, 0.02105934966489676416, 0.02237148466379134532, 0.02368361966268592647, 0.02499575466158050763, 0.02630788966047508878 ),
 .UNSPECIFIED. ) ;
#21049 = CARTESIAN_POINT ( 'NONE',  ( -0.2867679344610364334, -0.2867679344610368219, -2.028852075294276691 ) ) ;
#21050 = CARTESIAN_POINT ( 'NONE',  ( -1.620734908136482577, -0.5511811023622048555, -0.09757992244046775898 ) ) ;
#21051 = CARTESIAN_POINT ( 'NONE',  ( 0.9645669291338591078, -0.4536011799217368745, -0.2665933059059886201 ) ) ;
#21052 = CARTESIAN_POINT ( 'NONE',  ( 1.430446194225722500, 0.05413385826771666132, 0.4176697321401328100 ) ) ;
#21053 = CARTESIAN_POINT ( 'NONE',  ( -1.187664041994750175, -0.08942795157528024563, -0.3641732283464568787 ) ) ;
#21054 = CARTESIAN_POINT ( 'NONE',  ( -1.272965879265091305, -0.3690944881889763329, 0.3153832671262228327 ) ) ;
#21055 = CARTESIAN_POINT ( 'NONE',  ( -0.5708661417322828946, 0.1660481256975883668, -0.3530559997133364547 ) ) ;
#21056 = CARTESIAN_POINT ( 'NONE',  ( -0.02624671916010428221, 0.1283753931104746893, -0.1820866141732285504 ) ) ;
#21057 = CARTESIAN_POINT ( 'NONE',  ( -0.2814827926786539480, 0.08976297916237283014, 5.855142794233184844 ) ) ;
#21058 = CARTESIAN_POINT ( 'NONE',  ( 1.246719160104987623, -0.3690944881889763329, 0.3153832671262228327 ) ) ;
#21059 = CARTESIAN_POINT ( 'NONE',  ( 0.3543307086614181922, -0.6692913385826771977, 8.415575281601705876E-17 ) ) ;
#21060 = CARTESIAN_POINT ( 'NONE',  ( -0.5577427821522301654, -0.05778040916215560624, -0.4822834645669293319 ) ) ;
#21061 = AXIS2_PLACEMENT_3D ( 'NONE', #40510, #8114, #65367 ) ;
#21062 = CARTESIAN_POINT ( 'NONE',  ( -0.2867679344610364334, -0.2867679344610367109, -1.246062992125984481 ) ) ;
#21063 = CARTESIAN_POINT ( 'NONE',  ( 1.601049868766404982, 0.1283753931104748280, 0.1820866141732283561 ) ) ;
#21065 = CARTESIAN_POINT ( 'NONE',  ( 0.3937007874015754361, -0.1870078740157479769, 0.4822834645669291653 ) ) ;
#21064 = AXIS2_PLACEMENT_3D ( 'NONE', #80299, #3260, #48273 ) ;
#21066 = AXIS2_PLACEMENT_3D ( 'NONE', #51903, #71286, #73266 ) ;
#21067 = CARTESIAN_POINT ( 'NONE',  ( 0.07874015748031558404, -0.1870078740157479769, 0.4822834645669291653 ) ) ;
#21068 = CARTESIAN_POINT ( 'NONE',  ( 0.02624671916010564918, -0.5023911411419708095, -0.1820866141732282451 ) ) ;
#21069 = CARTESIAN_POINT ( 'NONE',  ( 1.220472440944879722, 1.496062992125984037, 0.5309055118110233007 ) ) ;
#21070 = CARTESIAN_POINT ( 'NONE',  ( -0.2165354330708654795, 0.07958543189024085140, 0.2665933059059887866 ) ) ;
#21071 = CARTESIAN_POINT ( 'NONE',  ( 0.6167979002624679463, 0.05413385826771626580, -0.4176697321401330321 ) ) ;
#21072 = CARTESIAN_POINT ( 'NONE',  ( -0.8202099737532801971, -0.5511811023622046335, 0.09757992244046803654 ) ) ;
#21073 = CARTESIAN_POINT ( 'NONE',  ( 4.893765752498283308E-17, -0.3996062992125985480, -0.9429133858267716439 ) ) ;
#21074 = CARTESIAN_POINT ( 'NONE',  ( -1.128608923884513837, 0.2306618581243847221, -0.2411417322834647770 ) ) ;
#21075 = DIRECTION ( 'NONE',  ( -3.736327486719276758E-15, 0.000000000000000000, -1.000000000000000000 ) ) ;
#21076 = ORIENTED_EDGE ( 'NONE', *, *, #76295, .T. ) ;
#21077 = CARTESIAN_POINT ( 'NONE',  ( -1.128608923884513837, 0.2306618581243847221, -0.2411417322834647770 ) ) ;
#21078 = CARTESIAN_POINT ( 'NONE',  ( -1.194225721784776262, -0.004921259842519870586, -0.3153832671262229437 ) ) ;
#21079 = CARTESIAN_POINT ( 'NONE',  ( 0.07217847769028949700, -0.05778040916215560624, -0.4822834645669293319 ) ) ;
#21080 = CARTESIAN_POINT ( 'NONE',  ( -1.673228346456691717, 0.1660481256975883668, -0.3530559997133364547 ) ) ;
#21081 = CARTESIAN_POINT ( 'NONE',  ( -0.9055118110236215490, -0.6692913385826771977, 8.415575281601705876E-17 ) ) ;
#21082 = CARTESIAN_POINT ( 'NONE',  ( 1.403614904275686858E-14, 1.537401574803149984, -3.937007874015761910 ) ) ;
#21083 = CARTESIAN_POINT ( 'NONE',  ( 0.7414698162729663755, -0.6692913385826773087, -0.1292274648535924053 ) ) ;
#21084 = CARTESIAN_POINT ( 'NONE',  ( 0.9580052493438327987, -0.4281496062992127816, -0.4176697321401328100 ) ) ;
#21085 = CARTESIAN_POINT ( 'NONE',  ( -0.3392501089628017219, -0.1958661417322836718, -2.564304461942256808 ) ) ;
#21086 = FACE_OUTER_BOUND ( 'NONE', #63123, .T. ) ;
#21087 = CARTESIAN_POINT ( 'NONE',  ( -1.463254593175852492, -0.6692913385826773087, -0.1292274648535924053 ) ) ;
#21088 = CARTESIAN_POINT ( 'NONE',  ( -0.2925321140481932924, 0.2925321140481931814, -0.6496062992125984925 ) ) ;
#21089 = VERTEX_POINT ( 'NONE', #73516 ) ;
#21090 = CARTESIAN_POINT ( 'NONE',  ( -0.5577427821522301654, -0.2845877964562159024, 0.3641732283464567677 ) ) ;
#21091 = CARTESIAN_POINT ( 'NONE',  ( -0.1958661417322836718, 0.3392501089628017219, -2.367454068241469756 ) ) ;
#21092 = ORIENTED_EDGE ( 'NONE', *, *, #49427, .F. ) ;
#21093 = CARTESIAN_POINT ( 'NONE',  ( 0.3871391076115492380, -0.05778040916215560624, -0.4822834645669293319 ) ) ;
#21094 = CARTESIAN_POINT ( 'NONE',  ( 0.01968503937007930540, 0.1660481256975885056, 0.3530559997133364547 ) ) ;
#21095 = CARTESIAN_POINT ( 'NONE',  ( -0.4790026246719152336, -0.05778040916215560624, -0.4822834645669293319 ) ) ;
#21096 = CARTESIAN_POINT ( 'NONE',  ( 1.358267716535433323, 0.1660481256975885056, 0.3530559997133364547 ) ) ;
#21097 = CARTESIAN_POINT ( 'NONE',  ( -0.9973753280839886548, 0.1283753931104748280, 0.1820866141732283561 ) ) ;
#21098 = CARTESIAN_POINT ( 'NONE',  ( 0.03198557873782978400, 1.064015804215618699, -1.607980685227602402 ) ) ;
#21099 = CARTESIAN_POINT ( 'NONE',  ( 0.5577427821522316087, -0.05778040916215522460, 0.4822834645669289988 ) ) ;
#21100 = CARTESIAN_POINT ( 'NONE',  ( 0.6758530183727039509, 0.1771653543307087075, -0.09757992244046823083 ) ) ;
#21101 = CARTESIAN_POINT ( 'NONE',  ( -0.3543307086614165824, 0.2952755905511811885, 0.000000000000000000 ) ) ;
#21102 = B_SPLINE_CURVE_WITH_KNOTS ( 'NONE', 3,
 ( #78605, #57953, #77762, #33554, #58808, #741, #46166, #45328, #32713, #44898, #71023, #1578 ),
 .UNSPECIFIED., .F., .F.,
 ( 4, 2, 2, 2, 2, 4 ),
 ( 0.05454303362711723779, 0.05585633982237087070, 0.05651299291999767327, 0.05716964601762447584, 0.05848295221287810874, 0.05979625840813173471 ),
 .UNSPECIFIED. ) ;
#21103 = CARTESIAN_POINT ( 'NONE',  ( -9.594673741351310580E-17, 0.3917322834645669549, -1.024915067420260728 ) ) ;
#21104 = CARTESIAN_POINT ( 'NONE',  ( -0.9711286089238838626, 0.2306618581243847221, -0.2411417322834647770 ) ) ;
#21105 = CARTESIAN_POINT ( 'NONE',  ( 0.5314960629921349211, 2.742779986175213569, -2.570293859026649308 ) ) ;
#21106 = CARTESIAN_POINT ( 'NONE',  ( 1.272965879265092637, -0.4281496062992127816, -0.4176697321401328100 ) ) ;
#21107 = CARTESIAN_POINT ( 'NONE',  ( -0.4044922606986716129, 1.289103360985772495, -2.048376007908625507 ) ) ;
#21108 = VERTEX_POINT ( 'NONE', #46979 ) ;
#21109 = CARTESIAN_POINT ( 'NONE',  ( -0.3917322834645670659, -7.196005306013484475E-17, -2.398313279036432100 ) ) ;
#21110 = CARTESIAN_POINT ( 'NONE',  ( -0.04593175853018302557, 0.2952755905511811885, 0.1292274648535926551 ) ) ;
#21111 = ORIENTED_EDGE ( 'NONE', *, *, #60327, .F. ) ;
#21112 = CARTESIAN_POINT ( 'NONE',  ( 0.9383202099737536495, -0.2845877964562159024, 0.3641732283464567677 ) ) ;
#21113 = CARTESIAN_POINT ( 'NONE',  ( -1.128608923884513837, -0.6046776061558807314, 0.2411417322834647770 ) ) ;
#21114 = CARTESIAN_POINT ( 'NONE',  ( 1.128608923884514947, 0.2306618581243848609, 0.2411417322834645549 ) ) ;
#21115 = CARTESIAN_POINT ( 'NONE',  ( 1.371391076115485719, -0.6692913385826773087, -0.1292274648535924053 ) ) ;
#21116 = CARTESIAN_POINT ( 'NONE',  ( 0.2230971128608929543, 0.05413385826771626580, -0.4176697321401330321 ) ) ;
#21117 = CARTESIAN_POINT ( 'NONE',  ( -0.4265091863517051496, -0.6692913385826771977, 0.1292274648535927661 ) ) ;
#21118 = CARTESIAN_POINT ( 'NONE',  ( 0.3917322834645669549, 0.1049643490035304660, -1.626640419947506411 ) ) ;
#21119 = CARTESIAN_POINT ( 'NONE',  ( -1.010498687664041384, -0.4281496062992127816, -0.4176697321401328100 ) ) ;
#21120 = CARTESIAN_POINT ( 'NONE',  ( -0.5839895013123351797, -0.6692913385826771977, 0.1292274648535927661 ) ) ;
#21121 = CARTESIAN_POINT ( 'NONE',  ( -0.6561679790026240244, 0.1283753931104746893, -0.1820866141732285504 ) ) ;
#21122 = DIRECTION ( 'NONE',  ( 0.000000000000000000, -0.5150380749100549327, -0.8571673007021117785 ) ) ;
#21123 = CARTESIAN_POINT ( 'NONE',  ( -0.7086614173228339419, -0.1870078740157480879, -0.4822834645669291653 ) ) ;
#21124 = CARTESIAN_POINT ( 'NONE',  ( 0.2493438320209980519, 0.009842519685039467087, 0.3409548833797002021 ) ) ;
#21125 = VECTOR ( 'NONE', #59576, 39.37007874015748854 ) ;
#21126 = CARTESIAN_POINT ( 'NONE',  ( 0.5577427821522314977, -0.3162353388693409650, -0.4822834645669289433 ) ) ;
#21127 = CARTESIAN_POINT ( 'NONE',  ( 0.1998031496062994405, -0.3460692066303958092, -1.666666666666666741 ) ) ;
#21128 = DIRECTION ( 'NONE',  ( 1.000000000000000000, -0.000000000000000000, -0.000000000000000000 ) ) ;
#21129 = EDGE_CURVE ( 'NONE', #24575, #62837, #73089, .T. ) ;
#21130 = VECTOR ( 'NONE', #64729, 39.37007874015748143 ) ;
#21131 = CARTESIAN_POINT ( 'NONE',  ( -0.1968503937007867743, 0.2952755905511811885, 0.000000000000000000 ) ) ;
#21132 = COLOUR_RGB ( '', 0.08235294, 0.09019608, 0.10196078) ;
#21133 = AXIS2_PLACEMENT_3D ( 'NONE', #82003, #82409, #18026 ) ;
#21135 = CARTESIAN_POINT ( 'NONE',  ( -0.8785612751854012803, -2.613618158232546091E-15, -0.3464511005275220379 ) ) ;
#21134 = CARTESIAN_POINT ( 'NONE',  ( 0.8464566929133866546, -0.4536011799217367080, 0.2665933059059888421 ) ) ;
#21136 = CARTESIAN_POINT ( 'NONE',  ( -1.157146581871515012E-16, 0.4724409448818898682, -0.5492125984251968740 ) ) ;
#21137 = CARTESIAN_POINT ( 'NONE',  ( 1.108923884514436686, -0.2845877964562161244, -0.3641732283464567121 ) ) ;
#21138 = CARTESIAN_POINT ( 'NONE',  ( 1.305774278215223960, 0.2952755905511810774, -0.1292274648535930714 ) ) ;
#21139 = CARTESIAN_POINT ( 'NONE',  ( 0.2891555358219910499, -0.2891555358219909944, -0.1751968503937007815 ) ) ;
#21140 = CARTESIAN_POINT ( 'NONE',  ( -0.3871391076115479057, -0.3162353388693409650, -0.4822834645669289433 ) ) ;
#21141 = DIRECTION ( 'NONE',  ( 1.000000000000000000, -0.000000000000000000, -0.000000000000000000 ) ) ;
#21142 = CARTESIAN_POINT ( 'NONE',  ( -1.627296587926508442, -0.6046776061558809534, -0.2411417322834644161 ) ) ;
#21143 = CARTESIAN_POINT ( 'NONE',  ( 0.006561679790026889343, -0.05778040916215522460, 0.4822834645669289988 ) ) ;
#21144 = CARTESIAN_POINT ( 'NONE',  ( -0.1974969037888704149, -0.3420746716998661063, -0.6148293963254595207 ) ) ;
#21145 = CARTESIAN_POINT ( 'NONE',  ( 1.207349081364829990, 0.2306618581243848609, 0.2411417322834645549 ) ) ;
#21146 = CARTESIAN_POINT ( 'NONE',  ( 0.7283464566929140904, -0.5400638737290845981, -0.3530559997133363437 ) ) ;
#21147 = CARTESIAN_POINT ( 'NONE',  ( 0.8530183727034128527, -0.3690944881889763329, 0.3153832671262228327 ) ) ;
#21148 = CARTESIAN_POINT ( 'NONE',  ( 0.3114547874990893916, 1.319604222443112151, 0.03199850469859417956 ) ) ;
#21149 = CARTESIAN_POINT ( 'NONE',  ( 0.5708661417322842269, 0.07958543189024085140, 0.2665933059059887866 ) ) ;
#21150 = LINE ( 'NONE', #47636, #48429 ) ;
#21151 = CARTESIAN_POINT ( 'NONE',  ( -0.3460692066303960313, 0.1998031496062989965, -1.362860892388451539 ) ) ;
#21152 = CARTESIAN_POINT ( 'NONE',  ( 0.6496062992125991586, -0.5400638737290845981, -0.3530559997133363437 ) ) ;
#21153 = CARTESIAN_POINT ( 'NONE',  ( 0.1958661417322836440, -0.3392501089628017219, -0.7139107611548556331 ) ) ;
#21154 = CARTESIAN_POINT ( 'NONE',  ( 0.3871391076115493490, -0.3162353388693405765, 0.4822834645669290543 ) ) ;
#21155 = CARTESIAN_POINT ( 'NONE',  ( -0.3608923884514428360, 0.2066929133858267931, 0.1054918080437490802 ) ) ;
#21156 = CARTESIAN_POINT ( 'NONE',  ( 0.5118110236220478892, 0.1771653543307087630, 0.000000000000000000 ) ) ;
#21157 = CARTESIAN_POINT ( 'NONE',  ( 0.4461942257217856311, 0.2306618581243847221, -0.2411417322834647770 ) ) ;
#21158 = CARTESIAN_POINT ( 'NONE',  ( -0.5314960629921148261, 2.755905511811024056, -3.184294706754632109 ) ) ;
#21159 = CARTESIAN_POINT ( 'NONE',  ( -0.7349081364829390672, 0.1283753931104746893, -0.1820866141732285504 ) ) ;
#21160 = CARTESIAN_POINT ( 'NONE',  ( -1.010498687664041384, -0.4281496062992127816, -0.4176697321401328100 ) ) ;
#21161 = CARTESIAN_POINT ( 'NONE',  ( -1.489501312335957062, -0.3162353388693409650, -0.4822834645669289433 ) ) ;
#21162 = CARTESIAN_POINT ( 'NONE',  ( 0.5446194225721792126, -0.3162353388693405765, 0.4822834645669290543 ) ) ;
#21163 = CARTESIAN_POINT ( 'NONE',  ( 1.620734908136483465, -0.6692913385826771977, 0.1292274648535927661 ) ) ;
#21164 = DIRECTION ( 'NONE',  ( -0.5653208194167064216, -0.6006868920394703437, 0.5653208194167143041 ) ) ;
#21165 = CARTESIAN_POINT ( 'NONE',  ( 0.4396325459317590445, -0.6692913385826771977, 0.1292274648535927661 ) ) ;
#21166 = CARTESIAN_POINT ( 'NONE',  ( -0.2925321140481930149, -0.2925321140481933480, 0.1791338582677164948 ) ) ;
#21167 = CARTESIAN_POINT ( 'NONE',  ( 0.3765318260368863412, 1.248382286832529831, 3.918973582884354823 ) ) ;
#21168 = CARTESIAN_POINT ( 'NONE',  ( 1.391076115485564868, 0.2306618581243847221, -0.2411417322834647770 ) ) ;
#21169 = CARTESIAN_POINT ( 'NONE',  ( -1.259842519685038686, -0.1870078740157479769, 0.3641732283464567677 ) ) ;
#21170 = B_SPLINE_CURVE_WITH_KNOTS ( 'NONE', 1,
 ( #33062, #58733 ),
 .UNSPECIFIED., .F., .F.,
 ( 2, 2 ),
 ( 0.000000000000000000, 0.002250000000000000264 ),
 .UNSPECIFIED. ) ;
#21171 = CARTESIAN_POINT ( 'NONE',  ( 1.246719160104987623, -0.004921259842519870586, -0.3153832671262229437 ) ) ;
#21172 = CARTESIAN_POINT ( 'NONE',  ( -1.417322834645668772, -0.1870078740157480601, -0.3641732283464567677 ) ) ;
#21173 = CARTESIAN_POINT ( 'NONE',  ( -0.7020997375328074108, -0.08942795157527998196, 0.3641732283464567121 ) ) ;
#21174 = LINE ( 'NONE', #7721, #19796 ) ;
#21175 = CARTESIAN_POINT ( 'NONE',  ( 0.6824146981627303710, 0.1283753931104746893, -0.1820866141732285504 ) ) ;
#21176 = CARTESIAN_POINT ( 'NONE',  ( 0.06561679790026316017, -0.4281496062992124485, 0.4176697321401328655 ) ) ;
#21177 = CARTESIAN_POINT ( 'NONE',  ( 1.069553805774278610, -0.6692913385826771977, 0.1292274648535927661 ) ) ;
#21178 = CARTESIAN_POINT ( 'NONE',  ( -0.1574803149606292529, -0.1870078740157480879, -0.4822834645669291653 ) ) ;
#21179 = CARTESIAN_POINT ( 'NONE',  ( 0.1049868766404206816, -0.5023911411419708095, -0.1820866141732282451 ) ) ;
#21180 = CARTESIAN_POINT ( 'NONE',  ( 1.220472440944882386, -0.6692913385826771977, 8.415575281601705876E-17 ) ) ;
#21181 = CARTESIAN_POINT ( 'NONE',  ( -0.2099737532808391427, 0.1539470093639523085, 0.1968503937007873850 ) ) ;
#21182 = CARTESIAN_POINT ( 'NONE',  ( -0.8792650918635160906, 0.05413385826771626580, -0.4176697321401330321 ) ) ;
#21183 = CARTESIAN_POINT ( 'NONE',  ( -0.3460692066303958092, -0.1998031496062994683, -0.9973753280839895430 ) ) ;
#21184 = CARTESIAN_POINT ( 'NONE',  ( 0.06596743314205978648, 0.004960608223778357855, -0.3437734562760192958 ) ) ;
#21185 = VECTOR ( 'NONE', #42101, 39.37007874015748854 ) ;
#21186 = CARTESIAN_POINT ( 'NONE',  ( -1.010498687664041384, 0.05413385826771666132, 0.4176697321401328100 ) ) ;
#21187 = CARTESIAN_POINT ( 'NONE',  ( 0.01312335958005323398, 0.05413385826771666132, 0.4176697321401328100 ) ) ;
#21188 = CARTESIAN_POINT ( 'NONE',  ( 0.3996062992125986035, 2.446882876249141962E-17, -2.480314960629921295 ) ) ;
#21189 = CARTESIAN_POINT ( 'NONE',  ( 0.3949938075777409408, 0.1058382717557500574, -1.856955380577427928 ) ) ;
#21190 = CARTESIAN_POINT ( 'NONE',  ( -0.1958661417322836718, 0.3392501089628017219, -0.6351706036745405903 ) ) ;
#21191 = LINE ( 'NONE', #41378, #7846 ) ;
#21192 = CARTESIAN_POINT ( 'NONE',  ( -1.240157480314959759, 0.07958543189024085140, 0.2665933059059887866 ) ) ;
#21193 = CARTESIAN_POINT ( 'NONE',  ( -0.1958661417322834220, -0.3392501089628018884, -1.002624671916010568 ) ) ;
#21194 = CARTESIAN_POINT ( 'NONE',  ( -1.574803149606298636, -0.1870078740157479769, 0.4822834645669291653 ) ) ;
#21195 = CARTESIAN_POINT ( 'NONE',  ( -0.1049643490035306742, 0.3917322834645668994, -0.08659485744650738392 ) ) ;
#21196 = CARTESIAN_POINT ( 'NONE',  ( 0.5905511811023629321, 0.2952755905511811885, 0.000000000000000000 ) ) ;
#21197 = CARTESIAN_POINT ( 'NONE',  ( -0.6692913385826764205, -0.5511811023622047445, 6.969142054262312111E-17 ) ) ;
#21198 = CARTESIAN_POINT ( 'NONE',  ( 1.069553805774278610, -0.6692913385826771977, 0.1292274648535927661 ) ) ;
#21199 = CARTESIAN_POINT ( 'NONE',  ( 0.2690288713910767848, -0.6692913385826773087, -0.1292274648535924053 ) ) ;
#21200 = CARTESIAN_POINT ( 'NONE',  ( 0.4582162924217514921, 1.413519198382197306, 1.024232834668445724 ) ) ;
#21201 = CARTESIAN_POINT ( 'NONE',  ( 0.2925321140481932369, 0.2925321140481932369, -2.500000000000000444 ) ) ;
#21202 = CARTESIAN_POINT ( 'NONE',  ( -0.1958661417322833942, -0.3392501089628018884, -1.164717478511497983 ) ) ;
#21203 = CARTESIAN_POINT ( 'NONE',  ( 1.437007874015748810, -0.5400638737290845981, -0.3530559997133363437 ) ) ;
#21204 = CARTESIAN_POINT ( 'NONE',  ( 0.1377952755905518800, -0.5400638737290844871, 0.3530559997133364547 ) ) ;
#21205 = CARTESIAN_POINT ( 'NONE',  ( 1.594488188976378673, 0.1660481256975885056, 0.3530559997133364547 ) ) ;
#21206 = CARTESIAN_POINT ( 'NONE',  ( 1.023622047244095334, -0.1870078740157479769, 0.4822834645669291653 ) ) ;
#21207 = CARTESIAN_POINT ( 'NONE',  ( 0.3917322834645670104, 2.398668435337828261E-17, -0.5177165354330709457 ) ) ;
#21208 = CARTESIAN_POINT ( 'NONE',  ( 0.09842519685039434474, -0.5400638737290845981, -0.3530559997133363437 ) ) ;
#21209 = CARTESIAN_POINT ( 'NONE',  ( 0.8530183727034128527, -0.4281496062992124485, 0.4176697321401328655 ) ) ;
#21210 = CARTESIAN_POINT ( 'NONE',  ( 0.1574803149606306130, -0.1870078740157480879, -0.4822834645669291653 ) ) ;
#21211 = CARTESIAN_POINT ( 'NONE',  ( 0.6233595800524942554, -0.08942795157528024563, -0.3641732283464568787 ) ) ;
#21212 = CARTESIAN_POINT ( 'NONE',  ( -1.266404199475064773, -0.3162353388693405765, 0.4822834645669290543 ) ) ;
#21213 = CARTESIAN_POINT ( 'NONE',  ( -1.594488188976377563, -0.5400638737290844871, 0.3530559997133364547 ) ) ;
#21214 = CARTESIAN_POINT ( 'NONE',  ( 0.8070866141732288002, 0.1660481256975885056, 0.3530559997133364547 ) ) ;
#21215 = CARTESIAN_POINT ( 'NONE',  ( -0.2065800152999316408, -0.3330030935792791524, -1.929133858267716217 ) ) ;
#21216 = CARTESIAN_POINT ( 'NONE',  ( -0.3392501089628017219, -0.1958661417322836718, -1.934383202099737575 ) ) ;
#21217 = VERTEX_POINT ( 'NONE', #15022 ) ;
#21218 = CARTESIAN_POINT ( 'NONE',  ( -0.1998031496062994683, 0.3460692066303958092, -0.4855643044619422644 ) ) ;
#21219 = ORIENTED_EDGE ( 'NONE', *, *, #59455, .T. ) ;
#21220 = CARTESIAN_POINT ( 'NONE',  ( 1.154855643044620184, -0.6046776061558807314, 0.2411417322834647770 ) ) ;
#21221 = CARTESIAN_POINT ( 'NONE',  ( 1.076115485564305141, -0.5023911411419708095, 0.1820866141732285504 ) ) ;
#21222 = CARTESIAN_POINT ( 'NONE',  ( 2.503252890251015828, 2.755905511811024056, 0.5314960629921260393 ) ) ;
#21223 = CARTESIAN_POINT ( 'NONE',  ( 0.4724409448818898682, 2.892866454678787531E-17, -0.03740157480314962313 ) ) ;
#21224 = CARTESIAN_POINT ( 'NONE',  ( 0.3973686378485507542, 0.03056273350766219865, -1.929133858267715773 ) ) ;
#21225 = CARTESIAN_POINT ( 'NONE',  ( -0.3917322834645671215, 0.1049643490035301469, -1.062335958005249603 ) ) ;
#21226 = CARTESIAN_POINT ( 'NONE',  ( 1.240157480314961314, -0.5400638737290844871, 0.3530559997133364547 ) ) ;
#21227 = CARTESIAN_POINT ( 'NONE',  ( -0.3974711515624869129, -0.004548682155782115578, -1.929133858267716439 ) ) ;
#21228 = CARTESIAN_POINT ( 'NONE',  ( -0.1837270341207343505, -0.6046776061558807314, 0.2411417322834647770 ) ) ;
#21229 = CARTESIAN_POINT ( 'NONE',  ( 1.279527559055118724, 0.1660481256975885056, 0.3530559997133364547 ) ) ;
#21230 = ORIENTED_EDGE ( 'NONE', *, *, #6995, .F. ) ;
#21231 = CARTESIAN_POINT ( 'NONE',  ( -1.712598425196849572, 0.1660481256975885056, 0.3530559997133364547 ) ) ;
#21232 = CARTESIAN_POINT ( 'NONE',  ( -1.096643835343520168, 1.126359415431272382, -0.2388483330940451010 ) ) ;
#21233 = DIRECTION ( 'NONE',  ( 0.8894554832758219121, 0.000000000000000000, 0.4570218192499936327 ) ) ;
#21234 = CARTESIAN_POINT ( 'NONE',  ( 1.568241469816273659, -0.08942795157528024563, -0.3641732283464568787 ) ) ;
#21235 = CARTESIAN_POINT ( 'NONE',  ( 1.948818897637795367, 0.000000000000000000, 5.544487991299990703 ) ) ;
#21236 = CARTESIAN_POINT ( 'NONE',  ( -0.9711286089238838626, 0.1283753931104746893, -0.1820866141732285504 ) ) ;
#21237 = CARTESIAN_POINT ( 'NONE',  ( -1.430446194225720724, 0.05413385826771626580, -0.4176697321401330321 ) ) ;
#21238 = CARTESIAN_POINT ( 'NONE',  ( 0.7217847769028878924, 0.05413385826771666132, 0.4176697321401328100 ) ) ;
#21239 = AXIS2_PLACEMENT_3D ( 'NONE', #50125, #82144, #32431 ) ;
#21240 = VERTEX_POINT ( 'NONE', #67198 ) ;
#21242 = CARTESIAN_POINT ( 'NONE',  ( -0.4265091863517051496, 0.2066929133858267098, -0.1054918080437494132 ) ) ;
#21241 = CARTESIAN_POINT ( 'NONE',  ( 1.443569553805774897, -0.6046776061558809534, -0.2411417322834644161 ) ) ;
#21243 = CARTESIAN_POINT ( 'NONE',  ( -0.6036745406824141069, 0.1283753931104748280, 0.1820866141732283561 ) ) ;
#21244 = CARTESIAN_POINT ( 'NONE',  ( 0.9251968503937015864, 0.1660481256975883668, -0.3530559997133364547 ) ) ;
#21245 = CARTESIAN_POINT ( 'NONE',  ( -1.646981627296586703, -0.3162353388693409650, -0.4822834645669289433 ) ) ;
#21246 = CARTESIAN_POINT ( 'NONE',  ( 0.1049643490035303689, 0.3917322834645668994, -1.175833702590864283 ) ) ;
#21247 = CARTESIAN_POINT ( 'NONE',  ( -0.6233595800524928121, -0.08942795157527998196, 0.3641732283464567121 ) ) ;
#21248 = CARTESIAN_POINT ( 'NONE',  ( 1.607611548556431069, -0.6692913385826773087, -0.1292274648535924053 ) ) ;
#21249 = CARTESIAN_POINT ( 'NONE',  ( -0.3392501089628019995, 0.1958661417322832277, -1.055774278215223294 ) ) ;
#21250 = CARTESIAN_POINT ( 'NONE',  ( 0.5708661417322841158, -0.5400638737290845981, -0.3530559997133363437 ) ) ;
#21251 = CARTESIAN_POINT ( 'NONE',  ( -0.9645669291338575535, 0.07958543189024071263, -0.2665933059059888421 ) ) ;
#21252 = CARTESIAN_POINT ( 'NONE',  ( -0.1509186351706028884, -0.08942795157527998196, 0.3641732283464567121 ) ) ;
#21253 = EDGE_CURVE ( 'NONE', #6920, #24806, #12039, .T. ) ;
#21254 = CARTESIAN_POINT ( 'NONE',  ( -0.3674540682414692561, -0.6046776061558809534, -0.2411417322834644161 ) ) ;
#21255 = CARTESIAN_POINT ( 'NONE',  ( -1.469816272965878357, 0.1283753931104748280, 0.1820866141732283561 ) ) ;
#21256 = CARTESIAN_POINT ( 'NONE',  ( 4.797336870675656522E-17, -0.3917322834645670659, -0.2329589483277709483 ) ) ;
#21257 = CARTESIAN_POINT ( 'NONE',  ( 0.6889763779527563470, 0.1660481256975883668, -0.3530559997133364547 ) ) ;
#21258 = EDGE_CURVE ( 'NONE', #10037, #73823, #26237, .T. ) ;
#21259 = CARTESIAN_POINT ( 'NONE',  ( 0.8776378784356307916, 4.512065407040659715E-16, 0.3791483426435169335 ) ) ;
#21260 = CARTESIAN_POINT ( 'NONE',  ( 0.3458507752293908943, -0.3458507752293908943, -1.592519685039370358 ) ) ;
#21261 = CARTESIAN_POINT ( 'NONE',  ( -0.8661417322834640276, -0.1870078740157480879, -0.4822834645669291653 ) ) ;
#21262 = CARTESIAN_POINT ( 'NONE',  ( -0.1902887139107604098, -0.5511811023622046335, 0.09757992244046803654 ) ) ;
#21263 = CARTESIAN_POINT ( 'NONE',  ( -1.482939632545930975, 0.05413385826771666132, 0.4176697321401328100 ) ) ;
#21264 = CARTESIAN_POINT ( 'NONE',  ( 0.4133858267716541968, 0.07958543189024085140, 0.2665933059059887866 ) ) ;
#21265 = CARTESIAN_POINT ( 'NONE',  ( -0.8136482939632537770, -0.5023911411419708095, 0.1820866141732285504 ) ) ;
#21266 = CARTESIAN_POINT ( 'NONE',  ( -1.233595800524933894, 0.2306618581243848609, 0.2411417322834645549 ) ) ;
#21267 = CARTESIAN_POINT ( 'NONE',  ( -1.410761154855642463, -0.05778040916215522460, 0.4822834645669289988 ) ) ;
#21268 = CARTESIAN_POINT ( 'NONE',  ( -1.437007874015747477, 0.1660481256975883668, -0.3530559997133364547 ) ) ;
#21269 = CARTESIAN_POINT ( 'NONE',  ( 1.036745406824147508, 0.009842519685039467087, 0.3409548833797002021 ) ) ;
#21270 = CARTESIAN_POINT ( 'NONE',  ( 0.7086614173228353852, -0.1870078740157479769, 0.3641732283464567677 ) ) ;
#21271 = CARTESIAN_POINT ( 'NONE',  ( 0.4855643044619430415, -0.4281496062992127816, -0.4176697321401328100 ) ) ;
#21272 = CARTESIAN_POINT ( 'NONE',  ( -1.312335958005248715, 0.2306618581243848609, 0.2411417322834645549 ) ) ;
#21273 = CARTESIAN_POINT ( 'NONE',  ( 1.587926509186352142, -0.004921259842519576551, 0.3153832671262227771 ) ) ;
#21274 = ORIENTED_EDGE ( 'NONE', *, *, #83070, .T. ) ;
#21275 = CARTESIAN_POINT ( 'NONE',  ( -0.3460692066303957537, -0.1998031496062994405, -2.806430446194225770 ) ) ;
#21276 = EDGE_CURVE ( 'NONE', #64597, #43450, #61225, .T. ) ;
#21277 = CARTESIAN_POINT ( 'NONE',  ( -1.299212598425196097, 0.1771653543307087630, 0.000000000000000000 ) ) ;
#21278 = CARTESIAN_POINT ( 'NONE',  ( -0.3477690288713902178, 0.2952755905511810774, -0.1292274648535930714 ) ) ;
#21279 = CARTESIAN_POINT ( 'NONE',  ( 0.1246719160104994284, -0.6692913385826771977, 0.1292274648535927661 ) ) ;
#21280 = CARTESIAN_POINT ( 'NONE',  ( -1.338582677165353729, -0.1870078740157480601, -0.3641732283464567677 ) ) ;
#21281 = CARTESIAN_POINT ( 'NONE',  ( -0.1070741851644056997, 0.3996062992125984925, -1.658136482939632339 ) ) ;
#21282 = CARTESIAN_POINT ( 'NONE',  ( -1.312335958005248715, -0.6046776061558809534, -0.2411417322834644161 ) ) ;
#21283 = CARTESIAN_POINT ( 'NONE',  ( 0.5118110236220480003, -0.6692913385826771977, 8.415575281601705876E-17 ) ) ;
#21284 = CARTESIAN_POINT ( 'NONE',  ( 0.1574803149606306130, -0.1870078740157480879, -0.4822834645669291653 ) ) ;
#21285 = EDGE_CURVE ( 'NONE', #7122, #32917, #22155, .T. ) ;
#21286 = CARTESIAN_POINT ( 'NONE',  ( 1.135170603674541256, 0.2952755905511811885, 0.1292274648535926551 ) ) ;
#21287 = CARTESIAN_POINT ( 'NONE',  ( -9.787531504996566615E-17, 0.3996062992125985480, -1.179133858267716661 ) ) ;
#21288 = CARTESIAN_POINT ( 'NONE',  ( 0.3996062992125986590, -0.1070741851644053111, -1.371391076115485053 ) ) ;
#21289 = CARTESIAN_POINT ( 'NONE',  ( -0.1974969037888706647, 0.3420746716998658843, -0.4855643044619423754 ) ) ;
#21290 =( REPRESENTATION_RELATIONSHIP ('NONE','NONE', #79348, #82043 ) REPRESENTATION_RELATIONSHIP_WITH_TRANSFORMATION ( #69979 )SHAPE_REPRESENTATION_RELATIONSHIP( ) );
#21291 = CARTESIAN_POINT ( 'NONE',  ( 0.3917322834645670104, 2.398668435337828261E-17, -0.2677165354330708347 ) ) ;
#21292 = CARTESIAN_POINT ( 'NONE',  ( 0.2099737532808405305, 0.1283753931104746893, -0.1820866141732285504 ) ) ;
#21293 = CARTESIAN_POINT ( 'NONE',  ( -0.4265091863517051496, 0.2952755905511810774, -0.1292274648535930714 ) ) ;
#21294 = CARTESIAN_POINT ( 'NONE',  ( 1.181102362204724976, -0.1870078740157480879, -0.4822834645669291653 ) ) ;
#21295 = CARTESIAN_POINT ( 'NONE',  ( -0.2891555358219911054, 0.2891555358219909388, -1.828740157480315487 ) ) ;
#21296 = CARTESIAN_POINT ( 'NONE',  ( 0.1377952755905518800, 0.07958543189024071263, -0.2665933059059888421 ) ) ;
#21297 = CARTESIAN_POINT ( 'NONE',  ( -0.9645669291338575535, 0.1660481256975883668, -0.3530559997133364547 ) ) ;
#21298 = CARTESIAN_POINT ( 'NONE',  ( -1.482939632545930975, 0.05413385826771666132, 0.4176697321401328100 ) ) ;
#21299 = CARTESIAN_POINT ( 'NONE',  ( -1.157146581871515012E-16, 0.4724409448818898682, -2.047244094488188892 ) ) ;
#21300 = CARTESIAN_POINT ( 'NONE',  ( 0.3738583250858177887, 0.1188761721681784872, -2.755905511811022279 ) ) ;
#21301 = VERTEX_POINT ( 'NONE', #75988 ) ;
#21302 = ORIENTED_EDGE ( 'NONE', *, *, #12502, .F. ) ;
#21303 = CARTESIAN_POINT ( 'NONE',  ( 1.476377952755906220, 0.1660481256975883668, -0.3530559997133364547 ) ) ;
#21304 = CARTESIAN_POINT ( 'NONE',  ( -1.535433070866141225, 0.2952755905511811885, 0.000000000000000000 ) ) ;
#21306 = CARTESIAN_POINT ( 'NONE',  ( -1.351706036745406347, -0.4281496062992124485, 0.4176697321401328655 ) ) ;
#21305 = CARTESIAN_POINT ( 'NONE',  ( -1.279527559055116948, 0.07958543189024071263, -0.2665933059059888421 ) ) ;
#21307 = CARTESIAN_POINT ( 'NONE',  ( 0.3917322834645668994, 0.1049643490035304522, -2.251949188155168979 ) ) ;
#21308 = FACE_OUTER_BOUND ( 'NONE', #64249, .T. ) ;
#21309 = CARTESIAN_POINT ( 'NONE',  ( 1.161417322834646493, -0.5400638737290844871, 0.3530559997133364547 ) ) ;
#21310 = CARTESIAN_POINT ( 'NONE',  ( -1.076115485564303809, 0.2306618581243848609, 0.2411417322834645549 ) ) ;
#21311 = CARTESIAN_POINT ( 'NONE',  ( -0.1902887139107604098, -0.6692913385826771977, 0.1292274648535927661 ) ) ;
#21312 = CARTESIAN_POINT ( 'NONE',  ( -0.1443569553805768291, 0.05413385826771666132, 0.4176697321401328100 ) ) ;
#21313 = CARTESIAN_POINT ( 'NONE',  ( -1.384514435695537005, -0.6692913385826773087, -0.1292274648535924053 ) ) ;
#21314 = CARTESIAN_POINT ( 'NONE',  ( -0.1049643490035301746, -0.3917322834645670659, -2.671896694716848764 ) ) ;
#21315 = CARTESIAN_POINT ( 'NONE',  ( 0.7480314960629927956, -0.6692913385826771977, 8.415575281601705876E-17 ) ) ;
#21316 = CARTESIAN_POINT ( 'NONE',  ( 0.1049643490035303689, 0.3917322834645670104, -1.875328083989501460 ) ) ;
#21317 = CARTESIAN_POINT ( 'NONE',  ( -1.272965879265091305, -0.004921259842519870586, -0.3153832671262229437 ) ) ;
#21318 = EDGE_LOOP ( 'NONE', ( #35521, #69428, #68534, #45200 ) ) ;
#21319 = CARTESIAN_POINT ( 'NONE',  ( 0.2891555358219910499, 0.2891555358219910499, -2.185039370078740273 ) ) ;
#21320 = ORIENTED_EDGE ( 'NONE', *, *, #68913, .F. ) ;
#21321 = CARTESIAN_POINT ( 'NONE',  ( -1.438119991934921238, 1.333025515147837403, 0.4284971980842492423 ) ) ;
#21322 = CARTESIAN_POINT ( 'NONE',  ( -1.082677165354329896, 0.1660481256975885056, 0.3530559997133364547 ) ) ;
#21323 = CARTESIAN_POINT ( 'NONE',  ( -1.450131233595799651, 0.2952755905511810774, -0.1292274648535930714 ) ) ;
#21324 = CARTESIAN_POINT ( 'NONE',  ( 0.1070741851644053527, 0.3996062992125986590, -0.7808398950131233418 ) ) ;
#21325 = CARTESIAN_POINT ( 'NONE',  ( -1.437007874015747477, -0.5400638737290844871, 0.3530559997133364547 ) ) ;
#21326 = CARTESIAN_POINT ( 'NONE',  ( -1.646981627296586703, -0.3162353388693409650, -0.4822834645669289433 ) ) ;
#21327 = EDGE_CURVE ( 'NONE', #76797, #60402, #42325, .T. ) ;
#21328 = CARTESIAN_POINT ( 'NONE',  ( -1.364829396325458521, -0.6046776061558807314, 0.2411417322834647770 ) ) ;
#21329 = DIRECTION ( 'NONE',  ( 0.000000000000000000, 1.224646799147351482E-16, 1.000000000000000000 ) ) ;
#21330 = CARTESIAN_POINT ( 'NONE',  ( -0.3392501089628017219, -0.1958661417322836718, 0.1778215223097112108 ) ) ;
#21331 = CARTESIAN_POINT ( 'NONE',  ( 0.1115485564304470323, 0.1771653543307087630, 0.09757992244046791164 ) ) ;
#21332 = CARTESIAN_POINT ( 'NONE',  ( 0.3917322834645670104, -0.1049643490035303411, -0.8261154855643043637 ) ) ;
#21333 = CARTESIAN_POINT ( 'NONE',  ( -0.9908136482939626788, -0.5511811023622048555, -0.09757992244046775898 ) ) ;
#21334 = CARTESIAN_POINT ( 'NONE',  ( -1.305774278215222184, 0.2952755905511811885, 0.1292274648535926551 ) ) ;
#21335 = CARTESIAN_POINT ( 'NONE',  ( 0.9055118110236227702, -0.6692913385826771977, 8.415575281601705876E-17 ) ) ;
#21336 = CARTESIAN_POINT ( 'NONE',  ( -1.010498687664041384, 0.05413385826771666132, 0.4176697321401328100 ) ) ;
#21337 = CARTESIAN_POINT ( 'NONE',  ( -9.594673741351313045E-17, 0.3917322834645670104, 0.007874015748031541057 ) ) ;
#21338 = VERTEX_POINT ( 'NONE', #30534 ) ;
#21339 = CARTESIAN_POINT ( 'NONE',  ( -1.213910761154854745, -0.6692913385826771977, 0.1292274648535927661 ) ) ;
#21340 = CARTESIAN_POINT ( 'NONE',  ( 1.010498687664042716, 0.05413385826771626580, -0.4176697321401330321 ) ) ;
#21341 = CARTESIAN_POINT ( 'NONE',  ( -1.633858267716534529, -0.4536011799217368745, -0.2665933059059886201 ) ) ;
#21342 = CARTESIAN_POINT ( 'NONE',  ( 0.4091458600556403535, 0.2362204724409449896, -1.391076115485564424 ) ) ;
#21343 = EDGE_CURVE ( 'NONE', #2483, #11553, #81486, .T. ) ;
#21344 = CARTESIAN_POINT ( 'NONE',  ( 1.850582881112983635, 1.063196196511240199, -0.01636564761925528647 ) ) ;
#21345 = CARTESIAN_POINT ( 'NONE',  ( 0.2867679344610365999, -0.2867679344610365444, -0.4055118110236220486 ) ) ;
#21346 = CARTESIAN_POINT ( 'NONE',  ( 0.1049643490035303689, 0.3917322834645670104, -2.597769028871390606 ) ) ;
#21347 = CARTESIAN_POINT ( 'NONE',  ( -0.3477690288713902178, 0.2952755905511810774, -0.1292274648535930714 ) ) ;
#21348 = CARTESIAN_POINT ( 'NONE',  ( -1.581364829396324945, -0.08942795157528024563, -0.3641732283464568787 ) ) ;
#21349 = CARTESIAN_POINT ( 'NONE',  ( -0.2925321140481930149, -0.2925321140481933480, -0.1358267716535433156 ) ) ;
#21351 = CARTESIAN_POINT ( 'NONE',  ( -0.4734416007054501607, 1.572145545125846144, 2.556694656352222594 ) ) ;
#21350 = CARTESIAN_POINT ( 'NONE',  ( -1.666666666666665853, 0.05413385826771626580, -0.4176697321401330321 ) ) ;
#21352 = CARTESIAN_POINT ( 'NONE',  ( -1.463254593175852492, -0.6692913385826773087, -0.1292274648535924053 ) ) ;
#21353 = CARTESIAN_POINT ( 'NONE',  ( -0.3674540682414692561, -0.6046776061558809534, -0.2411417322834644161 ) ) ;
#21354 = CARTESIAN_POINT ( 'NONE',  ( -0.3392501089628019439, 0.1958661417322832554, 0.2086807331046737768 ) ) ;
#21355 = CARTESIAN_POINT ( 'NONE',  ( 0.5446194225721792126, -0.08942795157528024563, -0.3641732283464568787 ) ) ;
#21356 = CARTESIAN_POINT ( 'NONE',  ( -0.2867679344610364334, -0.2867679344610367109, -0.1437007874015748810 ) ) ;
#21357 = CARTESIAN_POINT ( 'NONE',  ( 0.2427821522309719648, -0.08942795157527998196, 0.3641732283464567121 ) ) ;
#21358 = CARTESIAN_POINT ( 'NONE',  ( 0.9580052493438326877, -0.004921259842519576551, 0.3153832671262227771 ) ) ;
#21359 = CARTESIAN_POINT ( 'NONE',  ( 1.003937007874016185, 0.1660481256975883668, -0.3530559997133364547 ) ) ;
#21360 = CARTESIAN_POINT ( 'NONE',  ( 0.1837270341207357105, -0.5023911411419708095, -0.1820866141732282451 ) ) ;
#21361 = CARTESIAN_POINT ( 'NONE',  ( 0.3917322834645670104, -0.1049643490035303411, -1.993438320209974135 ) ) ;
#21362 = CARTESIAN_POINT ( 'NONE',  ( -1.246719160104985846, -0.4281496062992127816, -0.4176697321401328100 ) ) ;
#21363 = CARTESIAN_POINT ( 'NONE',  ( -0.2165354330708654795, -0.4536011799217368745, -0.2665933059059886201 ) ) ;
#21364 = CARTESIAN_POINT ( 'NONE',  ( -1.325459317585300889, -0.004921259842519576551, 0.3153832671262227771 ) ) ;
#21365 = CARTESIAN_POINT ( 'NONE',  ( -0.4724409448818895907, -0.1265901696524993070, -0.2801837270341207553 ) ) ;
#21366 = CARTESIAN_POINT ( 'NONE',  ( -1.082677165354329896, -0.4536011799217368745, -0.2665933059059886201 ) ) ;
#21367 = CARTESIAN_POINT ( 'NONE',  ( 0.4255982601316013469, 1.327156923586373161, -1.428513422047406944 ) ) ;
#21368 = CARTESIAN_POINT ( 'NONE',  ( -0.1115485564304453947, -0.6692913385826771977, 0.1292274648535927661 ) ) ;
#21369 = DIRECTION ( 'NONE',  ( -1.000000000000000000, 0.000000000000000000, 0.000000000000000000 ) ) ;
#21370 = CARTESIAN_POINT ( 'NONE',  ( 0.7349081364829402885, -0.5023911411419708095, -0.1820866141732282451 ) ) ;
#21371 = CARTESIAN_POINT ( 'NONE',  ( -0.1574803149606292529, -0.1870078740157479769, 0.3641732283464567677 ) ) ;
#21372 = CARTESIAN_POINT ( 'NONE',  ( -0.4855643044619415427, 0.05413385826771626580, -0.4176697321401330321 ) ) ;
#21373 = CARTESIAN_POINT ( 'NONE',  ( 2.795275590551181466, 1.968503937007874738, 0.000000000000000000 ) ) ;
#21374 = CARTESIAN_POINT ( 'NONE',  ( -1.089238845144356427, -0.3690944881889765550, -0.3153832671262227771 ) ) ;
#21375 = CARTESIAN_POINT ( 'NONE',  ( 0.2755905511811031494, 3.495546966070205708E-17, 6.062992125984251857 ) ) ;
#21376 = CARTESIAN_POINT ( 'NONE',  ( 0.5446194225721792126, -0.3162353388693405765, 0.4822834645669290543 ) ) ;
#21377 = ORIENTED_EDGE ( 'NONE', *, *, #1933, .F. ) ;
#21378 = CARTESIAN_POINT ( 'NONE',  ( 0.3996062992125985480, 2.446882876249141654E-17, -1.454724409448818756 ) ) ;
#21379 = DIRECTION ( 'NONE',  ( 0.000000000000000000, 0.000000000000000000, -1.000000000000000000 ) ) ;
#21380 = CARTESIAN_POINT ( 'NONE',  ( -0.3477690288713905509, -0.5511811023622046335, 0.09757992244046803654 ) ) ;
#21381 = CARTESIAN_POINT ( 'NONE',  ( -1.509186351706035767, -0.4281496062992124485, 0.4176697321401328655 ) ) ;
#21382 = CARTESIAN_POINT ( 'NONE',  ( 1.574803149606299746, -0.1870078740157480879, -0.4822834645669291653 ) ) ;
#21383 = CARTESIAN_POINT ( 'NONE',  ( -3.913197263145800520, 1.341570523813770954, -0.4323813531989676995 ) ) ;
#21384 = CARTESIAN_POINT ( 'NONE',  ( -0.6889763779527552368, -0.4536011799217368745, -0.2665933059059886201 ) ) ;
#21385 = CARTESIAN_POINT ( 'NONE',  ( 0.1216921365961834839, -0.3911666210184605585, -0.005627570198504562755 ) ) ;
#21386 = CARTESIAN_POINT ( 'NONE',  ( 1.069553805774278610, -0.6692913385826771977, 0.1292274648535927661 ) ) ;
#21387 = CARTESIAN_POINT ( 'NONE',  ( -0.2925321140481930704, -0.2925321140481933480, -0.05905511811023621965 ) ) ;
#21388 = CARTESIAN_POINT ( 'NONE',  ( -0.3917322834645671770, 0.1049643490035302024, -2.706712229167666184 ) ) ;
#21389 = CARTESIAN_POINT ( 'NONE',  ( -3.856579543051780856, 2.748002881374839390, -0.5314960629921259283 ) ) ;
#21390 = CARTESIAN_POINT ( 'NONE',  ( -1.725721784776902190, -0.05778040916215522460, 0.4822834645669289988 ) ) ;
#21391 = CARTESIAN_POINT ( 'NONE',  ( -1.279527559055116948, -0.5400638737290844871, 0.3530559997133364547 ) ) ;
#21392 = CARTESIAN_POINT ( 'NONE',  ( 1.338582677165355062, -0.1870078740157480879, -0.4822834645669291653 ) ) ;
#21393 = CARTESIAN_POINT ( 'NONE',  ( 0.3917322834645670104, -0.1049643490035303411, -2.400918635170603554 ) ) ;
#21394 = CARTESIAN_POINT ( 'NONE',  ( 1.108923884514436686, -0.2845877964562161244, -0.3641732283464567121 ) ) ;
#21395 =( BOUNDED_CURVE ( )  B_SPLINE_CURVE ( 1, ( #38176, #36943 ),
 .UNSPECIFIED., .F., .F. ) 
 B_SPLINE_CURVE_WITH_KNOTS ( ( 2, 2 ),
 ( 6.938893903907228378E-18, 0.002000000000000008715 ),
 .UNSPECIFIED. ) 
 CURVE ( )  GEOMETRIC_REPRESENTATION_ITEM ( )  RATIONAL_B_SPLINE_CURVE ( ( 0.9875488213027530104, 0.9875488213027530104 ) ) 
 REPRESENTATION_ITEM ( '' )  );
#21396 = CARTESIAN_POINT ( 'NONE',  ( 0.03280839895013198948, -0.6692913385826773087, -0.1292274648535924053 ) ) ;
#21397 = CARTESIAN_POINT ( 'NONE',  ( -0.4133858267716528645, -0.5400638737290844871, 0.3530559997133364547 ) ) ;
#21398 = CARTESIAN_POINT ( 'NONE',  ( -2.516666458577628163, 2.742784436987529606, -0.5314960629921260393 ) ) ;
#21399 = CARTESIAN_POINT ( 'NONE',  ( 3.900966923095589678, 2.677165354330708791, 0.5314960629921260393 ) ) ;
#21400 = CARTESIAN_POINT ( 'NONE',  ( 0.2952755905511816326, -0.4536011799217367080, 0.2665933059059888421 ) ) ;
#21401 = EDGE_CURVE ( 'NONE', #13953, #66690, #51586, .T. ) ;
#21402 = ORIENTED_EDGE ( 'NONE', *, *, #81194, .F. ) ;
#21403 = CARTESIAN_POINT ( 'NONE',  ( 0.1049643490035304799, -0.3917322834645670104, -0.3970009430784271487 ) ) ;
#21404 = VERTEX_POINT ( 'NONE', #68842 ) ;
#21405 = CARTESIAN_POINT ( 'NONE',  ( -0.3674540682414692561, -0.6046776061558809534, -0.2411417322834644161 ) ) ;
#21406 = CARTESIAN_POINT ( 'NONE',  ( 1.246719160104987623, -0.4281496062992124485, 0.4176697321401328655 ) ) ;
#21407 = CARTESIAN_POINT ( 'NONE',  ( 0.3674540682414705883, -0.6046776061558807314, 0.2411417322834647770 ) ) ;
#21408 = CARTESIAN_POINT ( 'NONE',  ( -0.5314960629921250401, 0.07958543189024085140, 0.2665933059059887866 ) ) ;
#21409 = CARTESIAN_POINT ( 'NONE',  ( 1.076115485564305141, 0.2306618581243847221, -0.2411417322834647770 ) ) ;
#21410 = EDGE_CURVE ( 'NONE', #32372, #70661, #38374, .T. ) ;
#21411 = CARTESIAN_POINT ( 'NONE',  ( -0.9711286089238838626, 0.2306618581243847221, -0.2411417322834647770 ) ) ;
#21412 = CARTESIAN_POINT ( 'NONE',  ( -0.07874015748031421014, -0.1870078740157480879, -0.4822834645669291653 ) ) ;
#21413 = CARTESIAN_POINT ( 'NONE',  ( -0.7414698162729651543, 0.2952755905511810774, -0.1292274648535930714 ) ) ;
#21414 = CARTESIAN_POINT ( 'NONE',  ( 1.259842519685040019, -0.1870078740157479769, 0.4822834645669291653 ) ) ;
#21415 = CARTESIAN_POINT ( 'NONE',  ( 1.082677165354331228, -0.5400638737290844871, 0.3530559997133364547 ) ) ;
#21416 = CARTESIAN_POINT ( 'NONE',  ( 1.207349081364829990, 0.2306618581243848609, 0.2411417322834645549 ) ) ;
#21417 = CARTESIAN_POINT ( 'NONE',  ( 0.1958661417322836440, -0.3392501089628017219, -0.5564304461942257696 ) ) ;
#21418 = CARTESIAN_POINT ( 'NONE',  ( -0.1049868766404193215, -0.5023911411419708095, 0.1820866141732285504 ) ) ;
#21419 = VERTEX_POINT ( 'NONE', #35613 ) ;
#21420 = CARTESIAN_POINT ( 'NONE',  ( 0.3949938075777409963, 2.418639510665530435E-17, -1.220472440944881942 ) ) ;
#21421 = EDGE_LOOP ( 'NONE', ( #17465, #803, #22546, #76661 ) ) ;
#21422 = CARTESIAN_POINT ( 'NONE',  ( -0.8858267716535425107, 0.07958543189024071263, -0.2665933059059888421 ) ) ;
#21423 = CARTESIAN_POINT ( 'NONE',  ( -0.1377952755905504645, -0.5400638737290845981, -0.3530559997133363437 ) ) ;
#21424 = CARTESIAN_POINT ( 'NONE',  ( 2.800975763475996860, 1.142877263639039853, 0.2639061591570066589 ) ) ;
#21425 = CARTESIAN_POINT ( 'NONE',  ( -0.3477690288713905509, -0.6692913385826771977, 0.1292274648535927661 ) ) ;
#21426 = CARTESIAN_POINT ( 'NONE',  ( -0.3608923884514428360, -0.6692913385826773087, -0.1292274648535924053 ) ) ;
#21427 = CARTESIAN_POINT ( 'NONE',  ( -0.7874015748031489847, -0.1870078740157480879, -0.4822834645669291653 ) ) ;
#21428 = CARTESIAN_POINT ( 'NONE',  ( -1.594488188976377563, -0.5400638737290844871, 0.3530559997133364547 ) ) ;
#21429 = CARTESIAN_POINT ( 'NONE',  ( 1.240157480314961314, 0.07958543189024071263, -0.2665933059059888421 ) ) ;
#21430 = CARTESIAN_POINT ( 'NONE',  ( -1.594488188976377119, 0.1660481256975883668, -0.3530559997133364547 ) ) ;
#21431 = CARTESIAN_POINT ( 'NONE',  ( -0.4091458600556402980, -0.2362204724409451284, -0.6017060367454067915 ) ) ;
#21432 = CARTESIAN_POINT ( 'NONE',  ( 0.5643044619422579178, -0.3690944881889765550, -0.3153832671262227771 ) ) ;
#21433 = CARTESIAN_POINT ( 'NONE',  ( 0.1443569553805781891, 0.05413385826771626580, -0.4176697321401330321 ) ) ;
#21434 = CARTESIAN_POINT ( 'NONE',  ( 0.1771653543307093182, -0.5400638737290845981, -0.3530559997133363437 ) ) ;
#21435 = VERTEX_POINT ( 'NONE', #11188 ) ;
#21436 = CARTESIAN_POINT ( 'NONE',  ( 0.2925321140481932369, 0.2925321140481932369, -1.870078740157480546 ) ) ;
#21437 = CARTESIAN_POINT ( 'NONE',  ( -0.2925321140481932369, 0.2925321140481931259, -1.041338582677165281 ) ) ;
#21438 = CARTESIAN_POINT ( 'NONE',  ( 0.3996062992125984925, 0.1070741851644054637, -0.3589238845144357426 ) ) ;
#21439 = CARTESIAN_POINT ( 'NONE',  ( -0.7217847769028863381, 0.05413385826771626580, -0.4176697321401330321 ) ) ;
#21440 = CARTESIAN_POINT ( 'NONE',  ( -1.157146581871515012E-16, 0.4724409448818898682, 0.1574803149606299191 ) ) ;
#21441 = CARTESIAN_POINT ( 'NONE',  ( -0.1049643490035307020, 0.3917322834645669549, -2.295931758530183497 ) ) ;
#21442 = CARTESIAN_POINT ( 'NONE',  ( -1.627296587926508442, 0.1283753931104748280, 0.1820866141732283561 ) ) ;
#21443 = CARTESIAN_POINT ( 'NONE',  ( 0.7086614173228352742, -0.1870078740157480879, -0.4822834645669291653 ) ) ;
#21444 = CARTESIAN_POINT ( 'NONE',  ( 0.7939632545931766261, -0.3162353388693409650, -0.4822834645669289433 ) ) ;
#21445 = CARTESIAN_POINT ( 'NONE',  ( -0.2034120734908128059, 0.1771653543307087630, 0.09757992244046791164 ) ) ;
#21446 = CARTESIAN_POINT ( 'NONE',  ( 0.1574803149606306130, -0.1870078740157479769, 0.4822834645669291653 ) ) ;
#21447 = CARTESIAN_POINT ( 'NONE',  ( 0.3458507752293908943, -0.3458507752293908943, -2.064960629921259283 ) ) ;
#21448 = CARTESIAN_POINT ( 'NONE',  ( -0.2624671916010490880, -0.5023911411419708095, 0.1820866141732285504 ) ) ;
#21449 = CARTESIAN_POINT ( 'NONE',  ( -0.04593175853018302557, -0.6692913385826773087, -0.1292274648535924053 ) ) ;
#21450 = CARTESIAN_POINT ( 'NONE',  ( -0.1058382717557503072, 0.3949938075777408852, -1.343175853018372834 ) ) ;
#21451 = CARTESIAN_POINT ( 'NONE',  ( 1.581364829396326277, -0.08942795157527998196, 0.3641732283464567121 ) ) ;
#21452 = CARTESIAN_POINT ( 'NONE',  ( 0.1706036745406830368, -0.004921259842519576551, 0.3153832671262227771 ) ) ;
#21453 = FACE_OUTER_BOUND ( 'NONE', #6801, .T. ) ;
#21454 = CARTESIAN_POINT ( 'NONE',  ( -0.9383202099737524282, -0.05778040916215522460, 0.4822834645669289988 ) ) ;
#21455 = CARTESIAN_POINT ( 'NONE',  ( -0.8136482939632537770, 0.1283753931104746893, -0.1820866141732285504 ) ) ;
#21456 = CARTESIAN_POINT ( 'NONE',  ( -1.033630966599879297, -2.567464376874931580E-15, -0.4445507791589072832 ) ) ;
#21457 = CARTESIAN_POINT ( 'NONE',  ( -0.6496062992125976043, -0.5400638737290844871, 0.3530559997133364547 ) ) ;
#21458 = CARTESIAN_POINT ( 'NONE',  ( -0.6102362204724400829, -0.5400638737290845981, -0.3530559997133363437 ) ) ;
#21459 = CARTESIAN_POINT ( 'NONE',  ( 0.04593175853018440641, -0.6692913385826771977, 0.1292274648535927661 ) ) ;
#21460 = CARTESIAN_POINT ( 'NONE',  ( 0.1998031496062992463, 0.3460692066303959202, -2.425853018372703396 ) ) ;
#21461 = CARTESIAN_POINT ( 'NONE',  ( 0.1958661417322836162, -0.3392501089628018329, -2.061660474244408014 ) ) ;
#21462 = CARTESIAN_POINT ( 'NONE',  ( -0.5314960629921124946, 2.746034003362847198, -3.861376881555341978 ) ) ;
#21463 = CARTESIAN_POINT ( 'NONE',  ( 0.6102362204724416372, 0.07958543189024071263, -0.2665933059059888421 ) ) ;
#21464 = CARTESIAN_POINT ( 'NONE',  ( 1.437007874015748810, 0.1660481256975885056, 0.3530559997133364547 ) ) ;
#21465 = CARTESIAN_POINT ( 'NONE',  ( -1.437007874015747477, -0.4536011799217367080, 0.2665933059059888421 ) ) ;
#21466 = CARTESIAN_POINT ( 'NONE',  ( 1.351706036745407680, 0.05413385826771666132, 0.4176697321401328100 ) ) ;
#21467 = CARTESIAN_POINT ( 'NONE',  ( -1.148293963254592542, -0.5511811023622048555, -0.09757992244046775898 ) ) ;
#21468 = CARTESIAN_POINT ( 'NONE',  ( -0.6364829396325453192, -0.3162353388693405765, 0.4822834645669290543 ) ) ;
#21469 = CARTESIAN_POINT ( 'NONE',  ( 0.2624671916010504757, 0.1283753931104748280, 0.1820866141732283561 ) ) ;
#21470 = CARTESIAN_POINT ( 'NONE',  ( -0.4724409448818898682, -8.678599364036362592E-17, -0.8267716535433070613 ) ) ;
#21471 = CARTESIAN_POINT ( 'NONE',  ( 0.5839895013123367340, -0.5511811023622048555, -0.09757992244046775898 ) ) ;
#21472 = CARTESIAN_POINT ( 'NONE',  ( 0.4724409448818904789, -0.1870078740157480879, -0.4822834645669291653 ) ) ;
#21473 = CARTESIAN_POINT ( 'NONE',  ( 0.1070741851644054776, -0.3996062992125984925, -0.4770341207349080848 ) ) ;
#21474 = CARTESIAN_POINT ( 'NONE',  ( -0.7808398950131225646, -0.05778040916215522460, 0.4822834645669289988 ) ) ;
#21475 = CARTESIAN_POINT ( 'NONE',  ( 4.797336870675656522E-17, -0.3917322834645670104, -1.265748031496062964 ) ) ;
#21476 = CARTESIAN_POINT ( 'NONE',  ( 0.9580052493438326877, -0.004921259842519576551, 0.3153832671262227771 ) ) ;
#21477 = CARTESIAN_POINT ( 'NONE',  ( 0.6102362204724416372, 0.1660481256975883668, -0.3530559997133364547 ) ) ;
#21478 = CARTESIAN_POINT ( 'NONE',  ( -0.1509186351706028884, -0.3162353388693409650, -0.4822834645669289433 ) ) ;
#21479 = CARTESIAN_POINT ( 'NONE',  ( -0.3412073490813641308, 0.1283753931104746893, -0.1820866141732285504 ) ) ;
#21480 = DIRECTION ( 'NONE',  ( 0.000000000000000000, -0.9925461516413219831, -0.1218693434051477398 ) ) ;
#21481 = CARTESIAN_POINT ( 'NONE',  ( -0.1312335958005241554, -0.5023911411419708095, -0.1820866141732282451 ) ) ;
#21482 = CARTESIAN_POINT ( 'NONE',  ( 0.3805774278215230400, -0.4281496062992124485, 0.4176697321401328655 ) ) ;
#21483 = CARTESIAN_POINT ( 'NONE',  ( -0.7349081364829390672, 0.1283753931104746893, -0.1820866141732285504 ) ) ;
#21484 = CARTESIAN_POINT ( 'NONE',  ( 0.3996062992125985480, 2.446882876249141654E-17, -1.139763779527559029 ) ) ;
#21485 = CARTESIAN_POINT ( 'NONE',  ( -1.030183727034119867, -0.3162353388693405765, 0.4822834645669290543 ) ) ;
#21486 = CARTESIAN_POINT ( 'NONE',  ( -0.8546455861312985958, -4.966502543501560364E-15, 0.3791483426435189319 ) ) ;
#21487 = VERTEX_POINT ( 'NONE', #17104 ) ;
#21488 = CARTESIAN_POINT ( 'NONE',  ( -1.187664041994750175, -0.08942795157528024563, -0.3641732283464568787 ) ) ;
#21489 = CARTESIAN_POINT ( 'NONE',  ( -0.1509186351706028884, -0.05778040916215522460, 0.4822834645669289988 ) ) ;
#21490 = CARTESIAN_POINT ( 'NONE',  ( -1.646981627296586703, -0.3162353388693409650, -0.4822834645669289433 ) ) ;
#21491 = CARTESIAN_POINT ( 'NONE',  ( -0.8530183727034112984, 0.05413385826771666132, 0.4176697321401328100 ) ) ;
#21492 = LINE ( 'NONE', #14782, #80805 ) ;
#21494 = CARTESIAN_POINT ( 'NONE',  ( 0.9448818897637802916, -0.1870078740157479769, 0.4822834645669291653 ) ) ;
#21493 = CARTESIAN_POINT ( 'NONE',  ( 1.043307086614173818, 0.1660481256975885056, 0.3530559997133364547 ) ) ;
#21495 = CARTESIAN_POINT ( 'NONE',  ( 0.8727034120734913358, -0.05778040916215522460, 0.4822834645669289988 ) ) ;
#21496 = CARTESIAN_POINT ( 'NONE',  ( -0.2952755905511805223, 0.1012011053420777407, 0.2882089793578257453 ) ) ;
#21497 = CARTESIAN_POINT ( 'NONE',  ( 0.1938976377952755792, 0.1938976377952755792, 0.07874015748031495954 ) ) ;
#21498 = CARTESIAN_POINT ( 'NONE',  ( -1.482939632545930975, -0.4281496062992127816, -0.4176697321401328100 ) ) ;
#21499 = EDGE_CURVE ( 'NONE', #32355, #20489, #61276, .T. ) ;
#21500 = CARTESIAN_POINT ( 'NONE',  ( -9.787531504996567848E-17, 0.3996062992125986035, -0.3149606299212598381 ) ) ;
#21501 = ORIENTED_EDGE ( 'NONE', *, *, #6391, .F. ) ;
#21502 = CARTESIAN_POINT ( 'NONE',  ( -0.3280839895013117347, -0.004921259842519870586, -0.3153832671262229437 ) ) ;
#21503 = CARTESIAN_POINT ( 'NONE',  ( -0.1958661417322836718, 0.3392501089628017219, -2.209973753280840114 ) ) ;
#21504 = ORIENTED_EDGE ( 'NONE', *, *, #4894, .F. ) ;
#21505 = CARTESIAN_POINT ( 'NONE',  ( 0.6889763779527563470, 0.1660481256975883668, -0.3530559997133364547 ) ) ;
#21506 = CARTESIAN_POINT ( 'NONE',  ( 0.2230971128608929543, 0.05413385826771626580, -0.4176697321401330321 ) ) ;
#21507 = CARTESIAN_POINT ( 'NONE',  ( -0.8464566929133852113, 0.1660481256975885056, 0.3530559997133364547 ) ) ;
#21508 = CARTESIAN_POINT ( 'NONE',  ( 1.686351706036745890, 0.2952755905511811885, 0.1292274648535926551 ) ) ;
#21509 = CARTESIAN_POINT ( 'NONE',  ( -0.8398950131233585692, 0.1283753931104748280, 0.1820866141732283561 ) ) ;
#21510 = CARTESIAN_POINT ( 'NONE',  ( -0.4603218807116740141, 1.653261878685372777, -2.586075122629556411 ) ) ;
#21511 = CARTESIAN_POINT ( 'NONE',  ( 0.3674540682414705883, -0.6046776061558807314, 0.2411417322834647770 ) ) ;
#21512 = CARTESIAN_POINT ( 'NONE',  ( 0.6824146981627303710, 0.1283753931104746893, -0.1820866141732285504 ) ) ;
#21513 = CARTESIAN_POINT ( 'NONE',  ( -0.9973753280839886548, 0.2306618581243848609, 0.2411417322834645549 ) ) ;
#21514 = CARTESIAN_POINT ( 'NONE',  ( 0.1958661417322836162, -0.3392501089628018329, -1.746699844323147843 ) ) ;
#21515 = CARTESIAN_POINT ( 'NONE',  ( -1.227034120734907141, -0.6692913385826773087, -0.1292274648535924053 ) ) ;
#21516 = CARTESIAN_POINT ( 'NONE',  ( -1.033630966599879297, -2.567464376874931580E-15, -0.4445507791589072832 ) ) ;
#21517 = CARTESIAN_POINT ( 'NONE',  ( 1.227034120734908917, 0.2952755905511810774, -0.1292274648535930714 ) ) ;
#21518 = CARTESIAN_POINT ( 'NONE',  ( 1.279527559055118724, -0.4536011799217368745, -0.2665933059059886201 ) ) ;
#21519 = ORIENTED_EDGE ( 'NONE', *, *, #52927, .F. ) ;
#21520 = CARTESIAN_POINT ( 'NONE',  ( -0.2867679344610365444, -0.2867679344610367664, -2.890439263288400618 ) ) ;
#21521 = CARTESIAN_POINT ( 'NONE',  ( -0.4461942257217840213, -0.6046776061558809534, -0.2411417322834644161 ) ) ;
#21522 = ORIENTED_EDGE ( 'NONE', *, *, #54718, .F. ) ;
#21523 = CARTESIAN_POINT ( 'NONE',  ( 0.9514435695538062676, -0.08942795157527998196, 0.3641732283464567121 ) ) ;
#21524 = CARTESIAN_POINT ( 'NONE',  ( -1.148293963254592542, -0.6692913385826773087, -0.1292274648535924053 ) ) ;
#21525 = CARTESIAN_POINT ( 'NONE',  ( 0.9186351706036751663, -0.6046776061558807314, 0.2411417322834647770 ) ) ;
#21526 = CARTESIAN_POINT ( 'NONE',  ( 0.9317585301837276734, -0.4281496062992124485, 0.4176697321401328655 ) ) ;
#21527 = CARTESIAN_POINT ( 'NONE',  ( 0.1049868766404206816, -0.6046776061558809534, -0.2411417322834644161 ) ) ;
#21528 = CARTESIAN_POINT ( 'NONE',  ( -0.5446194225721777693, -0.05778040916215522460, 0.4822834645669289988 ) ) ;
#21529 = CARTESIAN_POINT ( 'NONE',  ( -0.2867679344610364334, -0.2867679344610367109, -1.875984251968503935 ) ) ;
#21530 = CARTESIAN_POINT ( 'NONE',  ( 1.541994750656168645, -0.5511811023622046335, 0.09757992244046803654 ) ) ;
#21531 = CARTESIAN_POINT ( 'NONE',  ( -0.7874015748031489847, -0.1870078740157480879, -0.4822834645669291653 ) ) ;
#21532 = CARTESIAN_POINT ( 'NONE',  ( -0.5643044619422565855, -0.3690944881889763329, 0.3153832671262228327 ) ) ;
#21533 = CARTESIAN_POINT ( 'NONE',  ( -0.1208384647389192101, 0.3726288332213502641, 1.112018681666451222E-17 ) ) ;
#21534 = CARTESIAN_POINT ( 'NONE',  ( 1.561679790026247350, 0.05413385826771626580, -0.4176697321401330321 ) ) ;
#21535 = CARTESIAN_POINT ( 'NONE',  ( -0.3412073490813641308, -0.6046776061558807314, 0.2411417322834647770 ) ) ;
#21536 = CARTESIAN_POINT ( 'NONE',  ( 0.3996062992125984925, 0.1070741851644054637, -0.04396325459317586282 ) ) ;
#21537 = CARTESIAN_POINT ( 'NONE',  ( 0.6299212598425204535, -0.1870078740157479769, 0.4822834645669291653 ) ) ;
#21538 = CARTESIAN_POINT ( 'NONE',  ( -0.1070741851644051862, -0.3996062992125987146, -1.961942257217847763 ) ) ;
#21539 = DIRECTION ( 'NONE',  ( 0.000000000000000000, 0.000000000000000000, -1.000000000000000000 ) ) ;
#21540 = CARTESIAN_POINT ( 'NONE',  ( -0.02624671916010428221, 0.2306618581243847221, -0.2411417322834647770 ) ) ;
#21542 = CARTESIAN_POINT ( 'NONE',  ( -1.603475055217291612, 0.4410854135902511630, -0.04573490813648263542 ) ) ;
#21541 = CARTESIAN_POINT ( 'NONE',  ( 0.8595800524934390507, -0.2845877964562159024, 0.3641732283464567677 ) ) ;
#21543 = CARTESIAN_POINT ( 'NONE',  ( -0.1265901696524993347, 0.4724409448818895907, -0.5557742782152230721 ) ) ;
#21544 = CARTESIAN_POINT ( 'NONE',  ( 1.076115485564305141, 0.1283753931104746893, -0.1820866141732285504 ) ) ;
#21545 = CARTESIAN_POINT ( 'NONE',  ( 1.318897637795276356, 0.1660481256975883668, -0.3530559997133364547 ) ) ;
#21546 = CARTESIAN_POINT ( 'NONE',  ( 0.2891555358219910499, 0.2891555358219910499, -0.2145669291338582474 ) ) ;
#21547 = CARTESIAN_POINT ( 'NONE',  ( -0.3018372703412066094, 0.05413385826771666132, 0.4176697321401328100 ) ) ;
#21548 = CARTESIAN_POINT ( 'NONE',  ( -1.646981627296586703, -0.05778040916215522460, 0.4822834645669289988 ) ) ;
#21549 = CARTESIAN_POINT ( 'NONE',  ( 1.482939632545932307, -0.004921259842519870586, -0.3153832671262229437 ) ) ;
#21550 = CARTESIAN_POINT ( 'NONE',  ( -0.1706036745406816491, -0.4281496062992124485, 0.4176697321401328655 ) ) ;
#21551 = CARTESIAN_POINT ( 'NONE',  ( -0.3420746716998662729, 0.1974969037888702206, -0.4179790026246719137 ) ) ;
#21552 = CARTESIAN_POINT ( 'NONE',  ( 1.286089238845145033, -0.6046776061558809534, -0.2411417322834644161 ) ) ;
#21553 = CARTESIAN_POINT ( 'NONE',  ( 0.4396325459317590445, -0.6692913385826771977, 0.1292274648535927661 ) ) ;
#21554 = CARTESIAN_POINT ( 'NONE',  ( 0.5314960629921267055, -0.4536011799217367080, 0.2665933059059888421 ) ) ;
#21555 = DIRECTION ( 'NONE',  ( -0.000000000000000000, 1.000000000000000000, -0.000000000000000000 ) ) ;
#21556 = CARTESIAN_POINT ( 'NONE',  ( 0.4986876640419954376, -0.5023911411419708095, -0.1820866141732282451 ) ) ;
#21557 = CARTESIAN_POINT ( 'NONE',  ( -1.089238845144356427, 0.009842519685039463617, 0.3409548833797002576 ) ) ;
#21558 = CARTESIAN_POINT ( 'NONE',  ( -0.2925321140481930149, -0.2925321140481933480, -1.395669291338582640 ) ) ;
#21559 = CARTESIAN_POINT ( 'NONE',  ( 0.6561679790026253567, -0.6046776061558809534, -0.2411417322834644161 ) ) ;
#21560 = CARTESIAN_POINT ( 'NONE',  ( -0.2867679344610365999, 0.2867679344610364889, -1.271653543307086798 ) ) ;
#21561 = PLANE ( 'NONE',  #23756 ) ;
#21562 = DIRECTION ( 'NONE',  ( 0.000000000000000000, 0.000000000000000000, -1.000000000000000000 ) ) ;
#21563 = CARTESIAN_POINT ( 'NONE',  ( 0.04593175853018440641, 0.1771653543307087075, -0.09757992244046823083 ) ) ;
#21564 = CARTESIAN_POINT ( 'NONE',  ( 0.1968503937007881344, -0.6692913385826771977, 8.415575281601705876E-17 ) ) ;
#21565 = CARTESIAN_POINT ( 'NONE',  ( 1.253280839895013710, -0.08942795157528024563, -0.3641732283464568787 ) ) ;
#21566 = CARTESIAN_POINT ( 'NONE',  ( -1.364829396325458521, 0.1283753931104746893, -0.1820866141732285504 ) ) ;
#21567 = CARTESIAN_POINT ( 'NONE',  ( -1.017060367454067249, -0.3162353388693409650, -0.4822834645669289433 ) ) ;
#21568 = CARTESIAN_POINT ( 'NONE',  ( -1.699475065616797398, 0.2952755905511811885, 0.1292274648535926551 ) ) ;
#21569 = CARTESIAN_POINT ( 'NONE',  ( 0.4593175853018380828, 0.05413385826771626580, -0.4176697321401330321 ) ) ;
#21570 = CARTESIAN_POINT ( 'NONE',  ( 1.594488188976378673, -0.5400638737290845981, -0.3530559997133363437 ) ) ;
#21571 = DIRECTION ( 'NONE',  ( 0.000000000000000000, -1.000000000000000000, 0.000000000000000000 ) ) ;
#21572 = CARTESIAN_POINT ( 'NONE',  ( 0.5643044619422579178, -0.4281496062992127816, -0.4176697321401328100 ) ) ;
#21573 = CARTESIAN_POINT ( 'NONE',  ( 0.4724409448818896462, 0.1265901696524990294, -2.721128608923884418 ) ) ;
#21574 = CARTESIAN_POINT ( 'NONE',  ( 0.1818524038564936218, 1.098415106551606346, 3.932883554691550376 ) ) ;
#21575 = CARTESIAN_POINT ( 'NONE',  ( 1.305774278215223960, -0.6692913385826771977, 0.1292274648535927661 ) ) ;
#21576 = CARTESIAN_POINT ( 'NONE',  ( -1.272965879265091305, -0.3690944881889763329, 0.3153832671262228327 ) ) ;
#21577 = CARTESIAN_POINT ( 'NONE',  ( 1.325459317585302665, -0.3690944881889763329, 0.3153832671262228327 ) ) ;
#21578 = CARTESIAN_POINT ( 'NONE',  ( -1.259842519685038686, -0.1870078740157480601, -0.3641732283464567677 ) ) ;
#21579 = CARTESIAN_POINT ( 'NONE',  ( -0.8923884514435688198, -0.5023911411419708095, 0.1820866141732285504 ) ) ;
#21580 = CARTESIAN_POINT ( 'NONE',  ( 1.601049868766404982, 0.2306618581243848609, 0.2411417322834645549 ) ) ;
#21581 = CARTESIAN_POINT ( 'NONE',  ( 0.6233595800524939223, -0.2845877964562159024, 0.3641732283464567677 ) ) ;
#21582 = CARTESIAN_POINT ( 'NONE',  ( 0.2821522309711292364, 0.2952755905511810774, -0.1292274648535930714 ) ) ;
#21583 = CARTESIAN_POINT ( 'NONE',  ( 1.240157480314961314, -0.5400638737290844871, 0.3530559997133364547 ) ) ;
#21584 = CARTESIAN_POINT ( 'NONE',  ( -0.08530183727034056085, -0.3162353388693405765, 0.4822834645669290543 ) ) ;
#21585 = CARTESIAN_POINT ( 'NONE',  ( 0.2821522309711292364, -0.5511811023622046335, 0.09757992244046803654 ) ) ;
#21586 = CARTESIAN_POINT ( 'NONE',  ( 1.312335958005249825, 0.2306618581243847221, -0.2411417322834647770 ) ) ;
#21587 = ADVANCED_FACE ( 'NONE', ( #43145 ), #37264, .T. ) ;
#21588 = DIRECTION ( 'NONE',  ( -0.000000000000000000, -1.000000000000000000, -0.000000000000000000 ) ) ;
#21589 = CARTESIAN_POINT ( 'NONE',  ( -1.082677165354329896, 0.1660481256975885056, 0.3530559997133364547 ) ) ;
#21590 = CARTESIAN_POINT ( 'NONE',  ( 4.893765752498283924E-17, -0.3996062992125986035, -0.7086614173228346081 ) ) ;
#21591 = CARTESIAN_POINT ( 'NONE',  ( 1.013613127888309595, -4.408777212815537393E-16, -0.4445507791589063395 ) ) ;
#21592 = CARTESIAN_POINT ( 'NONE',  ( -0.8989501312335946848, -0.6692913385826771977, 0.1292274648535927661 ) ) ;
#21593 = CARTESIAN_POINT ( 'NONE',  ( 0.03280839895013198948, 0.2952755905511811885, 0.1292274648535926551 ) ) ;
#21594 = CARTESIAN_POINT ( 'NONE',  ( 0.3996062992125986590, -0.1070741851644053111, -2.631233595800525293 ) ) ;
#21595 = CARTESIAN_POINT ( 'NONE',  ( -0.3949938075777409963, -7.255918531996591613E-17, -2.244094488188976388 ) ) ;
#21596 = EDGE_LOOP ( 'NONE', ( #28774, #51280, #75457, #33719 ) ) ;
#21597 = CARTESIAN_POINT ( 'NONE',  ( -0.3917322834645670104, -7.196005306013484475E-17, -1.133858267716535195 ) ) ;
#21598 = EDGE_CURVE ( 'NONE', #69851, #44891, #2714, .T. ) ;
#21599 = CARTESIAN_POINT ( 'NONE',  ( 1.148293963254593653, 0.2952755905511810774, -0.1292274648535930714 ) ) ;
#21600 = CARTESIAN_POINT ( 'NONE',  ( -0.2462293917967295909, -2.567464376874931580E-15, -0.4445507791589072832 ) ) ;
#21602 = VECTOR ( 'NONE', #22735, 39.37007874015748143 ) ;
#21601 = CARTESIAN_POINT ( 'NONE',  ( -1.496062992125983815, -0.1870078740157480601, -0.3641732283464567677 ) ) ;
#21603 = CARTESIAN_POINT ( 'NONE',  ( 0.1958661417322836440, -0.3392501089628017219, -1.186351706036745446 ) ) ;
#21604 = CARTESIAN_POINT ( 'NONE',  ( 1.581364829396326277, -0.08942795157527998196, 0.3641732283464567121 ) ) ;
#21605 = CARTESIAN_POINT ( 'NONE',  ( -0.3917322834645669549, -7.196005306013483243E-17, 0.1955573735246212974 ) ) ;
#21606 = CARTESIAN_POINT ( 'NONE',  ( -0.1574803149606292529, -0.1870078740157480879, -0.4822834645669291653 ) ) ;
#21607 = CARTESIAN_POINT ( 'NONE',  ( -0.4790026246719154557, -0.2845877964562159024, 0.3641732283464567677 ) ) ;
#21608 = CARTESIAN_POINT ( 'NONE',  ( 0.9317585301837276734, -0.4281496062992124485, 0.4176697321401328655 ) ) ;
#21609 = CARTESIAN_POINT ( 'NONE',  ( 0.3018372703412079971, -0.4281496062992124485, 0.4176697321401328655 ) ) ;
#21610 = CARTESIAN_POINT ( 'NONE',  ( 2.362204724409448620, 1.929133858267716661, 8.247593713802677664E-15 ) ) ;
#21611 = CARTESIAN_POINT ( 'NONE',  ( -0.2925321140481930704, -0.2925321140481933480, -2.893700787401574992 ) ) ;
#21612 = CARTESIAN_POINT ( 'NONE',  ( -0.3917322834645670659, -7.196005306013484475E-17, -1.138470759351392969 ) ) ;
#21613 = CARTESIAN_POINT ( 'NONE',  ( 1.161417322834646493, -0.5400638737290844871, 0.3530559997133364547 ) ) ;
#21614 = CARTESIAN_POINT ( 'NONE',  ( 0.2624671916010504757, -0.6046776061558809534, -0.2411417322834644161 ) ) ;
#21615 = CARTESIAN_POINT ( 'NONE',  ( -0.8398950131233585692, 0.2306618581243848609, 0.2411417322834645549 ) ) ;
#21616 = CARTESIAN_POINT ( 'NONE',  ( 1.345144356955381593, -0.3162353388693409650, -0.4822834645669289433 ) ) ;
#21617 = CARTESIAN_POINT ( 'NONE',  ( 0.8267716535433078384, -0.6692913385826771977, 8.415575281601705876E-17 ) ) ;
#21618 = CARTESIAN_POINT ( 'NONE',  ( -0.1958661417322836718, 0.3392501089628017219, -0.5702099737532808632 ) ) ;
#21619 = CARTESIAN_POINT ( 'NONE',  ( -0.07217847769028813698, -0.3162353388693409650, -0.4822834645669289433 ) ) ;
#21620 = CARTESIAN_POINT ( 'NONE',  ( 0.5971128608923891301, 0.2952755905511810774, -0.1292274648535930714 ) ) ;
#21621 = CARTESIAN_POINT ( 'NONE',  ( 0.1706036745406830368, -0.4281496062992127816, -0.4176697321401328100 ) ) ;
#21622 = CARTESIAN_POINT ( 'NONE',  ( 0.9317585301837276734, -0.004921259842519870586, -0.3153832671262229437 ) ) ;
#21623 = CARTESIAN_POINT ( 'NONE',  ( -1.515748031496062076, 0.1660481256975883668, -0.3530559997133364547 ) ) ;
#21624 = CARTESIAN_POINT ( 'NONE',  ( -1.397637795275589623, 0.1660481256975885056, 0.3530559997133364547 ) ) ;
#21625 = CARTESIAN_POINT ( 'NONE',  ( 0.5905511811023629321, -0.6692913385826771977, 8.415575281601705876E-17 ) ) ;
#21626 = CARTESIAN_POINT ( 'NONE',  ( 0.2362204724409449064, 0.4091458600556404646, -0.5360892388451443669 ) ) ;
#21627 = CARTESIAN_POINT ( 'NONE',  ( -0.2867679344610365999, 0.2867679344610364889, -2.216535433070866201 ) ) ;
#21628 =( BOUNDED_CURVE ( )  B_SPLINE_CURVE ( 1, ( #79549, #46699 ),
 .UNSPECIFIED., .F., .F. ) 
 B_SPLINE_CURVE_WITH_KNOTS ( ( 2, 2 ),
 ( 0.000000000000000000, 0.002000000000000005246 ),
 .UNSPECIFIED. ) 
 CURVE ( )  GEOMETRIC_REPRESENTATION_ITEM ( )  RATIONAL_B_SPLINE_CURVE ( ( 0.9875488213027527884, 0.9875488213027527884 ) ) 
 REPRESENTATION_ITEM ( '' )  );
#21629 = VERTEX_POINT ( 'NONE', #5273 ) ;
#21630 = CARTESIAN_POINT ( 'NONE',  ( -0.3460692066303960868, 0.1998031496062990242, -0.3412073490813647969 ) ) ;
#21631 = VERTEX_POINT ( 'NONE', #24210 ) ;
#21632 = CARTESIAN_POINT ( 'NONE',  ( 1.056430446194226658, 0.2952755905511811885, 0.1292274648535926551 ) ) ;
#21633 = CARTESIAN_POINT ( 'NONE',  ( 0.7020997375328090762, -0.08942795157528024563, -0.3641732283464568787 ) ) ;
#21634 = CARTESIAN_POINT ( 'NONE',  ( 3.224202737261815166, 2.716535433070866645, -0.5314960629921260393 ) ) ;
#21635 = DIRECTION ( 'NONE',  ( -1.000000000000000000, -3.050063254464715781E-16, 0.000000000000000000 ) ) ;
#21636 = CARTESIAN_POINT ( 'NONE',  ( -1.614173228346456712, 1.818966223839196816, -0.1372047244094478091 ) ) ;
#21637 = CARTESIAN_POINT ( 'NONE',  ( 0.2867679344610365999, 0.2867679344610365999, -1.324803149606299302 ) ) ;
#21638 = CARTESIAN_POINT ( 'NONE',  ( -9.787531504996566615E-17, 0.3996062992125985480, -1.966535433070865979 ) ) ;
#21639 = CARTESIAN_POINT ( 'NONE',  ( -0.3964540044758075865, -0.009627693922155141845, -1.929133858265299484 ) ) ;
#21640 = CARTESIAN_POINT ( 'NONE',  ( -0.2952755905511804668, 0.1660481256975885056, 0.3530559997133364547 ) ) ;
#21641 = CARTESIAN_POINT ( 'NONE',  ( 0.9055118110236227702, -0.6692913385826771977, 8.415575281601705876E-17 ) ) ;
#21642 = ORIENTED_EDGE ( 'NONE', *, *, #74375, .F. ) ;
#21643 = CARTESIAN_POINT ( 'NONE',  ( -1.437007874015747477, -0.5400638737290844871, 0.3530559997133364547 ) ) ;
#21644 = CARTESIAN_POINT ( 'NONE',  ( -1.170004705068745876, -4.983732387537991731E-15, 0.3954985857520076920 ) ) ;
#21645 = CARTESIAN_POINT ( 'NONE',  ( -0.4094517204008080169, 3.916330350904249524, 5.973313079581500595 ) ) ;
#21646 = CARTESIAN_POINT ( 'NONE',  ( 1.469816272965879911, -0.5023911411419708095, 0.1820866141732285504 ) ) ;
#21647 = DIRECTION ( 'NONE',  ( 0.000000000000000000, 0.000000000000000000, -1.000000000000000000 ) ) ;
#21648 = CARTESIAN_POINT ( 'NONE',  ( -1.397637795275589623, -0.4536011799217368745, -0.2665933059059886201 ) ) ;
#21649 = LINE ( 'NONE', #70925, #44909 ) ;
#21650 = CARTESIAN_POINT ( 'NONE',  ( 0.3215223097112867578, -0.3162353388693409650, -0.4822834645669289433 ) ) ;
#21651 = ORIENTED_EDGE ( 'NONE', *, *, #15607, .T. ) ;
#21653 = CARTESIAN_POINT ( 'NONE',  ( -0.4600214019799515053, 0.000000000000000000, 0.3464511005275205946 ) ) ;
#21652 = CARTESIAN_POINT ( 'NONE',  ( 1.620734908136483465, -0.6692913385826771977, 0.1292274648535927661 ) ) ;
#21654 = CARTESIAN_POINT ( 'NONE',  ( -0.9186351706036736120, 0.1283753931104748280, 0.1820866141732283561 ) ) ;
#21655 = CARTESIAN_POINT ( 'NONE',  ( 0.7874015748031503170, -0.1870078740157480879, -0.4822834645669291653 ) ) ;
#21656 = CARTESIAN_POINT ( 'NONE',  ( 1.154855643044620184, 0.1283753931104746893, -0.1820866141732285504 ) ) ;
#21657 = CARTESIAN_POINT ( 'NONE',  ( 4.797336870675655290E-17, -0.3917322834645669549, -1.261135539861205412 ) ) ;
#21658 = CARTESIAN_POINT ( 'NONE',  ( -0.6102362204724400829, 0.07958543189024085140, 0.2665933059059887866 ) ) ;
#21659 = CARTESIAN_POINT ( 'NONE',  ( -1.581364829396324945, -0.08942795157528024563, -0.3641732283464568787 ) ) ;
#21660 = CARTESIAN_POINT ( 'NONE',  ( 0.2979138814448422101, 1.789193252437325743, 0.09652054087235428792 ) ) ;
#21661 = CARTESIAN_POINT ( 'NONE',  ( 0.5183727034120741983, 0.2952755905511810774, -0.1292274648535930714 ) ) ;
#21662 = CARTESIAN_POINT ( 'NONE',  ( -0.7742782152230962556, -0.3690944881889765550, -0.3153832671262227771 ) ) ;
#21663 = CARTESIAN_POINT ( 'NONE',  ( -0.2887139107611542133, 0.1283753931104748280, 0.1820866141732283561 ) ) ;
#21664 = AXIS2_PLACEMENT_3D ( 'NONE', #5031, #5439, #57175 ) ;
#21665 = CARTESIAN_POINT ( 'NONE',  ( -0.4790026246719154557, -0.3162353388693405765, 0.4822834645669290543 ) ) ;
#21666 = CARTESIAN_POINT ( 'NONE',  ( -1.528871391076114250, -0.5511811023622046335, 0.09757992244046803654 ) ) ;
#21667 = CARTESIAN_POINT ( 'NONE',  ( 0.3917322834645670104, 0.1049643490035304660, 0.03606992306330520509 ) ) ;
#21668 = CARTESIAN_POINT ( 'NONE',  ( 0.6496062992125991586, 0.1660481256975885056, 0.3530559997133364547 ) ) ;
#21669 = CARTESIAN_POINT ( 'NONE',  ( 0.1265901696524990572, -0.4724409448818897017, -0.2427821522309711322 ) ) ;
#21670 = CARTESIAN_POINT ( 'NONE',  ( 5.785732909357575061E-17, -0.4724409448818898682, -1.415354330708661346 ) ) ;
#21671 = CARTESIAN_POINT ( 'NONE',  ( -0.8727034120734901146, -0.05778040916215560624, -0.4822834645669293319 ) ) ;
#21672 = CARTESIAN_POINT ( 'NONE',  ( -0.3805774278215216522, -0.3690944881889765550, -0.3153832671262227771 ) ) ;
#21673 = CARTESIAN_POINT ( 'NONE',  ( -1.391076115485563314, -0.6046776061558809534, -0.2411417322834644161 ) ) ;
#21674 = CARTESIAN_POINT ( 'NONE',  ( 0.4658792650918641698, -0.08942795157528024563, -0.3641732283464568787 ) ) ;
#21675 = CARTESIAN_POINT ( 'NONE',  ( -0.5183727034120726440, -0.5511811023622048555, -0.09757992244046775898 ) ) ;
#21676 = CARTESIAN_POINT ( 'NONE',  ( -1.030183727034119867, -0.05778040916215560624, -0.4822834645669293319 ) ) ;
#21677 = CARTESIAN_POINT ( 'NONE',  ( 1.594488188976378673, 0.07958543189024085140, 0.2665933059059887866 ) ) ;
#21678 = CARTESIAN_POINT ( 'NONE',  ( 1.220472440944882608, 0.2952755905511811885, 0.000000000000000000 ) ) ;
#21679 = CARTESIAN_POINT ( 'NONE',  ( -1.614173228346456712, 2.362204724409448620, -0.1372047244094478091 ) ) ;
#21680 = CARTESIAN_POINT ( 'NONE',  ( 0.9908136482939640111, -0.5511811023622046335, 0.09757992244046803654 ) ) ;
#21681 = CARTESIAN_POINT ( 'NONE',  ( 0.4986876640419954376, -0.6046776061558809534, -0.2411417322834644161 ) ) ;
#21682 = CARTESIAN_POINT ( 'NONE',  ( -1.827151678354258069, 2.742788175498064529, 0.5314960629921260393 ) ) ;
#21683 = CARTESIAN_POINT ( 'NONE',  ( 1.213910761154856299, -0.5511811023622048555, -0.09757992244046775898 ) ) ;
#21684 = ORIENTED_EDGE ( 'NONE', *, *, #73728, .T. ) ;
#21685 = CARTESIAN_POINT ( 'NONE',  ( -9.787531504996566615E-17, 0.3996062992125985480, -2.753937007874015741 ) ) ;
#21686 = CARTESIAN_POINT ( 'NONE',  ( -1.213910761154854745, -0.5511811023622046335, 0.09757992244046803654 ) ) ;
#21687 = CARTESIAN_POINT ( 'NONE',  ( -0.3871391076115476282, -0.05778040916215522460, 0.4822834645669289988 ) ) ;
#21688 = CARTESIAN_POINT ( 'NONE',  ( 0.1181102362204730916, -0.6692913385826771977, 8.415575281601705876E-17 ) ) ;
#21689 = CARTESIAN_POINT ( 'NONE',  ( -1.515748031496062076, 0.07958543189024071263, -0.2665933059059888421 ) ) ;
#21690 = CARTESIAN_POINT ( 'NONE',  ( 0.3460692066303959202, -0.1998031496062991630, -1.756561679790026309 ) ) ;
#21691 = CARTESIAN_POINT ( 'NONE',  ( -1.358267716535432434, 0.1660481256975883668, -0.3530559997133364547 ) ) ;
#21692 = CARTESIAN_POINT ( 'NONE',  ( 0.3083989501312343062, -0.05778040916215560624, -0.4822834645669293319 ) ) ;
#21693 = CARTESIAN_POINT ( 'NONE',  ( -0.06561679790026180015, 0.05413385826771666132, 0.4176697321401328100 ) ) ;
#21694 = CARTESIAN_POINT ( 'NONE',  ( 1.036745406824147508, -0.4281496062992127816, -0.4176697321401328100 ) ) ;
#21695 = CARTESIAN_POINT ( 'NONE',  ( -0.2925321140481930149, -0.2925321140481933480, -0.9232283464566929387 ) ) ;
#21696 = CARTESIAN_POINT ( 'NONE',  ( -0.2925321140481930704, -0.2925321140481933480, -1.318897637795275690 ) ) ;
#21697 = CARTESIAN_POINT ( 'NONE',  ( 0.3949938075777411073, -0.1058382717557499464, -0.8989501312335956840 ) ) ;
#21698 = CARTESIAN_POINT ( 'NONE',  ( 0.2925321140481932369, 0.2925321140481932369, -2.342519685039369914 ) ) ;
#21699 = CARTESIAN_POINT ( 'NONE',  ( 0.2867679344610366554, 0.2867679344610366554, -0.2874015748031495399 ) ) ;
#21700 = CARTESIAN_POINT ( 'NONE',  ( -0.006561679790025524116, -0.2845877964562159024, 0.3641732283464567677 ) ) ;
#21701 = CARTESIAN_POINT ( 'NONE',  ( -0.3740157480314953431, -0.5400638737290845981, -0.3530559997133363437 ) ) ;
#21702 = CARTESIAN_POINT ( 'NONE',  ( 0.9186351706036751663, -0.6046776061558807314, 0.2411417322834647770 ) ) ;
#21703 = CARTESIAN_POINT ( 'NONE',  ( 0.3420746716998660508, 0.1974969037888705814, -1.625328083989501460 ) ) ;
#21704 = CARTESIAN_POINT ( 'NONE',  ( 0.1509186351706045259, -0.08942795157528024563, -0.3641732283464568787 ) ) ;
#21705 = CARTESIAN_POINT ( 'NONE',  ( -1.286089238845143479, 0.2306618581243847221, -0.2411417322834647770 ) ) ;
#21706 = CARTESIAN_POINT ( 'NONE',  ( 1.528871391076116026, -0.6692913385826773087, -0.1292274648535924053 ) ) ;
#21707 = CARTESIAN_POINT ( 'NONE',  ( 0.4724409448818897572, -0.1265901696524988906, -1.843832020997375309 ) ) ;
#21708 = CARTESIAN_POINT ( 'NONE',  ( 0.2898214735618554472, 0.2643935821217320292, -2.755905511811024944 ) ) ;
#21709 = VERTEX_POINT ( 'NONE', #17920 ) ;
#21710 = ORIENTED_EDGE ( 'NONE', *, *, #23233, .T. ) ;
#21711 = CARTESIAN_POINT ( 'NONE',  ( 1.122047244094488860, 0.1660481256975885056, 0.3530559997133364547 ) ) ;
#21712 = CARTESIAN_POINT ( 'NONE',  ( 1.502624671916010790, -0.2845877964562161244, -0.3641732283464567121 ) ) ;
#21714 = CARTESIAN_POINT ( 'NONE',  ( -0.9776902887139098386, 0.2952755905511810774, -0.1292274648535930714 ) ) ;
#21713 = CARTESIAN_POINT ( 'NONE',  ( -1.043307086614172041, -0.4536011799217367080, 0.2665933059059888421 ) ) ;
#21715 = CARTESIAN_POINT ( 'NONE',  ( -0.1049643490035306742, 0.3917322834645668994, -2.606279896816586117 ) ) ;
#21716 = CARTESIAN_POINT ( 'NONE',  ( -1.603475055217291612, 1.267857067133556281, 0.04573490813648255215 ) ) ;
#21717 = CARTESIAN_POINT ( 'NONE',  ( 1.397637795275591177, 0.1660481256975883668, -0.3530559997133364547 ) ) ;
#21718 = CARTESIAN_POINT ( 'NONE',  ( -1.673228346456691717, 0.1660481256975883668, -0.3530559997133364547 ) ) ;
#21719 = CARTESIAN_POINT ( 'NONE',  ( -0.02624671916010428221, -0.6046776061558807314, 0.2411417322834647770 ) ) ;
#21720 = CARTESIAN_POINT ( 'NONE',  ( -0.3543307086614165824, -0.6692913385826771977, 8.415575281601705876E-17 ) ) ;
#21721 = EDGE_CURVE ( 'NONE', #23879, #34573, #76198, .T. ) ;
#21722 = CARTESIAN_POINT ( 'NONE',  ( -1.279527559055116948, 0.1660481256975883668, -0.3530559997133364547 ) ) ;
#21723 = CARTESIAN_POINT ( 'NONE',  ( 0.1049643490035304522, -0.3917322834645668994, -2.842500369257531023 ) ) ;
#21724 = CARTESIAN_POINT ( 'NONE',  ( 0.5380577427821529035, 0.05413385826771626580, -0.4176697321401330321 ) ) ;
#21725 = CARTESIAN_POINT ( 'NONE',  ( 0.3392501089628018884, -0.1958661417322834220, -1.829396325459317518 ) ) ;
#21726 = CARTESIAN_POINT ( 'NONE',  ( -1.213910761154854745, -0.5511811023622046335, 0.09757992244046803654 ) ) ;
#21727 = ORIENTED_EDGE ( 'NONE', *, *, #31689, .T. ) ;
#21728 = CARTESIAN_POINT ( 'NONE',  ( 0.1974969037888706369, -0.3420746716998659953, -2.454068241469816503 ) ) ;
#21729 = ORIENTED_EDGE ( 'NONE', *, *, #20862, .T. ) ;
#21730 = CARTESIAN_POINT ( 'NONE',  ( 0.1181102362204724532, 0.04921259842519689481, -0.08523872084492506440 ) ) ;
#21731 = CARTESIAN_POINT ( 'NONE',  ( -1.633858267716534529, -0.5400638737290845981, -0.3530559997133363437 ) ) ;
#21732 = CARTESIAN_POINT ( 'NONE',  ( 1.443569553805774897, 0.2306618581243848609, 0.2411417322834645549 ) ) ;
#21733 = CARTESIAN_POINT ( 'NONE',  ( -0.3460692066303958092, -0.1998031496062994683, -0.6824146981627295938 ) ) ;
#21734 = CARTESIAN_POINT ( 'NONE',  ( -1.502624671916009680, -0.05778040916215560624, -0.4822834645669293319 ) ) ;
#21735 = CARTESIAN_POINT ( 'NONE',  ( -1.515748031496062076, 0.1660481256975883668, -0.3530559997133364547 ) ) ;
#21736 = CARTESIAN_POINT ( 'NONE',  ( -0.03443470937339728616, 0.2755905511811023723, -1.537015892239756099 ) ) ;
#21737 = DIRECTION ( 'NONE',  ( -0.000000000000000000, -1.000000000000000000, -0.000000000000000000 ) ) ;
#21738 = CARTESIAN_POINT ( 'NONE',  ( -0.1049643490035302024, -0.3917322834645671215, 0.1581364829396324501 ) ) ;
#21739 = CARTESIAN_POINT ( 'NONE',  ( -0.3740157480314953431, 0.07958543189024085140, 0.2665933059059887866 ) ) ;
#21740 = CARTESIAN_POINT ( 'NONE',  ( -0.8727034120734901146, -0.08942795157528024563, -0.3641732283464568787 ) ) ;
#21741 = CARTESIAN_POINT ( 'NONE',  ( -1.187664041994749731, -0.3162353388693405765, 0.4822834645669290543 ) ) ;
#21742 = CARTESIAN_POINT ( 'NONE',  ( 0.9317585301837276734, -0.4281496062992124485, 0.4176697321401328655 ) ) ;
#21743 = CARTESIAN_POINT ( 'NONE',  ( -0.9645669291338575535, 0.1660481256975883668, -0.3530559997133364547 ) ) ;
#21744 = CARTESIAN_POINT ( 'NONE',  ( 4.797336870675656522E-17, -0.3917322834645670104, 0.08661417322834649712 ) ) ;
#21745 = VERTEX_POINT ( 'NONE', #61700 ) ;
#21746 = CARTESIAN_POINT ( 'NONE',  ( -1.371391076115484609, -0.6692913385826771977, 0.1292274648535927661 ) ) ;
#21747 = CARTESIAN_POINT ( 'NONE',  ( -1.358267716535432434, 0.07958543189024071263, -0.2665933059059888421 ) ) ;
#21748 = CARTESIAN_POINT ( 'NONE',  ( -0.02462164107398554652, 1.075056246094946211, 0.2372787660107268937 ) ) ;
#21749 = CARTESIAN_POINT ( 'NONE',  ( -1.157146581871515012E-16, 0.4724409448818898682, -1.102362204724409489 ) ) ;
#21750 = CARTESIAN_POINT ( 'NONE',  ( 1.867828664896292956, 1.081851677178494286, -0.1334749385307716363 ) ) ;
#21751 = ADVANCED_FACE ( 'NONE', ( #55368 ), #49057, .T. ) ;
#21752 = CARTESIAN_POINT ( 'NONE',  ( 0.1049643490035304938, -0.3917322834645669549, -0.5498687664041993495 ) ) ;
#21753 = CARTESIAN_POINT ( 'NONE',  ( 0.2867679344610366554, -0.2867679344610365444, -2.230314960629921295 ) ) ;
#21754 = CARTESIAN_POINT ( 'NONE',  ( -0.1771653543307080136, 0.1660481256975883668, -0.3530559997133364547 ) ) ;
#21755 = CARTESIAN_POINT ( 'NONE',  ( 1.607611548556431069, -0.6692913385826773087, -0.1292274648535924053 ) ) ;
#21756 = CARTESIAN_POINT ( 'NONE',  ( 0.3460692066303959202, -0.1998031496062991630, -0.1817585301837270351 ) ) ;
#21758 = CARTESIAN_POINT ( 'NONE',  ( -0.6430446194225712953, 0.009842519685039147898, -0.3409548833797004797 ) ) ;
#21757 = CARTESIAN_POINT ( 'NONE',  ( -1.555118110236219930, 0.1660481256975885056, 0.3530559997133364547 ) ) ;
#21759 = CARTESIAN_POINT ( 'NONE',  ( -1.581364829396324945, -0.3162353388693405765, 0.4822834645669290543 ) ) ;
#21760 = CARTESIAN_POINT ( 'NONE',  ( -0.4330708661417315697, 0.2952755905511811885, 0.000000000000000000 ) ) ;
#21761 = CARTESIAN_POINT ( 'NONE',  ( -0.1049643490035301746, -0.3917322834645670659, 0.1627489745744900018 ) ) ;
#21762 = CARTESIAN_POINT ( 'NONE',  ( 0.5577427821522314977, -0.2845877964562161244, -0.3641732283464567121 ) ) ;
#21763 = CARTESIAN_POINT ( 'NONE',  ( 0.3392501089628018884, -0.1958661417322834220, -0.03215223097112869521 ) ) ;
#21764 = CARTESIAN_POINT ( 'NONE',  ( 0.2165354330708668673, -0.4536011799217367080, 0.2665933059059888421 ) ) ;
#21765 = CARTESIAN_POINT ( 'NONE',  ( 1.069553805774278610, -0.5511811023622046335, 0.09757992244046803654 ) ) ;
#21766 = CARTESIAN_POINT ( 'NONE',  ( 1.082677165354331228, -0.5400638737290844871, 0.3530559997133364547 ) ) ;
#21767 = CIRCLE ( 'NONE', #39239, 3.937007874015748143 ) ;
#21768 = CARTESIAN_POINT ( 'NONE',  ( -0.3215223097112853146, -0.08942795157528024563, -0.3641732283464568787 ) ) ;
#21769 = CARTESIAN_POINT ( 'NONE',  ( 4.797336870675656522E-17, -0.3917322834645670104, -2.118110236220472675 ) ) ;
#21770 = CARTESIAN_POINT ( 'NONE',  ( -1.364829396325458521, -0.6046776061558807314, 0.2411417322834647770 ) ) ;
#21771 = CARTESIAN_POINT ( 'NONE',  ( -0.1312335958005241554, 0.1283753931104748280, 0.1820866141732283561 ) ) ;
#21772 = CARTESIAN_POINT ( 'NONE',  ( -1.135170603674539924, 0.1771653543307087075, -0.09757992244046823083 ) ) ;
#21773 = CARTESIAN_POINT ( 'NONE',  ( -0.1265901696524986964, -0.4724409448818899238, -0.3064304461942257141 ) ) ;
#21774 = CARTESIAN_POINT ( 'NONE',  ( -1.076115485564303809, -0.5023911411419708095, -0.1820866141732282451 ) ) ;
#21775 = CARTESIAN_POINT ( 'NONE',  ( 8.195543980992789655E-16, -0.1870078740157480879, -0.4822834645669291653 ) ) ;
#21776 = CARTESIAN_POINT ( 'NONE',  ( 1.660104986876641320, -0.08942795157527998196, 0.3641732283464567121 ) ) ;
#21777 = CARTESIAN_POINT ( 'NONE',  ( 0.6167979002624678353, -0.3690944881889763329, 0.3153832671262228327 ) ) ;
#21778 = CARTESIAN_POINT ( 'NONE',  ( -0.1049868766404193215, 0.1283753931104746893, -0.1820866141732285504 ) ) ;
#21779 = CARTESIAN_POINT ( 'NONE',  ( -0.6692913385826764205, 0.2952755905511811885, 0.000000000000000000 ) ) ;
#21780 = CARTESIAN_POINT ( 'NONE',  ( -1.640419947506561060, -0.4281496062992127816, -0.4176697321401328100 ) ) ;
#21781 = CARTESIAN_POINT ( 'NONE',  ( -1.135170603674539924, 0.1771653543307087075, -0.09757992244046823083 ) ) ;
#21782 = CARTESIAN_POINT ( 'NONE',  ( 0.6889763779527560139, 0.000000000000000000, 0.000000000000000000 ) ) ;
#21783 = CARTESIAN_POINT ( 'NONE',  ( 0.5643044619422579178, 0.05413385826771666132, 0.4176697321401328100 ) ) ;
#21784 = VERTEX_POINT ( 'NONE', #31345 ) ;
#21785 = CARTESIAN_POINT ( 'NONE',  ( -0.3996062992125985480, -7.340648628747423112E-17, -1.690944881889763884 ) ) ;
#21786 = CARTESIAN_POINT ( 'NONE',  ( -0.3083989501312330295, -0.08942795157527998196, 0.3641732283464567121 ) ) ;
#21787 = CARTESIAN_POINT ( 'NONE',  ( -0.08530183727034056085, -0.05778040916215560624, -0.4822834645669293319 ) ) ;
#21788 = CARTESIAN_POINT ( 'NONE',  ( -1.640419947506561060, 0.05413385826771666132, 0.4176697321401328100 ) ) ;
#21789 = CARTESIAN_POINT ( 'NONE',  ( -1.502624671916009680, -0.2845877964562159024, 0.3641732283464567677 ) ) ;
#21790 = CARTESIAN_POINT ( 'NONE',  ( 1.515748031496063408, 0.1660481256975885056, 0.3530559997133364547 ) ) ;
#21791 = CARTESIAN_POINT ( 'NONE',  ( -0.7808398950131225646, -0.08942795157527998196, 0.3641732283464567121 ) ) ;
#21792 = CARTESIAN_POINT ( 'NONE',  ( -1.092023077763013772, -4.378520898609941727E-15, 0.4281989832122466977 ) ) ;
#21793 = CARTESIAN_POINT ( 'NONE',  ( -9.787531504996567848E-17, 0.3996062992125986035, -0.1574803149606299191 ) ) ;
#21794 = CARTESIAN_POINT ( 'NONE',  ( -0.3392501089628017219, -0.1958661417322836995, -2.411436638616484718 ) ) ;
#21795 = CARTESIAN_POINT ( 'NONE',  ( -3.900966923095589678, 2.677165354330708791, -0.5314960629921260393 ) ) ;
#21796 = CARTESIAN_POINT ( 'NONE',  ( 0.9514435695538062676, -0.08942795157527998196, 0.3641732283464567121 ) ) ;
#21797 = CARTESIAN_POINT ( 'NONE',  ( -0.4724409448818898682, -8.678599364036362592E-17, -2.086614173228346303 ) ) ;
#21798 = CARTESIAN_POINT ( 'NONE',  ( 0.8398950131233602345, 0.2306618581243847221, -0.2411417322834647770 ) ) ;
#21799 = CARTESIAN_POINT ( 'NONE',  ( -0.1049643490035302024, -0.3917322834645671215, -2.361548556430446144 ) ) ;
#21800 = CARTESIAN_POINT ( 'NONE',  ( 1.358267716535433323, 0.07958543189024085140, 0.2665933059059887866 ) ) ;
#21801 =( BOUNDED_CURVE ( )  B_SPLINE_CURVE ( 2, ( #51573, #6146, #51160, #12063, #70535, #64645, #65068, #76040, #50343, #44026, #50755, #57066, #58317 ),
 .UNSPECIFIED., .F., .F. ) 
 B_SPLINE_CURVE_WITH_KNOTS ( ( 3, 2, 2, 2, 2, 2, 3 ),
 ( 0.06250000000000000000, 0.06666666666666666574, 0.07083333333333333148, 0.07500000000000001110, 0.07916666666666666297, 0.08333333333333334259, 0.08750000000000000833 ),
 .UNSPECIFIED. ) 
 CURVE ( )  GEOMETRIC_REPRESENTATION_ITEM ( )  RATIONAL_B_SPLINE_CURVE ( ( 1.000000000000000000, 0.9659258262890683122, 1.000000000000000000, 0.9659258262890683122, 1.000000000000000000, 0.9659258262890683122, 1.000000000000000000, 0.9659258262890683122, 1.000000000000000000, 0.9659258262890683122, 1.000000000000000000, 0.9659258262890682012, 1.000000000000000222 ) ) 
 REPRESENTATION_ITEM ( '' )  );
#21802 = CARTESIAN_POINT ( 'NONE',  ( 0.1968503937007881344, -0.6692913385826771977, 8.415575281601705876E-17 ) ) ;
#21803 = CARTESIAN_POINT ( 'NONE',  ( -0.3280839895013117347, 0.05413385826771626580, -0.4176697321401330321 ) ) ;
#21804 = CARTESIAN_POINT ( 'NONE',  ( 1.568241469816273659, -0.05778040916215560624, -0.4822834645669293319 ) ) ;
#21805 = CARTESIAN_POINT ( 'NONE',  ( -0.4091458600556405756, 0.2362204724409446288, -0.8136482939632546652 ) ) ;
#21806 = CARTESIAN_POINT ( 'NONE',  ( 0.1070741851644054915, -0.3996062992125985480, -1.975065616797900159 ) ) ;
#21807 = CARTESIAN_POINT ( 'NONE',  ( 0.1706036745406830368, -0.004921259842519576551, 0.3153832671262227771 ) ) ;
#21808 = ORIENTED_EDGE ( 'NONE', *, *, #73302, .F. ) ;
#21809 = CARTESIAN_POINT ( 'NONE',  ( -0.1958661417322836995, 0.3392501089628017219, -0.1673421504275084681 ) ) ;
#21810 = ORIENTED_EDGE ( 'NONE', *, *, #29128, .F. ) ;
#21811 = CARTESIAN_POINT ( 'NONE',  ( -0.5971128608923877978, 0.2952755905511811885, 0.1292274648535926551 ) ) ;
#21812 = CARTESIAN_POINT ( 'NONE',  ( 1.489501312335958172, -0.05778040916215560624, -0.4822834645669293319 ) ) ;
#21813 = CARTESIAN_POINT ( 'NONE',  ( 0.04593175853018440641, -0.6692913385826771977, 0.1292274648535927661 ) ) ;
#21814 = CARTESIAN_POINT ( 'NONE',  ( -0.2296587926509179312, -0.08942795157527998196, 0.3641732283464567121 ) ) ;
#21815 = CARTESIAN_POINT ( 'NONE',  ( 0.7283464566929143125, 0.1660481256975885056, 0.3530559997133364547 ) ) ;
#21816 = CARTESIAN_POINT ( 'NONE',  ( -0.7611548556430438595, -0.6046776061558809534, -0.2411417322834644161 ) ) ;
#21817 = EDGE_CURVE ( 'NONE', #23246, #24385, #60234, .T. ) ;
#21818 = CARTESIAN_POINT ( 'NONE',  ( -0.4658792650918627265, -0.05778040916215522460, 0.4822834645669289988 ) ) ;
#21819 = CARTESIAN_POINT ( 'NONE',  ( -0.9383202099737524282, -0.05778040916215522460, 0.4822834645669289988 ) ) ;
#21820 = CARTESIAN_POINT ( 'NONE',  ( 1.161417322834646271, 0.1660481256975883668, -0.3530559997133364547 ) ) ;
#21821 = CIRCLE ( 'NONE', #28552, 2.362204724409449064 ) ;
#21822 = CARTESIAN_POINT ( 'NONE',  ( 0.8202099737532813073, 0.2952755905511811885, 0.1292274648535926551 ) ) ;
#21823 = CARTESIAN_POINT ( 'NONE',  ( 0.8923884514435703741, 0.2306618581243848609, 0.2411417322834645549 ) ) ;
#21824 = CARTESIAN_POINT ( 'NONE',  ( -0.1049643490035307020, 0.3917322834645669549, -0.4711286089238844177 ) ) ;
#21825 = CARTESIAN_POINT ( 'NONE',  ( 0.1706036745406830368, -0.3690944881889765550, -0.3153832671262227771 ) ) ;
#21826 = ORIENTED_EDGE ( 'NONE', *, *, #65042, .T. ) ;
#21827 = CARTESIAN_POINT ( 'NONE',  ( 4.837279021331060870E-17, -0.3949938075777409963, -1.181102362204724532 ) ) ;
#21828 = VERTEX_POINT ( 'NONE', #77220 ) ;
#21829 = CARTESIAN_POINT ( 'NONE',  ( -0.9908136482939626788, -0.5511811023622048555, -0.09757992244046775898 ) ) ;
#21830 = CARTESIAN_POINT ( 'NONE',  ( -0.2362204724409440182, -0.1870078740157479769, 0.4822834645669291653 ) ) ;
#21831 = DIRECTION ( 'NONE',  ( 0.7071067811865495711, -0.000000000000000000, -0.7071067811865454633 ) ) ;
#21832 = CARTESIAN_POINT ( 'NONE',  ( -0.4265091863517051496, 0.2952755905511810774, -0.1292274648535930714 ) ) ;
#21833 = CARTESIAN_POINT ( 'NONE',  ( -0.5774278215223089816, 0.2306618581243847221, -0.2411417322834647770 ) ) ;
#21834 = CARTESIAN_POINT ( 'NONE',  ( -1.200787401574802349, -0.5400638737290844871, 0.3530559997133364547 ) ) ;
#21835 = CARTESIAN_POINT ( 'NONE',  ( -1.325459317585300889, -0.4281496062992127816, -0.4176697321401328100 ) ) ;
#21836 = CARTESIAN_POINT ( 'NONE',  ( 1.227034120734908917, 0.1771653543307087075, -0.09757992244046823083 ) ) ;
#21837 = CARTESIAN_POINT ( 'NONE',  ( 0.4091458600556404646, -0.2362204724409448231, -1.049868766404199460 ) ) ;
#21838 = CARTESIAN_POINT ( 'NONE',  ( 0.2430399508222474414, 0.1677739497468299368, 5.760042173782278674 ) ) ;
#21839 = CARTESIAN_POINT ( 'NONE',  ( 0.5971128608923890191, -0.5511811023622046335, 0.09757992244046803654 ) ) ;
#21840 = CARTESIAN_POINT ( 'NONE',  ( 0.1771653543307093182, -0.5400638737290845981, -0.3530559997133363437 ) ) ;
#21841 = CARTESIAN_POINT ( 'NONE',  ( 0.2887139107611556010, 0.2306618581243847221, -0.2411417322834647770 ) ) ;
#21842 = VERTEX_POINT ( 'NONE', #25027 ) ;
#21843 = CARTESIAN_POINT ( 'NONE',  ( -0.2925321140481932924, 0.2925321140481931814, -1.594488188976378229 ) ) ;
#21844 = CARTESIAN_POINT ( 'NONE',  ( 0.1341536278048623965, 1.050682278017460725, 0.2827841492639507348 ) ) ;
#21845 = EDGE_LOOP ( 'NONE', ( #57298, #22467, #76075, #8485 ) ) ;
#21846 = CARTESIAN_POINT ( 'NONE',  ( 0.3996062992125986035, -0.1070741851644052972, -1.290682414698162583 ) ) ;
#21847 = CARTESIAN_POINT ( 'NONE',  ( 0.1070741851644053388, 0.3996062992125986035, -0.5426509186351704539 ) ) ;
#21848 = CARTESIAN_POINT ( 'NONE',  ( -0.3608923884514428360, -0.6692913385826773087, -0.1292274648535924053 ) ) ;
#21849 = CARTESIAN_POINT ( 'NONE',  ( 0.4091458600556403535, 0.2362204724409449896, 0.02624671916010498651 ) ) ;
#21850 = CARTESIAN_POINT ( 'NONE',  ( -0.1049643490035307020, 0.3917322834645669549, -2.453412073490813139 ) ) ;
#21851 = CARTESIAN_POINT ( 'NONE',  ( -1.528871391076114250, -0.5511811023622046335, 0.09757992244046803654 ) ) ;
#21852 = CARTESIAN_POINT ( 'NONE',  ( 0.9514435695538062676, -0.05778040916215522460, 0.4822834645669289988 ) ) ;
#21853 = CARTESIAN_POINT ( 'NONE',  ( 0.9973753280839902091, -0.6046776061558807314, 0.2411417322834647770 ) ) ;
#21854 = CARTESIAN_POINT ( 'NONE',  ( -0.2493438320209966919, -0.3690944881889763329, 0.3153832671262228327 ) ) ;
#21855 = CARTESIAN_POINT ( 'NONE',  ( 0.02624671916010564918, 0.2306618581243848609, 0.2411417322834645549 ) ) ;
#21856 = CARTESIAN_POINT ( 'NONE',  ( -0.1265901696524993347, 0.4724409448818895907, -1.815616797900262425 ) ) ;
#21857 = CARTESIAN_POINT ( 'NONE',  ( -0.08530183727034056085, -0.2845877964562159024, 0.3641732283464567677 ) ) ;
#21858 = CARTESIAN_POINT ( 'NONE',  ( -0.4790026246719154557, -0.3162353388693405765, 0.4822834645669290543 ) ) ;
#21859 = CARTESIAN_POINT ( 'NONE',  ( 0.3949938075777409408, -0.1058382717557499186, -1.763123359580052396 ) ) ;
#21860 = CARTESIAN_POINT ( 'NONE',  ( -1.469816272965878357, -0.6046776061558809534, -0.2411417322834644161 ) ) ;
#21861 = CARTESIAN_POINT ( 'NONE',  ( 0.1771653543307093182, 0.07958543189024085140, 0.2665933059059887866 ) ) ;
#21862 = CARTESIAN_POINT ( 'NONE',  ( 1.653543307086614789, -0.1870078740157479769, 0.3641732283464567677 ) ) ;
#21863 = CARTESIAN_POINT ( 'NONE',  ( -0.9448818897637790704, -0.1870078740157479769, 0.4822834645669291653 ) ) ;
#21864 = CARTESIAN_POINT ( 'NONE',  ( -0.8661417322834640276, -0.1870078740157479769, 0.3641732283464567677 ) ) ;
#21865 = CARTESIAN_POINT ( 'NONE',  ( -1.646051170424378096, -0.1870078740157480046, 1.254653134982923898E-17 ) ) ;
#21866 = CARTESIAN_POINT ( 'NONE',  ( -1.128608923884513837, -0.6046776061558807314, 0.2411417322834647770 ) ) ;
#21867 = CARTESIAN_POINT ( 'NONE',  ( -0.6496062992125976043, 0.1660481256975883668, -0.3530559997133364547 ) ) ;
#21868 = CARTESIAN_POINT ( 'NONE',  ( 0.1837270341207357105, -0.6046776061558809534, -0.2411417322834644161 ) ) ;
#21869 = CARTESIAN_POINT ( 'NONE',  ( -0.1070741851644056997, 0.3996062992125984925, -2.603018372703412631 ) ) ;
#21870 = CARTESIAN_POINT ( 'NONE',  ( -0.1049643490035306742, 0.3917322834645668994, -2.448799581855955587 ) ) ;
#21871 = CARTESIAN_POINT ( 'NONE',  ( 2.362204724409448620, 0.000000000000000000, 8.247593713802677664E-15 ) ) ;
#21872 = CARTESIAN_POINT ( 'NONE',  ( 0.3215223097112867578, -0.2845877964562161244, -0.3641732283464567121 ) ) ;
#21873 = CARTESIAN_POINT ( 'NONE',  ( 0.9383202099737536495, -0.3162353388693405765, 0.4822834645669290543 ) ) ;
#21874 = CARTESIAN_POINT ( 'NONE',  ( -1.266404199475064773, -0.2845877964562159024, 0.3641732283464567677 ) ) ;
#21875 = EDGE_CURVE ( 'NONE', #7209, #47808, #46707, .T. ) ;
#21876 = CARTESIAN_POINT ( 'NONE',  ( 1.213910761154856299, 0.2952755905511811885, 0.1292274648535926551 ) ) ;
#21877 = CARTESIAN_POINT ( 'NONE',  ( -1.653543307086613234, -0.1870078740157480601, -0.3641732283464567677 ) ) ;
#21878 = AXIS2_PLACEMENT_3D ( 'NONE', #51328, #34919, #9658 ) ;
#21879 = CARTESIAN_POINT ( 'NONE',  ( -0.4396325459317579898, 0.2952755905511811885, 0.1292274648535926551 ) ) ;
#21880 = CARTESIAN_POINT ( 'NONE',  ( 0.3083989501312343062, -0.08942795157528024563, -0.3641732283464568787 ) ) ;
#21881 = CARTESIAN_POINT ( 'NONE',  ( -0.3458507752293906723, -0.3458507752293910609, -0.8464566929133857665 ) ) ;
#21882 = CARTESIAN_POINT ( 'NONE',  ( 0.7677165354330716118, -0.4536011799217367080, 0.2665933059059888421 ) ) ;
#21883 = ADVANCED_FACE ( 'NONE', ( #63752 ), #12836, .F. ) ;
#21884 = CARTESIAN_POINT ( 'NONE',  ( 0.05249343832021075018, -0.6046776061558807314, 0.2411417322834647770 ) ) ;
#21885 = CARTESIAN_POINT ( 'NONE',  ( -0.1998031496062991630, -0.3460692066303959202, -0.4573490813648293796 ) ) ;
#21886 = CARTESIAN_POINT ( 'NONE',  ( -0.8530183727034112984, -0.4281496062992127816, -0.4176697321401328100 ) ) ;
#21887 = CARTESIAN_POINT ( 'NONE',  ( -0.3392501089628019995, 0.1958661417322832277, -1.685695538057742970 ) ) ;
#21888 = CARTESIAN_POINT ( 'NONE',  ( 1.030183727034121421, -0.2845877964562161244, -0.3641732283464567121 ) ) ;
#21889 = CARTESIAN_POINT ( 'NONE',  ( -0.03280839895013062252, 0.2952755905511810774, -0.1292274648535930714 ) ) ;
#21890 = CARTESIAN_POINT ( 'NONE',  ( -0.1706036745406816491, 0.05413385826771626580, -0.4176697321401330321 ) ) ;
#21891 = CARTESIAN_POINT ( 'NONE',  ( -0.2821522309711278487, -0.5511811023622048555, -0.09757992244046775898 ) ) ;
#21892 = FACE_OUTER_BOUND ( 'NONE', #58336, .T. ) ;
#21893 = CARTESIAN_POINT ( 'NONE',  ( -0.6102362204724400829, -0.4536011799217368745, -0.2665933059059886201 ) ) ;
#21894 = CARTESIAN_POINT ( 'NONE',  ( 0.3871391076115493490, -0.3162353388693405765, 0.4822834645669290543 ) ) ;
#21895 = CARTESIAN_POINT ( 'NONE',  ( -0.5774278215223089816, 0.1283753931104746893, -0.1820866141732285504 ) ) ;
#21896 = CARTESIAN_POINT ( 'NONE',  ( -0.3460692066303957537, -0.1998031496062994405, -0.9166666666666666297 ) ) ;
#21897 = CARTESIAN_POINT ( 'NONE',  ( -1.207349081364828436, -0.6046776061558807314, 0.2411417322834647770 ) ) ;
#21898 = LINE ( 'NONE', #2133, #42058 ) ;
#21899 = VERTEX_POINT ( 'NONE', #19549 ) ;
#21900 = CARTESIAN_POINT ( 'NONE',  ( -1.148293963254592542, -0.5511811023622048555, -0.09757992244046775898 ) ) ;
#21901 = CARTESIAN_POINT ( 'NONE',  ( -0.01312335958005186876, -0.4281496062992124485, 0.4176697321401328655 ) ) ;
#21902 = B_SPLINE_CURVE_WITH_KNOTS ( 'NONE', 3,
 ( #30391, #18600, #3908, #69932 ),
 .UNSPECIFIED., .F., .F.,
 ( 4, 4 ),
 ( 0.1795298335526529787, 0.1809577925700027734 ),
 .UNSPECIFIED. ) ;
#21903 = EDGE_CURVE ( 'NONE', #199, #35363, #5967, .T. ) ;
#21904 = CARTESIAN_POINT ( 'NONE',  ( -1.482939632545930975, -0.4281496062992127816, -0.4176697321401328100 ) ) ;
#21905 = CARTESIAN_POINT ( 'NONE',  ( -0.8136482939632537770, 0.2306618581243847221, -0.2411417322834647770 ) ) ;
#21906 = CARTESIAN_POINT ( 'NONE',  ( 0.1265901696524990572, -0.4724409448818897017, -2.132545931758530244 ) ) ;
#21907 = CARTESIAN_POINT ( 'NONE',  ( 1.404199475065617708, 0.05413385826771626580, -0.4176697321401330321 ) ) ;
#21908 = CARTESIAN_POINT ( 'NONE',  ( 0.8530183727034128527, -0.4281496062992124485, 0.4176697321401328655 ) ) ;
#21909 = DIRECTION ( 'NONE',  ( -1.000000000000000000, 0.000000000000000000, -1.047444401652940480E-14 ) ) ;
#21910 = DIRECTION ( 'NONE',  ( 1.734723475976807489E-15, 0.000000000000000000, -1.000000000000000000 ) ) ;
#21911 = CARTESIAN_POINT ( 'NONE',  ( 0.2597599741900292747, -0.1405915162213216552, 5.593567858643828217 ) ) ;
#21912 = CARTESIAN_POINT ( 'NONE',  ( -1.653543307086613234, -0.1870078740157480879, -0.4822834645669291653 ) ) ;
#21913 = CARTESIAN_POINT ( 'NONE',  ( -0.2925321140481932924, 0.2925321140481931814, -0.3346456692913385988 ) ) ;
#21915 = EDGE_CURVE ( 'NONE', #37974, #57515, #34926, .T. ) ;
#21914 = ORIENTED_EDGE ( 'NONE', *, *, #10296, .T. ) ;
#21916 = CARTESIAN_POINT ( 'NONE',  ( -0.5905511811023613777, -0.5511811023622047445, 6.969142054262312111E-17 ) ) ;
#21917 = CARTESIAN_POINT ( 'NONE',  ( 4.797336870675656522E-17, -0.3917322834645670104, -2.275590551181102317 ) ) ;
#21918 = ORIENTED_EDGE ( 'NONE', *, *, #15090, .T. ) ;
#21919 = CARTESIAN_POINT ( 'NONE',  ( 1.003937007874016185, 0.1660481256975883668, -0.3530559997133364547 ) ) ;
#21920 = CARTESIAN_POINT ( 'NONE',  ( 0.2034120734908142214, 0.2952755905511810774, -0.1292274648535930714 ) ) ;
#21921 = CARTESIAN_POINT ( 'NONE',  ( -0.5052493438320203589, 0.2952755905511810774, -0.1292274648535930714 ) ) ;
#21922 = CARTESIAN_POINT ( 'NONE',  ( 1.522309711286089939, 0.2306618581243848609, 0.2411417322834645549 ) ) ;
#21923 = VECTOR ( 'NONE', #34936, 39.37007874015748143 ) ;
#21924 = CARTESIAN_POINT ( 'NONE',  ( -1.482939632545930975, -0.004921259842519576551, 0.3153832671262227771 ) ) ;
#21925 = CARTESIAN_POINT ( 'NONE',  ( 0.01745729623385432541, 1.063258500840309706, -1.453357034165985828 ) ) ;
#21926 = CARTESIAN_POINT ( 'NONE',  ( 0.3740157480314966754, -0.5400638737290844871, 0.3530559997133364547 ) ) ;
#21927 = CARTESIAN_POINT ( 'NONE',  ( 0.7020997375328090762, -0.08942795157528024563, -0.3641732283464568787 ) ) ;
#21928 = CARTESIAN_POINT ( 'NONE',  ( -0.6692913385826764205, 0.2952755905511811885, 0.000000000000000000 ) ) ;
#21929 = CARTESIAN_POINT ( 'NONE',  ( -0.3392501089628018329, -0.1958661417322836440, -1.549849450622360791 ) ) ;
#21930 = CARTESIAN_POINT ( 'NONE',  ( -1.148293963254592542, 0.2952755905511811885, 0.1292274648535926551 ) ) ;
#21931 = CARTESIAN_POINT ( 'NONE',  ( -1.673228346456691717, 0.07958543189024071263, -0.2665933059059888421 ) ) ;
#21932 = EDGE_CURVE ( 'NONE', #32199, #23562, #55165, .T. ) ;
#21933 = CARTESIAN_POINT ( 'NONE',  ( 0.9842519685039378130, -0.6692913385826771977, 8.415575281601705876E-17 ) ) ;
#21934 = CARTESIAN_POINT ( 'NONE',  ( 1.371391076115485941, 0.1771653543307087630, 0.09757992244046791164 ) ) ;
#21935 = ORIENTED_EDGE ( 'NONE', *, *, #55786, .T. ) ;
#21936 = CARTESIAN_POINT ( 'NONE',  ( -0.2867679344610367109, 0.2867679344610365444, -2.851069184548242763 ) ) ;
#21937 = CARTESIAN_POINT ( 'NONE',  ( -0.5511811023622038563, -0.1870078740157479769, 0.4822834645669291653 ) ) ;
#21938 = ORIENTED_EDGE ( 'NONE', *, *, #45519, .T. ) ;
#21939 = CARTESIAN_POINT ( 'NONE',  ( 0.2887139107611556010, -0.5023911411419708095, 0.1820866141732285504 ) ) ;
#21940 = CARTESIAN_POINT ( 'NONE',  ( -1.049868766404198794, 0.2306618581243847221, -0.2411417322834647770 ) ) ;
#21941 = CARTESIAN_POINT ( 'NONE',  ( 0.9448818897637802916, -0.1870078740157479769, 0.4822834645669291653 ) ) ;
#21942 = CARTESIAN_POINT ( 'NONE',  ( 1.010498687664042716, 0.05413385826771626580, -0.4176697321401330321 ) ) ;
#21943 = CARTESIAN_POINT ( 'NONE',  ( -0.1049868766404193215, 0.2306618581243847221, -0.2411417322834647770 ) ) ;
#21944 = VECTOR ( 'NONE', #69819, 39.37007874015748143 ) ;
#21945 = CARTESIAN_POINT ( 'NONE',  ( -0.2427821522309703550, -0.3162353388693405765, 0.4822834645669290543 ) ) ;
#21946 = CARTESIAN_POINT ( 'NONE',  ( 0.2867679344610365999, 0.2867679344610365999, -2.269685039370078705 ) ) ;
#21947 = CARTESIAN_POINT ( 'NONE',  ( 1.601049868766404982, 0.1283753931104748280, 0.1820866141732283561 ) ) ;
#21948 = CARTESIAN_POINT ( 'NONE',  ( -0.5774278215223089816, -0.6046776061558807314, 0.2411417322834647770 ) ) ;
#21949 = CARTESIAN_POINT ( 'NONE',  ( -0.4133858267716528645, -0.4536011799217367080, 0.2665933059059888421 ) ) ;
#21950 = CARTESIAN_POINT ( 'NONE',  ( 1.496062992125985147, -0.1870078740157479769, 0.4822834645669291653 ) ) ;
#21951 = CARTESIAN_POINT ( 'NONE',  ( 1.450131233595801428, -0.6692913385826773087, -0.1292274648535924053 ) ) ;
#21952 = CARTESIAN_POINT ( 'NONE',  ( -0.7677165354330699465, 0.1660481256975885056, 0.3530559997133364547 ) ) ;
#21953 = CARTESIAN_POINT ( 'NONE',  ( -0.3996062992125986590, 0.1070741851644051723, 0.2053805774278214813 ) ) ;
#21954 = CARTESIAN_POINT ( 'NONE',  ( 0.7283464566929140904, -0.5400638737290845981, -0.3530559997133363437 ) ) ;
#21955 = CARTESIAN_POINT ( 'NONE',  ( -0.3460692066303960868, 0.1998031496062990242, -1.758530183727034180 ) ) ;
#21956 = CARTESIAN_POINT ( 'NONE',  ( 3.908320185825791881, 1.537401574803149984, 0.4744094488188975722 ) ) ;
#21957 = CARTESIAN_POINT ( 'NONE',  ( -0.3018372703412066094, -0.4281496062992127816, -0.4176697321401328100 ) ) ;
#21958 = CARTESIAN_POINT ( 'NONE',  ( -1.161417322834644716, 0.07958543189024085140, 0.2665933059059887866 ) ) ;
#21959 = CARTESIAN_POINT ( 'NONE',  ( 1.043307086614173818, 0.07958543189024085140, 0.2665933059059887866 ) ) ;
#21960 = CARTESIAN_POINT ( 'NONE',  ( -0.1265901696524993347, 0.4724409448818895907, -0.8707349081364830212 ) ) ;
#21961 = CARTESIAN_POINT ( 'NONE',  ( 1.115485564304462551, -0.3690944881889765550, -0.3153832671262227771 ) ) ;
#21962 = CARTESIAN_POINT ( 'NONE',  ( 0.8530183727034126306, 0.05413385826771626580, -0.4176697321401330321 ) ) ;
#21963 = CARTESIAN_POINT ( 'NONE',  ( 0.3420746716998660508, 0.1974969037888705814, -0.3654855643044619407 ) ) ;
#21964 = CARTESIAN_POINT ( 'NONE',  ( -0.2230971128608915943, -0.4281496062992127816, -0.4176697321401328100 ) ) ;
#21965 = CARTESIAN_POINT ( 'NONE',  ( -0.6299212598425164567, 1.724409448818897905, -0.9285414500055737541 ) ) ;
#21966 = CARTESIAN_POINT ( 'NONE',  ( 1.266404199475066328, -0.08942795157527998196, 0.3641732283464567121 ) ) ;
#21967 = CARTESIAN_POINT ( 'NONE',  ( -0.3871391076115479057, -0.3162353388693409650, -0.4822834645669289433 ) ) ;
#21968 = CARTESIAN_POINT ( 'NONE',  ( 0.3420746716998660508, 0.1974969037888705814, -0.5229658792650918597 ) ) ;
#21969 = CARTESIAN_POINT ( 'NONE',  ( 1.437007874015748810, -0.5400638737290845981, -0.3530559997133363437 ) ) ;
#21970 = CARTESIAN_POINT ( 'NONE',  ( 0.1049868766404206816, -0.6046776061558809534, -0.2411417322834644161 ) ) ;
#21971 = CARTESIAN_POINT ( 'NONE',  ( 0.4265091863517067594, 0.1771653543307087630, 0.09757992244046791164 ) ) ;
#21972 = CARTESIAN_POINT ( 'NONE',  ( -0.4091458600556402980, -0.2362204724409451284, -0.1292650918635170620 ) ) ;
#21973 = CARTESIAN_POINT ( 'NONE',  ( 0.3608923884514443348, -0.5511811023622046335, 0.09757992244046803654 ) ) ;
#21974 = CARTESIAN_POINT ( 'NONE',  ( -1.541994750656167090, -0.6692913385826773087, -0.1292274648535924053 ) ) ;
#21975 = CARTESIAN_POINT ( 'NONE',  ( 0.3460692066303958092, 0.1998031496062993018, -1.467847769028871596 ) ) ;
#21976 = CARTESIAN_POINT ( 'NONE',  ( 0.8070866141732289112, -0.5400638737290845981, -0.3530559997133363437 ) ) ;
#21977 = CARTESIAN_POINT ( 'NONE',  ( 0.1049643490035304938, -0.3917322834645669549, -1.022309711286088829 ) ) ;
#21978 = CARTESIAN_POINT ( 'NONE',  ( 1.574803149606299746, -0.1870078740157480601, -0.3641732283464567677 ) ) ;
#21979 = CARTESIAN_POINT ( 'NONE',  ( -0.3910482532979368542, -0.02544847934398145398, -4.648478490738263808E-18 ) ) ;
#21980 = CARTESIAN_POINT ( 'NONE',  ( 0.01312335958005323398, -0.004921259842519576551, 0.3153832671262227771 ) ) ;
#21981 = ADVANCED_FACE ( 'NONE', ( #45627 ), #51516, .F. ) ;
#21982 = CARTESIAN_POINT ( 'NONE',  ( 0.1246719160104994284, 0.2952755905511810774, -0.1292274648535930714 ) ) ;
#21983 = CARTESIAN_POINT ( 'NONE',  ( 1.528871391076116026, 0.1771653543307087630, 0.09757992244046791164 ) ) ;
#21984 = CARTESIAN_POINT ( 'NONE',  ( -1.345144356955379816, -0.08942795157528024563, -0.3641732283464568787 ) ) ;
#21985 = CARTESIAN_POINT ( 'NONE',  ( -1.646981627296586703, -0.3162353388693409650, -0.4822834645669289433 ) ) ;
#21986 = VECTOR ( 'NONE', #60087, 39.37007874015748143 ) ;
#21987 = CARTESIAN_POINT ( 'NONE',  ( 0.5643044619422579178, 0.05413385826771666132, 0.4176697321401328100 ) ) ;
#21988 = CARTESIAN_POINT ( 'NONE',  ( -1.620734908136482577, 0.1771653543307087630, 0.09757992244046791164 ) ) ;
#21989 = CARTESIAN_POINT ( 'NONE',  ( 1.586052503253845281, 1.299212598425198095, -0.1653254495020587411 ) ) ;
#21990 = CARTESIAN_POINT ( 'NONE',  ( 0.7283464566929140904, -0.5400638737290845981, -0.3530559997133363437 ) ) ;
#21991 = CARTESIAN_POINT ( 'NONE',  ( 1.194225721784777594, 0.05413385826771666132, 0.4176697321401328100 ) ) ;
#21992 = CARTESIAN_POINT ( 'NONE',  ( 1.174540682414699111, -0.3162353388693405765, 0.4822834645669290543 ) ) ;
#21993 = DIRECTION ( 'NONE',  ( 0.000000000000000000, 1.000000000000000000, -0.000000000000000000 ) ) ;
#21994 = CARTESIAN_POINT ( 'NONE',  ( 1.115485564304462551, -0.3690944881889765550, -0.3153832671262227771 ) ) ;
#21995 = CARTESIAN_POINT ( 'NONE',  ( -1.568241469816272105, -0.2845877964562161244, -0.3641732283464567121 ) ) ;
#21996 = CARTESIAN_POINT ( 'NONE',  ( -0.7874015748031489847, -0.1870078740157480601, -0.3641732283464567677 ) ) ;
#21997 = CARTESIAN_POINT ( 'NONE',  ( 1.220472440944881942, 1.496062992125984037, -0.5309055118110238558 ) ) ;
#21998 = CARTESIAN_POINT ( 'NONE',  ( 0.6102362204724416372, -0.4536011799217367080, 0.2665933059059888421 ) ) ;
#21999 = CIRCLE ( 'NONE', #75772, 3.543307086614173151 ) ;
#22000 = CARTESIAN_POINT ( 'NONE',  ( 0.2952755905511819101, 0.1660481256975883668, -0.3530559997133364547 ) ) ;
#22001 = CARTESIAN_POINT ( 'NONE',  ( 0.8005249343832027131, 0.05413385826771666132, 0.4176697321401328100 ) ) ;
#22002 = CARTESIAN_POINT ( 'NONE',  ( -0.4527559055118102749, -0.5400638737290845981, -0.3530559997133363437 ) ) ;
#22003 = CARTESIAN_POINT ( 'NONE',  ( 0.1509186351706042484, -0.2845877964562159024, 0.3641732283464567677 ) ) ;
#22004 = CARTESIAN_POINT ( 'NONE',  ( 1.338582677165355062, -0.1870078740157480879, -0.4822834645669291653 ) ) ;
#22005 = CARTESIAN_POINT ( 'NONE',  ( -1.614173228346456712, 2.401574803149606474, -0.1372047244094478091 ) ) ;
#22006 = CARTESIAN_POINT ( 'NONE',  ( -0.9842519685039365918, -0.6692913385826771977, 8.415575281601705876E-17 ) ) ;
#22008 = CARTESIAN_POINT ( 'NONE',  ( -0.3996062992125986035, -7.340648628747425578E-17, -0.8267716535433070613 ) ) ;
#22007 = FACE_OUTER_BOUND ( 'NONE', #19625, .T. ) ;
#22009 = DIRECTION ( 'NONE',  ( -0.000000000000000000, 1.000000000000000000, -0.000000000000000000 ) ) ;
#22010 = CARTESIAN_POINT ( 'NONE',  ( -0.6496062992125976043, 0.1660481256975883668, -0.3530559997133364547 ) ) ;
#22011 = CARTESIAN_POINT ( 'NONE',  ( -0.5839895013123351797, 0.2952755905511810774, -0.1292274648535930714 ) ) ;
#22012 = CARTESIAN_POINT ( 'NONE',  ( -0.3460692066303958092, -0.1998031496062994683, -2.887139107611548461 ) ) ;
#22013 = CARTESIAN_POINT ( 'NONE',  ( -0.1974969037888706647, 0.3420746716998658843, -2.375328083989501238 ) ) ;
#22014 = VERTEX_POINT ( 'NONE', #26278 ) ;
#22015 = CARTESIAN_POINT ( 'NONE',  ( 0.9186351706036752773, 0.1283753931104746893, -0.1820866141732285504 ) ) ;
#22016 = CARTESIAN_POINT ( 'NONE',  ( -0.3917322834645670104, -7.196005306013484475E-17, -0.8188976377952754682 ) ) ;
#22017 = CARTESIAN_POINT ( 'NONE',  ( 1.017060367454068581, -0.05778040916215560624, -0.4822834645669293319 ) ) ;
#22018 = CARTESIAN_POINT ( 'NONE',  ( 0.5027385518326215053, 1.496062992125283708, 0.5309055118110234117 ) ) ;
#22019 = CARTESIAN_POINT ( 'NONE',  ( -1.233595800524933894, 0.1283753931104748280, 0.1820866141732283561 ) ) ;
#22020 = CARTESIAN_POINT ( 'NONE',  ( 1.417322834645670104, -0.1870078740157480879, -0.4822834645669291653 ) ) ;
#22021 = CARTESIAN_POINT ( 'NONE',  ( -1.482939632545930975, -0.4281496062992127816, -0.4176697321401328100 ) ) ;
#22022 = CARTESIAN_POINT ( 'NONE',  ( 0.1958661417322836162, -0.3392501089628018329, -0.3293770096774785161 ) ) ;
#22023 = CARTESIAN_POINT ( 'NONE',  ( 0.1574803149606306130, -0.1870078740157480879, -0.4822834645669291653 ) ) ;
#22024 = CARTESIAN_POINT ( 'NONE',  ( -0.3740157480314953431, -0.4536011799217368745, -0.2665933059059886201 ) ) ;
#22025 = CARTESIAN_POINT ( 'NONE',  ( 0.9448818897637802916, -0.1870078740157479769, 0.4822834645669291653 ) ) ;
#22026 = CARTESIAN_POINT ( 'NONE',  ( -0.1771653543307080136, -0.5400638737290844871, 0.3530559997133364547 ) ) ;
#22027 = DIRECTION ( 'NONE',  ( 0.000000000000000000, 0.000000000000000000, 1.000000000000000000 ) ) ;
#22028 = DIRECTION ( 'NONE',  ( 0.000000000000000000, 0.000000000000000000, 1.000000000000000000 ) ) ;
#22029 = CARTESIAN_POINT ( 'NONE',  ( 0.3392501089628018884, -0.1958661417322833942, -1.834008817094174848 ) ) ;
#22030 = CARTESIAN_POINT ( 'NONE',  ( 0.7808398950131241190, -0.05778040916215560624, -0.4822834645669293319 ) ) ;
#22031 = CARTESIAN_POINT ( 'NONE',  ( 0.03280839895013198948, 0.2952755905511811885, 0.1292274648535926551 ) ) ;
#22032 = CARTESIAN_POINT ( 'NONE',  ( -1.023622047244093558, -0.1870078740157479769, 0.4822834645669291653 ) ) ;
#22033 = CARTESIAN_POINT ( 'NONE',  ( 1.089238845144357537, -0.4281496062992124485, 0.4176697321401328655 ) ) ;
#22034 = B_SPLINE_CURVE_WITH_KNOTS ( 'NONE', 3,
 ( #41159, #34853, #60515, #2864, #28527, #77812, #20143, #45792, #39496, #13838, #65184, #7520, #74401, #23448, #16745, #11249, #54184, #17568 ),
 .UNSPECIFIED., .F., .F.,
 ( 4, 2, 2, 2, 2, 2, 2, 2, 4 ),
 ( 0.000000000000000000, 0.001588476978679734600, 0.002382715468019601900, 0.002779834712689535550, 0.002978394335024502158, 0.003077674146191985462, 0.003127314051775727331, 0.003152134004567599349, 0.003176953957359471368 ),
 .UNSPECIFIED. ) ;
#22035 = CARTESIAN_POINT ( 'NONE',  ( 0.9514435695538062676, -0.3162353388693409650, -0.4822834645669289433 ) ) ;
#22036 = CARTESIAN_POINT ( 'NONE',  ( -9.594673741351313045E-17, 0.3917322834645670104, -0.8720472440944883052 ) ) ;
#22037 = CARTESIAN_POINT ( 'NONE',  ( -0.1640419947506555343, -0.3162353388693405765, 0.4822834645669290543 ) ) ;
#22038 = CARTESIAN_POINT ( 'NONE',  ( 0.6955380577427828781, -0.4281496062992124485, 0.4176697321401328655 ) ) ;
#22039 = CARTESIAN_POINT ( 'NONE',  ( -0.1771653543307080136, 0.1660481256975883668, -0.3530559997133364547 ) ) ;
#22040 = CARTESIAN_POINT ( 'NONE',  ( 0.7480314960629927956, 0.1771653543307087630, 0.000000000000000000 ) ) ;
#22041 = CARTESIAN_POINT ( 'NONE',  ( -1.259842519685038686, -0.1870078740157479769, 0.4822834645669291653 ) ) ;
#22042 = CARTESIAN_POINT ( 'NONE',  ( -1.640419947506561060, -0.4281496062992127816, -0.4176697321401328100 ) ) ;
#22043 = CARTESIAN_POINT ( 'NONE',  ( 0.1640419947506569498, -0.05778040916215522460, 0.4822834645669289988 ) ) ;
#22044 = CARTESIAN_POINT ( 'NONE',  ( -0.4359958488159582091, 1.724409448818897905, -3.937007874015763687 ) ) ;
#22045 = CARTESIAN_POINT ( 'NONE',  ( 0.3917322834645670104, -0.1049643490035303411, -2.308398950131233640 ) ) ;
#22046 = ORIENTED_EDGE ( 'NONE', *, *, #64557, .F. ) ;
#22047 = ORIENTED_EDGE ( 'NONE', *, *, #55030, .F. ) ;
#22048 = CARTESIAN_POINT ( 'NONE',  ( 1.069553805774278832, 0.2952755905511810774, -0.1292274648535930714 ) ) ;
#22049 = CARTESIAN_POINT ( 'NONE',  ( 0.7349081364829402885, -0.5023911411419708095, -0.1820866141732282451 ) ) ;
#22050 = DIRECTION ( 'NONE',  ( -0.000000000000000000, -1.000000000000000000, -0.000000000000000000 ) ) ;
#22051 = FACE_OUTER_BOUND ( 'NONE', #66881, .T. ) ;
#22052 = CARTESIAN_POINT ( 'NONE',  ( 0.1958661417322836440, -0.3392501089628017219, -1.121391076115485719 ) ) ;
#22053 = VECTOR ( 'NONE', #13912, 39.37007874015749564 ) ;
#22054 = CARTESIAN_POINT ( 'NONE',  ( -0.3460692066303960313, 0.1998031496062989965, -1.835301837270341352 ) ) ;
#22055 = CARTESIAN_POINT ( 'NONE',  ( -0.8727034120734901146, -0.3162353388693405765, 0.4822834645669290543 ) ) ;
#22056 = CARTESIAN_POINT ( 'NONE',  ( -0.6561679790026240244, -0.6046776061558807314, 0.2411417322834647770 ) ) ;
#22057 = CARTESIAN_POINT ( 'NONE',  ( 1.141732283464567566, 0.2952755905511811885, 0.000000000000000000 ) ) ;
#22058 = ORIENTED_EDGE ( 'NONE', *, *, #26365, .T. ) ;
#22059 = CARTESIAN_POINT ( 'NONE',  ( 1.594488188976378673, 0.1660481256975885056, 0.3530559997133364547 ) ) ;
#22060 = CARTESIAN_POINT ( 'NONE',  ( -1.120715528315120002, 1.066117147761049821, 0.06272875519749153417 ) ) ;
#22061 = APPLICATION_PROTOCOL_DEFINITION ( 'draft international standard', 'automotive_design', 1998, #67026 ) ;
#22062 = CARTESIAN_POINT ( 'NONE',  ( 1.581364829396326277, -0.2845877964562161244, -0.3641732283464567121 ) ) ;
#22063 = B_SPLINE_CURVE_WITH_KNOTS ( 'NONE', 3,
 ( #28446, #47795, #54523, #42308, #73912, #3612, #15847 ),
 .UNSPECIFIED., .F., .F.,
 ( 4, 3, 4 ),
 ( 7.703719777548943412E-34, 0.001246232571205256601, 0.002492492258783256774 ),
 .UNSPECIFIED. ) ;
#22064 = CARTESIAN_POINT ( 'NONE',  ( -0.1070741851644057135, 0.3996062992125984925, -2.130577427821522374 ) ) ;
#22065 = CARTESIAN_POINT ( 'NONE',  ( -1.456692913385826182, 0.1771653543307087630, 0.000000000000000000 ) ) ;
#22066 = DIRECTION ( 'NONE',  ( 0.000000000000000000, 0.000000000000000000, -1.000000000000000000 ) ) ;
#22067 = CARTESIAN_POINT ( 'NONE',  ( 0.2362204724409456558, -0.1870078740157479769, 0.4822834645669291653 ) ) ;
#22069 = DIRECTION ( 'NONE',  ( -0.000000000000000000, 1.000000000000000000, -0.000000000000000000 ) ) ;
#22068 = CARTESIAN_POINT ( 'NONE',  ( -0.4824498642376744417, -2.567464376874931580E-15, -0.4445507791589072832 ) ) ;
#22070 = CARTESIAN_POINT ( 'NONE',  ( -0.9514435695538050464, -0.2845877964562159024, 0.3641732283464567677 ) ) ;
#22071 = CARTESIAN_POINT ( 'NONE',  ( 0.6036745406824154392, 0.2306618581243847221, -0.2411417322834647770 ) ) ;
#22072 = CARTESIAN_POINT ( 'NONE',  ( 1.456692913385827515, 0.1771653543307087630, 0.000000000000000000 ) ) ;
#22073 = EDGE_CURVE ( 'NONE', #33549, #17115, #8898, .T. ) ;
#22074 = CARTESIAN_POINT ( 'NONE',  ( -0.2867679344610364334, -0.2867679344610368219, -1.241450500491126707 ) ) ;
#22075 = CARTESIAN_POINT ( 'NONE',  ( -0.8267716535433065062, -0.5511811023622047445, 6.969142054262312111E-17 ) ) ;
#22076 = CARTESIAN_POINT ( 'NONE',  ( 1.161417322834646493, -0.5400638737290844871, 0.3530559997133364547 ) ) ;
#22077 = CARTESIAN_POINT ( 'NONE',  ( 0.1230917936933036416, 1.944006284485450209, 0.2881873359806741419 ) ) ;
#22078 = CARTESIAN_POINT ( 'NONE',  ( -0.3412073490813641308, -0.6046776061558807314, 0.2411417322834647770 ) ) ;
#22079 = CARTESIAN_POINT ( 'NONE',  ( -1.128608923884513837, 0.1283753931104746893, -0.1820866141732285504 ) ) ;
#22080 = CARTESIAN_POINT ( 'NONE',  ( -0.4658792650918627265, -0.08942795157527998196, 0.3641732283464567121 ) ) ;
#22081 = CARTESIAN_POINT ( 'NONE',  ( -0.4396325459317579898, 0.2952755905511811885, 0.1292274648535926551 ) ) ;
#22082 = CARTESIAN_POINT ( 'NONE',  ( 1.640419947506562393, -0.4281496062992124485, 0.4176697321401328655 ) ) ;
#22083 = CARTESIAN_POINT ( 'NONE',  ( 0.1049643490035303967, 0.3917322834645670659, -0.3051374260180596543 ) ) ;
#22084 = CARTESIAN_POINT ( 'NONE',  ( 0.4002624671916016896, -0.3162353388693409650, -0.4822834645669289433 ) ) ;
#22085 = CARTESIAN_POINT ( 'NONE',  ( -0.6299212598425059095, 1.724409448818897905, -3.937007874015764131 ) ) ;
#22086 = CARTESIAN_POINT ( 'NONE',  ( -0.4091458600556402980, -0.2362204724409451284, -1.704068241469816058 ) ) ;
#22087 = CARTESIAN_POINT ( 'NONE',  ( -0.8202099737532801971, -0.6692913385826771977, 0.1292274648535927661 ) ) ;
#22088 = CARTESIAN_POINT ( 'NONE',  ( -0.1049868766404193215, 0.1283753931104746893, -0.1820866141732285504 ) ) ;
#22089 = CARTESIAN_POINT ( 'NONE',  ( -1.528871391076114250, -0.6692913385826771977, 0.1292274648535927661 ) ) ;
#22090 = CARTESIAN_POINT ( 'NONE',  ( 0.2165354330708668673, -0.5400638737290844871, 0.3530559997133364547 ) ) ;
#22091 = CARTESIAN_POINT ( 'NONE',  ( 0.2755905511811031494, 0.1771653543307087630, 0.000000000000000000 ) ) ;
#22092 = CARTESIAN_POINT ( 'NONE',  ( -0.8267716535433065062, -0.5511811023622047445, 6.969142054262312111E-17 ) ) ;
#22093 = CARTESIAN_POINT ( 'NONE',  ( -0.9973753280839886548, -0.6046776061558809534, -0.2411417322834644161 ) ) ;
#22094 = CARTESIAN_POINT ( 'NONE',  ( -1.384514435695537005, 0.2952755905511811885, 0.1292274648535926551 ) ) ;
#22095 = CARTESIAN_POINT ( 'NONE',  ( 1.174540682414699111, -0.3162353388693405765, 0.4822834645669290543 ) ) ;
#22096 = CARTESIAN_POINT ( 'NONE',  ( 0.1181102362204724532, -0.09842519685039369248, 5.158493410915829266E-18 ) ) ;
#22097 = CARTESIAN_POINT ( 'NONE',  ( 0.8661417322834653598, -0.1870078740157479769, 0.3641732283464567677 ) ) ;
#22098 = AXIS2_PLACEMENT_3D ( 'NONE', #9136, #2406, #28064 ) ;
#22099 = CARTESIAN_POINT ( 'NONE',  ( 0.8595800524934390507, -0.3162353388693405765, 0.4822834645669290543 ) ) ;
#22100 = DIRECTION ( 'NONE',  ( 1.000000000000000000, 0.000000000000000000, 3.455050906509825972E-15 ) ) ;
#22101 = CARTESIAN_POINT ( 'NONE',  ( 1.351706036745407458, -0.3690944881889765550, -0.3153832671262227771 ) ) ;
#22102 = EDGE_LOOP ( 'NONE', ( #9225, #47181, #19433, #49575 ) ) ;
#22103 = CARTESIAN_POINT ( 'NONE',  ( -0.6233595800524928121, -0.3162353388693409650, -0.4822834645669289433 ) ) ;
#22104 = CARTESIAN_POINT ( 'NONE',  ( 4.893765752498283308E-17, -0.3996062992125985480, -2.832677165354331006 ) ) ;
#22105 = CARTESIAN_POINT ( 'NONE',  ( -1.358267716535432434, -0.4536011799217367080, 0.2665933059059888421 ) ) ;
#22106 = CARTESIAN_POINT ( 'NONE',  ( -0.5708661417322825615, -0.5400638737290844871, 0.3530559997133364547 ) ) ;
#22107 = CARTESIAN_POINT ( 'NONE',  ( 0.2362204724409456558, -0.1870078740157480879, -0.4822834645669291653 ) ) ;
#22108 = CARTESIAN_POINT ( 'NONE',  ( -1.627296587926508442, -0.5023911411419708095, -0.1820866141732282451 ) ) ;
#22109 = CARTESIAN_POINT ( 'NONE',  ( -0.1998031496062994405, 0.3460692066303957537, -2.294619422572178546 ) ) ;
#22110 = CARTESIAN_POINT ( 'NONE',  ( -1.345144356955379816, -0.05778040916215560624, -0.4822834645669293319 ) ) ;
#22111 = CARTESIAN_POINT ( 'NONE',  ( 0.4133858267716541968, 0.1660481256975885056, 0.3530559997133364547 ) ) ;
#22112 = CARTESIAN_POINT ( 'NONE',  ( -0.1246719160104980823, -0.6692913385826773087, -0.1292274648535924053 ) ) ;
#22113 = CARTESIAN_POINT ( 'NONE',  ( 1.161417322834646271, 0.1660481256975883668, -0.3530559997133364547 ) ) ;
#22114 = DIRECTION ( 'NONE',  ( -0.000000000000000000, -0.000000000000000000, 1.000000000000000000 ) ) ;
#22115 = CARTESIAN_POINT ( 'NONE',  ( -0.3460692066303958092, -0.1998031496062994683, -1.942257217847769057 ) ) ;
#22116 = CARTESIAN_POINT ( 'NONE',  ( 0.1974969037888706369, -0.3420746716998659953, -1.194225721784776928 ) ) ;
#22117 = CARTESIAN_POINT ( 'NONE',  ( -9.787531504996567848E-17, 0.3996062992125986035, -2.362204724409448620 ) ) ;
#22118 = CARTESIAN_POINT ( 'NONE',  ( 0.1265901696524989184, 0.4724409448818898127, -0.6233595800524933672 ) ) ;
#22119 = CARTESIAN_POINT ( 'NONE',  ( 0.3917322834645670104, 2.398668435337828261E-17, -0.1102362204724409017 ) ) ;
#22120 = CARTESIAN_POINT ( 'NONE',  ( -0.1902887139107604098, -0.5511811023622046335, 0.09757992244046803654 ) ) ;
#22121 = CARTESIAN_POINT ( 'NONE',  ( -0.1968503937007867743, -0.6692913385826771977, 8.415575281601705876E-17 ) ) ;
#22122 = CARTESIAN_POINT ( 'NONE',  ( 0.7939632545931766261, -0.05778040916215522460, 0.4822834645669289988 ) ) ;
#22123 = CARTESIAN_POINT ( 'NONE',  ( -0.2891555358219911054, 0.2891555358219909388, -1.986220472440945128 ) ) ;
#22124 = CARTESIAN_POINT ( 'NONE',  ( 0.03937007874015833325, -0.5511811023622047445, 6.969142054262312111E-17 ) ) ;
#22125 =( BOUNDED_CURVE ( )  B_SPLINE_CURVE ( 2, ( #39081, #64344, #378, #5846, #82471, #37838, #18895, #45385, #32771, #24786, #50455, #44544, #6680 ),
 .UNSPECIFIED., .F., .F. ) 
 B_SPLINE_CURVE_WITH_KNOTS ( ( 3, 2, 2, 2, 2, 2, 3 ),
 ( 0.6733310946348007864, 0.6742424242424241987, 0.6780303030303029832, 0.6818181818181817677, 0.6856060606060605522, 0.6893939393939394478, 0.6903052690015629711 ),
 .UNSPECIFIED. ) 
 CURVE ( )  GEOMETRIC_REPRESENTATION_ITEM ( )  RATIONAL_B_SPLINE_CURVE ( ( 0.9875488213027523443, 0.9918020599134680371, 1.000000000000000000, 0.9659258262890683122, 1.000000000000000000, 0.9659258262890683122, 1.000000000000000000, 0.9659258262890683122, 1.000000000000000000, 0.9659258262890683122, 1.000000000000000000, 0.9918020599134671489, 0.9875488213027514561 ) ) 
 REPRESENTATION_ITEM ( '' )  );
#22126 = CARTESIAN_POINT ( 'NONE',  ( -1.187664041994749731, -0.3162353388693405765, 0.4822834645669290543 ) ) ;
#22127 = CARTESIAN_POINT ( 'NONE',  ( 1.122047244094488860, 0.1660481256975885056, 0.3530559997133364547 ) ) ;
#22128 = CARTESIAN_POINT ( 'NONE',  ( -0.3458507752293909498, 0.3458507752293907833, -2.066929133858267154 ) ) ;
#22129 = CARTESIAN_POINT ( 'NONE',  ( 0.4848199769444405671, 1.968301573707853303, 0.4917377963708856048 ) ) ;
#22130 = ORIENTED_EDGE ( 'NONE', *, *, #37699, .T. ) ;
#22131 = ORIENTED_EDGE ( 'NONE', *, *, #72797, .T. ) ;
#22132 = CARTESIAN_POINT ( 'NONE',  ( 1.056430446194226436, -0.6692913385826773087, -0.1292274648535924053 ) ) ;
#22133 = CARTESIAN_POINT ( 'NONE',  ( -1.568241469816272105, -0.05778040916215522460, 0.4822834645669289988 ) ) ;
#22135 = CARTESIAN_POINT ( 'NONE',  ( -1.207349081364828436, -0.6046776061558807314, 0.2411417322834647770 ) ) ;
#22134 = CARTESIAN_POINT ( 'NONE',  ( -1.135170603674539924, 0.1771653543307087075, -0.09757992244046823083 ) ) ;
#22136 = CARTESIAN_POINT ( 'NONE',  ( -0.3392501089628019439, 0.1958661417322832554, -2.311004306265404651 ) ) ;
#22137 = CARTESIAN_POINT ( 'NONE',  ( 1.348312163386739426, 0.2755905511811023723, 0.8577811012195456497 ) ) ;
#22138 = CARTESIAN_POINT ( 'NONE',  ( 1.207349081364829990, 0.2306618581243848609, 0.2411417322834645549 ) ) ;
#22139 = CARTESIAN_POINT ( 'NONE',  ( -1.601049868766403650, -0.6046776061558807314, 0.2411417322834647770 ) ) ;
#22140 = CARTESIAN_POINT ( 'NONE',  ( -0.1181102362204717315, 0.2952755905511811885, 0.000000000000000000 ) ) ;
#22141 = CARTESIAN_POINT ( 'NONE',  ( 0.03937007874015806264, 0.2952755905511811885, 0.000000000000000000 ) ) ;
#22142 = CARTESIAN_POINT ( 'NONE',  ( -1.417322834645668772, -0.1870078740157480879, -0.4822834645669291653 ) ) ;
#22143 = B_SPLINE_CURVE_WITH_KNOTS ( 'NONE', 3,
 ( #25452, #25040, #6105, #70492 ),
 .UNSPECIFIED., .F., .F.,
 ( 4, 4 ),
 ( 3.593986969187450165E-07, 0.001287825409103224641 ),
 .UNSPECIFIED. ) ;
#22144 = CARTESIAN_POINT ( 'NONE',  ( 0.1958661417322836440, -0.3392501089628017219, -0.3339895013123360679 ) ) ;
#22145 = CARTESIAN_POINT ( 'NONE',  ( 0.1574803149606306130, -0.1870078740157479769, 0.4822834645669291653 ) ) ;
#22146 = CARTESIAN_POINT ( 'NONE',  ( 4.797336870675656522E-17, -0.3917322834645670104, -1.960629921259842368 ) ) ;
#22147 = CARTESIAN_POINT ( 'NONE',  ( -1.312335958005248715, 0.1283753931104748280, 0.1820866141732283561 ) ) ;
#22148 = ORIENTED_EDGE ( 'NONE', *, *, #33639, .T. ) ;
#22149 = CARTESIAN_POINT ( 'NONE',  ( -0.2891555358219908833, -0.2891555358219912164, -2.421259842519685623 ) ) ;
#22150 = ORIENTED_EDGE ( 'NONE', *, *, #34100, .F. ) ;
#22151 = DIRECTION ( 'NONE',  ( -1.000000000000000000, -0.000000000000000000, -0.000000000000000000 ) ) ;
#22152 = CARTESIAN_POINT ( 'NONE',  ( -1.660104986876639543, -0.05778040916215560624, -0.4822834645669293319 ) ) ;
#22153 = CARTESIAN_POINT ( 'NONE',  ( -0.1070741851644056997, 0.3996062992125986035, -0.9514435695538056015 ) ) ;
#22154 = CARTESIAN_POINT ( 'NONE',  ( -1.463254593175852492, -0.6692913385826773087, -0.1292274648535924053 ) ) ;
#22155 = LINE ( 'NONE', #56604, #77376 ) ;
#22156 = CARTESIAN_POINT ( 'NONE',  ( 0.1938976377952755792, 0.1938976377952755792, -0.3740157480314971750 ) ) ;
#22157 = CARTESIAN_POINT ( 'NONE',  ( -1.572991167713776672, 2.401574803149606474, 0.1227090857360981641 ) ) ;
#22158 = CARTESIAN_POINT ( 'NONE',  ( -0.3392501089628019995, 0.1958661417322832277, 0.04658792650918625738 ) ) ;
#22159 = CARTESIAN_POINT ( 'NONE',  ( -0.4330708661417315697, -0.5511811023622047445, 6.969142054262312111E-17 ) ) ;
#22160 = CARTESIAN_POINT ( 'NONE',  ( -0.7414698162729651543, 0.1771653543307087075, -0.09757992244046823083 ) ) ;
#22161 = AXIS2_PLACEMENT_3D ( 'NONE', #51950, #47305, #78497 ) ;
#22162 = CARTESIAN_POINT ( 'NONE',  ( -1.181102362204723644, -0.1870078740157479769, 0.4822834645669291653 ) ) ;
#22163 = CARTESIAN_POINT ( 'NONE',  ( 0.4658792650918640033, -0.3162353388693405765, 0.4822834645669290543 ) ) ;
#22164 = CARTESIAN_POINT ( 'NONE',  ( -0.7611548556430438595, -0.6046776061558809534, -0.2411417322834644161 ) ) ;
#22165 = CARTESIAN_POINT ( 'NONE',  ( -0.3392501089628019995, 0.1958661417322832277, 0.1391076115485564701 ) ) ;
#22166 = ORIENTED_EDGE ( 'NONE', *, *, #4970, .T. ) ;
#22167 = CARTESIAN_POINT ( 'NONE',  ( -1.568241469816272105, -0.3162353388693409650, -0.4822834645669289433 ) ) ;
#22168 = PLANE ( 'NONE',  #17865 ) ;
#22169 = CARTESIAN_POINT ( 'NONE',  ( 0.1265901696524990294, -0.4724409448818896462, -1.187664041994750619 ) ) ;
#22170 = CARTESIAN_POINT ( 'NONE',  ( 1.901586028222546521, 1.118719813955014741, -0.2236424093447257344 ) ) ;
#22171 = EDGE_CURVE ( 'NONE', #949, #30946, #50495, .T. ) ;
#22172 = CARTESIAN_POINT ( 'NONE',  ( -0.1958661417322836718, 0.3392501089628017219, -0.7926509186351704539 ) ) ;
#22173 = CARTESIAN_POINT ( 'NONE',  ( -0.1049643490035307020, 0.3917322834645669549, -2.295931758530183497 ) ) ;
#22174 = CARTESIAN_POINT ( 'NONE',  ( -0.7939632545931750718, -0.05778040916215560624, -0.4822834645669293319 ) ) ;
#22175 = CARTESIAN_POINT ( 'NONE',  ( 1.489501312335958172, -0.3162353388693405765, 0.4822834645669290543 ) ) ;
#22176 = CARTESIAN_POINT ( 'NONE',  ( -0.2925321140481932369, 0.2925321140481931259, -0.2539370078740156855 ) ) ;
#22178 = CARTESIAN_POINT ( 'NONE',  ( -0.4695140184743471501, 1.605872332714552542, 2.565964038698629768 ) ) ;
#22177 = CARTESIAN_POINT ( 'NONE',  ( -1.313877454013331780, 0.000000000000000000, 0.7983292792091805090 ) ) ;
#22179 = CARTESIAN_POINT ( 'NONE',  ( -1.437007874015747477, -0.5400638737290844871, 0.3530559997133364547 ) ) ;
#22180 = CARTESIAN_POINT ( 'NONE',  ( -0.6955380577427815458, -0.4281496062992127816, -0.4176697321401328100 ) ) ;
#22181 = AXIS2_PLACEMENT_3D ( 'NONE', #10265, #78902, #73411 ) ;
#22182 = CARTESIAN_POINT ( 'NONE',  ( -9.594673741351310580E-17, 0.3917322834645669549, 0.2349274522647787078 ) ) ;
#22183 = CARTESIAN_POINT ( 'NONE',  ( 0.3805774278215230400, -0.004921259842519870586, -0.3153832671262229437 ) ) ;
#22184 = CARTESIAN_POINT ( 'NONE',  ( -0.3392501089628017219, -0.1958661417322836718, -0.4520997375328084655 ) ) ;
#22185 = CARTESIAN_POINT ( 'NONE',  ( 0.1968503937007881344, -0.5511811023622047445, 6.969142054262312111E-17 ) ) ;
#22186 = CARTESIAN_POINT ( 'NONE',  ( 1.115485564304462551, -0.004921259842519576551, 0.3153832671262227771 ) ) ;
#22187 = CARTESIAN_POINT ( 'NONE',  ( 1.128608923884514947, 0.2306618581243848609, 0.2411417322834645549 ) ) ;
#22188 = CARTESIAN_POINT ( 'NONE',  ( -0.09842519685039295696, -0.4536011799217367080, 0.2665933059059888421 ) ) ;
#22189 = CARTESIAN_POINT ( 'NONE',  ( -0.3392501089628017219, -0.1958661417322836718, -1.776902887139107490 ) ) ;
#22190 = CARTESIAN_POINT ( 'NONE',  ( 1.437007874015748810, 0.1660481256975885056, 0.3530559997133364547 ) ) ;
#22191 = B_SPLINE_CURVE_WITH_KNOTS ( 'NONE', 3,
 ( #57981, #32319, #346, #52500, #32739, #72308, #78209, #26841 ),
 .UNSPECIFIED., .F., .F.,
 ( 4, 2, 2, 4 ),
 ( 0.000000000000000000, 0.002441020876198872046, 0.003661531314298308287, 0.004882041752397744960 ),
 .UNSPECIFIED. ) ;
#22192 = CARTESIAN_POINT ( 'NONE',  ( -1.095800524934382292, -0.2845877964562161244, -0.3641732283464567121 ) ) ;
#22193 = CARTESIAN_POINT ( 'NONE',  ( -0.4091458600556402980, -0.2362204724409451284, -0.4442257217847768724 ) ) ;
#22194 = CARTESIAN_POINT ( 'NONE',  ( -1.017060367454067249, -0.08942795157527998196, 0.3641732283464567121 ) ) ;
#22195 = CARTESIAN_POINT ( 'NONE',  ( 0.03937007874015833325, -0.6692913385826771977, 8.415575281601705876E-17 ) ) ;
#22196 = CARTESIAN_POINT ( 'NONE',  ( 1.522309711286089939, 0.1283753931104748280, 0.1820866141732283561 ) ) ;
#22197 = CARTESIAN_POINT ( 'NONE',  ( 0.4199475065616803948, -0.5023911411419708095, -0.1820866141732282451 ) ) ;
#22198 = CARTESIAN_POINT ( 'NONE',  ( -0.3937007874015740483, -0.1870078740157480601, -0.3641732283464567677 ) ) ;
#22199 = B_SPLINE_CURVE_WITH_KNOTS ( 'NONE', 3,
 ( #27325, #59312, #27746, #26071, #77432, #45420, #52985, #13459, #46682, #39116, #8396, #72375 ),
 .UNSPECIFIED., .F., .F.,
 ( 4, 2, 2, 2, 2, 4 ),
 ( 0.007992874908875674880, 0.009303755029337829399, 0.01061463514979998392, 0.01192551527026214017, 0.01258095533049322090, 0.01323639539072430336 ),
 .UNSPECIFIED. ) ;
#22200 = CARTESIAN_POINT ( 'NONE',  ( -0.5971128608923877978, -0.6692913385826773087, -0.1292274648535924053 ) ) ;
#22201 = DIRECTION ( 'NONE',  ( -3.491481338843132961E-15, -0.000000000000000000, 1.000000000000000000 ) ) ;
#22202 = CARTESIAN_POINT ( 'NONE',  ( 2.795275590551181466, 1.968503937007874960, 0.000000000000000000 ) ) ;
#22203 = CARTESIAN_POINT ( 'NONE',  ( 0.2296587926509192634, -0.3162353388693405765, 0.4822834645669290543 ) ) ;
#22204 = CARTESIAN_POINT ( 'NONE',  ( 4.893765752498283308E-17, -0.3996062992125985480, -1.730314960629921517 ) ) ;
#22205 = CARTESIAN_POINT ( 'NONE',  ( 1.528871391076116026, -0.6692913385826773087, -0.1292274648535924053 ) ) ;
#22206 = CARTESIAN_POINT ( 'NONE',  ( -0.07874015748031421014, -0.1870078740157480601, -0.3641732283464567677 ) ) ;
#22207 = CARTESIAN_POINT ( 'NONE',  ( -0.1706036745406816491, -0.4281496062992124485, 0.4176697321401328655 ) ) ;
#22208 = CARTESIAN_POINT ( 'NONE',  ( -1.391076115485563314, -0.6046776061558809534, -0.2411417322834644161 ) ) ;
#22209 = CARTESIAN_POINT ( 'NONE',  ( -1.443569553805773564, 0.1283753931104746893, -0.1820866141732285504 ) ) ;
#22210 = CARTESIAN_POINT ( 'NONE',  ( 1.128608923884515169, -0.6046776061558809534, -0.2411417322834644161 ) ) ;
#22211 = CARTESIAN_POINT ( 'NONE',  ( -0.7545931758530177724, 0.1771653543307087630, 0.09757992244046791164 ) ) ;
#22212 = CARTESIAN_POINT ( 'NONE',  ( -0.1998031496062994405, 0.3460692066303957537, -0.4048556430446194621 ) ) ;
#22213 = CARTESIAN_POINT ( 'NONE',  ( 0.2925321140481932369, 0.2925321140481932369, 0.01968503937007873641 ) ) ;
#22214 = CARTESIAN_POINT ( 'NONE',  ( 4.797336870675656522E-17, -0.3917322834645670659, -2.752643987697849237 ) ) ;
#22215 = CARTESIAN_POINT ( 'NONE',  ( -1.456692913385826182, -0.6692913385826771977, 8.415575281601705876E-17 ) ) ;
#22216 = CARTESIAN_POINT ( 'NONE',  ( 1.555118110236221041, 0.07958543189024071263, -0.2665933059059888421 ) ) ;
#22217 = CARTESIAN_POINT ( 'NONE',  ( 1.246719160104987623, -0.3690944881889763329, 0.3153832671262228327 ) ) ;
#22218 = CARTESIAN_POINT ( 'NONE',  ( -1.594488188976377563, -0.5400638737290844871, 0.3530559997133364547 ) ) ;
#22219 = CARTESIAN_POINT ( 'NONE',  ( 0.7808398950131240079, -0.3162353388693405765, 0.4822834645669290543 ) ) ;
#22220 = CARTESIAN_POINT ( 'NONE',  ( 0.1058382717557500852, -0.3949938075777408852, -0.9494750656167980640 ) ) ;
#22221 = CARTESIAN_POINT ( 'NONE',  ( 1.391076115485564868, 0.1283753931104746893, -0.1820866141732285504 ) ) ;
#22222 = CARTESIAN_POINT ( 'NONE',  ( 0.05905511811023709395, -0.5400638737290844871, 0.3530559997133364547 ) ) ;
#22223 = CARTESIAN_POINT ( 'NONE',  ( -0.3215223097112853146, -0.05778040916215560624, -0.4822834645669293319 ) ) ;
#22224 = CARTESIAN_POINT ( 'NONE',  ( 1.653543307086614789, -0.1870078740157479769, 0.4822834645669291653 ) ) ;
#22225 = CARTESIAN_POINT ( 'NONE',  ( -0.2362204724409451284, 0.4091458600556402425, -0.6430446194225721834 ) ) ;
#22226 = LINE ( 'NONE', #34863, #10261 ) ;
#22227 = VECTOR ( 'NONE', #80088, 39.37007874015748143 ) ;
#22228 = CARTESIAN_POINT ( 'NONE',  ( 0.1574803149606306130, -0.1870078740157479769, 0.3641732283464567677 ) ) ;
#22229 = VERTEX_POINT ( 'NONE', #26700 ) ;
#22230 = CARTESIAN_POINT ( 'NONE',  ( 0.3917322834645670659, 2.398668435337828261E-17, -0.4298093420285583055 ) ) ;
#22231 = EDGE_LOOP ( 'NONE', ( #15841, #21729, #58267, #83206 ) ) ;
#22232 = CARTESIAN_POINT ( 'NONE',  ( -0.3740157480314953431, -0.5400638737290845981, -0.3530559997133363437 ) ) ;
#22233 = CARTESIAN_POINT ( 'NONE',  ( 0.9711286089238851948, 0.2306618581243848609, 0.2411417322834645549 ) ) ;
#22234 = CARTESIAN_POINT ( 'NONE',  ( 0.3083989501312343062, -0.05778040916215560624, -0.4822834645669293319 ) ) ;
#22235 = CARTESIAN_POINT ( 'NONE',  ( -0.2034120734908128059, 0.1771653543307087630, 0.09757992244046791164 ) ) ;
#22236 = CARTESIAN_POINT ( 'NONE',  ( 0.9383202099737538715, -0.05778040916215560624, -0.4822834645669293319 ) ) ;
#22237 = CARTESIAN_POINT ( 'NONE',  ( -0.9317585301837263412, -0.4281496062992127816, -0.4176697321401328100 ) ) ;
#22238 = CARTESIAN_POINT ( 'NONE',  ( -0.5511811023622041894, -0.1870078740157480879, -0.4822834645669291653 ) ) ;
#22239 = CARTESIAN_POINT ( 'NONE',  ( -1.003937007874015297, -0.5400638737290845981, -0.3530559997133363437 ) ) ;
#22240 = CARTESIAN_POINT ( 'NONE',  ( 1.003937007874016185, 0.1660481256975883668, -0.3530559997133364547 ) ) ;
#22241 = CARTESIAN_POINT ( 'NONE',  ( 0.8727034120734912248, -0.3162353388693409650, -0.4822834645669289433 ) ) ;
#22242 = CARTESIAN_POINT ( 'NONE',  ( 0.9580052493438327987, -0.4281496062992127816, -0.4176697321401328100 ) ) ;
#22243 = CARTESIAN_POINT ( 'NONE',  ( 0.3392501089628018884, -0.1958661417322834220, -0.7270341207349080292 ) ) ;
#22244 = CARTESIAN_POINT ( 'NONE',  ( -0.1377952755905504645, -0.4536011799217368745, -0.2665933059059886201 ) ) ;
#22245 = ORIENTED_EDGE ( 'NONE', *, *, #43710, .F. ) ;
#22246 = CARTESIAN_POINT ( 'NONE',  ( 0.3949938075777411073, -0.1058382717557499464, -1.056430446194225770 ) ) ;
#22247 = ORIENTED_EDGE ( 'NONE', *, *, #9984, .T. ) ;
#22248 = CARTESIAN_POINT ( 'NONE',  ( -0.9383202099737524282, -0.08942795157527998196, 0.3641732283464567121 ) ) ;
#22249 = CARTESIAN_POINT ( 'NONE',  ( -0.5380577427821514602, 0.05413385826771666132, 0.4176697321401328100 ) ) ;
#22250 = CARTESIAN_POINT ( 'NONE',  ( -0.4744094488189106174, 1.537401574803149984, 3.908320185825790105 ) ) ;
#22251 = CARTESIAN_POINT ( 'NONE',  ( -0.3083989501312330295, -0.05778040916215522460, 0.4822834645669289988 ) ) ;
#22252 = CARTESIAN_POINT ( 'NONE',  ( -0.5577427821522301654, -0.05778040916215560624, -0.4822834645669293319 ) ) ;
#22253 = CARTESIAN_POINT ( 'NONE',  ( -1.292650918635170010, 0.2952755905511810774, -0.1292274648535930714 ) ) ;
#22254 = CARTESIAN_POINT ( 'NONE',  ( -1.561679790026246017, 0.05413385826771666132, 0.4176697321401328100 ) ) ;
#22255 = CARTESIAN_POINT ( 'NONE',  ( 0.9317585301837276734, -0.004921259842519870586, -0.3153832671262229437 ) ) ;
#22256 = CARTESIAN_POINT ( 'NONE',  ( -0.4091458600556405756, 0.2362204724409446288, -0.4179790026246719137 ) ) ;
#22257 = CARTESIAN_POINT ( 'NONE',  ( -1.586688153636163001, 2.388437996263389707, 0.1275903502784764276 ) ) ;
#22258 = CARTESIAN_POINT ( 'NONE',  ( 0.3149606299212603933, -0.1870078740157479769, 0.3641732283464567677 ) ) ;
#22259 = CARTESIAN_POINT ( 'NONE',  ( 0.07874015748031558404, -0.1870078740157479769, 0.4822834645669291653 ) ) ;
#22260 = CARTESIAN_POINT ( 'NONE',  ( 0.1706036745406830368, -0.4281496062992127816, -0.4176697321401328100 ) ) ;
#22261 = VERTEX_POINT ( 'NONE', #52355 ) ;
#22262 = CARTESIAN_POINT ( 'NONE',  ( 0.1070741851644054915, -0.3996062992125986035, -1.817585301837270517 ) ) ;
#22263 = DIRECTION ( 'NONE',  ( 0.000000000000000000, 0.000000000000000000, 1.000000000000000000 ) ) ;
#22264 = ORIENTED_EDGE ( 'NONE', *, *, #73388, .F. ) ;
#22265 = CARTESIAN_POINT ( 'NONE',  ( -0.1070741851644056997, 0.3996062992125984925, -1.343175853018372834 ) ) ;
#22266 = CARTESIAN_POINT ( 'NONE',  ( 0.3996062992125985480, 2.446882876249141654E-17, -0.6673228346456693272 ) ) ;
#22267 = CARTESIAN_POINT ( 'NONE',  ( -0.8267716535433065062, -0.5511811023622047445, 6.969142054262312111E-17 ) ) ;
#22268 = CARTESIAN_POINT ( 'NONE',  ( -0.4593175853018366950, 0.05413385826771666132, 0.4176697321401328100 ) ) ;
#22269 = CARTESIAN_POINT ( 'NONE',  ( -0.4724409448818899238, 0.1265901696524986686, -0.1902887139107611314 ) ) ;
#22270 = CARTESIAN_POINT ( 'NONE',  ( 0.1049643490035303689, 0.3917322834645670104, -2.597769028871390606 ) ) ;
#22271 = CARTESIAN_POINT ( 'NONE',  ( -1.561679790026246017, -0.3690944881889765550, -0.3153832671262227771 ) ) ;
#22272 = CARTESIAN_POINT ( 'NONE',  ( 0.6824146981627303710, 0.2306618581243847221, -0.2411417322834647770 ) ) ;
#22273 = CARTESIAN_POINT ( 'NONE',  ( 0.3543307086614181922, -0.6692913385826771977, 8.415575281601705876E-17 ) ) ;
#22274 = CARTESIAN_POINT ( 'NONE',  ( -0.7217847769028863381, -0.3690944881889763329, 0.3153832671262228327 ) ) ;
#22275 = CARTESIAN_POINT ( 'NONE',  ( 0.1902887139107617975, 0.2952755905511811885, 0.1292274648535926551 ) ) ;
#22276 = CARTESIAN_POINT ( 'NONE',  ( -0.4724409448818898682, -8.678599364036362592E-17, -1.848425196850393526 ) ) ;
#22277 = CARTESIAN_POINT ( 'NONE',  ( -0.006561679790025524116, -0.08942795157528024563, -0.3641732283464568787 ) ) ;
#22278 = CARTESIAN_POINT ( 'NONE',  ( -0.4396325459317579898, 0.2952755905511811885, 0.1292274648535926551 ) ) ;
#22279 = CARTESIAN_POINT ( 'NONE',  ( 4.837279021331061486E-17, -0.3949938075777409963, -1.887795275590550936 ) ) ;
#22280 = CARTESIAN_POINT ( 'NONE',  ( -1.594488188976377563, -0.5400638737290844871, 0.3530559997133364547 ) ) ;
#22281 = CARTESIAN_POINT ( 'NONE',  ( -0.03937007874015669567, -0.5511811023622047445, 6.969142054262312111E-17 ) ) ;
#22282 = CARTESIAN_POINT ( 'NONE',  ( 1.633858267716535639, -0.4536011799217367080, 0.2665933059059888421 ) ) ;
#22283 = CARTESIAN_POINT ( 'NONE',  ( -1.213910761154854745, 0.2952755905511810774, -0.1292274648535930714 ) ) ;
#22284 = CARTESIAN_POINT ( 'NONE',  ( -0.5577427821522301654, -0.2845877964562159024, 0.3641732283464567677 ) ) ;
#22285 = CARTESIAN_POINT ( 'NONE',  ( -0.3458507752293909498, 0.3458507752293908388, -2.301181102362204633 ) ) ;
#22286 = CARTESIAN_POINT ( 'NONE',  ( -1.095800524934382292, -0.05778040916215522460, 0.4822834645669289988 ) ) ;
#22287 = CARTESIAN_POINT ( 'NONE',  ( -0.2230971128608915943, 0.05413385826771666132, 0.4176697321401328100 ) ) ;
#22288 = CARTESIAN_POINT ( 'NONE',  ( -9.787531504996566615E-17, 0.3996062992125985480, -2.438976377952756014 ) ) ;
#22289 = CARTESIAN_POINT ( 'NONE',  ( -0.1049643490035301746, -0.3917322834645670659, -2.356936064795589036 ) ) ;
#22290 = CARTESIAN_POINT ( 'NONE',  ( 0.5314960629920851831, 2.725289161120230563, 3.884611959489594035 ) ) ;
#22291 = CARTESIAN_POINT ( 'NONE',  ( 0.1902887139107617975, -0.5511811023622048555, -0.09757992244046775898 ) ) ;
#22292 = CARTESIAN_POINT ( 'NONE',  ( 1.108923884514436242, -0.05778040916215522460, 0.4822834645669289988 ) ) ;
#22293 = CARTESIAN_POINT ( 'NONE',  ( -1.220472440944881054, 0.1771653543307087630, 0.000000000000000000 ) ) ;
#22294 = CARTESIAN_POINT ( 'NONE',  ( 1.312335958005250269, -0.6046776061558807314, 0.2411417322834647770 ) ) ;
#22295 = CARTESIAN_POINT ( 'NONE',  ( -1.601049868766403650, -0.5023911411419708095, 0.1820866141732285504 ) ) ;
#22296 = CARTESIAN_POINT ( 'NONE',  ( -0.4527559055118102749, 0.1660481256975885056, 0.3530559997133364547 ) ) ;
#22297 = CARTESIAN_POINT ( 'NONE',  ( 0.04593175853018440641, -0.5511811023622046335, 0.09757992244046803654 ) ) ;
#22298 = CARTESIAN_POINT ( 'NONE',  ( -3.937007874015748143, 2.165354330708661568, 0.6299212598425196763 ) ) ;
#22299 = CARTESIAN_POINT ( 'NONE',  ( 0.4855643044619428750, -0.004921259842519576551, 0.3153832671262227771 ) ) ;
#22300 = EDGE_CURVE ( 'NONE', #29190, #64851, #81283, .T. ) ;
#22301 = CARTESIAN_POINT ( 'NONE',  ( -0.1312335958005241554, -0.6046776061558809534, -0.2411417322834644161 ) ) ;
#22302 =( BOUNDED_CURVE ( )  B_SPLINE_CURVE ( 1, ( #22068, #22892 ),
 .UNSPECIFIED., .F., .F. ) 
 B_SPLINE_CURVE_WITH_KNOTS ( ( 2, 2 ),
 ( 1.734723475976807094E-18, 0.002000000000000001776 ),
 .UNSPECIFIED. ) 
 CURVE ( )  GEOMETRIC_REPRESENTATION_ITEM ( )  RATIONAL_B_SPLINE_CURVE ( ( 0.9875488213027523443, 0.9875488213027523443 ) ) 
 REPRESENTATION_ITEM ( '' )  );
#22303 = CARTESIAN_POINT ( 'NONE',  ( -0.1070741851644051862, -0.3996062992125986590, -0.3064304461942257141 ) ) ;
#22304 = EDGE_CURVE ( 'NONE', #59607, #5541, #6511, .T. ) ;
#22305 = CARTESIAN_POINT ( 'NONE',  ( -1.259842519685038686, -0.1870078740157479769, 0.4822834645669291653 ) ) ;
#22306 = CARTESIAN_POINT ( 'NONE',  ( -0.2867679344610364334, -0.2867679344610367109, -2.033464566929133355 ) ) ;
#22307 = CARTESIAN_POINT ( 'NONE',  ( 0.9317585301837276734, -0.3690944881889763329, 0.3153832671262228327 ) ) ;
#22308 = CARTESIAN_POINT ( 'NONE',  ( -0.1115485564304453947, -0.6692913385826771977, 0.1292274648535927661 ) ) ;
#22309 = CARTESIAN_POINT ( 'NONE',  ( -0.3149606299212590610, -0.1870078740157480879, -0.4822834645669291653 ) ) ;
#22310 = CARTESIAN_POINT ( 'NONE',  ( -0.5183727034120726440, 0.1771653543307087630, 0.09757992244046791164 ) ) ;
#22311 = CARTESIAN_POINT ( 'NONE',  ( 1.191111281560510715, -4.927456884911482678E-16, 0.4445507791589062840 ) ) ;
#22312 = CARTESIAN_POINT ( 'NONE',  ( -0.3871391076115476282, -0.08942795157527998196, 0.3641732283464567121 ) ) ;
#22313 = CARTESIAN_POINT ( 'NONE',  ( 0.4265091863517067594, 0.2952755905511811885, 0.1292274648535926551 ) ) ;
#22314 = CARTESIAN_POINT ( 'NONE',  ( -0.6692913385826764205, -0.5511811023622047445, 6.969142054262312111E-17 ) ) ;
#22315 = CARTESIAN_POINT ( 'NONE',  ( -0.3996062992125985480, -7.340648628747423112E-17, -1.061023622047243986 ) ) ;
#22316 = CARTESIAN_POINT ( 'NONE',  ( -1.332020997375327642, -0.05778040916215522460, 0.4822834645669289988 ) ) ;
#22317 = CARTESIAN_POINT ( 'NONE',  ( 0.000000000000000000, 1.724409448818897461, 0.000000000000000000 ) ) ;
#22318 = ORIENTED_EDGE ( 'NONE', *, *, #6995, .T. ) ;
#22319 = CARTESIAN_POINT ( 'NONE',  ( -1.227034120734907585, 0.1771653543307087630, 0.09757992244046791164 ) ) ;
#22320 = CARTESIAN_POINT ( 'NONE',  ( -0.5249343832020990641, -0.6046776061558809534, -0.2411417322834644161 ) ) ;
#22321 = CARTESIAN_POINT ( 'NONE',  ( -1.620734908136482577, -0.6692913385826773087, -0.1292274648535924053 ) ) ;
#22322 = CARTESIAN_POINT ( 'NONE',  ( -1.240157480314959759, -0.5400638737290845981, -0.3530559997133363437 ) ) ;
#22323 = CARTESIAN_POINT ( 'NONE',  ( -0.4724409448818898682, -8.678599364036362592E-17, -2.163385826771653697 ) ) ;
#22324 = EDGE_CURVE ( 'NONE', #44273, #44157, #65392, .T. ) ;
#22325 = CARTESIAN_POINT ( 'NONE',  ( 1.443569553805774897, -0.6046776061558809534, -0.2411417322834644161 ) ) ;
#22326 = CARTESIAN_POINT ( 'NONE',  ( 0.9120734908136490793, 0.2952755905511810774, -0.1292274648535930714 ) ) ;
#22327 = CARTESIAN_POINT ( 'NONE',  ( -0.2867679344610364334, -0.2867679344610367109, -2.728346456692912536 ) ) ;
#22329 = VECTOR ( 'NONE', #7906, 39.37007874015748854 ) ;
#22328 = CARTESIAN_POINT ( 'NONE',  ( 1.614173228346457378, 0.2753471884572478157, 0.1372047244094478646 ) ) ;
#22330 = EDGE_CURVE ( 'NONE', #64851, #35306, #60714, .T. ) ;
#22331 = CARTESIAN_POINT ( 'NONE',  ( -1.627296587926508442, -0.6046776061558809534, -0.2411417322834644161 ) ) ;
#22332 = CARTESIAN_POINT ( 'NONE',  ( -0.1998031496062991907, -0.3460692066303959757, -0.5380577427821522374 ) ) ;
#22333 = ORIENTED_EDGE ( 'NONE', *, *, #49427, .T. ) ;
#22334 = CARTESIAN_POINT ( 'NONE',  ( -0.4921259842519677963, 0.07958543189024071263, -0.2665933059059888421 ) ) ;
#22335 = CARTESIAN_POINT ( 'NONE',  ( 0.3917322834645670104, -0.1049643490035303411, -2.308398950131233640 ) ) ;
#22336 = EDGE_LOOP ( 'NONE', ( #2894, #52771, #69276, #57517 ) ) ;
#22337 = CARTESIAN_POINT ( 'NONE',  ( 0.7480314960629927956, -0.6692913385826771977, 8.415575281601705876E-17 ) ) ;
#22339 = CARTESIAN_POINT ( 'NONE',  ( -0.2887139107611542133, 0.2306618581243848609, 0.2411417322834645549 ) ) ;
#22338 = PRODUCT_RELATED_PRODUCT_CATEGORY ( 'part', '', ( #46652 ) ) ;
#22340 = CARTESIAN_POINT ( 'NONE',  ( -0.7152230971128602510, -0.3162353388693405765, 0.4822834645669290543 ) ) ;
#22341 = CARTESIAN_POINT ( 'NONE',  ( 1.325459317585302665, -0.4281496062992124485, 0.4176697321401328655 ) ) ;
#22342 = CARTESIAN_POINT ( 'NONE',  ( -1.187664041994749731, -0.2845877964562159024, 0.3641732283464567677 ) ) ;
#22343 = CARTESIAN_POINT ( 'NONE',  ( 0.4724409448818881474, -0.1265901696525019160, -2.078083989501312345 ) ) ;
#22344 = CARTESIAN_POINT ( 'NONE',  ( 0.2624671916010504757, 0.2306618581243848609, 0.2411417322834645549 ) ) ;
#22345 = CARTESIAN_POINT ( 'NONE',  ( -0.8070866141732276899, 0.1660481256975883668, -0.3530559997133364547 ) ) ;
#22346 = CARTESIAN_POINT ( 'NONE',  ( 0.1958661417322834497, 0.3392501089628018329, -1.641712967682728008 ) ) ;
#22347 = CARTESIAN_POINT ( 'NONE',  ( -1.089238845144356427, -0.4281496062992127816, -0.4176697321401328100 ) ) ;
#22348 = CARTESIAN_POINT ( 'NONE',  ( 0.03411923929626541063, 1.063910482648552369, -2.873164143118426495 ) ) ;
#22349 = CARTESIAN_POINT ( 'NONE',  ( 0.8464566929133866546, -0.5400638737290844871, 0.3530559997133364547 ) ) ;
#22350 = CARTESIAN_POINT ( 'NONE',  ( 1.227034120734908917, 0.1771653543307087075, -0.09757992244046823083 ) ) ;
#22351 = VERTEX_POINT ( 'NONE', #39745 ) ;
#22352 = CARTESIAN_POINT ( 'NONE',  ( -0.3392501089628017219, -0.1958661417322836995, -2.726397268537744445 ) ) ;
#22353 = CARTESIAN_POINT ( 'NONE',  ( -0.5971128608923877978, -0.6692913385826773087, -0.1292274648535924053 ) ) ;
#22354 = EDGE_LOOP ( 'NONE', ( #27015, #43188, #61, #78956 ) ) ;
#22356 = AXIS2_PLACEMENT_3D ( 'NONE', #50713, #76412, #58694 ) ;
#22355 = CARTESIAN_POINT ( 'NONE',  ( 0.2034120734908142214, 0.1771653543307087075, -0.09757992244046823083 ) ) ;
#22357 = CARTESIAN_POINT ( 'NONE',  ( -0.9842519685039365918, -0.6692913385826771977, 8.415575281601705876E-17 ) ) ;
#22358 = CARTESIAN_POINT ( 'NONE',  ( 0.8005249343832027131, 0.05413385826771666132, 0.4176697321401328100 ) ) ;
#22359 = CARTESIAN_POINT ( 'NONE',  ( 0.9120734908136489683, -0.6692913385826771977, 0.1292274648535927661 ) ) ;
#22360 = CARTESIAN_POINT ( 'NONE',  ( -0.1968503937007867743, -0.6692913385826771977, 8.415575281601705876E-17 ) ) ;
#22361 = CARTESIAN_POINT ( 'NONE',  ( 0.3392501089628018884, -0.1958661417322833942, -1.361567872212285257 ) ) ;
#22362 = CARTESIAN_POINT ( 'NONE',  ( -0.8464566929133852113, 0.1660481256975885056, 0.3530559997133364547 ) ) ;
#22363 = CARTESIAN_POINT ( 'NONE',  ( 0.3392501089628018884, -0.1958661417322834220, -2.079396325459317740 ) ) ;
#22364 = CARTESIAN_POINT ( 'NONE',  ( -1.601049868766403650, -0.6046776061558807314, 0.2411417322834647770 ) ) ;
#22365 = CARTESIAN_POINT ( 'NONE',  ( -0.6824146981627288167, 0.2306618581243848609, 0.2411417322834645549 ) ) ;
#22366 = CARTESIAN_POINT ( 'NONE',  ( -0.4855643044619415427, -0.004921259842519870586, -0.3153832671262229437 ) ) ;
#22367 = CARTESIAN_POINT ( 'NONE',  ( 1.391076115485564868, 0.2306618581243847221, -0.2411417322834647770 ) ) ;
#22368 = CARTESIAN_POINT ( 'NONE',  ( 1.673228346456693494, 0.1660481256975885056, 0.3530559997133364547 ) ) ;
#22369 = CARTESIAN_POINT ( 'NONE',  ( -1.095800524934382292, -0.05778040916215522460, 0.4822834645669289988 ) ) ;
#22370 = CARTESIAN_POINT ( 'NONE',  ( -0.3996062992125984925, -0.1070741851644056858, 0.1922572178477690297 ) ) ;
#22371 = CARTESIAN_POINT ( 'NONE',  ( 0.8333333333333340365, 0.2952755905511810774, -0.1292274648535930714 ) ) ;
#22372 = CARTESIAN_POINT ( 'NONE',  ( -0.2925321140481930704, -0.2925321140481933480, -1.948818897637795144 ) ) ;
#22373 = CARTESIAN_POINT ( 'NONE',  ( 1.586052503253845503, 1.023622047244095556, 0.1653254495020588799 ) ) ;
#22374 = CARTESIAN_POINT ( 'NONE',  ( -0.1246719160104980823, -0.6692913385826773087, -0.1292274648535924053 ) ) ;
#22375 = CARTESIAN_POINT ( 'NONE',  ( -0.9514435695538050464, -0.08942795157528024563, -0.3641732283464568787 ) ) ;
#22376 = CARTESIAN_POINT ( 'NONE',  ( 0.4068241469816281097, -0.004921259842519576551, 0.3153832671262227771 ) ) ;
#22377 = CARTESIAN_POINT ( 'NONE',  ( 0.2362204724409449064, 0.4091458600556404646, -0.5360892388451443669 ) ) ;
#22378 = CARTESIAN_POINT ( 'NONE',  ( 1.089238845144357759, -0.004921259842519870586, -0.3153832671262229437 ) ) ;
#22379 = B_SPLINE_CURVE_WITH_KNOTS ( 'NONE', 3,
 ( #61346, #21398, #27707, #47880 ),
 .UNSPECIFIED., .F., .F.,
 ( 4, 4 ),
 ( 0.1658669167714240389, 0.1672512987629738990 ),
 .UNSPECIFIED. ) ;
#22380 = CARTESIAN_POINT ( 'NONE',  ( 0.9055118110236227702, -0.6692913385826771977, 8.415575281601705876E-17 ) ) ;
#22381 = CARTESIAN_POINT ( 'NONE',  ( 4.837279021331061486E-17, -0.3949938075777409963, -0.6279527559055118058 ) ) ;
#22382 = CARTESIAN_POINT ( 'NONE',  ( -0.5314960629921254842, -0.5400638737290845981, -0.3530559997133363437 ) ) ;
#22383 = FACE_OUTER_BOUND ( 'NONE', #59815, .T. ) ;
#22384 = CARTESIAN_POINT ( 'NONE',  ( 1.233595800524935227, -0.5023911411419708095, 0.1820866141732285504 ) ) ;
#22385 = CARTESIAN_POINT ( 'NONE',  ( -0.5643044619422565855, 0.05413385826771626580, -0.4176697321401330321 ) ) ;
#22386 = CARTESIAN_POINT ( 'NONE',  ( -0.1974969037888706924, 0.3420746716998658843, -0.5623359580052492701 ) ) ;
#22387 = CARTESIAN_POINT ( 'NONE',  ( 1.108923884514436686, -0.3162353388693409650, -0.4822834645669289433 ) ) ;
#22388 = CARTESIAN_POINT ( 'NONE',  ( 5.463695987328526437E-16, -0.1870078740157479769, 0.4822834645669291653 ) ) ;
#22389 = CARTESIAN_POINT ( 'NONE',  ( 0.5511811023622055217, -0.1870078740157479769, 0.3641732283464567677 ) ) ;
#22390 = CARTESIAN_POINT ( 'NONE',  ( -0.2774512451045073602, 1.152276239669946856, -1.087282494290732870 ) ) ;
#22391 = CARTESIAN_POINT ( 'NONE',  ( 0.5052493438320218022, -0.5511811023622048555, -0.09757992244046775898 ) ) ;
#22392 = CARTESIAN_POINT ( 'NONE',  ( 0.000000000000000000, 2.559055118110236560, 0.000000000000000000 ) ) ;
#22393 = EDGE_CURVE ( 'NONE', #43641, #70804, #15642, .T. ) ;
#22394 = CARTESIAN_POINT ( 'NONE',  ( -9.787531504996566615E-17, 0.3996062992125985480, -1.179133858267716661 ) ) ;
#22395 = CARTESIAN_POINT ( 'NONE',  ( 0.6430446194225729606, -0.4281496062992127816, -0.4176697321401328100 ) ) ;
#22396 = VECTOR ( 'NONE', #61716, 39.37007874015748143 ) ;
#22397 = CARTESIAN_POINT ( 'NONE',  ( 0.2867679344610365999, 0.2867679344610365999, -1.074803149606299080 ) ) ;
#22398 = AXIS2_PLACEMENT_3D ( 'NONE', #23363, #54515, #54097 ) ;
#22399 = CARTESIAN_POINT ( 'NONE',  ( -0.4724409448818898682, 5.785732909357575061E-17, -2.755905511811024056 ) ) ;
#22400 = CARTESIAN_POINT ( 'NONE',  ( -0.2955417804206763588, 0.2579773093944630613, -1.506228638669166960E-17 ) ) ;
#22401 = CARTESIAN_POINT ( 'NONE',  ( 0.1443569553805781891, -0.3690944881889763329, 0.3153832671262228327 ) ) ;
#22402 = CARTESIAN_POINT ( 'NONE',  ( 8.195543980992789655E-16, -0.1870078740157480879, -0.4822834645669291653 ) ) ;
#22403 = CARTESIAN_POINT ( 'NONE',  ( 1.502624671916010790, -0.08942795157527998196, 0.3641732283464567121 ) ) ;
#22404 = CARTESIAN_POINT ( 'NONE',  ( -1.207349081364828880, 0.1283753931104746893, -0.1820866141732285504 ) ) ;
#22405 = CARTESIAN_POINT ( 'NONE',  ( -1.541994750656167090, 0.2952755905511811885, 0.1292274648535926551 ) ) ;
#22406 = CARTESIAN_POINT ( 'NONE',  ( 0.4068241469816281097, 0.05413385826771666132, 0.4176697321401328100 ) ) ;
#22407 = CARTESIAN_POINT ( 'NONE',  ( 1.135170603674541256, -0.6692913385826773087, -0.1292274648535924053 ) ) ;
#22408 = EDGE_CURVE ( 'NONE', #47922, #21629, #12156, .T. ) ;
#22409 = CARTESIAN_POINT ( 'NONE',  ( -0.02865809819635581693, 1.063823086577868615, -1.634058138423551076 ) ) ;
#22410 = CARTESIAN_POINT ( 'NONE',  ( 0.3937007874015754361, -0.1870078740157480879, -0.4822834645669291653 ) ) ;
#22411 = CARTESIAN_POINT ( 'NONE',  ( 1.332020997375329197, -0.3162353388693405765, 0.4822834645669290543 ) ) ;
#22412 = CARTESIAN_POINT ( 'NONE',  ( 1.128608923884515169, -0.6046776061558809534, -0.2411417322834644161 ) ) ;
#22413 = CARTESIAN_POINT ( 'NONE',  ( 1.003937007874016407, -0.4536011799217367080, 0.2665933059059888421 ) ) ;
#22414 = CARTESIAN_POINT ( 'NONE',  ( 1.535433070866142558, 0.2952755905511811885, 0.000000000000000000 ) ) ;
#22415 = CARTESIAN_POINT ( 'NONE',  ( -0.9383202099737524282, -0.2845877964562161244, -0.3641732283464567121 ) ) ;
#22416 = CARTESIAN_POINT ( 'NONE',  ( 0.5118110236220478892, 0.1771653543307087630, 0.000000000000000000 ) ) ;
#22417 = CARTESIAN_POINT ( 'NONE',  ( 0.2165354330708668673, -0.5400638737290844871, 0.3530559997133364547 ) ) ;
#22418 = CARTESIAN_POINT ( 'NONE',  ( 0.6299212598425204535, -0.1870078740157479769, 0.4822834645669291653 ) ) ;
#22419 = CARTESIAN_POINT ( 'NONE',  ( -0.3149606299212590610, -0.1870078740157480879, -0.4822834645669291653 ) ) ;
#22420 = CARTESIAN_POINT ( 'NONE',  ( 0.1640419947506569498, -0.08942795157527998196, 0.3641732283464567121 ) ) ;
#22421 = CARTESIAN_POINT ( 'NONE',  ( 0.7611548556430451917, -0.6046776061558807314, 0.2411417322834647770 ) ) ;
#22422 = CARTESIAN_POINT ( 'NONE',  ( 0.000000000000000000, 2.755905511811024056, 0.000000000000000000 ) ) ;
#22423 = CARTESIAN_POINT ( 'NONE',  ( -0.9514435695538050464, -0.3162353388693405765, 0.4822834645669290543 ) ) ;
#22425 = CARTESIAN_POINT ( 'NONE',  ( -0.3460692066303960868, 0.1998031496062990242, -0.6561679790026246906 ) ) ;
#22424 = CARTESIAN_POINT ( 'NONE',  ( -1.069553805774277722, 0.2952755905511811885, 0.1292274648535926551 ) ) ;
#22426 = CARTESIAN_POINT ( 'NONE',  ( 2.161121219943137106, 1.597527518877484676, -0.4706608522957222984 ) ) ;
#22427 = CARTESIAN_POINT ( 'NONE',  ( -0.8464566929133852113, 0.1660481256975885056, 0.3530559997133364547 ) ) ;
#22428 = CARTESIAN_POINT ( 'NONE',  ( -0.6496062992125976043, -0.5400638737290844871, 0.3530559997133364547 ) ) ;
#22429 = CARTESIAN_POINT ( 'NONE',  ( -0.4091458600556405756, 0.2362204724409446288, -0.02624671916010498651 ) ) ;
#22430 = CARTESIAN_POINT ( 'NONE',  ( 0.3949938075777411073, -0.1058382717557499464, -2.158792650918635481 ) ) ;
#22431 = VERTEX_POINT ( 'NONE', #21222 ) ;
#22432 = CARTESIAN_POINT ( 'NONE',  ( 0.5774278215223104249, 0.1283753931104748280, 0.1820866141732283561 ) ) ;
#22433 = CARTESIAN_POINT ( 'NONE',  ( -0.2867679344610364334, -0.2867679344610367109, -0.8385826771653541734 ) ) ;
#22434 = CARTESIAN_POINT ( 'NONE',  ( 1.082677165354331228, -0.5400638737290844871, 0.3530559997133364547 ) ) ;
#22435 = CARTESIAN_POINT ( 'NONE',  ( -0.2477166185931099773, 5.952911114587291371E-15, -0.3791483426435156012 ) ) ;
#22436 = CARTESIAN_POINT ( 'NONE',  ( -1.410761154855642463, -0.08942795157527998196, 0.3641732283464567121 ) ) ;
#22437 = CARTESIAN_POINT ( 'NONE',  ( 1.502624671916010790, -0.05778040916215522460, 0.4822834645669289988 ) ) ;
#22438 = CARTESIAN_POINT ( 'NONE',  ( -1.561679790026246017, 0.05413385826771666132, 0.4176697321401328100 ) ) ;
#22439 = CARTESIAN_POINT ( 'NONE',  ( 0.2887139107611556010, 0.2306618581243847221, -0.2411417322834647770 ) ) ;
#22440 = CIRCLE ( 'NONE', #54691, 0.09842519685039365085 ) ;
#22441 = CARTESIAN_POINT ( 'NONE',  ( -0.3917322834645669549, -7.196005306013483243E-17, -0.1194032563966385962 ) ) ;
#22442 = CARTESIAN_POINT ( 'NONE',  ( -0.05905511811023545637, 0.1660481256975885056, 0.3530559997133364547 ) ) ;
#22443 = CARTESIAN_POINT ( 'NONE',  ( -0.8858267716535425107, 0.07958543189024071263, -0.2665933059059888421 ) ) ;
#22444 = CARTESIAN_POINT ( 'NONE',  ( 0.9776902887139113929, 0.2952755905511811885, 0.1292274648535926551 ) ) ;
#22445 = CARTESIAN_POINT ( 'NONE',  ( -0.03937007874015669567, -0.6692913385826771977, 8.415575281601705876E-17 ) ) ;
#22446 = VECTOR ( 'NONE', #56333, 39.37007874015748143 ) ;
#22447 = CARTESIAN_POINT ( 'NONE',  ( -0.4724409448818898682, -8.678599364036362592E-17, -0.5118110236220472231 ) ) ;
#22448 = CARTESIAN_POINT ( 'NONE',  ( 0.1958661417322834775, 0.3392501089628018884, -1.715898580873702617 ) ) ;
#22449 = CARTESIAN_POINT ( 'NONE',  ( 0.6561679790026253567, -0.6046776061558809534, -0.2411417322834644161 ) ) ;
#22450 = AXIS2_PLACEMENT_3D ( 'NONE', #18220, #44268, #5574 ) ;
#22451 = CARTESIAN_POINT ( 'NONE',  ( 0.1509186351706042484, -0.3162353388693405765, 0.4822834645669290543 ) ) ;
#22452 = CARTESIAN_POINT ( 'NONE',  ( -0.8923884514435688198, -0.6046776061558807314, 0.2411417322834647770 ) ) ;
#22453 = EDGE_CURVE ( 'NONE', #36503, #68098, #42459, .T. ) ;
#22454 = CARTESIAN_POINT ( 'NONE',  ( 1.220472440944882386, -0.6692913385826771977, 8.415575281601705876E-17 ) ) ;
#22455 = CARTESIAN_POINT ( 'NONE',  ( 0.5052493438320218022, -0.6692913385826773087, -0.1292274648535924053 ) ) ;
#22456 = CARTESIAN_POINT ( 'NONE',  ( -0.1958661417322836718, 0.3392501089628017219, -1.042650918635170676 ) ) ;
#22457 = CARTESIAN_POINT ( 'NONE',  ( -0.3674540682414692561, -0.6046776061558809534, -0.2411417322834644161 ) ) ;
#22458 = CARTESIAN_POINT ( 'NONE',  ( 0.8202099737532814183, -0.6692913385826773087, -0.1292274648535924053 ) ) ;
#22459 = CARTESIAN_POINT ( 'NONE',  ( 0.1771653543307093182, -0.5400638737290845981, -0.3530559997133363437 ) ) ;
#22460 = ADVANCED_FACE ( 'NONE', ( #9017 ), #59932, .F. ) ;
#22461 = CARTESIAN_POINT ( 'NONE',  ( 0.7414698162729663755, 0.1771653543307087630, 0.09757992244046791164 ) ) ;
#22462 = CARTESIAN_POINT ( 'NONE',  ( -1.305774278215222184, -0.6692913385826773087, -0.1292274648535924053 ) ) ;
#22463 = CARTESIAN_POINT ( 'NONE',  ( -0.06838555148300114184, 1.067631514832608319, -2.869717892578235841 ) ) ;
#22464 = CARTESIAN_POINT ( 'NONE',  ( 0.4593175853018379162, -0.4281496062992124485, 0.4176697321401328655 ) ) ;
#22465 = CARTESIAN_POINT ( 'NONE',  ( -0.1049643490035307020, 0.3917322834645669549, -2.518372703412073754 ) ) ;
#22466 = ORIENTED_EDGE ( 'NONE', *, *, #39648, .T. ) ;
#22467 = ORIENTED_EDGE ( 'NONE', *, *, #31058, .T. ) ;
#22468 = CARTESIAN_POINT ( 'NONE',  ( 1.010498687664042716, -0.4281496062992124485, 0.4176697321401328655 ) ) ;
#22469 = CARTESIAN_POINT ( 'NONE',  ( 0.6364829396325465405, -0.08942795157527998196, 0.3641732283464567121 ) ) ;
#22471 = CARTESIAN_POINT ( 'NONE',  ( 0.4724409448818898682, 2.892866454678787531E-17, -2.399606299212598604 ) ) ;
#22470 = DIRECTION ( 'NONE',  ( -1.000000000000000000, -0.000000000000000000, -0.000000000000000000 ) ) ;
#22472 = CARTESIAN_POINT ( 'NONE',  ( 0.1438724767639566193, -0.4624630002188719891, -0.005627570198504299945 ) ) ;
#22473 = CARTESIAN_POINT ( 'NONE',  ( -9.594673741351313045E-17, 0.3917322834645670104, -1.344488188976378007 ) ) ;
#22474 = CARTESIAN_POINT ( 'NONE',  ( 0.3996062992125984925, 0.1070741851644054637, -2.406167979002624246 ) ) ;
#22475 = CARTESIAN_POINT ( 'NONE',  ( -0.6561679790026240244, 0.2306618581243847221, -0.2411417322834647770 ) ) ;
#22476 = CARTESIAN_POINT ( 'NONE',  ( -0.7677165354330699465, 0.1660481256975885056, 0.3530559997133364547 ) ) ;
#22477 = CARTESIAN_POINT ( 'NONE',  ( 0.5118110236220478892, 0.2952755905511811885, 0.000000000000000000 ) ) ;
#22478 = ORIENTED_EDGE ( 'NONE', *, *, #29420, .T. ) ;
#22479 = CARTESIAN_POINT ( 'NONE',  ( 1.299212598425197429, 0.2952755905511811885, 0.000000000000000000 ) ) ;
#22480 = CARTESIAN_POINT ( 'NONE',  ( 1.653543307086614789, -0.1870078740157479769, 0.3641732283464567677 ) ) ;
#22481 = CARTESIAN_POINT ( 'NONE',  ( 1.640419947506562393, -0.3690944881889763329, 0.3153832671262228327 ) ) ;
#22482 = CARTESIAN_POINT ( 'NONE',  ( -0.3460692066303957537, -0.1998031496062994405, -2.019028871391076230 ) ) ;
#22483 = CARTESIAN_POINT ( 'NONE',  ( -1.227034120734907141, -0.5511811023622048555, -0.09757992244046775898 ) ) ;
#22484 = CARTESIAN_POINT ( 'NONE',  ( 0.2867679344610365999, -0.2867679344610365444, 0.06692913385826775030 ) ) ;
#22485 = CARTESIAN_POINT ( 'NONE',  ( 0.3674540682414705883, -0.6046776061558807314, 0.2411417322834647770 ) ) ;
#22487 = DIRECTION ( 'NONE',  ( 0.000000000000000000, -0.000000000000000000, 1.000000000000000000 ) ) ;
#22486 = CARTESIAN_POINT ( 'NONE',  ( 1.364829396325460076, 0.2306618581243848609, 0.2411417322834645549 ) ) ;
#22488 = CARTESIAN_POINT ( 'NONE',  ( -1.325459317585300889, -0.3690944881889765550, -0.3153832671262227771 ) ) ;
#22489 =( BOUNDED_CURVE ( )  B_SPLINE_CURVE ( 2, ( #72475, #53088, #71220, #27427, #46364, #1360, #27012 ),
 .UNSPECIFIED., .F., .F. ) 
 B_SPLINE_CURVE_WITH_KNOTS ( ( 3, 2, 2, 3 ),
 ( 0.8096947309984371399, 0.8106060606060605522, 0.8143939393939394478, 0.8181818181818182323 ),
 .UNSPECIFIED. ) 
 CURVE ( )  GEOMETRIC_REPRESENTATION_ITEM ( )  RATIONAL_B_SPLINE_CURVE ( ( 0.9875488213027523443, 0.9918020599134680371, 1.000000000000000000, 0.9659258262890683122, 1.000000000000000000, 0.9659258262890683122, 1.000000000000000000 ) ) 
 REPRESENTATION_ITEM ( '' )  );
#22490 = CARTESIAN_POINT ( 'NONE',  ( 0.4461942257217856311, 0.2306618581243847221, -0.2411417322834647770 ) ) ;
#22491 = CARTESIAN_POINT ( 'NONE',  ( 1.345144356955381593, -0.2845877964562161244, -0.3641732283464567121 ) ) ;
#22492 = CARTESIAN_POINT ( 'NONE',  ( -0.3917322834645669549, -7.196005306013483243E-17, -1.379245776081677866 ) ) ;
#22493 = CARTESIAN_POINT ( 'NONE',  ( -1.076115485564303809, 0.1283753931104748280, 0.1820866141732283561 ) ) ;
#22494 = CARTESIAN_POINT ( 'NONE',  ( 1.266404199475066328, -0.3162353388693409650, -0.4822834645669289433 ) ) ;
#22495 = CARTESIAN_POINT ( 'NONE',  ( -0.4724409448818898682, -8.678599364036362592E-17, -2.635826771653543066 ) ) ;
#22496 = CARTESIAN_POINT ( 'NONE',  ( -0.1377952755905504645, 0.1660481256975885056, 0.3530559997133364547 ) ) ;
#22497 = CARTESIAN_POINT ( 'NONE',  ( -1.502624671916009680, -0.2845877964562159024, 0.3641732283464567677 ) ) ;
#22498 = CARTESIAN_POINT ( 'NONE',  ( -0.4396325459317579898, 0.1771653543307087630, 0.09757992244046791164 ) ) ;
#22499 = CARTESIAN_POINT ( 'NONE',  ( -0.8136482939632537770, -0.6046776061558807314, 0.2411417322834647770 ) ) ;
#22500 = CARTESIAN_POINT ( 'NONE',  ( -1.633858267716534529, 0.07958543189024085140, 0.2665933059059887866 ) ) ;
#22501 = CARTESIAN_POINT ( 'NONE',  ( -0.3917322834645670659, -7.196005306013484475E-17, -0.3510691845482433182 ) ) ;
#22502 = CARTESIAN_POINT ( 'NONE',  ( 0.3018372703412079971, -0.4281496062992124485, 0.4176697321401328655 ) ) ;
#22503 = AXIS2_PLACEMENT_3D ( 'NONE', #51887, #71268, #26650 ) ;
#22504 = CARTESIAN_POINT ( 'NONE',  ( 1.141392835773559211, 0.3937007874015747699, 0.9435581901042713326 ) ) ;
#22505 = AXIS2_PLACEMENT_3D ( 'NONE', #79608, #40045, #4623 ) ;
#22506 = CARTESIAN_POINT ( 'NONE',  ( -0.3458507752293906723, -0.3458507752293910609, -1.553149606299212726 ) ) ;
#22507 = CARTESIAN_POINT ( 'NONE',  ( -1.364829396325458521, 0.2306618581243847221, -0.2411417322834647770 ) ) ;
#22508 = CARTESIAN_POINT ( 'NONE',  ( -0.8136482939632537770, -0.5023911411419708095, 0.1820866141732285504 ) ) ;
#22509 = CYLINDRICAL_SURFACE ( 'NONE', #78372, 0.4822834645669291653 ) ;
#22510 = CARTESIAN_POINT ( 'NONE',  ( -0.03937007874015669567, 0.2952755905511811885, 0.000000000000000000 ) ) ;
#22511 = CARTESIAN_POINT ( 'NONE',  ( 0.3083989501312343062, -0.08942795157528024563, -0.3641732283464568787 ) ) ;
#22512 = CARTESIAN_POINT ( 'NONE',  ( -0.7152230971128602510, -0.08942795157528024563, -0.3641732283464568787 ) ) ;
#22513 = CARTESIAN_POINT ( 'NONE',  ( -1.601049868766403650, -0.6046776061558807314, 0.2411417322834647770 ) ) ;
#22514 = CARTESIAN_POINT ( 'NONE',  ( -1.620734908136482577, -0.6692913385826773087, -0.1292274648535924053 ) ) ;
#22515 = CARTESIAN_POINT ( 'NONE',  ( 1.371391076115485941, 0.2952755905511811885, 0.1292274648535926551 ) ) ;
#22516 = CARTESIAN_POINT ( 'NONE',  ( 0.008542603271838917003, 1.062992125984252745, 1.850393700787401619 ) ) ;
#22517 = CARTESIAN_POINT ( 'NONE',  ( 0.9580052493438327987, -0.3690944881889765550, -0.3153832671262227771 ) ) ;
#22518 = CARTESIAN_POINT ( 'NONE',  ( 0.8923884514435703741, 0.2306618581243848609, 0.2411417322834645549 ) ) ;
#22519 = CARTESIAN_POINT ( 'NONE',  ( 1.568241469816273437, -0.2845877964562159024, 0.3641732283464567677 ) ) ;
#22520 = EDGE_LOOP ( 'NONE', ( #45321, #71370, #51682, #10540, #44365, #19751, #14589 ) ) ;
#22521 = CARTESIAN_POINT ( 'NONE',  ( -1.220472440944881054, -0.6692913385826771977, 8.415575281601705876E-17 ) ) ;
#22522 = CARTESIAN_POINT ( 'NONE',  ( -0.9317585301837263412, -0.4281496062992127816, -0.4176697321401328100 ) ) ;
#22523 = CARTESIAN_POINT ( 'NONE',  ( 0.2887139107611556010, -0.6046776061558807314, 0.2411417322834647770 ) ) ;
#22524 = CARTESIAN_POINT ( 'NONE',  ( -1.318897637795274802, -0.4536011799217368745, -0.2665933059059886201 ) ) ;
#22525 = CARTESIAN_POINT ( 'NONE',  ( -0.3996062992125984925, -0.1070741851644056858, -2.327427821522309870 ) ) ;
#22526 = CARTESIAN_POINT ( 'NONE',  ( 1.351706036745407458, -0.3690944881889765550, -0.3153832671262227771 ) ) ;
#22527 = CARTESIAN_POINT ( 'NONE',  ( 0.4330708661417329575, 0.2952755905511811885, 0.000000000000000000 ) ) ;
#22528 = CARTESIAN_POINT ( 'NONE',  ( 0.7808398950131240079, -0.3162353388693405765, 0.4822834645669290543 ) ) ;
#22529 = B_SPLINE_CURVE_WITH_KNOTS ( 'NONE', 3,
 ( #61805, #24320, #30224, #4554 ),
 .UNSPECIFIED., .F., .F.,
 ( 4, 4 ),
 ( 3.593986969179100008E-07, 0.001287825409103298150 ),
 .UNSPECIFIED. ) ;
#22530 = CARTESIAN_POINT ( 'NONE',  ( 1.666666666666667185, 0.05413385826771666132, 0.4176697321401328100 ) ) ;
#22531 = CARTESIAN_POINT ( 'NONE',  ( 0.3460692066303959202, 0.1998031496062993295, -1.706036745406824151 ) ) ;
#22532 = CARTESIAN_POINT ( 'NONE',  ( -0.1974969037888706647, 0.3420746716998658843, -1.272965879265091749 ) ) ;
#22533 = CARTESIAN_POINT ( 'NONE',  ( 4.893765752498283924E-17, -0.3996062992125986035, -2.440944881889763884 ) ) ;
#22534 = CARTESIAN_POINT ( 'NONE',  ( -0.7443564562302430465, 1.971400176305090124, -0.5309055118110235227 ) ) ;
#22535 = CARTESIAN_POINT ( 'NONE',  ( -0.1958661417322834220, -0.3392501089628018884, -0.2152230971128608339 ) ) ;
#22536 = CARTESIAN_POINT ( 'NONE',  ( 0.09842519685039434474, -0.4536011799217368745, -0.2665933059059886201 ) ) ;
#22537 = CARTESIAN_POINT ( 'NONE',  ( -0.4593175853018366950, 0.05413385826771666132, 0.4176697321401328100 ) ) ;
#22538 = CARTESIAN_POINT ( 'NONE',  ( 0.8267716535433077274, 0.2952755905511811885, 0.000000000000000000 ) ) ;
#22539 = CARTESIAN_POINT ( 'NONE',  ( 0.3420746716998660508, 0.1974969037888705814, -2.255249343832021136 ) ) ;
#22540 = CARTESIAN_POINT ( 'NONE',  ( -0.02624671916010428221, 0.1283753931104746893, -0.1820866141732285504 ) ) ;
#22541 = CARTESIAN_POINT ( 'NONE',  ( -1.181102362204723644, -0.1870078740157479769, 0.4822834645669291653 ) ) ;
#22542 = CARTESIAN_POINT ( 'NONE',  ( 1.371391076115485719, -0.6692913385826773087, -0.1292274648535924053 ) ) ;
#22543 = CARTESIAN_POINT ( 'NONE',  ( -0.4724409448818898682, -8.678599364036362592E-17, -2.401574803149606474 ) ) ;
#22544 = CARTESIAN_POINT ( 'NONE',  ( 0.3996062992125986590, -0.1070741851644053111, -1.686351706036745446 ) ) ;
#22545 = CARTESIAN_POINT ( 'NONE',  ( -1.586052503253846169, 1.850393700787402729, -0.1653254495020583803 ) ) ;
#22546 = ORIENTED_EDGE ( 'NONE', *, *, #76757, .F. ) ;
#22547 = EDGE_CURVE ( 'NONE', #34953, #50774, #3113, .T. ) ;
#22548 = VERTEX_POINT ( 'NONE', #52776 ) ;
#22549 = CARTESIAN_POINT ( 'NONE',  ( 1.141732283464567566, 0.2952755905511811885, 0.000000000000000000 ) ) ;
#22550 = CARTESIAN_POINT ( 'NONE',  ( -1.581364829396324945, -0.3162353388693405765, 0.4822834645669290543 ) ) ;
#22552 = CARTESIAN_POINT ( 'NONE',  ( -1.555118110236219930, -0.5400638737290845981, -0.3530559997133363437 ) ) ;
#22551 = CARTESIAN_POINT ( 'NONE',  ( -1.200787401574802349, -0.4536011799217367080, 0.2665933059059888421 ) ) ;
#22553 = CARTESIAN_POINT ( 'NONE',  ( 0.3392501089628018329, -0.1958661417322834497, -2.862185408627609728 ) ) ;
#22554 = LINE ( 'NONE', #22137, #8774 ) ;
#22555 = CARTESIAN_POINT ( 'NONE',  ( 1.404199475065617708, 0.05413385826771626580, -0.4176697321401330321 ) ) ;
#22556 = CARTESIAN_POINT ( 'NONE',  ( -1.686351706036744558, 0.2952755905511810774, -0.1292274648535930714 ) ) ;
#22557 = CARTESIAN_POINT ( 'NONE',  ( 0.006561679790026889343, -0.05778040916215522460, 0.4822834645669289988 ) ) ;
#22558 = CARTESIAN_POINT ( 'NONE',  ( -0.6955380577427815458, -0.4281496062992127816, -0.4176697321401328100 ) ) ;
#22559 = CARTESIAN_POINT ( 'NONE',  ( -1.646981627296586703, -0.05778040916215522460, 0.4822834645669289988 ) ) ;
#22560 = CARTESIAN_POINT ( 'NONE',  ( 0.2867679344610365999, 0.2867679344610365999, -0.06496062992125994917 ) ) ;
#22561 = CARTESIAN_POINT ( 'NONE',  ( 0.1115485564304467270, -0.6692913385826773087, -0.1292274648535924053 ) ) ;
#22562 = AXIS2_PLACEMENT_3D ( 'NONE', #42196, #15725, #61566 ) ;
#22563 = CARTESIAN_POINT ( 'NONE',  ( -0.3917322834645669549, -0.1049643490035306603, -2.085301837270341352 ) ) ;
#22564 = CARTESIAN_POINT ( 'NONE',  ( -1.095800524934382292, -0.2845877964562161244, -0.3641732283464567121 ) ) ;
#22565 = ORIENTED_EDGE ( 'NONE', *, *, #30606, .F. ) ;
#22566 = CARTESIAN_POINT ( 'NONE',  ( 0.3949938075777409408, 0.1058382717557500574, -2.329396325459317740 ) ) ;
#22567 = ORIENTED_EDGE ( 'NONE', *, *, #71288, .T. ) ;
#22568 = CARTESIAN_POINT ( 'NONE',  ( -0.6399301791983041943, -2.567464376874931580E-15, -0.4445507791589072832 ) ) ;
#22569 = AXIS2_PLACEMENT_3D ( 'NONE', #48798, #54704, #47974 ) ;
#22570 = CARTESIAN_POINT ( 'NONE',  ( -1.653543307086613234, -0.1870078740157480879, -0.4822834645669291653 ) ) ;
#22571 = CARTESIAN_POINT ( 'NONE',  ( 0.3996062992125986590, -0.1070741851644053111, -1.056430446194225992 ) ) ;
#22572 = DIRECTION ( 'NONE',  ( 1.000000000000000000, 3.096699300667737957E-16, -1.692413147294446216E-16 ) ) ;
#22573 = CARTESIAN_POINT ( 'NONE',  ( -1.692913385826770645, 0.2952755905511811885, 0.000000000000000000 ) ) ;
#22574 = LINE ( 'NONE', #34794, #71925 ) ;
#22575 = CARTESIAN_POINT ( 'NONE',  ( 0.1958661417322836440, -0.3392501089628017219, 0.1384514435695537171 ) ) ;
#22576 = CARTESIAN_POINT ( 'NONE',  ( -0.4986876640419939388, 0.1283753931104746893, -0.1820866141732285504 ) ) ;
#22577 = CARTESIAN_POINT ( 'NONE',  ( -0.7480314960629914633, 0.1771653543307087630, 0.000000000000000000 ) ) ;
#22578 = CARTESIAN_POINT ( 'NONE',  ( -1.391076115485563314, -0.6046776061558809534, -0.2411417322834644161 ) ) ;
#22579 = CARTESIAN_POINT ( 'NONE',  ( 0.6561679790026253567, 0.2306618581243848609, 0.2411417322834645549 ) ) ;
#22580 = CARTESIAN_POINT ( 'NONE',  ( -1.332020997375327642, -0.05778040916215522460, 0.4822834645669289988 ) ) ;
#22581 = CARTESIAN_POINT ( 'NONE',  ( -0.2867679344610364334, -0.2867679344610367109, 0.1062992125984252439 ) ) ;
#22582 = ORIENTED_EDGE ( 'NONE', *, *, #5358, .F. ) ;
#22583 = CARTESIAN_POINT ( 'NONE',  ( -1.377952755905511140, -0.6692913385826771977, 8.415575281601705876E-17 ) ) ;
#22584 = CARTESIAN_POINT ( 'NONE',  ( -0.2087913723976026203, -0.2087913723976025926, 0.1248231986745540339 ) ) ;
#22585 = CARTESIAN_POINT ( 'NONE',  ( 0.2362204724409449064, 0.4091458600556404646, -1.719160104986876769 ) ) ;
#22586 = CARTESIAN_POINT ( 'NONE',  ( 2.167277156196865118, 1.503024749832830853, -0.4732391302016644152 ) ) ;
#22587 = CARTESIAN_POINT ( 'NONE',  ( -0.1958661417322836718, 0.3392501089628017219, -0.6351706036745405903 ) ) ;
#22588 = CARTESIAN_POINT ( 'NONE',  ( 0.3917322834645669549, 0.1049643490035304660, -2.729002624671915900 ) ) ;
#22589 = CARTESIAN_POINT ( 'NONE',  ( -0.8792650918635160906, -0.4281496062992124485, 0.4176697321401328655 ) ) ;
#22590 = CARTESIAN_POINT ( 'NONE',  ( 1.463254593175853824, -0.6692913385826771977, 0.1292274648535927661 ) ) ;
#22592 = FACE_OUTER_BOUND ( 'NONE', #13342, .T. ) ;
#22591 = CARTESIAN_POINT ( 'NONE',  ( -1.660104986876639543, -0.05778040916215560624, -0.4822834645669293319 ) ) ;
#22593 = CARTESIAN_POINT ( 'NONE',  ( -1.515748031496062076, 0.1660481256975883668, -0.3530559997133364547 ) ) ;
#22594 = CARTESIAN_POINT ( 'NONE',  ( -0.7677165354330699465, 0.1660481256975885056, 0.3530559997133364547 ) ) ;
#22595 = CARTESIAN_POINT ( 'NONE',  ( 0.3917322834645669549, 2.398668435337827645E-17, 0.1168172160443062824 ) ) ;
#22596 = CARTESIAN_POINT ( 'NONE',  ( -0.1574803149606292529, -0.1870078740157479769, 0.3641732283464567677 ) ) ;
#22597 = CARTESIAN_POINT ( 'NONE',  ( 0.1049643490035303689, 0.3917322834645670104, -0.5505249343832021580 ) ) ;
#22598 = CARTESIAN_POINT ( 'NONE',  ( -0.2624671916010490880, -0.5023911411419708095, 0.1820866141732285504 ) ) ;
#22599 = CARTESIAN_POINT ( 'NONE',  ( 0.8923884514435701520, -0.5023911411419708095, -0.1820866141732282451 ) ) ;
#22600 = CARTESIAN_POINT ( 'NONE',  ( 0.7939632545931766261, -0.05778040916215522460, 0.4822834645669289988 ) ) ;
#22601 = UNCERTAINTY_MEASURE_WITH_UNIT (LENGTH_MEASURE( 1.000000000000000082E-05 ), #12933, 'distance_accuracy_value', 'NONE');
#22602 = CARTESIAN_POINT ( 'NONE',  ( -0.2296587926509179312, -0.08942795157527998196, 0.3641732283464567121 ) ) ;
#22603 = CARTESIAN_POINT ( 'NONE',  ( -0.3917322834645670104, -7.196005306013484475E-17, -2.236220472440944906 ) ) ;
#22604 = CARTESIAN_POINT ( 'NONE',  ( 1.384514435695538337, -0.6692913385826771977, 0.1292274648535927661 ) ) ;
#22605 = CARTESIAN_POINT ( 'NONE',  ( -1.345144356955379816, -0.2845877964562159024, 0.3641732283464567677 ) ) ;
#22606 = CARTESIAN_POINT ( 'NONE',  ( -0.4091458600556405756, 0.2362204724409446288, -0.2604986876640419946 ) ) ;
#22607 = CARTESIAN_POINT ( 'NONE',  ( 0.2493438320209980519, -0.4281496062992127816, -0.4176697321401328100 ) ) ;
#22608 = CARTESIAN_POINT ( 'NONE',  ( 0.1115485564304470323, 0.2952755905511811885, 0.1292274648535926551 ) ) ;
#22609 = CARTESIAN_POINT ( 'NONE',  ( 1.496062992125985147, -0.1870078740157479769, 0.3641732283464567677 ) ) ;
#22610 = CARTESIAN_POINT ( 'NONE',  ( 0.4002624671916016896, -0.2845877964562161244, -0.3641732283464567121 ) ) ;
#22611 = CARTESIAN_POINT ( 'NONE',  ( -0.1902887139107604098, -0.5511811023622046335, 0.09757992244046803654 ) ) ;
#22612 = CARTESIAN_POINT ( 'NONE',  ( -0.7349081364829387342, -0.6046776061558807314, 0.2411417322834647770 ) ) ;
#22613 = CARTESIAN_POINT ( 'NONE',  ( 3.224202737261815166, 2.716535433070866645, -0.5314960629921260393 ) ) ;
#22614 = CARTESIAN_POINT ( 'NONE',  ( -0.3458507752293909498, 0.3458507752293908388, -1.986220472440944684 ) ) ;
#22615 = CARTESIAN_POINT ( 'NONE',  ( 0.01968503937007957949, -0.5400638737290845981, -0.3530559997133363437 ) ) ;
#22616 = CARTESIAN_POINT ( 'NONE',  ( -0.1070741851644056997, 0.3996062992125984925, -1.500656167979002031 ) ) ;
#22617 =( BOUNDED_CURVE ( )  B_SPLINE_CURVE ( 3, ( #46888, #32605, #58268, #65452 ),
 .UNSPECIFIED., .F., .F. ) 
 B_SPLINE_CURVE_WITH_KNOTS ( ( 4, 4 ),
 ( 1.506235357477418768, 1.510153102763379218 ),
 .UNSPECIFIED. ) 
 CURVE ( )  GEOMETRIC_REPRESENTATION_ITEM ( )  RATIONAL_B_SPLINE_CURVE ( ( 1.000000000000000000, 0.9999987209397318555, 0.9999987209397318555, 1.000000000000000000 ) ) 
 REPRESENTATION_ITEM ( '' )  );
#22618 = CARTESIAN_POINT ( 'NONE',  ( 1.561679790026247350, -0.4281496062992124485, 0.4176697321401328655 ) ) ;
#22619 = CARTESIAN_POINT ( 'NONE',  ( -0.04593175853018302557, -0.5511811023622048555, -0.09757992244046775898 ) ) ;
#22620 = CARTESIAN_POINT ( 'NONE',  ( -0.1902887139107604098, -0.6692913385826771977, 0.1292274648535927661 ) ) ;
#22621 = CARTESIAN_POINT ( 'NONE',  ( -1.522309711286088607, -0.6046776061558807314, 0.2411417322834647770 ) ) ;
#22622 = CARTESIAN_POINT ( 'NONE',  ( -1.601049868766403650, 0.1283753931104746893, -0.1820866141732285504 ) ) ;
#22623 = CARTESIAN_POINT ( 'NONE',  ( 1.371391076115485941, 0.2952755905511811885, 0.1292274648535926551 ) ) ;
#22624 = DIRECTION ( 'NONE',  ( 0.000000000000000000, 0.000000000000000000, -1.000000000000000000 ) ) ;
#22625 = CARTESIAN_POINT ( 'NONE',  ( -0.5446194225721777693, -0.2845877964562161244, -0.3641732283464567121 ) ) ;
#22626 = CARTESIAN_POINT ( 'NONE',  ( 0.3996062992125985480, -0.1070741851644052972, -0.3458005249343831244 ) ) ;
#22627 = CARTESIAN_POINT ( 'NONE',  ( -9.787531504996567848E-17, 0.3996062992125986035, -0.6299212598425196763 ) ) ;
#22628 = CARTESIAN_POINT ( 'NONE',  ( 4.797336870675656522E-17, -0.3917322834645670659, -2.910124302658479767 ) ) ;
#22629 = CARTESIAN_POINT ( 'NONE',  ( 1.423884514435696413, -0.2845877964562161244, -0.3641732283464567121 ) ) ;
#22630 = CARTESIAN_POINT ( 'NONE',  ( 1.220472440944882386, -0.5511811023622047445, 6.969142054262312111E-17 ) ) ;
#22631 = CARTESIAN_POINT ( 'NONE',  ( -1.515748031496062076, 0.1660481256975883668, -0.3530559997133364547 ) ) ;
#22632 = CARTESIAN_POINT ( 'NONE',  ( 0.8923884514435701520, -0.6046776061558809534, -0.2411417322834644161 ) ) ;
#22633 = CARTESIAN_POINT ( 'NONE',  ( 0.3420746716998660508, -0.1974969037888704149, -0.9691601049868767692 ) ) ;
#22634 = CARTESIAN_POINT ( 'NONE',  ( 1.043307086614173818, 0.07958543189024085140, 0.2665933059059887866 ) ) ;
#22635 = ADVANCED_FACE ( 'NONE', ( #47294 ), #61272, .F. ) ;
#22636 = CARTESIAN_POINT ( 'NONE',  ( 0.1706036745406830368, -0.4281496062992127816, -0.4176697321401328100 ) ) ;
#22637 = CARTESIAN_POINT ( 'NONE',  ( -1.003937007874014853, 0.1660481256975885056, 0.3530559997133364547 ) ) ;
#22638 = CYLINDRICAL_SURFACE ( 'NONE', #65144, 0.5120078740157480990 ) ;
#22639 = CARTESIAN_POINT ( 'NONE',  ( 0.1265901696524990294, -0.4724409448818896462, -1.030183727034120533 ) ) ;
#22640 = CARTESIAN_POINT ( 'NONE',  ( 0.3996062992125986035, 2.446882876249141962E-17, -2.322834645669291209 ) ) ;
#22641 = CARTESIAN_POINT ( 'NONE',  ( 0.3477690288713918276, 0.1771653543307087630, 0.09757992244046791164 ) ) ;
#22642 = VERTEX_POINT ( 'NONE', #34690 ) ;
#22643 = CARTESIAN_POINT ( 'NONE',  ( -0.1049643490035302301, -0.3917322834645671770, -0.2263972685377446670 ) ) ;
#22644 = VERTEX_POINT ( 'NONE', #28778 ) ;
#22645 = EDGE_CURVE ( 'NONE', #1571, #30834, #41411, .T. ) ;
#22646 = CARTESIAN_POINT ( 'NONE',  ( -0.6430446194225716283, -0.4281496062992124485, 0.4176697321401328655 ) ) ;
#22647 = CARTESIAN_POINT ( 'NONE',  ( -0.3674540682414689785, 0.2306618581243848609, 0.2411417322834645549 ) ) ;
#22648 = CARTESIAN_POINT ( 'NONE',  ( -0.5118110236220466680, 0.1771653543307087630, 0.000000000000000000 ) ) ;
#22649 = CARTESIAN_POINT ( 'NONE',  ( 0.8661417322834653598, -0.1870078740157479769, 0.4822834645669291653 ) ) ;
#22650 = CARTESIAN_POINT ( 'NONE',  ( -1.056430446194224881, -0.6692913385826771977, 0.1292274648535927661 ) ) ;
#22651 = CARTESIAN_POINT ( 'NONE',  ( -0.3740157480314953431, -0.5400638737290845981, -0.3530559997133363437 ) ) ;
#22652 = CARTESIAN_POINT ( 'NONE',  ( 1.062992125984252745, -0.6692913385826771977, 8.415575281601705876E-17 ) ) ;
#22653 = CARTESIAN_POINT ( 'NONE',  ( 1.023622047244095112, -0.1870078740157480879, -0.4822834645669291653 ) ) ;
#22654 = CARTESIAN_POINT ( 'NONE',  ( 0.7020997375328090762, -0.3162353388693405765, 0.4822834645669290543 ) ) ;
#22655 = CARTESIAN_POINT ( 'NONE',  ( -0.3917322834645670104, -7.196005306013484475E-17, -1.133858267716535195 ) ) ;
#22656 = CARTESIAN_POINT ( 'NONE',  ( -0.1771653543307080136, 0.07958543189024071263, -0.2665933059059888421 ) ) ;
#22657 = VERTEX_POINT ( 'NONE', #20808 ) ;
#22658 = CARTESIAN_POINT ( 'NONE',  ( -0.3420746716998659953, -0.1974969037888706647, -0.8398950131233596794 ) ) ;
#22659 = ORIENTED_EDGE ( 'NONE', *, *, #22774, .F. ) ;
#22660 = CARTESIAN_POINT ( 'NONE',  ( -0.9251968503937002541, 0.07958543189024085140, 0.2665933059059887866 ) ) ;
#22661 = CARTESIAN_POINT ( 'NONE',  ( -0.6496062992125976043, 0.1660481256975883668, -0.3530559997133364547 ) ) ;
#22662 = LINE ( 'NONE', #55047, #28725 ) ;
#22663 = CARTESIAN_POINT ( 'NONE',  ( -0.4461942257217840213, 0.2306618581243848609, 0.2411417322834645549 ) ) ;
#22664 = CARTESIAN_POINT ( 'NONE',  ( -0.5380577427821514602, -0.4281496062992127816, -0.4176697321401328100 ) ) ;
#22665 = CARTESIAN_POINT ( 'NONE',  ( -1.141732283464566011, 0.2952755905511811885, 0.000000000000000000 ) ) ;
#22666 = CARTESIAN_POINT ( 'NONE',  ( -1.587926509186350810, -0.4281496062992124485, 0.4176697321401328655 ) ) ;
#22667 = CARTESIAN_POINT ( 'NONE',  ( 0.8267716535433078384, -0.5511811023622047445, 6.969142054262312111E-17 ) ) ;
#22668 = LINE ( 'NONE', #48327, #75366 ) ;
#22669 = CARTESIAN_POINT ( 'NONE',  ( 0.4724409448818905899, -0.1265901696524973641, -0.6607611548556431291 ) ) ;
#22670 = CARTESIAN_POINT ( 'NONE',  ( 0.6036745406824153282, -0.5023911411419708095, 0.1820866141732285504 ) ) ;
#22671 = CARTESIAN_POINT ( 'NONE',  ( -0.03280839895013062252, 0.2952755905511810774, -0.1292274648535930714 ) ) ;
#22672 = CARTESIAN_POINT ( 'NONE',  ( 0.4724409448818904789, -0.1870078740157480879, -0.4822834645669291653 ) ) ;
#22673 = VERTEX_POINT ( 'NONE', #33441 ) ;
#22674 = CARTESIAN_POINT ( 'NONE',  ( 0.3460692066303959757, -0.1998031496062991907, -1.679790026246719137 ) ) ;
#22675 = DIRECTION ( 'NONE',  ( 1.000000000000000000, -0.000000000000000000, -0.000000000000000000 ) ) ;
#22676 = ORIENTED_EDGE ( 'NONE', *, *, #71970, .T. ) ;
#22677 = CARTESIAN_POINT ( 'NONE',  ( 0.3996062992125985480, 2.446882876249141654E-17, -1.139763779527559029 ) ) ;
#22678 = CARTESIAN_POINT ( 'NONE',  ( -0.7998211177050861265, -2.609869883881465018E-15, -0.3464511005275220379 ) ) ;
#22679 = CARTESIAN_POINT ( 'NONE',  ( -0.5314960629921254842, -0.4536011799217368745, -0.2665933059059886201 ) ) ;
#22680 = CARTESIAN_POINT ( 'NONE',  ( -1.141732283464566011, -0.6692913385826771977, 8.415575281601705876E-17 ) ) ;
#22681 = CARTESIAN_POINT ( 'NONE',  ( 0.2362204724409449064, 0.4091458600556404646, -0.6167979002624671692 ) ) ;
#22682 = CARTESIAN_POINT ( 'NONE',  ( 0.2867679344610365999, -0.2867679344610365444, -2.545275590551181022 ) ) ;
#22683 = CARTESIAN_POINT ( 'NONE',  ( 1.528871391076116026, 0.2952755905511811885, 0.1292274648535926551 ) ) ;
#22684 = CARTESIAN_POINT ( 'NONE',  ( 1.056430446194226436, -0.6692913385826773087, -0.1292274648535924053 ) ) ;
#22685 = CARTESIAN_POINT ( 'NONE',  ( 0.6955380577427828781, -0.4281496062992124485, 0.4176697321401328655 ) ) ;
#22686 = CARTESIAN_POINT ( 'NONE',  ( -0.6364829396325453192, -0.08942795157528024563, -0.3641732283464568787 ) ) ;
#22687 = CARTESIAN_POINT ( 'NONE',  ( -0.006561679790025524116, -0.3162353388693405765, 0.4822834645669290543 ) ) ;
#22688 = CARTESIAN_POINT ( 'NONE',  ( -0.2362204724409447953, -0.4091458600556404646, -2.189632545931758489 ) ) ;
#22689 = CARTESIAN_POINT ( 'NONE',  ( -0.3083989501312330295, -0.2845877964562161244, -0.3641732283464567121 ) ) ;
#22690 = CARTESIAN_POINT ( 'NONE',  ( -0.3149606299212590610, -0.1870078740157479769, 0.4822834645669291653 ) ) ;
#22691 = CARTESIAN_POINT ( 'NONE',  ( -0.1058382717557497660, -0.3949938075777411073, -1.881233595800524849 ) ) ;
#22692 = CARTESIAN_POINT ( 'NONE',  ( -1.574803149606298636, -0.1870078740157479769, 0.4822834645669291653 ) ) ;
#22693 = CARTESIAN_POINT ( 'NONE',  ( 0.02624671916010564918, 0.1283753931104748280, 0.1820866141732283561 ) ) ;
#22694 = CARTESIAN_POINT ( 'NONE',  ( 1.430446194225722500, -0.3690944881889765550, -0.3153832671262227771 ) ) ;
#22695 = CARTESIAN_POINT ( 'NONE',  ( -1.272965879265091305, -0.4281496062992124485, 0.4176697321401328655 ) ) ;
#22696 = CARTESIAN_POINT ( 'NONE',  ( -0.7611548556430438595, -0.5023911411419708095, -0.1820866141732282451 ) ) ;
#22697 = DIRECTION ( 'NONE',  ( 0.000000000000000000, 0.000000000000000000, -1.000000000000000000 ) ) ;
#22698 = CARTESIAN_POINT ( 'NONE',  ( -0.9645669291338575535, -0.5400638737290844871, 0.3530559997133364547 ) ) ;
#22699 = CARTESIAN_POINT ( 'NONE',  ( -0.5708661417322825615, -0.5400638737290844871, 0.3530559997133364547 ) ) ;
#22700 = CARTESIAN_POINT ( 'NONE',  ( 0.2493438320209980519, 0.05413385826771666132, 0.4176697321401328100 ) ) ;
#22701 = CARTESIAN_POINT ( 'NONE',  ( -0.1049643490035301746, -0.3917322834645670659, -2.514416379756218678 ) ) ;
#22702 = EDGE_CURVE ( 'NONE', #66965, #54650, #20392, .T. ) ;
#22703 = CARTESIAN_POINT ( 'NONE',  ( -1.867405098639518091, 1.081388112195859508, -0.1351566381869792888 ) ) ;
#22704 = CARTESIAN_POINT ( 'NONE',  ( 0.2755905511811031494, 0.1771653543307087630, 0.000000000000000000 ) ) ;
#22705 = CARTESIAN_POINT ( 'NONE',  ( 0.9580052493438326877, 0.05413385826771666132, 0.4176697321401328100 ) ) ;
#22706 = CARTESIAN_POINT ( 'NONE',  ( -1.148293963254592542, -0.5511811023622048555, -0.09757992244046775898 ) ) ;
#22707 = CARTESIAN_POINT ( 'NONE',  ( 1.174540682414699111, -0.3162353388693405765, 0.4822834645669290543 ) ) ;
#22708 = CARTESIAN_POINT ( 'NONE',  ( -1.719160104986876103, -0.004921259842519576551, 0.3153832671262227771 ) ) ;
#22709 = EDGE_CURVE ( 'NONE', #62412, #50709, #41150, .T. ) ;
#22710 = CARTESIAN_POINT ( 'NONE',  ( -0.4790026246719154557, -0.3162353388693405765, 0.4822834645669290543 ) ) ;
#22711 = CARTESIAN_POINT ( 'NONE',  ( 0.1377952755905518800, 0.07958543189024071263, -0.2665933059059888421 ) ) ;
#22712 = CARTESIAN_POINT ( 'NONE',  ( 0.1265901696524990572, -0.4724409448818897017, -0.8727034120734907807 ) ) ;
#22713 = CARTESIAN_POINT ( 'NONE',  ( 0.7808398950131240079, -0.2845877964562159024, 0.3641732283464567677 ) ) ;
#22714 = CARTESIAN_POINT ( 'NONE',  ( -0.03937007874015669567, 0.2952755905511811885, 0.000000000000000000 ) ) ;
#22715 = CARTESIAN_POINT ( 'NONE',  ( 0.3996062992125986035, -0.1070741851644052972, -0.1883202099737532054 ) ) ;
#22716 = CARTESIAN_POINT ( 'NONE',  ( -0.9251968503937002541, 0.1660481256975885056, 0.3530559997133364547 ) ) ;
#22717 = CARTESIAN_POINT ( 'NONE',  ( 4.797336870675656522E-17, -0.3917322834645670104, -1.738188976377952777 ) ) ;
#22718 = CARTESIAN_POINT ( 'NONE',  ( 0.8989501312335963501, -0.5511811023622048555, -0.09757992244046775898 ) ) ;
#22719 = CARTESIAN_POINT ( 'NONE',  ( -0.09842519685039295696, -0.5400638737290844871, 0.3530559997133364547 ) ) ;
#22720 = CARTESIAN_POINT ( 'NONE',  ( -0.3215223097112853146, -0.05778040916215560624, -0.4822834645669293319 ) ) ;
#22721 = CARTESIAN_POINT ( 'NONE',  ( -0.4330708661417315697, -0.5511811023622047445, 6.969142054262312111E-17 ) ) ;
#22722 = CARTESIAN_POINT ( 'NONE',  ( -0.1938976377952756625, -0.1938976377952756625, -0.3740157480314971750 ) ) ;
#22723 = CARTESIAN_POINT ( 'NONE',  ( -0.6627296587926501115, 0.1771653543307087075, -0.09757992244046823083 ) ) ;
#22724 = CARTESIAN_POINT ( 'NONE',  ( 0.2099737532808405305, -0.6046776061558807314, 0.2411417322834647770 ) ) ;
#22725 = CARTESIAN_POINT ( 'NONE',  ( -1.108923884514435132, -0.2845877964562159024, 0.3641732283464567677 ) ) ;
#22726 = CARTESIAN_POINT ( 'NONE',  ( 0.3996062992125986035, -0.1070741851644052972, -0.8182414698162727706 ) ) ;
#22727 = CARTESIAN_POINT ( 'NONE',  ( -1.003937007874014853, 0.1660481256975885056, 0.3530559997133364547 ) ) ;
#22728 = CARTESIAN_POINT ( 'NONE',  ( 0.1265901696524989184, 0.4724409448818898127, -2.589895013123359568 ) ) ;
#22729 = ORIENTED_EDGE ( 'NONE', *, *, #70277, .F. ) ;
#22730 = CARTESIAN_POINT ( 'NONE',  ( -1.502624671916009680, -0.08942795157528024563, -0.3641732283464568787 ) ) ;
#22731 = CARTESIAN_POINT ( 'NONE',  ( -0.6036745406824141069, 0.2306618581243848609, 0.2411417322834645549 ) ) ;
#22732 = CARTESIAN_POINT ( 'NONE',  ( 0.2567756966273455066, 1.138473552315965032, -1.484942126512834859 ) ) ;
#22733 = CARTESIAN_POINT ( 'NONE',  ( -1.397637795275589623, -0.5400638737290845981, -0.3530559997133363437 ) ) ;
#22734 = CARTESIAN_POINT ( 'NONE',  ( 0.1958661417322834775, 0.3392501089628018884, -1.646325459317585338 ) ) ;
#22735 = DIRECTION ( 'NONE',  ( -0.000000000000000000, -1.000000000000000000, -0.000000000000000000 ) ) ;
#22736 = CARTESIAN_POINT ( 'NONE',  ( 1.522309711286089939, 0.2306618581243848609, 0.2411417322834645549 ) ) ;
#22737 = CARTESIAN_POINT ( 'NONE',  ( 0.6036745406824154392, 0.2306618581243847221, -0.2411417322834647770 ) ) ;
#22738 = CARTESIAN_POINT ( 'NONE',  ( -0.1998031496062994405, 0.3460692066303957537, -2.294619422572178546 ) ) ;
#22739 = CARTESIAN_POINT ( 'NONE',  ( -1.660104986876639543, -0.05778040916215560624, -0.4822834645669293319 ) ) ;
#22740 = CARTESIAN_POINT ( 'NONE',  ( 0.3996062992125986035, 2.446882876249141962E-17, -0.5905511811023621549 ) ) ;
#22741 = EDGE_LOOP ( 'NONE', ( #63011, #47825 ) ) ;
#22742 = CARTESIAN_POINT ( 'NONE',  ( -0.8267716535433065062, 0.1771653543307087630, 0.000000000000000000 ) ) ;
#22743 = CARTESIAN_POINT ( 'NONE',  ( 0.2867679344610365999, 0.2867679344610365999, -2.177165354330708347 ) ) ;
#22744 = ORIENTED_EDGE ( 'NONE', *, *, #17348, .T. ) ;
#22745 = CARTESIAN_POINT ( 'NONE',  ( 0.6299212598425204535, -0.1870078740157479769, 0.4822834645669291653 ) ) ;
#22746 = CARTESIAN_POINT ( 'NONE',  ( -0.4790026246719154557, -0.3162353388693405765, 0.4822834645669290543 ) ) ;
#22747 = CARTESIAN_POINT ( 'NONE',  ( -1.227034120734907141, -0.6692913385826773087, -0.1292274648535924053 ) ) ;
#22748 = CARTESIAN_POINT ( 'NONE',  ( 1.095800524934383846, -0.05778040916215560624, -0.4822834645669293319 ) ) ;
#22749 = CARTESIAN_POINT ( 'NONE',  ( -1.266404199475064773, -0.08942795157528024563, -0.3641732283464568787 ) ) ;
#22750 = CARTESIAN_POINT ( 'NONE',  ( 0.05679685702235415246, 1.066397369817506435, -1.517643113990623238 ) ) ;
#22751 = CARTESIAN_POINT ( 'NONE',  ( 0.4986876640419954376, -0.6046776061558809534, -0.2411417322834644161 ) ) ;
#22752 = CARTESIAN_POINT ( 'NONE',  ( -0.6889763779527552368, 0.1660481256975885056, 0.3530559997133364547 ) ) ;
#22753 = CARTESIAN_POINT ( 'NONE',  ( -0.3917322834645669549, -7.196005306013483243E-17, -1.694206406002937593 ) ) ;
#22754 = CARTESIAN_POINT ( 'NONE',  ( -1.174540682414697335, -0.05778040916215522460, 0.4822834645669289988 ) ) ;
#22755 = CARTESIAN_POINT ( 'NONE',  ( 0.3230088838496886772, 1.189621120221110440, -2.759465352243644531 ) ) ;
#22756 = CARTESIAN_POINT ( 'NONE',  ( 0.8070866141732289112, -0.5400638737290845981, -0.3530559997133363437 ) ) ;
#22757 = CARTESIAN_POINT ( 'NONE',  ( 1.128608923884515169, -0.5023911411419708095, -0.1820866141732282451 ) ) ;
#22758 = ORIENTED_EDGE ( 'NONE', *, *, #66685, .F. ) ;
#22759 = CARTESIAN_POINT ( 'NONE',  ( -0.2867679344610367109, 0.2867679344610365444, -2.693588869587613566 ) ) ;
#22760 = CARTESIAN_POINT ( 'NONE',  ( -0.2821522309711278487, -0.6692913385826773087, -0.1292274648535924053 ) ) ;
#22761 = ORIENTED_EDGE ( 'NONE', *, *, #31743, .T. ) ;
#22762 = CARTESIAN_POINT ( 'NONE',  ( 0.3805774278215230400, -0.004921259842519870586, -0.3153832671262229437 ) ) ;
#22763 = CARTESIAN_POINT ( 'NONE',  ( -0.1265901696524993347, 0.4724409448818896462, -0.1640419947506561726 ) ) ;
#22764 = CARTESIAN_POINT ( 'NONE',  ( 0.7808398950131240079, -0.3162353388693405765, 0.4822834645669290543 ) ) ;
#22765 = CARTESIAN_POINT ( 'NONE',  ( 1.049868766404200127, -0.6046776061558809534, -0.2411417322834644161 ) ) ;
#22766 = CARTESIAN_POINT ( 'NONE',  ( -0.3608923884514428360, -0.6692913385826773087, -0.1292274648535924053 ) ) ;
#22767 = CARTESIAN_POINT ( 'NONE',  ( 0.3917322834645670659, 2.398668435337828261E-17, -1.374691231792337653 ) ) ;
#22768 = CARTESIAN_POINT ( 'NONE',  ( -0.8595800524934373854, -0.05778040916215522460, 0.4822834645669289988 ) ) ;
#22769 = CARTESIAN_POINT ( 'NONE',  ( 0.3392501089628018329, 0.1958661417322835607, -2.420603674540682260 ) ) ;
#22770 = CARTESIAN_POINT ( 'NONE',  ( -1.614173228346456268, -0.6692913385826771977, 8.415575281601705876E-17 ) ) ;
#22771 = CARTESIAN_POINT ( 'NONE',  ( -0.8727034120734901146, -0.3162353388693405765, 0.4822834645669290543 ) ) ;
#22772 = CARTESIAN_POINT ( 'NONE',  ( 1.128608923884515169, -0.6046776061558809534, -0.2411417322834644161 ) ) ;
#22773 = DIRECTION ( 'NONE',  ( -1.000000000000000000, -0.000000000000000000, -0.000000000000000000 ) ) ;
#22774 = EDGE_CURVE ( 'NONE', #62196, #82474, #63968, .T. ) ;
#22775 = CARTESIAN_POINT ( 'NONE',  ( -0.8267716535433065062, -0.6692913385826771977, 8.415575281601705876E-17 ) ) ;
#22776 = CARTESIAN_POINT ( 'NONE',  ( -0.3996062992125986590, 0.1070741851644051723, -0.1095800524934383152 ) ) ;
#22777 = EDGE_CURVE ( 'NONE', #55729, #16379, #1869, .T. ) ;
#22778 = CARTESIAN_POINT ( 'NONE',  ( 0.3608923884514443348, 0.2952755905511810774, -0.1292274648535930714 ) ) ;
#22779 = CARTESIAN_POINT ( 'NONE',  ( 0.1998031496062994405, -0.3460692066303958092, -1.824146981627296604 ) ) ;
#22780 = ADVANCED_FACE ( 'NONE', ( #78901 ), #46877, .F. ) ;
#22781 = CARTESIAN_POINT ( 'NONE',  ( -0.6167979002624665030, -0.4281496062992127816, -0.4176697321401328100 ) ) ;
#22782 = CARTESIAN_POINT ( 'NONE',  ( -1.476377952755905110, 0.07958543189024085140, 0.2665933059059887866 ) ) ;
#22783 = CARTESIAN_POINT ( 'NONE',  ( 0.4593175853018380828, -0.004921259842519870586, -0.3153832671262229437 ) ) ;
#22784 = CARTESIAN_POINT ( 'NONE',  ( 1.377952755905512472, -0.6692913385826771977, 8.415575281601705876E-17 ) ) ;
#22785 = CARTESIAN_POINT ( 'NONE',  ( -0.2362204724409451284, 0.4091458600556402425, -0.5623359580052492701 ) ) ;
#22786 = CARTESIAN_POINT ( 'NONE',  ( 0.9908136482939640111, -0.5511811023622046335, 0.09757992244046803654 ) ) ;
#22787 = CARTESIAN_POINT ( 'NONE',  ( 0.6102362204724416372, -0.5400638737290844871, 0.3530559997133364547 ) ) ;
#22788 = CARTESIAN_POINT ( 'NONE',  ( 0.1974969037888704704, 0.3420746716998660508, -0.5360892388451443669 ) ) ;
#22789 = CARTESIAN_POINT ( 'NONE',  ( -0.2952755905511804668, 0.1660481256975885056, 0.3530559997133364547 ) ) ;
#22790 = DIRECTION ( 'NONE',  ( 0.000000000000000000, 0.000000000000000000, -1.000000000000000000 ) ) ;
#22791 = CARTESIAN_POINT ( 'NONE',  ( 1.515748031496063186, -0.4536011799217368745, -0.2665933059059886201 ) ) ;
#22792 = CARTESIAN_POINT ( 'NONE',  ( -0.6692913385826764205, -0.6692913385826771977, 8.415575281601705876E-17 ) ) ;
#22793 = CARTESIAN_POINT ( 'NONE',  ( -0.2891555358219909388, -0.2891555358219912164, -0.6082677165354331006 ) ) ;
#22794 = CARTESIAN_POINT ( 'NONE',  ( 1.259842519685040019, -0.1870078740157480879, -0.4822834645669291653 ) ) ;
#22795 = CARTESIAN_POINT ( 'NONE',  ( 0.1706036745406830368, 0.05413385826771666132, 0.4176697321401328100 ) ) ;
#22796 = CARTESIAN_POINT ( 'NONE',  ( 0.3937007874015754361, -0.1870078740157479769, 0.3641732283464567677 ) ) ;
#22797 = CARTESIAN_POINT ( 'NONE',  ( -0.4588941285983808571, 1.412993309469693370, -1.023939894463827160 ) ) ;
#22798 = EDGE_CURVE ( 'NONE', #77721, #39649, #62008, .T. ) ;
#22799 = CARTESIAN_POINT ( 'NONE',  ( -0.05905511811023545637, 0.07958543189024085140, 0.2665933059059887866 ) ) ;
#22800 = CARTESIAN_POINT ( 'NONE',  ( 0.8202099737532813073, 0.1771653543307087630, 0.09757992244046791164 ) ) ;
#22801 = B_SPLINE_CURVE_WITH_KNOTS ( 'NONE', 3,
 ( #72419, #77902, #20233, #40424 ),
 .UNSPECIFIED., .F., .F.,
 ( 4, 4 ),
 ( 3.210432057687317930E-07, 0.001287787053612126330 ),
 .UNSPECIFIED. ) ;
#22802 = CARTESIAN_POINT ( 'NONE',  ( -1.607611548556429737, 0.2952755905511810774, -0.1292274648535930714 ) ) ;
#22803 = CARTESIAN_POINT ( 'NONE',  ( -0.3996062992125985480, -7.340648628747423112E-17, -1.375984251968504157 ) ) ;
#22804 = CARTESIAN_POINT ( 'NONE',  ( 0.9317585301837276734, 0.05413385826771626580, -0.4176697321401330321 ) ) ;
#22805 = EDGE_CURVE ( 'NONE', #81379, #9709, #30430, .T. ) ;
#22806 = CARTESIAN_POINT ( 'NONE',  ( 0.1958661417322834775, 0.3392501089628018884, -1.081364829396325389 ) ) ;
#22807 = CARTESIAN_POINT ( 'NONE',  ( 1.496062992125985147, -0.1870078740157479769, 0.3641732283464567677 ) ) ;
#22808 = CARTESIAN_POINT ( 'NONE',  ( -0.1208384647389192101, 0.3726288332213502641, 1.112018681666451222E-17 ) ) ;
#22809 = CARTESIAN_POINT ( 'NONE',  ( 0.07217847769028949700, -0.08942795157528024563, -0.3641732283464568787 ) ) ;
#22810 = CARTESIAN_POINT ( 'NONE',  ( 0.2165354330708668673, -0.5400638737290844871, 0.3530559997133364547 ) ) ;
#22811 = CARTESIAN_POINT ( 'NONE',  ( 1.581364829396326277, -0.2845877964562161244, -0.3641732283464567121 ) ) ;
#22812 = CARTESIAN_POINT ( 'NONE',  ( -1.463254593175852492, -0.5511811023622048555, -0.09757992244046775898 ) ) ;
#22813 = CARTESIAN_POINT ( 'NONE',  ( -1.351706036745406347, 0.05413385826771626580, -0.4176697321401330321 ) ) ;
#22814 = CARTESIAN_POINT ( 'NONE',  ( 0.5118110236220480003, -0.6692913385826771977, 8.415575281601705876E-17 ) ) ;
#22815 = CARTESIAN_POINT ( 'NONE',  ( 1.056430446194226658, 0.2952755905511811885, 0.1292274648535926551 ) ) ;
#22816 = CARTESIAN_POINT ( 'NONE',  ( -0.01122658826027363339, 1.063090000085920250, -1.632673439369667800 ) ) ;
#22817 = CARTESIAN_POINT ( 'NONE',  ( 0.05249343832021075018, 0.2306618581243847221, -0.2411417322834647770 ) ) ;
#22818 = CARTESIAN_POINT ( 'NONE',  ( 1.423884514435696413, -0.3162353388693409650, -0.4822834645669289433 ) ) ;
#22819 = CARTESIAN_POINT ( 'NONE',  ( 0.9908136482939640111, -0.6692913385826771977, 0.1292274648535927661 ) ) ;
#22820 = CARTESIAN_POINT ( 'NONE',  ( -1.614173228346457378, 1.330640075373402897, 0.1372047244094476981 ) ) ;
#22821 = CARTESIAN_POINT ( 'NONE',  ( 0.9251968503937015864, 0.07958543189024071263, -0.2665933059059888421 ) ) ;
#22822 = CARTESIAN_POINT ( 'NONE',  ( -1.574803149606298192, -0.1870078740157480601, -0.3641732283464567677 ) ) ;
#22823 = CARTESIAN_POINT ( 'NONE',  ( -0.1115485564304456306, 0.1771653543307087075, -0.09757992244046823083 ) ) ;
#22824 = CARTESIAN_POINT ( 'NONE',  ( 0.2493438320209980519, 0.05413385826771666132, 0.4176697321401328100 ) ) ;
#22825 = CARTESIAN_POINT ( 'NONE',  ( 0.5118110236220478892, 0.2952755905511811885, 0.000000000000000000 ) ) ;
#22826 = CARTESIAN_POINT ( 'NONE',  ( -0.2362204724409440182, -0.1870078740157479769, 0.4822834645669291653 ) ) ;
#22827 = CARTESIAN_POINT ( 'NONE',  ( -0.3018372703412066094, -0.004921259842519576551, 0.3153832671262227771 ) ) ;
#22828 = CARTESIAN_POINT ( 'NONE',  ( 0.7020997375328090762, -0.05778040916215560624, -0.4822834645669293319 ) ) ;
#22829 = CARTESIAN_POINT ( 'NONE',  ( 0.9973753280839902091, -0.5023911411419708095, 0.1820866141732285504 ) ) ;
#22830 = CARTESIAN_POINT ( 'NONE',  ( 0.2017716535433070613, -0.2017716535433070890, -0.3937007874015748254 ) ) ;
#22832 = DIRECTION ( 'NONE',  ( 0.000000000000000000, -1.000000000000000000, 0.000000000000000000 ) ) ;
#22831 = LINE ( 'NONE', #29962, #62137 ) ;
#22833 = CARTESIAN_POINT ( 'NONE',  ( 2.362204724409448620, 0.03937007874015751446, 8.247593713802677664E-15 ) ) ;
#22834 = CARTESIAN_POINT ( 'NONE',  ( -1.351706036745406347, -0.4281496062992124485, 0.4176697321401328655 ) ) ;
#22835 = CARTESIAN_POINT ( 'NONE',  ( -0.6889763779527552368, -0.5400638737290845981, -0.3530559997133363437 ) ) ;
#22836 = CARTESIAN_POINT ( 'NONE',  ( -0.4724409448818895907, -0.1265901696524993070, 0.1115485564304461719 ) ) ;
#22837 = CARTESIAN_POINT ( 'NONE',  ( -0.2891555358219911054, 0.2891555358219909388, -2.381889763779527769 ) ) ;
#22838 = EDGE_LOOP ( 'NONE', ( #60563, #45790, #78348, #79512 ) ) ;
#22839 = CARTESIAN_POINT ( 'NONE',  ( 0.6299212598425204535, -0.1870078740157480601, -0.3641732283464567677 ) ) ;
#22840 = CARTESIAN_POINT ( 'NONE',  ( 0.3917322834645670104, -0.1049643490035303411, -1.048556430446194287 ) ) ;
#22841 = CARTESIAN_POINT ( 'NONE',  ( 1.089238845144357537, -0.4281496062992124485, 0.4176697321401328655 ) ) ;
#22842 = CARTESIAN_POINT ( 'NONE',  ( 0.4091458600556403535, 0.2362204724409449896, -2.335958005249343827 ) ) ;
#22843 = CARTESIAN_POINT ( 'NONE',  ( 3.900966923095587457, 2.682389230697235671, -0.5314960629921258173 ) ) ;
#22844 = CARTESIAN_POINT ( 'NONE',  ( -1.358267716535432434, 0.07958543189024071263, -0.2665933059059888421 ) ) ;
#22845 = CARTESIAN_POINT ( 'NONE',  ( 1.581364829396326277, -0.3162353388693409650, -0.4822834645669289433 ) ) ;
#22846 = CARTESIAN_POINT ( 'NONE',  ( 1.358267716535433323, -0.4536011799217368745, -0.2665933059059886201 ) ) ;
#22847 = CARTESIAN_POINT ( 'NONE',  ( 0.5183727034120741983, -0.6692913385826771977, 0.1292274648535927661 ) ) ;
#22848 = CARTESIAN_POINT ( 'NONE',  ( 0.1049643490035304522, -0.3917322834645668994, -0.1653350149268222880 ) ) ;
#22849 = EDGE_CURVE ( 'NONE', #79084, #5432, #24111, .T. ) ;
#22850 = CARTESIAN_POINT ( 'NONE',  ( 0.06561679790026316017, -0.4281496062992124485, 0.4176697321401328655 ) ) ;
#22851 = CARTESIAN_POINT ( 'NONE',  ( -0.7217847769028863381, -0.004921259842519870586, -0.3153832671262229437 ) ) ;
#22852 = CARTESIAN_POINT ( 'NONE',  ( 0.3674540682414705883, 0.2306618581243847221, -0.2411417322834647770 ) ) ;
#22853 = CARTESIAN_POINT ( 'NONE',  ( -0.2362204724409442680, -0.1870078740157480879, -0.4822834645669291653 ) ) ;
#22854 = CARTESIAN_POINT ( 'NONE',  ( -1.191441481664478497, -1.283732188437465593E-15, -0.4281993546915544568 ) ) ;
#22855 = FACE_OUTER_BOUND ( 'NONE', #39438, .T. ) ;
#22856 = CARTESIAN_POINT ( 'NONE',  ( 0.1049643490035304799, -0.3917322834645670104, -1.656843462763466723 ) ) ;
#22857 = CARTESIAN_POINT ( 'NONE',  ( 0.8333333333333340365, -0.6692913385826771977, 0.1292274648535927661 ) ) ;
#22858 = CARTESIAN_POINT ( 'NONE',  ( -0.07874015748031421014, -0.1870078740157480879, -0.4822834645669291653 ) ) ;
#22859 = CARTESIAN_POINT ( 'NONE',  ( -0.9317585301837263412, -0.4281496062992127816, -0.4176697321401328100 ) ) ;
#22860 = CARTESIAN_POINT ( 'NONE',  ( 0.9711286089238851948, 0.2306618581243848609, 0.2411417322834645549 ) ) ;
#22861 = CARTESIAN_POINT ( 'NONE',  ( 0.4593175853018380828, 0.05413385826771626580, -0.4176697321401330321 ) ) ;
#22862 = CARTESIAN_POINT ( 'NONE',  ( -0.3392501089628017219, -0.1958661417322836718, -0.9245406824146982228 ) ) ;
#22863 = CARTESIAN_POINT ( 'NONE',  ( -0.5118110236220466680, -0.6692913385826771977, 8.415575281601705876E-17 ) ) ;
#22864 = CARTESIAN_POINT ( 'NONE',  ( 0.3280839895013130669, -0.4281496062992127816, -0.4176697321401328100 ) ) ;
#22865 = CARTESIAN_POINT ( 'NONE',  ( -0.5774278215223089816, -0.6046776061558807314, 0.2411417322834647770 ) ) ;
#22866 = CARTESIAN_POINT ( 'NONE',  ( 0.6299212598425204535, -0.1870078740157480601, -0.3641732283464567677 ) ) ;
#22867 = CARTESIAN_POINT ( 'NONE',  ( -1.732283464566928277, -0.1870078740157479769, 0.4822834645669291653 ) ) ;
#22868 = DIRECTION ( 'NONE',  ( -0.2810846377148224495, 0.6785983445458426688, -0.6785983445458504404 ) ) ;
#22869 = CARTESIAN_POINT ( 'NONE',  ( 0.5314960629921264834, 0.1660481256975883668, -0.3530559997133364547 ) ) ;
#22870 = CARTESIAN_POINT ( 'NONE',  ( -0.2362204724409447953, -0.4091458600556404646, -0.9297900262467192478 ) ) ;
#22871 = CARTESIAN_POINT ( 'NONE',  ( 0.3917322834645670104, 2.398668435337828261E-17, -2.472440944881889813 ) ) ;
#22872 = ORIENTED_EDGE ( 'NONE', *, *, #64509, .F. ) ;
#22873 = EDGE_LOOP ( 'NONE', ( #69676, #929, #81343, #73256 ) ) ;
#22874 = CARTESIAN_POINT ( 'NONE',  ( 0.5577427821522316087, -0.05778040916215522460, 0.4822834645669289988 ) ) ;
#22875 = CARTESIAN_POINT ( 'NONE',  ( 0.3937007874015754361, -0.1870078740157480601, -0.3641732283464567677 ) ) ;
#22877 = FACE_OUTER_BOUND ( 'NONE', #79391, .T. ) ;
#22876 = PLANE ( 'NONE',  #16257 ) ;
#22878 = CARTESIAN_POINT ( 'NONE',  ( -0.1049643490035302024, -0.3917322834645671215, -0.9442257217847768169 ) ) ;
#22879 = CARTESIAN_POINT ( 'NONE',  ( 0.6299212598425341092, 1.724409448818898127, -3.937007874015759690 ) ) ;
#22880 = CARTESIAN_POINT ( 'NONE',  ( 0.000000000000000000, 2.755905511811024056, 0.000000000000000000 ) ) ;
#22881 = CARTESIAN_POINT ( 'NONE',  ( 4.797336870675656522E-17, -0.3917322834645670104, -1.580708661417322913 ) ) ;
#22882 = CARTESIAN_POINT ( 'NONE',  ( -0.1070741851644056997, 0.3996062992125984925, -2.603018372703412631 ) ) ;
#22883 = CARTESIAN_POINT ( 'NONE',  ( 0.8333333333333340365, 0.2952755905511810774, -0.1292274648535930714 ) ) ;
#22884 = CARTESIAN_POINT ( 'NONE',  ( -0.7480314960629914633, -0.6692913385826771977, 8.415575281601705876E-17 ) ) ;
#22885 = CARTESIAN_POINT ( 'NONE',  ( -0.5577427821522301654, -0.05778040916215560624, -0.4822834645669293319 ) ) ;
#22886 = CARTESIAN_POINT ( 'NONE',  ( 0.8727034120734912248, -0.3162353388693409650, -0.4822834645669289433 ) ) ;
#22887 = CARTESIAN_POINT ( 'NONE',  ( 1.555118110236221041, -0.5400638737290844871, 0.3530559997133364547 ) ) ;
#22888 = CARTESIAN_POINT ( 'NONE',  ( 1.181102362204725198, -0.1870078740157479769, 0.3641732283464567677 ) ) ;
#22889 = CARTESIAN_POINT ( 'NONE',  ( -1.141732283464566011, 0.1771653543307087630, 0.000000000000000000 ) ) ;
#22890 = CARTESIAN_POINT ( 'NONE',  ( -9.594673741351313045E-17, 0.3917322834645670104, 0.1653543307086614844 ) ) ;
#22891 = CARTESIAN_POINT ( 'NONE',  ( 8.195543980992789655E-16, -0.1870078740157480879, -0.4822834645669291653 ) ) ;
#22893 = DIRECTION ( 'NONE',  ( 3.096699300667737957E-16, -1.000000000000000000, 0.000000000000000000 ) ) ;
#22892 = CARTESIAN_POINT ( 'NONE',  ( -0.5611900217179893735, -2.567464376874931580E-15, -0.4445507791589072832 ) ) ;
#22894 = CARTESIAN_POINT ( 'NONE',  ( -1.089238845144356427, -0.004921259842519576551, 0.3153832671262227771 ) ) ;
#22895 = CARTESIAN_POINT ( 'NONE',  ( 0.4527559055118117182, 0.1660481256975883668, -0.3530559997133364547 ) ) ;
#22896 = CARTESIAN_POINT ( 'NONE',  ( 1.207349081364829990, -0.5023911411419708095, -0.1820866141732282451 ) ) ;
#22897 = CARTESIAN_POINT ( 'NONE',  ( -0.3392501089628018329, -0.1958661417322836440, -1.077408505740470535 ) ) ;
#22898 = AXIS2_PLACEMENT_3D ( 'NONE', #40919, #67428, #16923 ) ;
#22899 = CARTESIAN_POINT ( 'NONE',  ( -1.069553805774277722, 0.1771653543307087630, 0.09757992244046791164 ) ) ;
#22900 = CARTESIAN_POINT ( 'NONE',  ( 1.417322834645670104, -0.1870078740157480879, -0.4822834645669291653 ) ) ;
#22901 = CARTESIAN_POINT ( 'NONE',  ( 0.3095674345919382509, 1.709700804348449843, 0.04767548262574627937 ) ) ;
#22902 = CARTESIAN_POINT ( 'NONE',  ( -0.3674540682414692561, -0.6046776061558809534, -0.2411417322834644161 ) ) ;
#22903 = CARTESIAN_POINT ( 'NONE',  ( -1.377952755905511140, -0.5511811023622047445, 6.969142054262312111E-17 ) ) ;
#22904 = CARTESIAN_POINT ( 'NONE',  ( -0.7349081364829390672, 0.2306618581243847221, -0.2411417322834647770 ) ) ;
#22905 = CARTESIAN_POINT ( 'NONE',  ( -1.358267716535432434, -0.4536011799217367080, 0.2665933059059888421 ) ) ;
#22906 = CARTESIAN_POINT ( 'NONE',  ( 0.3917322834645670104, 0.1049643490035304660, -0.2788907068579546400 ) ) ;
#22907 = CARTESIAN_POINT ( 'NONE',  ( 0.4658792650918640033, -0.3162353388693405765, 0.4822834645669290543 ) ) ;
#22908 = DIRECTION ( 'NONE',  ( -0.000000000000000000, -1.000000000000000000, -0.000000000000000000 ) ) ;
#22909 = CARTESIAN_POINT ( 'NONE',  ( 1.240157480314961314, -0.5400638737290844871, 0.3530559997133364547 ) ) ;
#22910 = CARTESIAN_POINT ( 'NONE',  ( -0.3458507752293906723, -0.3458507752293910609, -2.025590551181101873 ) ) ;
#22911 = CARTESIAN_POINT ( 'NONE',  ( -1.397637795275589623, 0.1660481256975885056, 0.3530559997133364547 ) ) ;
#22912 = CARTESIAN_POINT ( 'NONE',  ( -0.7414698162729651543, 0.1771653543307087075, -0.09757992244046823083 ) ) ;
#22913 = ADVANCED_FACE ( 'NONE', ( #22877 ), #80566, .F. ) ;
#22914 = CARTESIAN_POINT ( 'NONE',  ( -0.4921259842519677408, 0.1012011053420775880, -0.2882089793578256898 ) ) ;
#22915 = CARTESIAN_POINT ( 'NONE',  ( -0.1640419947506553400, -0.05778040916215560624, -0.4822834645669293319 ) ) ;
#22916 = CARTESIAN_POINT ( 'NONE',  ( 0.5774278215223104249, 0.1283753931104748280, 0.1820866141732283561 ) ) ;
#22917 = CARTESIAN_POINT ( 'NONE',  ( -1.115485564304461219, -0.3690944881889763329, 0.3153832671262228327 ) ) ;
#22918 = CARTESIAN_POINT ( 'NONE',  ( -1.312335958005248715, -0.6046776061558809534, -0.2411417322834644161 ) ) ;
#22920 = B_SPLINE_CURVE_WITH_KNOTS ( 'NONE', 3,
 ( #25441, #51107, #76804, #44784, #70481, #45210, #64590, #6926, #58259, #74242, #35513, #35934, #46879, #21224, #40580, #9019, #3531, #59934 ),
 .UNSPECIFIED., .F., .F.,
 ( 4, 2, 2, 2, 2, 2, 2, 2, 4 ),
 ( 1.401326170026117541E-16, 0.001588476978679904169, 0.002382715468019786214, 0.002779834712689726369, 0.002978394335024696880, 0.003077674146192181919, 0.003127314051775924655, 0.003152134004567797108, 0.003176953957359669126 ),
 .UNSPECIFIED. ) ;
#22919 = CARTESIAN_POINT ( 'NONE',  ( -1.633858267716534529, -0.5400638737290845981, -0.3530559997133363437 ) ) ;
#22921 = CARTESIAN_POINT ( 'NONE',  ( 1.299212598425197429, -0.6692913385826771977, 8.415575281601705876E-17 ) ) ;
#22922 = CARTESIAN_POINT ( 'NONE',  ( -0.4359958488159582091, 1.724409448818897905, -3.937007874015763687 ) ) ;
#22923 = CARTESIAN_POINT ( 'NONE',  ( 0.3674540682414705883, -0.5023911411419708095, 0.1820866141732285504 ) ) ;
#22924 = CARTESIAN_POINT ( 'NONE',  ( 1.082677165354331228, 0.1660481256975883668, -0.3530559997133364547 ) ) ;
#22925 = EDGE_CURVE ( 'NONE', #82069, #9892, #13211, .T. ) ;
#22926 = CARTESIAN_POINT ( 'NONE',  ( -0.6299212598425230070, 2.165354330708661568, 0.9285414500055690912 ) ) ;
#22927 = CARTESIAN_POINT ( 'NONE',  ( 1.305774278215223960, 0.1771653543307087075, -0.09757992244046823083 ) ) ;
#22928 = ORIENTED_EDGE ( 'NONE', *, *, #42996, .T. ) ;
#22929 = CARTESIAN_POINT ( 'NONE',  ( -1.246719160104985846, -0.4281496062992127816, -0.4176697321401328100 ) ) ;
#22930 = CARTESIAN_POINT ( 'NONE',  ( -0.9580052493438311334, 0.05413385826771626580, -0.4176697321401330321 ) ) ;
#22931 = CARTESIAN_POINT ( 'NONE',  ( 0.2690288713910767848, -0.6692913385826773087, -0.1292274648535924053 ) ) ;
#22932 = CARTESIAN_POINT ( 'NONE',  ( -9.787531504996567848E-17, 0.3996062992125986035, -0.1574803149606299746 ) ) ;
#22933 = CARTESIAN_POINT ( 'NONE',  ( 4.893765752498283308E-17, -0.3996062992125985480, -2.202755905511811108 ) ) ;
#22934 = CARTESIAN_POINT ( 'NONE',  ( 0.8530183727034126306, 0.05413385826771626580, -0.4176697321401330321 ) ) ;
#22935 = CARTESIAN_POINT ( 'NONE',  ( 1.443569553805774897, 0.1283753931104748280, 0.1820866141732283561 ) ) ;
#22936 = CARTESIAN_POINT ( 'NONE',  ( 0.1640419947506569498, -0.3162353388693409650, -0.4822834645669289433 ) ) ;
#22937 = CARTESIAN_POINT ( 'NONE',  ( 0.6364829396325465405, -0.05778040916215522460, 0.4822834645669289988 ) ) ;
#22938 = CARTESIAN_POINT ( 'NONE',  ( -0.3996062992125986035, -0.1070741851644056997, -1.778215223097112663 ) ) ;
#22939 = CARTESIAN_POINT ( 'NONE',  ( 0.1974969037888704704, 0.3420746716998660508, -1.246719160104986734 ) ) ;
#22940 = CARTESIAN_POINT ( 'NONE',  ( 0.3996062992125986590, -0.1070741851644053111, -2.316272965879265122 ) ) ;
#22941 = CARTESIAN_POINT ( 'NONE',  ( -2.543486866223389153, 2.716535433070866645, 0.5314960629921260393 ) ) ;
#22942 = CARTESIAN_POINT ( 'NONE',  ( -0.1958661417322834220, -0.3392501089628018884, -0.05774278215223092176 ) ) ;
#22943 = CARTESIAN_POINT ( 'NONE',  ( 0.03280839895013198948, 0.1771653543307087630, 0.09757992244046791164 ) ) ;
#22944 = CARTESIAN_POINT ( 'NONE',  ( -0.3083989501312330295, -0.05778040916215522460, 0.4822834645669289988 ) ) ;
#22945 = CARTESIAN_POINT ( 'NONE',  ( 1.049868766404200127, -0.6046776061558809534, -0.2411417322834644161 ) ) ;
#22946 = CARTESIAN_POINT ( 'NONE',  ( -0.3420746716998662729, 0.1974969037888702206, -2.307742782152230721 ) ) ;
#22947 = ADVANCED_FACE ( 'NONE', ( #74239 ), #49780, .T. ) ;
#22948 = CARTESIAN_POINT ( 'NONE',  ( 0.1706036745406830368, -0.3690944881889765550, -0.3153832671262227771 ) ) ;
#22949 = CARTESIAN_POINT ( 'NONE',  ( -1.213910761154854745, -0.6692913385826771977, 0.1292274648535927661 ) ) ;
#22950 = CARTESIAN_POINT ( 'NONE',  ( 1.358267716535433323, -0.5400638737290845981, -0.3530559997133363437 ) ) ;
#22951 = CARTESIAN_POINT ( 'NONE',  ( -0.2362204724409451284, 0.4091458600556402425, -2.375328083989501238 ) ) ;
#22952 = CARTESIAN_POINT ( 'NONE',  ( 0.3996062992125986035, 2.446882876249141962E-17, -1.692913385826771533 ) ) ;
#22953 = CARTESIAN_POINT ( 'NONE',  ( 0.4848630542936496757, 1.968099216065433366, 0.4919401540133064299 ) ) ;
#22954 = ORIENTED_EDGE ( 'NONE', *, *, #15339, .F. ) ;
#22955 = CARTESIAN_POINT ( 'NONE',  ( 1.023622047244095112, -0.1870078740157480879, -0.4822834645669291653 ) ) ;
#22956 = EDGE_CURVE ( 'NONE', #61385, #10785, #51879, .T. ) ;
#22957 = CARTESIAN_POINT ( 'NONE',  ( 1.220472440944882386, -0.5511811023622047445, 6.969142054262312111E-17 ) ) ;
#22959 = CARTESIAN_POINT ( 'NONE',  ( -1.627296587926508442, 0.2306618581243848609, 0.2411417322834645549 ) ) ;
#22958 = CARTESIAN_POINT ( 'NONE',  ( 1.673228346456693494, 0.1660481256975885056, 0.3530559997133364547 ) ) ;
#22960 = CARTESIAN_POINT ( 'NONE',  ( 0.3392501089628018884, -0.1958661417322834220, 0.1253280839895012100 ) ) ;
#22961 = DIRECTION ( 'NONE',  ( -3.491481338843132961E-15, -0.000000000000000000, 1.000000000000000000 ) ) ;
#22962 = CARTESIAN_POINT ( 'NONE',  ( 1.181102362204725198, -0.1870078740157479769, 0.4822834645669291653 ) ) ;
#22963 = CARTESIAN_POINT ( 'NONE',  ( -1.666666666666665853, 0.05413385826771626580, -0.4176697321401330321 ) ) ;
#22964 = CARTESIAN_POINT ( 'NONE',  ( -0.5905511811023615998, 0.2952755905511811885, 0.000000000000000000 ) ) ;
#22965 = CARTESIAN_POINT ( 'NONE',  ( -0.5183727034120726440, -0.6692913385826773087, -0.1292274648535924053 ) ) ;
#22966 = CARTESIAN_POINT ( 'NONE',  ( 1.423884514435696191, -0.05778040916215522460, 0.4822834645669289988 ) ) ;
#22967 = CARTESIAN_POINT ( 'NONE',  ( 0.1958661417322834775, 0.3392501089628018884, -0.2290026246719160941 ) ) ;
#22968 = CARTESIAN_POINT ( 'NONE',  ( 0.1181102362204730916, -0.6692913385826771977, 8.415575281601705876E-17 ) ) ;
#22969 = CARTESIAN_POINT ( 'NONE',  ( 0.1958661417322836440, -0.3392501089628017219, -2.446194225721784576 ) ) ;
#22970 = CARTESIAN_POINT ( 'NONE',  ( 1.482939632545932307, -0.4281496062992124485, 0.4176697321401328655 ) ) ;
#22971 = ORIENTED_EDGE ( 'NONE', *, *, #57708, .F. ) ;
#22972 = CARTESIAN_POINT ( 'NONE',  ( -0.3949938075777409963, -7.255918531996591613E-17, -2.559055118110236560 ) ) ;
#22973 = EDGE_LOOP ( 'NONE', ( #76073, #71015, #22582, #78080 ) ) ;
#22974 = LINE ( 'NONE', #21730, #63718 ) ;
#22975 = CARTESIAN_POINT ( 'NONE',  ( -1.699475065616797398, 0.2952755905511811885, 0.1292274648535926551 ) ) ;
#22976 = CARTESIAN_POINT ( 'NONE',  ( -0.3460692066303960868, 0.1998031496062990242, -0.9711286089238845287 ) ) ;
#22977 = CARTESIAN_POINT ( 'NONE',  ( -1.646051170424378096, 0.000000000000000000, 0.3464511005275205946 ) ) ;
#22978 = CARTESIAN_POINT ( 'NONE',  ( -0.1450607720586916394, 0.000000000000000000, 0.3464511005275205946 ) ) ;
#22979 = CARTESIAN_POINT ( 'NONE',  ( 0.4527559055118117182, 0.1660481256975883391, -0.3530559997133364547 ) ) ;
#22980 = CARTESIAN_POINT ( 'NONE',  ( 0.9337842054690638216, -6.978086149529499157E-16, -0.3954974714151469617 ) ) ;
#22981 = CARTESIAN_POINT ( 'NONE',  ( 0.3917322834645670104, -0.1049643490035303411, 0.1187664041994749703 ) ) ;
#22982 =( BOUNDED_CURVE ( )  B_SPLINE_CURVE ( 2, ( #48381, #79997, #60609, #2958, #73673, #28623, #22311 ),
 .UNSPECIFIED., .F., .F. ) 
 B_SPLINE_CURVE_WITH_KNOTS ( ( 3, 2, 2, 3 ),
 ( 0.1363636363636363535, 0.1401515151515151381, 0.1439393939393939503, 0.1448507235470174181 ),
 .UNSPECIFIED. ) 
 CURVE ( )  GEOMETRIC_REPRESENTATION_ITEM ( )  RATIONAL_B_SPLINE_CURVE ( ( 1.000000000000000000, 0.9659258262890683122, 1.000000000000000000, 0.9659258262890683122, 1.000000000000000000, 0.9918020599134675930, 0.9875488213027519002 ) ) 
 REPRESENTATION_ITEM ( '' )  );
#22983 = CARTESIAN_POINT ( 'NONE',  ( -0.3543307086614165824, 0.1771653543307087630, 0.000000000000000000 ) ) ;
#22984 = CARTESIAN_POINT ( 'NONE',  ( -1.410761154855642463, -0.08942795157527998196, 0.3641732283464567121 ) ) ;
#22985 = CARTESIAN_POINT ( 'NONE',  ( -1.220472440944881054, -0.6692913385826771977, 8.415575281601705876E-17 ) ) ;
#22986 = CARTESIAN_POINT ( 'NONE',  ( 0.3608923884514443348, 0.2952755905511810774, -0.1292274648535930714 ) ) ;
#22987 = CARTESIAN_POINT ( 'NONE',  ( -1.351706036745406347, -0.4281496062992124485, 0.4176697321401328655 ) ) ;
#22988 = AXIS2_PLACEMENT_3D ( 'NONE', #9287, #29865, #2971 ) ;
#22989 = CARTESIAN_POINT ( 'NONE',  ( 0.2867679344610365999, -0.2867679344610365444, 0.06692913385826775030 ) ) ;
#22990 = ORIENTED_EDGE ( 'NONE', *, *, #41310, .T. ) ;
#22991 = CARTESIAN_POINT ( 'NONE',  ( -1.240157480314959759, -0.5400638737290845981, -0.3530559997133363437 ) ) ;
#22992 = DIRECTION ( 'NONE',  ( -3.096699300667737957E-16, 1.000000000000000000, -0.000000000000000000 ) ) ;
#22993 = CARTESIAN_POINT ( 'NONE',  ( 0.2362204724409451007, -0.4091458600556402980, -1.666666666666666741 ) ) ;
#22994 = DIRECTION ( 'NONE',  ( -0.000000000000000000, -1.000000000000000000, 0.000000000000000000 ) ) ;
#22995 = CARTESIAN_POINT ( 'NONE',  ( 0.1958661417322836440, -0.3392501089628017219, -0.5564304461942257696 ) ) ;
#22996 = DIRECTION ( 'NONE',  ( -0.7071067811865487940, 0.000000000000000000, 0.7071067811865463515 ) ) ;
#22997 = CARTESIAN_POINT ( 'NONE',  ( -0.6364829396325453192, -0.05778040916215560624, -0.4822834645669293319 ) ) ;
#22998 = CARTESIAN_POINT ( 'NONE',  ( 1.384514435695538559, 0.2952755905511810774, -0.1292274648535930714 ) ) ;
#23000 = CARTESIAN_POINT ( 'NONE',  ( -0.4469779880792152382, 1.697109554835841916, 2.611722799339278200 ) ) ;
#22999 = CARTESIAN_POINT ( 'NONE',  ( -1.732283464566928277, -0.1870078740157479769, 0.4822834645669291653 ) ) ;
#23001 = CARTESIAN_POINT ( 'NONE',  ( 1.456692913385827515, -0.6692913385826771977, 8.415575281601705876E-17 ) ) ;
#23002 = CARTESIAN_POINT ( 'NONE',  ( -0.6692913385826764205, -0.6692913385826771977, 8.415575281601705876E-17 ) ) ;
#23003 = CARTESIAN_POINT ( 'NONE',  ( -0.3392501089628018329, -0.1958661417322836440, -0.1325266159766911034 ) ) ;
#23004 = CARTESIAN_POINT ( 'NONE',  ( 0.006561679790026889343, -0.08942795157527998196, 0.3641732283464567121 ) ) ;
#23005 = CARTESIAN_POINT ( 'NONE',  ( 0.2867679344610366554, -0.2867679344610365444, -0.3405511811023621549 ) ) ;
#23006 = CARTESIAN_POINT ( 'NONE',  ( -0.2493438320209966919, -0.3690944881889763329, 0.3153832671262228327 ) ) ;
#23007 = CARTESIAN_POINT ( 'NONE',  ( 0.8005249343832027131, -0.004921259842519576551, 0.3153832671262227771 ) ) ;
#23008 = CARTESIAN_POINT ( 'NONE',  ( 0.5905511811023629321, -0.6692913385826771977, 8.415575281601705876E-17 ) ) ;
#23009 = CARTESIAN_POINT ( 'NONE',  ( -0.1640419947506553400, -0.08942795157528024563, -0.3641732283464568787 ) ) ;
#23010 = CARTESIAN_POINT ( 'NONE',  ( 0.3392501089628018884, -0.1958661417322834220, -2.144356955380577467 ) ) ;
#23011 = CARTESIAN_POINT ( 'NONE',  ( -1.646981627296586703, -0.05778040916215522460, 0.4822834645669289988 ) ) ;
#23012 = CARTESIAN_POINT ( 'NONE',  ( -1.200787401574802349, -0.4536011799217367080, 0.2665933059059888421 ) ) ;
#23013 = CARTESIAN_POINT ( 'NONE',  ( 0.2362204724409451007, -0.4091458600556402980, -0.6410761154855643129 ) ) ;
#23014 = CARTESIAN_POINT ( 'NONE',  ( 0.1902887139107617975, 0.2952755905511811885, 0.1292274648535926551 ) ) ;
#23015 = EDGE_CURVE ( 'NONE', #35589, #23460, #81482, .T. ) ;
#23016 = CARTESIAN_POINT ( 'NONE',  ( -0.4330708661417315697, -0.6692913385826771977, 8.415575281601705876E-17 ) ) ;
#23017 = CARTESIAN_POINT ( 'NONE',  ( 1.614173228346457378, -0.5511811023622047445, 6.969142054262312111E-17 ) ) ;
#23018 = CARTESIAN_POINT ( 'NONE',  ( 0.01968503937007930540, 0.07958543189024085140, 0.2665933059059887866 ) ) ;
#23019 = CARTESIAN_POINT ( 'NONE',  ( -0.1968503937007867743, -0.6692913385826771977, 8.415575281601705876E-17 ) ) ;
#23020 = CARTESIAN_POINT ( 'NONE',  ( -0.5511811023622038563, -0.1870078740157479769, 0.4822834645669291653 ) ) ;
#23021 = DIRECTION ( 'NONE',  ( 0.000000000000000000, -0.000000000000000000, 1.000000000000000000 ) ) ;
#23022 = CARTESIAN_POINT ( 'NONE',  ( -0.1265901696524993347, 0.4724409448818896462, -0.3215223097112860917 ) ) ;
#23023 = CARTESIAN_POINT ( 'NONE',  ( 0.3543307086614181922, -0.6692913385826771977, 8.415575281601705876E-17 ) ) ;
#23024 = CIRCLE ( 'NONE', #40459, 0.3051181102362204856 ) ;
#23025 = CARTESIAN_POINT ( 'NONE',  ( 0.1998031496062992463, 0.3460692066303959202, -2.110892388451443225 ) ) ;
#23026 = CARTESIAN_POINT ( 'NONE',  ( 1.469816272965879911, 0.2306618581243847221, -0.2411417322834647770 ) ) ;
#23027 = CARTESIAN_POINT ( 'NONE',  ( -0.5643044619422565855, -0.004921259842519870586, -0.3153832671262229437 ) ) ;
#23028 = CARTESIAN_POINT ( 'NONE',  ( -0.4790026246719154557, -0.3162353388693405765, 0.4822834645669290543 ) ) ;
#23029 = CARTESIAN_POINT ( 'NONE',  ( -1.646981627296586703, -0.08942795157527998196, 0.3641732283464567121 ) ) ;
#23030 = CARTESIAN_POINT ( 'NONE',  ( 1.463254593175853824, -0.6692913385826771977, 0.1292274648535927661 ) ) ;
#23031 = CARTESIAN_POINT ( 'NONE',  ( -1.463254593175852492, 0.2952755905511811885, 0.1292274648535926551 ) ) ;
#23032 = CARTESIAN_POINT ( 'NONE',  ( -0.8727034120734901146, -0.08942795157528024563, -0.3641732283464568787 ) ) ;
#23033 = CARTESIAN_POINT ( 'NONE',  ( 0.1998031496062992463, 0.3460692066303959202, -0.3786089238845143923 ) ) ;
#23034 = CARTESIAN_POINT ( 'NONE',  ( -0.2925321140481932924, 0.2925321140481931814, -0.4921259842519684624 ) ) ;
#23035 = CARTESIAN_POINT ( 'NONE',  ( -0.2891555358219908833, -0.2891555358219912164, 0.09842519685039366473 ) ) ;
#23036 = CARTESIAN_POINT ( 'NONE',  ( 1.391076115485564868, 0.1283753931104746893, -0.1820866141732285504 ) ) ;
#23037 = CARTESIAN_POINT ( 'NONE',  ( 1.299212598425197429, 0.1771653543307087630, 0.000000000000000000 ) ) ;
#23038 = CARTESIAN_POINT ( 'NONE',  ( 1.023622047244095112, -0.1870078740157480879, -0.4822834645669291653 ) ) ;
#23039 = CARTESIAN_POINT ( 'NONE',  ( 0.4593175853018379717, 0.009842519685039147898, -0.3409548833797004797 ) ) ;
#23040 = CARTESIAN_POINT ( 'NONE',  ( 0.8727034120734912248, -0.3162353388693409650, -0.4822834645669289433 ) ) ;
#23041 = CARTESIAN_POINT ( 'NONE',  ( -0.2891555358219909388, -0.2891555358219912164, -0.9232283464566930498 ) ) ;
#23042 = CARTESIAN_POINT ( 'NONE',  ( 1.246719160104987623, -0.004921259842519870586, -0.3153832671262229437 ) ) ;
#23043 = CARTESIAN_POINT ( 'NONE',  ( 0.2624671916010504757, 0.2306618581243848609, 0.2411417322834645549 ) ) ;
#23044 = CARTESIAN_POINT ( 'NONE',  ( -0.8530183727034112984, 0.05413385826771666132, 0.4176697321401328100 ) ) ;
#23045 = CARTESIAN_POINT ( 'NONE',  ( 1.312335958005250269, -0.6046776061558807314, 0.2411417322834647770 ) ) ;
#23046 = CARTESIAN_POINT ( 'NONE',  ( -0.4091458600556405756, 0.2362204724409446288, -1.128608923884514503 ) ) ;
#23047 = CARTESIAN_POINT ( 'NONE',  ( -0.1070741851644051862, -0.3996062992125986590, -2.119422572178477626 ) ) ;
#23048 = CARTESIAN_POINT ( 'NONE',  ( 0.2493438320209980519, -0.3690944881889765550, -0.3153832671262227771 ) ) ;
#23049 = VERTEX_POINT ( 'NONE', #10263 ) ;
#23050 = CARTESIAN_POINT ( 'NONE',  ( -0.1958661417322836995, 0.3392501089628017219, -0.6397830953093982531 ) ) ;
#23051 = ORIENTED_EDGE ( 'NONE', *, *, #33188, .F. ) ;
#23052 = CARTESIAN_POINT ( 'NONE',  ( -0.8333333333333323711, -0.6692913385826773087, -0.1292274648535924053 ) ) ;
#23053 = CARTESIAN_POINT ( 'NONE',  ( -0.3937007874015740483, -0.1870078740157479769, 0.4822834645669291653 ) ) ;
#23054 = CARTESIAN_POINT ( 'NONE',  ( -0.3215223097112853146, -0.05778040916215560624, -0.4822834645669293319 ) ) ;
#23055 = CARTESIAN_POINT ( 'NONE',  ( 0.7611548556430454138, 0.2306618581243847221, -0.2411417322834647770 ) ) ;
#23056 = CARTESIAN_POINT ( 'NONE',  ( -0.8464566929133852113, 0.1660481256975885056, 0.3530559997133364547 ) ) ;
#23057 = CARTESIAN_POINT ( 'NONE',  ( -0.5971128608923877978, 0.2952755905511811885, 0.1292274648535926551 ) ) ;
#23058 = CARTESIAN_POINT ( 'NONE',  ( 1.194225721784777594, -0.4281496062992127816, -0.4176697321401328100 ) ) ;
#23059 = CARTESIAN_POINT ( 'NONE',  ( 0.4921259842519691285, 0.1660481256975885056, 0.3530559997133364547 ) ) ;
#23060 = CARTESIAN_POINT ( 'NONE',  ( 0.6364829396325465405, -0.3162353388693409650, -0.4822834645669289433 ) ) ;
#23061 = CARTESIAN_POINT ( 'NONE',  ( 0.2867679344610365999, 0.2867679344610365999, -1.232283464566929387 ) ) ;
#23062 = CARTESIAN_POINT ( 'NONE',  ( -0.5643044619422565855, -0.3690944881889763329, 0.3153832671262228327 ) ) ;
#23063 = VERTEX_POINT ( 'NONE', #61174 ) ;
#23064 = CARTESIAN_POINT ( 'NONE',  ( 0.1974969037888706369, -0.3420746716998659953, -1.036745406824147064 ) ) ;
#23065 = VERTEX_POINT ( 'NONE', #75480 ) ;
#23066 = CARTESIAN_POINT ( 'NONE',  ( -0.6955380577427815458, -0.3690944881889765550, -0.3153832671262227771 ) ) ;
#23067 = CARTESIAN_POINT ( 'NONE',  ( -0.3280839895013117347, 0.05413385826771626580, -0.4176697321401330321 ) ) ;
#23068 = FACE_OUTER_BOUND ( 'NONE', #19568, .T. ) ;
#23069 = CARTESIAN_POINT ( 'NONE',  ( -0.5446194225721777693, -0.3162353388693409650, -0.4822834645669289433 ) ) ;
#23070 = CARTESIAN_POINT ( 'NONE',  ( -1.010498687664041384, -0.4281496062992127816, -0.4176697321401328100 ) ) ;
#23071 = CARTESIAN_POINT ( 'NONE',  ( -1.338582677165353729, -0.1870078740157479769, 0.4822834645669291653 ) ) ;
#23072 = CARTESIAN_POINT ( 'NONE',  ( -1.259842519685038686, -0.1870078740157479769, 0.4822834645669291653 ) ) ;
#23073 = CARTESIAN_POINT ( 'NONE',  ( 0.7611548556430454138, 0.1283753931104746893, -0.1820866141732285504 ) ) ;
#23074 = CARTESIAN_POINT ( 'NONE',  ( 0.4678446894728544025, 1.617652276888540852, 1.019864652736552690 ) ) ;
#23075 = CARTESIAN_POINT ( 'NONE',  ( -1.600415083108464254, 2.375314266909943406, 0.1324231768467336867 ) ) ;
#23076 = CARTESIAN_POINT ( 'NONE',  ( 0.4527559055118117182, -0.4536011799217367080, 0.2665933059059888421 ) ) ;
#23077 = CARTESIAN_POINT ( 'NONE',  ( 0.2362204724409456558, -0.1870078740157479769, 0.4822834645669291653 ) ) ;
#23078 = CARTESIAN_POINT ( 'NONE',  ( -0.1574803149606292529, -0.1870078740157480879, -0.4822834645669291653 ) ) ;
#23079 = ORIENTED_EDGE ( 'NONE', *, *, #76884, .F. ) ;
#23080 = AXIS2_PLACEMENT_3D ( 'NONE', #39324, #1458, #624 ) ;
#23081 = CARTESIAN_POINT ( 'NONE',  ( 4.893765752498283924E-17, -0.3996062992125986035, -1.811023622047244208 ) ) ;
#23082 = LINE ( 'NONE', #68131, #53319 ) ;
#23083 = ORIENTED_EDGE ( 'NONE', *, *, #17293, .F. ) ;
#23084 = CARTESIAN_POINT ( 'NONE',  ( 0.3460692066303959202, -0.1998031496062991630, -0.9691601049868766582 ) ) ;
#23085 = CARTESIAN_POINT ( 'NONE',  ( 1.614173228346457378, 0.2952755905511811885, 0.000000000000000000 ) ) ;
#23086 = CARTESIAN_POINT ( 'NONE',  ( -0.9251968503937002541, 0.07958543189024085140, 0.2665933059059887866 ) ) ;
#23087 = CARTESIAN_POINT ( 'NONE',  ( -1.023622047244094002, -0.1870078740157480879, -0.4822834645669291653 ) ) ;
#23088 = CARTESIAN_POINT ( 'NONE',  ( 0.2362204724409449064, 0.4091458600556404646, -0.3018372703412073310 ) ) ;
#23089 = DIRECTION ( 'NONE',  ( -0.000000000000000000, 1.000000000000000000, -0.000000000000000000 ) ) ;
#23090 = CARTESIAN_POINT ( 'NONE',  ( -0.3917322834645669549, -0.1049643490035306603, -2.335301837270341352 ) ) ;
#23091 = CARTESIAN_POINT ( 'NONE',  ( -1.502624671916009680, -0.2845877964562159024, 0.3641732283464567677 ) ) ;
#23092 = CARTESIAN_POINT ( 'NONE',  ( 0.4790026246719167324, -0.05778040916215522460, 0.4822834645669289988 ) ) ;
#23093 = CARTESIAN_POINT ( 'NONE',  ( 0.5249343832021005074, -0.6046776061558807314, 0.2411417322834647770 ) ) ;
#23094 = CARTESIAN_POINT ( 'NONE',  ( -0.5380577427821514602, -0.004921259842519576551, 0.3153832671262227771 ) ) ;
#23095 = CARTESIAN_POINT ( 'NONE',  ( -0.07874015748031421014, -0.1870078740157480879, -0.4822834645669291653 ) ) ;
#23096 = CARTESIAN_POINT ( 'NONE',  ( 0.2362204724409451007, -0.4091458600556402980, -2.373359580052493367 ) ) ;
#23097 = CARTESIAN_POINT ( 'NONE',  ( -0.5118110236220466680, -0.6692913385826771977, 8.415575281601705876E-17 ) ) ;
#23098 = CARTESIAN_POINT ( 'NONE',  ( 0.3420746716998660508, 0.1974969037888705814, -1.940288713910761187 ) ) ;
#23099 = CARTESIAN_POINT ( 'NONE',  ( 1.259842519685040019, -0.1870078740157479769, 0.3641732283464567677 ) ) ;
#23100 = CARTESIAN_POINT ( 'NONE',  ( 0.1443569553805781891, -0.3690944881889763329, 0.3153832671262228327 ) ) ;
#23101 = CARTESIAN_POINT ( 'NONE',  ( 1.213910761154856299, 0.1771653543307087630, 0.09757992244046791164 ) ) ;
#23102 = CARTESIAN_POINT ( 'NONE',  ( -0.9711286089238838626, -0.6046776061558807314, 0.2411417322834647770 ) ) ;
#23103 = CARTESIAN_POINT ( 'NONE',  ( -1.332020997375327642, -0.08942795157527998196, 0.3641732283464567121 ) ) ;
#23104 = CARTESIAN_POINT ( 'NONE',  ( -1.614173228346457378, 0.7166040191147894367, 0.1372047244094476981 ) ) ;
#23105 = CARTESIAN_POINT ( 'NONE',  ( -1.253280839895012377, -0.05778040916215522460, 0.4822834645669289988 ) ) ;
#23106 = CARTESIAN_POINT ( 'NONE',  ( -0.5971128608923877978, -0.6692913385826773087, -0.1292274648535924053 ) ) ;
#23107 = EDGE_CURVE ( 'NONE', #25632, #44077, #34222, .T. ) ;
#23108 =( BOUNDED_CURVE ( )  B_SPLINE_CURVE ( 1, ( #9425, #60761 ),
 .UNSPECIFIED., .F., .F. ) 
 B_SPLINE_CURVE_WITH_KNOTS ( ( 2, 2 ),
 ( 0.0007457734483630323874, 0.002000000000000001776 ),
 .UNSPECIFIED. ) 
 CURVE ( )  GEOMETRIC_REPRESENTATION_ITEM ( )  RATIONAL_B_SPLINE_CURVE ( ( 0.9875488213027523443, 0.9875488213027523443 ) ) 
 REPRESENTATION_ITEM ( '' )  );
#23109 = CARTESIAN_POINT ( 'NONE',  ( 0.3280839895013130669, -0.4281496062992127816, -0.4176697321401328100 ) ) ;
#23110 = CARTESIAN_POINT ( 'NONE',  ( 0.3917322834645669549, 2.398668435337827645E-17, -2.560348138286403064 ) ) ;
#23111 = CARTESIAN_POINT ( 'NONE',  ( -1.850582881112984746, 1.063196196511240865, 0.01636564761927281758 ) ) ;
#23112 = CARTESIAN_POINT ( 'NONE',  ( 0.1771653543307093182, -0.4536011799217368745, -0.2665933059059886201 ) ) ;
#23113 = CARTESIAN_POINT ( 'NONE',  ( 0.8595800524934390507, -0.05778040916215560624, -0.4822834645669293319 ) ) ;
#23114 = CARTESIAN_POINT ( 'NONE',  ( -0.4091458600556405756, 0.2362204724409446288, -1.047900262467191590 ) ) ;
#23115 = CARTESIAN_POINT ( 'NONE',  ( 0.5380577427821529035, -0.4281496062992124485, 0.4176697321401328655 ) ) ;
#23116 = CARTESIAN_POINT ( 'NONE',  ( -1.528871391076114250, 0.1771653543307087075, -0.09757992244046823083 ) ) ;
#23117 = CARTESIAN_POINT ( 'NONE',  ( -1.397637795275589623, 0.1660481256975885056, 0.3530559997133364547 ) ) ;
#23118 = CARTESIAN_POINT ( 'NONE',  ( -1.056430446194224881, 0.2952755905511810774, -0.1292274648535930714 ) ) ;
#23119 = CARTESIAN_POINT ( 'NONE',  ( -0.4068241469816264999, -0.3690944881889763329, 0.3153832671262228327 ) ) ;
#23120 = CARTESIAN_POINT ( 'NONE',  ( 0.2952755905511810774, 3.616083068348483797E-17, 6.062992125984251857 ) ) ;
#23121 = CARTESIAN_POINT ( 'NONE',  ( 0.7480314960629927956, -0.5511811023622047445, 6.969142054262312111E-17 ) ) ;
#23122 = CARTESIAN_POINT ( 'NONE',  ( -0.1509186351706028884, -0.3162353388693409650, -0.4822834645669289433 ) ) ;
#23123 = CARTESIAN_POINT ( 'NONE',  ( 0.2925321140481932369, 0.2925321140481932369, -0.3720472440944882497 ) ) ;
#23124 = CARTESIAN_POINT ( 'NONE',  ( -1.181102362204723644, -0.1870078740157480879, -0.4822834645669291653 ) ) ;
#23125 = CARTESIAN_POINT ( 'NONE',  ( 0.3917322834645670104, -0.1049643490035303411, -1.928477690288713742 ) ) ;
#23126 = CARTESIAN_POINT ( 'NONE',  ( 0.8792650918635177559, -0.3690944881889765550, -0.3153832671262227771 ) ) ;
#23127 = CARTESIAN_POINT ( 'NONE',  ( 0.01312335958005323398, -0.4281496062992127816, -0.4176697321401328100 ) ) ;
#23128 = CARTESIAN_POINT ( 'NONE',  ( -0.4133858267716528645, -0.5400638737290844871, 0.3530559997133364547 ) ) ;
#23129 = CARTESIAN_POINT ( 'NONE',  ( -0.5905511811023613777, -0.5511811023622047445, 6.969142054262312111E-17 ) ) ;
#23130 = DIRECTION ( 'NONE',  ( 0.000000000000000000, -0.000000000000000000, 1.000000000000000000 ) ) ;
#23131 = CARTESIAN_POINT ( 'NONE',  ( -0.5577427821522301654, -0.2845877964562159024, 0.3641732283464567677 ) ) ;
#23132 = CARTESIAN_POINT ( 'NONE',  ( 0.4330708661417329575, 0.2952755905511811885, 0.000000000000000000 ) ) ;
#23133 = CARTESIAN_POINT ( 'NONE',  ( -0.9776902887139098386, -0.5511811023622046335, 0.09757992244046803654 ) ) ;
#23134 = CARTESIAN_POINT ( 'NONE',  ( 0.3460692066303959202, -0.1998031496062991630, -1.284120734908136496 ) ) ;
#23135 = CARTESIAN_POINT ( 'NONE',  ( 1.548556430446194954, -0.6046776061558807314, 0.2411417322834647770 ) ) ;
#23136 = ORIENTED_EDGE ( 'NONE', *, *, #16862, .T. ) ;
#23137 = CARTESIAN_POINT ( 'NONE',  ( -1.725721784776902190, -0.08942795157527998196, 0.3641732283464567121 ) ) ;
#23138 = CARTESIAN_POINT ( 'NONE',  ( -0.4199475065616791736, 0.2306618581243847221, -0.2411417322834647770 ) ) ;
#23139 = CARTESIAN_POINT ( 'NONE',  ( -1.076115485564303809, -0.6046776061558809534, -0.2411417322834644161 ) ) ;
#23140 = CARTESIAN_POINT ( 'NONE',  ( -0.3392501089628017219, -0.1958661417322836718, -1.711942257217847763 ) ) ;
#23141 = CARTESIAN_POINT ( 'NONE',  ( 0.4091458600556404646, -0.2362204724409448231, -2.152230971128608950 ) ) ;
#23142 = CARTESIAN_POINT ( 'NONE',  ( 1.437007874015748810, -0.5400638737290845981, -0.3530559997133363437 ) ) ;
#23143 = CARTESIAN_POINT ( 'NONE',  ( 0.3608923884514443348, -0.6692913385826771977, 0.1292274648535927661 ) ) ;
#23144 = CARTESIAN_POINT ( 'NONE',  ( 0.1208384647389237204, -0.3726288332213487653, -2.755905511811024056 ) ) ;
#23145 = CARTESIAN_POINT ( 'NONE',  ( -0.1070741851644051862, -0.3996062992125986035, -2.196194225721784576 ) ) ;
#23146 = CARTESIAN_POINT ( 'NONE',  ( 1.522309711286089939, -0.5023911411419708095, -0.1820866141732282451 ) ) ;
#23147 = CARTESIAN_POINT ( 'NONE',  ( 0.3460692066303959202, 0.1998031496062993295, -0.9186351706036745002 ) ) ;
#23148 = ORIENTED_EDGE ( 'NONE', *, *, #75249, .T. ) ;
#23149 = CARTESIAN_POINT ( 'NONE',  ( -1.069553805774277722, -0.5511811023622048555, -0.09757992244046775898 ) ) ;
#23150 = CARTESIAN_POINT ( 'NONE',  ( 0.1049643490035304938, -0.3917322834645669549, -2.439632545931758045 ) ) ;
#23151 = VERTEX_POINT ( 'NONE', #11503 ) ;
#23152 = CARTESIAN_POINT ( 'NONE',  ( 0.7874015748031503170, -0.1870078740157479769, 0.4822834645669291653 ) ) ;
#23153 = CARTESIAN_POINT ( 'NONE',  ( -0.3543307086614165824, -0.6692913385826771977, 8.415575281601705876E-17 ) ) ;
#23154 = CARTESIAN_POINT ( 'NONE',  ( -1.017060367454067249, -0.05778040916215522460, 0.4822834645669289988 ) ) ;
#23155 = CARTESIAN_POINT ( 'NONE',  ( 1.076115485564305141, 0.2306618581243847221, -0.2411417322834647770 ) ) ;
#23156 = CARTESIAN_POINT ( 'NONE',  ( -1.141732283464566011, 0.1771653543307087630, 0.000000000000000000 ) ) ;
#23157 = CARTESIAN_POINT ( 'NONE',  ( 0.000000000000000000, 0.000000000000000000, 0.000000000000000000 ) ) ;
#23158 = CARTESIAN_POINT ( 'NONE',  ( 0.1902887139107617975, -0.6692913385826773087, -0.1292274648535924053 ) ) ;
#23159 = CARTESIAN_POINT ( 'NONE',  ( -0.8858267716535425107, -0.5400638737290844871, 0.3530559997133364547 ) ) ;
#23160 = CARTESIAN_POINT ( 'NONE',  ( 4.797336870675655290E-17, -0.3917322834645669549, -1.733576484743095669 ) ) ;
#23161 = DIRECTION ( 'NONE',  ( 1.000000000000000000, 0.000000000000000000, 0.000000000000000000 ) ) ;
#23162 = CARTESIAN_POINT ( 'NONE',  ( 0.3726288332213487653, 0.1208384647389236927, -1.220472440944882164 ) ) ;
#23163 = CARTESIAN_POINT ( 'NONE',  ( 1.062992125984252745, 0.2952755905511811885, 0.000000000000000000 ) ) ;
#23164 = CARTESIAN_POINT ( 'NONE',  ( -0.1049643490035307020, 0.3917322834645669549, -2.768372703412072866 ) ) ;
#23165 = CARTESIAN_POINT ( 'NONE',  ( 1.312335958005250269, -0.5023911411419708095, 0.1820866141732285504 ) ) ;
#23166 = VERTEX_POINT ( 'NONE', #29194 ) ;
#23167 = CARTESIAN_POINT ( 'NONE',  ( -0.1058382717557503211, 0.3949938075777409408, 0.1509186351706036378 ) ) ;
#23168 = CARTESIAN_POINT ( 'NONE',  ( -0.5118110236220466680, 0.2952755905511811885, 0.000000000000000000 ) ) ;
#23169 = ORIENTED_EDGE ( 'NONE', *, *, #28151, .T. ) ;
#23170 = CARTESIAN_POINT ( 'NONE',  ( 0.3215223097112867578, -0.08942795157527998196, 0.3641732283464567121 ) ) ;
#23171 = CARTESIAN_POINT ( 'NONE',  ( -1.443569553805773564, -0.6046776061558807314, 0.2411417322834647770 ) ) ;
#23172 = CARTESIAN_POINT ( 'NONE',  ( 0.6036745406824153282, -0.6046776061558807314, 0.2411417322834647770 ) ) ;
#23173 = CARTESIAN_POINT ( 'NONE',  ( 0.7152230971128614723, -0.3162353388693409650, -0.4822834645669289433 ) ) ;
#23174 = CARTESIAN_POINT ( 'NONE',  ( -0.01312335958005186876, -0.4281496062992124485, 0.4176697321401328655 ) ) ;
#23175 = CARTESIAN_POINT ( 'NONE',  ( 0.3917322834645670659, 2.398668435337828261E-17, -1.217210916831708012 ) ) ;
#23176 = CARTESIAN_POINT ( 'NONE',  ( -0.6299212598425188991, -0.1870078740157480879, -0.4822834645669291653 ) ) ;
#23177 = CARTESIAN_POINT ( 'NONE',  ( 0.3917322834645670104, -0.1049643490035303411, -2.085958005249344271 ) ) ;
#23178 = CARTESIAN_POINT ( 'NONE',  ( -1.541994750656167090, 0.2952755905511811885, 0.1292274648535926551 ) ) ;
#23179 = CARTESIAN_POINT ( 'NONE',  ( -0.8989501312335946848, -0.6692913385826771977, 0.1292274648535927661 ) ) ;
#23180 = CARTESIAN_POINT ( 'NONE',  ( 1.404199475065617708, 0.05413385826771626580, -0.4176697321401330321 ) ) ;
#23181 = CARTESIAN_POINT ( 'NONE',  ( 1.082677165354331228, 0.1660481256975883668, -0.3530559997133364547 ) ) ;
#23182 = CARTESIAN_POINT ( 'NONE',  ( 0.3996062992125986035, 0.1070741851644054776, -0.5971128608923884640 ) ) ;
#23183 = CARTESIAN_POINT ( 'NONE',  ( -1.128608923884513837, -0.6046776061558807314, 0.2411417322834647770 ) ) ;
#23184 = CARTESIAN_POINT ( 'NONE',  ( -0.1998031496062994405, 0.3460692066303957537, 0.2250656167979002698 ) ) ;
#23185 = CARTESIAN_POINT ( 'NONE',  ( 0.1574803149606306130, -0.1870078740157479769, 0.4822834645669291653 ) ) ;
#23186 = CARTESIAN_POINT ( 'NONE',  ( -0.1998031496062994683, 0.3460692066303958092, -2.217847769028871596 ) ) ;
#23187 = CARTESIAN_POINT ( 'NONE',  ( -0.4330708661417315697, -0.6692913385826771977, 8.415575281601705876E-17 ) ) ;
#23188 = CARTESIAN_POINT ( 'NONE',  ( 1.660104986876641320, -0.05778040916215522460, 0.4822834645669289988 ) ) ;
#23189 = CARTESIAN_POINT ( 'NONE',  ( 0.6430446194225729606, -0.3690944881889765550, -0.3153832671262227771 ) ) ;
#23190 = CARTESIAN_POINT ( 'NONE',  ( 1.325459317585302665, 0.05413385826771626580, -0.4176697321401330321 ) ) ;
#23191 = CARTESIAN_POINT ( 'NONE',  ( -0.1265901696524986964, -0.4724409448818899238, -0.9363517060367454459 ) ) ;
#23192 = CARTESIAN_POINT ( 'NONE',  ( 0.5774278215223104249, 0.1283753931104748280, 0.1820866141732283561 ) ) ;
#23193 = CARTESIAN_POINT ( 'NONE',  ( 0.9251968503937015864, -0.5400638737290844871, 0.3530559997133364547 ) ) ;
#23194 = VECTOR ( 'NONE', #15877, 39.37007874015748143 ) ;
#23195 = CARTESIAN_POINT ( 'NONE',  ( -0.3949938075777409963, -7.255918531996591613E-17, -0.5885826771653542844 ) ) ;
#23196 = CARTESIAN_POINT ( 'NONE',  ( -0.8792650918635160906, 0.05413385826771626580, -0.4176697321401330321 ) ) ;
#23197 = CARTESIAN_POINT ( 'NONE',  ( -1.614173228346457378, 2.157411728916712068, 0.1372047244094476981 ) ) ;
#23198 = CARTESIAN_POINT ( 'NONE',  ( 1.240157480314961314, -0.4536011799217367080, 0.2665933059059888421 ) ) ;
#23199 = CARTESIAN_POINT ( 'NONE',  ( -0.7742782152230965886, 0.05413385826771666132, 0.4176697321401328100 ) ) ;
#23200 = CARTESIAN_POINT ( 'NONE',  ( 0.1706036745406830368, 0.05413385826771666132, 0.4176697321401328100 ) ) ;
#23201 = CARTESIAN_POINT ( 'NONE',  ( 0.1443569553805781891, 0.009842519685039147898, -0.3409548833797004797 ) ) ;
#23202 = CARTESIAN_POINT ( 'NONE',  ( 0.07217847769028949700, -0.05778040916215560624, -0.4822834645669293319 ) ) ;
#23203 = CARTESIAN_POINT ( 'NONE',  ( 0.3280839895013130669, -0.3690944881889765550, -0.3153832671262227771 ) ) ;
#23204 = FACE_OUTER_BOUND ( 'NONE', #37674, .T. ) ;
#23205 = CARTESIAN_POINT ( 'NONE',  ( 0.05249343832021075018, -0.5023911411419708095, 0.1820866141732285504 ) ) ;
#23206 = CARTESIAN_POINT ( 'NONE',  ( 0.8792650918635177559, -0.3690944881889765550, -0.3153832671262227771 ) ) ;
#23207 = CARTESIAN_POINT ( 'NONE',  ( 3.937007874015748143, 1.537401574803149984, 2.901595197523589142E-16 ) ) ;
#23208 = CARTESIAN_POINT ( 'NONE',  ( -0.1998031496062994405, 0.3460692066303957537, -1.822178477690288956 ) ) ;
#23209 = CARTESIAN_POINT ( 'NONE',  ( 0.4986876640419954376, -0.6046776061558809534, -0.2411417322834644161 ) ) ;
#23210 = ADVANCED_FACE ( 'NONE', ( #62841 ), #70703, .F. ) ;
#23211 = CARTESIAN_POINT ( 'NONE',  ( 0.3392501089628018329, 0.1958661417322835607, -1.225721784776902634 ) ) ;
#23212 = CARTESIAN_POINT ( 'NONE',  ( 1.541994750656168645, 0.1771653543307087075, -0.09757992244046823083 ) ) ;
#23213 = CARTESIAN_POINT ( 'NONE',  ( -0.1614515132151654597, 0.3594585737333474973, 1.112018681666451376E-17 ) ) ;
#23214 = CARTESIAN_POINT ( 'NONE',  ( 0.08530183727034192087, -0.2845877964562161244, -0.3641732283464567121 ) ) ;
#23215 = CARTESIAN_POINT ( 'NONE',  ( 0.08530183727034192087, -0.05778040916215522460, 0.4822834645669289988 ) ) ;
#23216 = CARTESIAN_POINT ( 'NONE',  ( 1.259842519685040019, -0.1870078740157480601, -0.3641732283464567677 ) ) ;
#23217 = CARTESIAN_POINT ( 'NONE',  ( -1.332020997375327642, -0.2845877964562161244, -0.3641732283464567121 ) ) ;
#23218 = CARTESIAN_POINT ( 'NONE',  ( -1.299212598425196097, -0.6692913385826771977, 8.415575281601705876E-17 ) ) ;
#23219 = CARTESIAN_POINT ( 'NONE',  ( 0.2296587926509192634, -0.3162353388693405765, 0.4822834645669290543 ) ) ;
#23220 = CARTESIAN_POINT ( 'NONE',  ( 1.167979002624672580, -0.4281496062992124485, 0.4176697321401328655 ) ) ;
#23221 = CARTESIAN_POINT ( 'NONE',  ( 1.595398199321655275, 1.309738123151863665, -0.1559797534342494130 ) ) ;
#23222 = CARTESIAN_POINT ( 'NONE',  ( 0.3608923884514443348, 0.2952755905511810774, -0.1292274648535930714 ) ) ;
#23223 = CARTESIAN_POINT ( 'NONE',  ( 1.272965879265092637, -0.4281496062992127816, -0.4176697321401328100 ) ) ;
#23224 = CARTESIAN_POINT ( 'NONE',  ( 1.102362204724410155, -0.1870078740157480879, -0.4822834645669291653 ) ) ;
#23225 = CARTESIAN_POINT ( 'NONE',  ( -1.673228346456691717, 0.07958543189024071263, -0.2665933059059888421 ) ) ;
#23226 = CARTESIAN_POINT ( 'NONE',  ( 0.8727034120734913358, -0.08942795157527998196, 0.3641732283464567121 ) ) ;
#23227 = CARTESIAN_POINT ( 'NONE',  ( 1.482939632545932307, -0.4281496062992124485, 0.4176697321401328655 ) ) ;
#23228 = CARTESIAN_POINT ( 'NONE',  ( -0.04593175853018302557, -0.5511811023622048555, -0.09757992244046775898 ) ) ;
#23229 = CARTESIAN_POINT ( 'NONE',  ( -0.4396325459317577122, -0.6692913385826773087, -0.1292274648535924053 ) ) ;
#23230 = CARTESIAN_POINT ( 'NONE',  ( 0.6167979002624678353, -0.4281496062992124485, 0.4176697321401328655 ) ) ;
#23231 = CARTESIAN_POINT ( 'NONE',  ( -0.3215223097112853146, -0.05778040916215560624, -0.4822834645669293319 ) ) ;
#23232 = CIRCLE ( 'NONE', #411, 0.5120078740157480990 ) ;
#23233 = EDGE_CURVE ( 'NONE', #13300, #8463, #51821, .T. ) ;
#23234 = CARTESIAN_POINT ( 'NONE',  ( 0.3917322834645670659, -0.1049643490035303273, -2.155531126805461550 ) ) ;
#23235 = CARTESIAN_POINT ( 'NONE',  ( -0.1837270341207343505, -0.5023911411419708095, 0.1820866141732285504 ) ) ;
#23236 = CARTESIAN_POINT ( 'NONE',  ( 0.6102362204724416372, -0.5400638737290844871, 0.3530559997133364547 ) ) ;
#23237 = CARTESIAN_POINT ( 'NONE',  ( 1.030183727034121421, -0.08942795157527998196, 0.3641732283464567121 ) ) ;
#23238 = CARTESIAN_POINT ( 'NONE',  ( 0.4177787735907000366, 1.299212598425196985, -1.736336963694947944 ) ) ;
#23240 = CARTESIAN_POINT ( 'NONE',  ( -2.362204724409448620, 1.724409448818897905, 0.5118110236220224651 ) ) ;
#23239 = CARTESIAN_POINT ( 'NONE',  ( -1.732283464566928277, -0.1870078740157479769, 0.3641732283464567677 ) ) ;
#23241 = CARTESIAN_POINT ( 'NONE',  ( 2.158445410120265695, 1.605872332714552986, -0.4695140184743379352 ) ) ;
#23242 = CARTESIAN_POINT ( 'NONE',  ( -1.161417322834644716, 0.1660481256975885056, 0.3530559997133364547 ) ) ;
#23243 = CARTESIAN_POINT ( 'NONE',  ( -0.5314960629921254842, -0.5400638737290845981, -0.3530559997133363437 ) ) ;
#23244 = CARTESIAN_POINT ( 'NONE',  ( 5.785732909357575061E-17, -0.4724409448818898682, -0.07874015748031495954 ) ) ;
#23245 = CARTESIAN_POINT ( 'NONE',  ( -0.3949938075777409408, -0.1058382717557502933, -2.408136482939633449 ) ) ;
#23246 = VERTEX_POINT ( 'NONE', #22471 ) ;
#23247 = CARTESIAN_POINT ( 'NONE',  ( 0.5052493438320218022, -0.5511811023622048555, -0.09757992244046775898 ) ) ;
#23249 = CARTESIAN_POINT ( 'NONE',  ( 0.2867679344610365999, 0.2867679344610365999, -0.7598425196850391306 ) ) ;
#23248 = VECTOR ( 'NONE', #15383, 39.37007874015748143 ) ;
#23250 = CARTESIAN_POINT ( 'NONE',  ( 1.305774278215223960, 0.2952755905511810774, -0.1292274648535930714 ) ) ;
#23251 = CARTESIAN_POINT ( 'NONE',  ( -0.2362204724409451284, 0.4091458600556402425, -2.532808398950130879 ) ) ;
#23252 = CARTESIAN_POINT ( 'NONE',  ( 1.614173228346457378, 0.7166040191147859950, -0.1372047244094476148 ) ) ;
#23253 = CARTESIAN_POINT ( 'NONE',  ( -0.2952755905511805223, 0.1660481256975885056, 0.3530559997133364547 ) ) ;
#23254 = CARTESIAN_POINT ( 'NONE',  ( 1.686351706036745890, 0.2952755905511811885, 0.1292274648535926551 ) ) ;
#23255 = CARTESIAN_POINT ( 'NONE',  ( 1.253280839895013710, -0.2845877964562159024, 0.3641732283464567677 ) ) ;
#23256 = CARTESIAN_POINT ( 'NONE',  ( 0.3346456692913393205, -0.5400638737290845981, -0.3530559997133363437 ) ) ;
#23257 = CARTESIAN_POINT ( 'NONE',  ( -0.3917322834645668994, -0.1049643490035306742, -0.4409255661079247157 ) ) ;
#23258 = CARTESIAN_POINT ( 'NONE',  ( 0.07217847769028949700, -0.3162353388693405765, 0.4822834645669290543 ) ) ;
#23259 = CARTESIAN_POINT ( 'NONE',  ( -0.8070866141732276899, -0.4536011799217367080, 0.2665933059059888421 ) ) ;
#23260 = EDGE_CURVE ( 'NONE', #32253, #2483, #55264, .T. ) ;
#23261 = CARTESIAN_POINT ( 'NONE',  ( 0.5380577427821529035, 0.05413385826771626580, -0.4176697321401330321 ) ) ;
#23262 = CARTESIAN_POINT ( 'NONE',  ( -0.1706036745406816491, -0.4281496062992124485, 0.4176697321401328655 ) ) ;
#23263 = CARTESIAN_POINT ( 'NONE',  ( -1.614173228346456712, 2.094556775020298467, -0.1372047244094478091 ) ) ;
#23264 = CARTESIAN_POINT ( 'NONE',  ( 0.3996062992125986035, 2.446882876249141962E-17, -2.952755905511811108 ) ) ;
#23265 = CARTESIAN_POINT ( 'NONE',  ( 0.3392501089628018329, 0.1958661417322835607, -1.702775221293650443 ) ) ;
#23266 = CARTESIAN_POINT ( 'NONE',  ( 0.7086614173228353852, -0.1870078740157479769, 0.4822834645669291653 ) ) ;
#23267 = CARTESIAN_POINT ( 'NONE',  ( -0.3215223097112853146, -0.3162353388693405765, 0.4822834645669290543 ) ) ;
#23268 = CARTESIAN_POINT ( 'NONE',  ( -1.345144356955379816, -0.3162353388693405765, 0.4822834645669290543 ) ) ;
#23269 = CARTESIAN_POINT ( 'NONE',  ( 1.200787401574803681, -0.5400638737290845981, -0.3530559997133363437 ) ) ;
#23270 = CARTESIAN_POINT ( 'NONE',  ( 0.5708661417322842269, 0.1660481256975885056, 0.3530559997133364547 ) ) ;
#23271 = CARTESIAN_POINT ( 'NONE',  ( 0.3392501089628018884, -0.1958661417322834220, -1.134514435695538115 ) ) ;
#23272 = CARTESIAN_POINT ( 'NONE',  ( -0.3280839895013117347, -0.4281496062992124485, 0.4176697321401328655 ) ) ;
#23273 = CARTESIAN_POINT ( 'NONE',  ( 0.1706036745406830368, -0.4281496062992127816, -0.4176697321401328100 ) ) ;
#23274 = CARTESIAN_POINT ( 'NONE',  ( -0.3871391076115476282, -0.05778040916215522460, 0.4822834645669289988 ) ) ;
#23275 = CARTESIAN_POINT ( 'NONE',  ( 0.4658792650918641698, -0.08942795157528024563, -0.3641732283464568787 ) ) ;
#23276 = CARTESIAN_POINT ( 'NONE',  ( 1.627296587926509996, -0.5023911411419708095, 0.1820866141732285504 ) ) ;
#23277 = CARTESIAN_POINT ( 'NONE',  ( -0.4122598602536396428, 1.300945800302086619, -2.666505492093648844 ) ) ;
#23278 = CARTESIAN_POINT ( 'NONE',  ( 0.4724409448818904789, -0.1870078740157479769, 0.4822834645669291653 ) ) ;
#23279 =( NAMED_UNIT ( * ) PLANE_ANGLE_UNIT ( ) SI_UNIT ( $, .RADIAN. ) );
#23280 = CARTESIAN_POINT ( 'NONE',  ( 1.345144356955381593, -0.3162353388693409650, -0.4822834645669289433 ) ) ;
#23281 = CARTESIAN_POINT ( 'NONE',  ( 0.2867679344610365999, 0.2867679344610365999, -2.492125984251968518 ) ) ;
#23282 = VERTEX_POINT ( 'NONE', #23287 ) ;
#23283 = ORIENTED_EDGE ( 'NONE', *, *, #35630, .F. ) ;
#23284 = CARTESIAN_POINT ( 'NONE',  ( 0.5839895013123367340, 0.2952755905511811885, 0.1292274648535926551 ) ) ;
#23285 = CARTESIAN_POINT ( 'NONE',  ( 0.3805774278215230400, -0.004921259842519870586, -0.3153832671262229437 ) ) ;
#23287 = CARTESIAN_POINT ( 'NONE',  ( -0.2952755905511810774, 1.832348042626885162E-19, 5.524802951929911998 ) ) ;
#23286 = CARTESIAN_POINT ( 'NONE',  ( 1.686351706036745890, 0.1771653543307087630, 0.09757992244046791164 ) ) ;
#23288 = CARTESIAN_POINT ( 'NONE',  ( -0.1049643490035302024, -0.3917322834645671215, -0.7867454068241470644 ) ) ;
#23289 = CARTESIAN_POINT ( 'NONE',  ( 0.3458507752293908943, -0.3458507752293908943, -0.01771653543307087630 ) ) ;
#23290 = CARTESIAN_POINT ( 'NONE',  ( 2.362204724409448620, 0.03937007874015751446, 0.5118110236220555498 ) ) ;
#23291 = CARTESIAN_POINT ( 'NONE',  ( -0.2925321140481932369, 0.2925321140481931259, -2.301181102362204633 ) ) ;
#23292 = CARTESIAN_POINT ( 'NONE',  ( 0.7283464566929140904, -0.5400638737290845981, -0.3530559997133363437 ) ) ;
#23293 = CARTESIAN_POINT ( 'NONE',  ( -0.7545931758530176614, -0.6692913385826773087, -0.1292274648535924053 ) ) ;
#23294 = VECTOR ( 'NONE', #79781, 39.37007874015748143 ) ;
#23295 = CARTESIAN_POINT ( 'NONE',  ( -0.7742782152230965886, 0.05413385826771666132, 0.4176697321401328100 ) ) ;
#23296 = CARTESIAN_POINT ( 'NONE',  ( 0.4724409448818904789, -0.1870078740157479769, 0.4822834645669291653 ) ) ;
#23297 = CARTESIAN_POINT ( 'NONE',  ( 1.266404199475066328, -0.05778040916215522460, 0.4822834645669289988 ) ) ;
#23298 = CARTESIAN_POINT ( 'NONE',  ( -0.3503937007874015630, -0.3733313776025732333, -0.4921259842519685179 ) ) ;
#23299 = APPLICATION_PROTOCOL_DEFINITION ( 'draft international standard', 'automotive_design', 1998, #25567 ) ;
#23300 = CARTESIAN_POINT ( 'NONE',  ( 1.364829396325460076, 0.1283753931104748280, 0.1820866141732283561 ) ) ;
#23301 = CARTESIAN_POINT ( 'NONE',  ( -0.2925321140481930149, -0.2925321140481933480, -2.025590551181102317 ) ) ;
#23302 = CARTESIAN_POINT ( 'NONE',  ( -1.489501312335957062, -0.08942795157527998196, 0.3641732283464567121 ) ) ;
#23303 = CARTESIAN_POINT ( 'NONE',  ( 1.604771003085129433, 0.7690346235818159570, 0.1466069496707750608 ) ) ;
#23304 = CARTESIAN_POINT ( 'NONE',  ( 0.3346456692913393205, -0.5400638737290845981, -0.3530559997133363437 ) ) ;
#23306 = CARTESIAN_POINT ( 'NONE',  ( 0.5314960629920851831, 2.559055118110236560, 3.900966923095595451 ) ) ;
#23305 = CARTESIAN_POINT ( 'NONE',  ( 1.102362204724410155, -0.1870078740157480879, -0.4822834645669291653 ) ) ;
#23307 = CARTESIAN_POINT ( 'NONE',  ( -1.358267716535432434, 0.07958543189024071263, -0.2665933059059888421 ) ) ;
#23308 = CARTESIAN_POINT ( 'NONE',  ( 0.3280839895013130669, -0.4281496062992127816, -0.4176697321401328100 ) ) ;
#23309 = CARTESIAN_POINT ( 'NONE',  ( 1.089238845144357537, -0.3690944881889763329, 0.3153832671262228327 ) ) ;
#23310 = CARTESIAN_POINT ( 'NONE',  ( 0.2867679344610365999, 0.2867679344610365999, -1.635151287892701255 ) ) ;
#23311 = AXIS2_PLACEMENT_3D ( 'NONE', #14490, #60330, #51913 ) ;
#23312 = CARTESIAN_POINT ( 'NONE',  ( -1.358267716535432434, 0.07958543189024071263, -0.2665933059059888421 ) ) ;
#23313 = CARTESIAN_POINT ( 'NONE',  ( 1.377952755905512472, 0.2952755905511811885, 0.000000000000000000 ) ) ;
#23314 = CARTESIAN_POINT ( 'NONE',  ( 0.2451238321738833381, 1.888229281464673948, 0.1947436408813261743 ) ) ;
#23315 = CARTESIAN_POINT ( 'NONE',  ( 0.07874015748031558404, -0.1870078740157480601, -0.3641732283464567677 ) ) ;
#23316 = CARTESIAN_POINT ( 'NONE',  ( -0.07217847769028813698, -0.3162353388693409650, -0.4822834645669289433 ) ) ;
#23317 = CARTESIAN_POINT ( 'NONE',  ( -1.167979002624671470, -0.004921259842519576551, 0.3153832671262227771 ) ) ;
#23318 = CARTESIAN_POINT ( 'NONE',  ( -0.7545931758530177724, 0.2952755905511811885, 0.1292274648535926551 ) ) ;
#23319 = CARTESIAN_POINT ( 'NONE',  ( 1.345144356955381593, -0.05778040916215522460, 0.4822834645669289988 ) ) ;
#23320 = CARTESIAN_POINT ( 'NONE',  ( -0.2867679344610365444, -0.2867679344610367664, -0.6857148538395820836 ) ) ;
#23321 = CARTESIAN_POINT ( 'NONE',  ( 0.4177787735906999811, 1.312623414240995157, -1.714017618091133288 ) ) ;
#23322 = CARTESIAN_POINT ( 'NONE',  ( 1.312335958005249825, 0.2306618581243847221, -0.2411417322834647770 ) ) ;
#23323 = CARTESIAN_POINT ( 'NONE',  ( 0.3458507752293908943, -0.3458507752293908943, -1.907480314960629197 ) ) ;
#23324 = CARTESIAN_POINT ( 'NONE',  ( -1.069553805774277722, 0.2952755905511811885, 0.1292274648535926551 ) ) ;
#23325 = CARTESIAN_POINT ( 'NONE',  ( -1.141732283464566011, 0.1771653543307087630, 0.000000000000000000 ) ) ;
#23326 = CARTESIAN_POINT ( 'NONE',  ( -0.5446194225721777693, -0.2845877964562161244, -0.3641732283464567121 ) ) ;
#23327 = DIRECTION ( 'NONE',  ( 8.659560562354975999E-17, -0.7071067811865437980, 0.7071067811865511255 ) ) ;
#23328 = CARTESIAN_POINT ( 'NONE',  ( 0.02624671916010564918, -0.6046776061558809534, -0.2411417322834644161 ) ) ;
#23329 = CARTESIAN_POINT ( 'NONE',  ( -0.01968503937007793844, 0.07958543189024071263, -0.2665933059059888421 ) ) ;
#23330 = CARTESIAN_POINT ( 'NONE',  ( -1.161417322834644716, -0.4536011799217368745, -0.2665933059059886201 ) ) ;
#23331 = CARTESIAN_POINT ( 'NONE',  ( -1.548556430446193399, 0.2306618581243848609, 0.2411417322834645549 ) ) ;
#23332 = CARTESIAN_POINT ( 'NONE',  ( 1.482939632545932307, -0.004921259842519870586, -0.3153832671262229437 ) ) ;
#23333 = CARTESIAN_POINT ( 'NONE',  ( 1.266404199475066328, -0.3162353388693409650, -0.4822834645669289433 ) ) ;
#23334 = DIRECTION ( 'NONE',  ( 0.000000000000000000, 0.000000000000000000, 1.000000000000000000 ) ) ;
#23335 = CARTESIAN_POINT ( 'NONE',  ( 0.6102362204724416372, 0.07958543189024071263, -0.2665933059059888421 ) ) ;
#23336 = CARTESIAN_POINT ( 'NONE',  ( 0.8136482939632553313, -0.6046776061558809534, -0.2411417322834644161 ) ) ;
#23337 = ADVANCED_FACE ( 'NONE', ( #62416 ), #73828, .F. ) ;
#23338 = CARTESIAN_POINT ( 'NONE',  ( 0.8661417322834652488, -0.1870078740157480601, -0.3641732283464567677 ) ) ;
#23339 = ORIENTED_EDGE ( 'NONE', *, *, #42958, .F. ) ;
#23340 = CARTESIAN_POINT ( 'NONE',  ( -1.377952755905511140, -0.6692913385826771977, 8.415575281601705876E-17 ) ) ;
#23341 = CARTESIAN_POINT ( 'NONE',  ( -0.7152230971128602510, -0.3162353388693405765, 0.4822834645669290543 ) ) ;
#23342 = CARTESIAN_POINT ( 'NONE',  ( -0.1968503937007867743, -0.6692913385826771977, 8.415575281601705876E-17 ) ) ;
#23343 = DIRECTION ( 'NONE',  ( 0.000000000000000000, 0.000000000000000000, 1.000000000000000000 ) ) ;
#23344 = CARTESIAN_POINT ( 'NONE',  ( 0.2925321140481932369, -0.2925321140481931814, -2.379921259842520342 ) ) ;
#23345 = CARTESIAN_POINT ( 'NONE',  ( 0.8398950131233602345, 0.2306618581243847221, -0.2411417322834647770 ) ) ;
#23346 = CARTESIAN_POINT ( 'NONE',  ( 1.318897637795276356, 0.07958543189024071263, -0.2665933059059888421 ) ) ;
#23347 = CARTESIAN_POINT ( 'NONE',  ( -0.1246719160104980823, -0.6692913385826773087, -0.1292274648535924053 ) ) ;
#23348 = CARTESIAN_POINT ( 'NONE',  ( 0.8858267716535438430, -0.5400638737290845981, -0.3530559997133363437 ) ) ;
#23349 = CARTESIAN_POINT ( 'NONE',  ( -0.3996062992125986035, -7.340648628747425578E-17, -1.614173228346456712 ) ) ;
#23350 = CARTESIAN_POINT ( 'NONE',  ( -0.3949938075777411628, 0.1058382717557497937, -0.9776902887139109488 ) ) ;
#23351 = CARTESIAN_POINT ( 'NONE',  ( -9.787531504996567848E-17, 0.3996062992125986035, -2.519685039370078705 ) ) ;
#23352 = FACE_OUTER_BOUND ( 'NONE', #619, .T. ) ;
#23353 = AXIS2_PLACEMENT_3D ( 'NONE', #74900, #17248, #43282 ) ;
#23354 = CARTESIAN_POINT ( 'NONE',  ( 0.3917322834645670104, -0.1049643490035303273, -0.4186351706036745557 ) ) ;
#23355 = CARTESIAN_POINT ( 'NONE',  ( -0.5249343832020990641, -0.5023911411419708095, -0.1820866141732282451 ) ) ;
#23356 = CARTESIAN_POINT ( 'NONE',  ( -0.5774278215223089816, 0.2306618581243847221, -0.2411417322834647770 ) ) ;
#23357 = CARTESIAN_POINT ( 'NONE',  ( 1.043307086614173818, -0.5400638737290845981, -0.3530559997133363437 ) ) ;
#23358 = CARTESIAN_POINT ( 'NONE',  ( -0.3420746716998662729, 0.1974969037888702206, -2.150262467191601523 ) ) ;
#23359 = CARTESIAN_POINT ( 'NONE',  ( -1.574803149606298192, -0.1870078740157480879, -0.4822834645669291653 ) ) ;
#23360 = CARTESIAN_POINT ( 'NONE',  ( 1.030183727034121421, -0.3162353388693409650, -0.4822834645669289433 ) ) ;
#23361 = CARTESIAN_POINT ( 'NONE',  ( -0.2362204724409451284, 0.4091458600556402425, -2.532808398950130879 ) ) ;
#23362 = CARTESIAN_POINT ( 'NONE',  ( -0.3996062992125986035, -7.340648628747425578E-17, -1.614173228346456712 ) ) ;
#23363 = CARTESIAN_POINT ( 'NONE',  ( 0.000000000000000000, 0.000000000000000000, 0.000000000000000000 ) ) ;
#23364 = ADVANCED_FACE ( 'NONE', ( #42642 ), #68339, .T. ) ;
#23365 = CARTESIAN_POINT ( 'NONE',  ( 0.8858267716535438430, -0.5400638737290845981, -0.3530559997133363437 ) ) ;
#23366 = TOROIDAL_SURFACE ( 'NONE', #58321, 0.1574803149606295860, 0.01968503937007873988 ) ;
#23367 = CARTESIAN_POINT ( 'NONE',  ( 1.102362204724410155, -0.1870078740157479769, 0.3641732283464567677 ) ) ;
#23368 = PRODUCT_DEFINITION ( 'UNKNOWN', '', #2033, #63882 ) ;
#23370 = CARTESIAN_POINT ( 'NONE',  ( -1.489501312335957062, -0.05778040916215522460, 0.4822834645669289988 ) ) ;
#23369 = CARTESIAN_POINT ( 'NONE',  ( 1.607611548556431069, -0.6692913385826773087, -0.1292274648535924053 ) ) ;
#23371 = CARTESIAN_POINT ( 'NONE',  ( -0.2867679344610366554, 0.2867679344610365444, -2.776883571357268821 ) ) ;
#23372 = DIRECTION ( 'NONE',  ( -3.491481338843132961E-15, -0.000000000000000000, 1.000000000000000000 ) ) ;
#23373 = CARTESIAN_POINT ( 'NONE',  ( 0.9055118110236227702, 0.2952755905511811885, 0.000000000000000000 ) ) ;
#23374 = CARTESIAN_POINT ( 'NONE',  ( 1.371391076115485941, 0.1771653543307087630, 0.09757992244046791164 ) ) ;
#23375 = CARTESIAN_POINT ( 'NONE',  ( -0.3674540682414692561, -0.6046776061558809534, -0.2411417322834644161 ) ) ;
#23376 = CARTESIAN_POINT ( 'NONE',  ( -0.4790026246719154557, -0.3162353388693405765, 0.4822834645669290543 ) ) ;
#23377 = CARTESIAN_POINT ( 'NONE',  ( 1.541994750656168645, -0.6692913385826771977, 0.1292274648535927661 ) ) ;
#23378 = CARTESIAN_POINT ( 'NONE',  ( -0.1958661417322834220, -0.3392501089628018884, 0.007217847769028785422 ) ) ;
#23379 = CARTESIAN_POINT ( 'NONE',  ( 0.1049868766404206816, -0.6046776061558809534, -0.2411417322834644161 ) ) ;
#23380 = CARTESIAN_POINT ( 'NONE',  ( 4.797336870675656522E-17, -0.3917322834645670104, -2.433070866141732402 ) ) ;
#23381 = CARTESIAN_POINT ( 'NONE',  ( 1.646981627296588035, -0.3162353388693405765, 0.4822834645669290543 ) ) ;
#23382 = ORIENTED_EDGE ( 'NONE', *, *, #79680, .T. ) ;
#23383 = CARTESIAN_POINT ( 'NONE',  ( -0.3949938075777409408, -0.1058382717557502933, -2.565616797900262647 ) ) ;
#23384 = ORIENTED_EDGE ( 'NONE', *, *, #63827, .F. ) ;
#23385 = FACE_OUTER_BOUND ( 'NONE', #1534, .T. ) ;
#23386 = CARTESIAN_POINT ( 'NONE',  ( -1.679790026246718693, 0.2306618581243847221, -0.2411417322834647770 ) ) ;
#23387 = CARTESIAN_POINT ( 'NONE',  ( -0.3460692066303960868, 0.1998031496062990242, -1.128608923884514503 ) ) ;
#23388 = CARTESIAN_POINT ( 'NONE',  ( 1.679790026246720025, 0.1283753931104748280, 0.1820866141732283561 ) ) ;
#23389 = CARTESIAN_POINT ( 'NONE',  ( -0.1049868766404193215, 0.1539470093639521697, -0.1968503937007875793 ) ) ;
#23390 = CARTESIAN_POINT ( 'NONE',  ( 0.4037097067573611753, 1.223219560026271499E-15, 0.4445507791589056734 ) ) ;
#23391 = CARTESIAN_POINT ( 'NONE',  ( 0.9333857237505069904, -6.978086149529499157E-16, -0.3791475997938232867 ) ) ;
#23392 = EDGE_CURVE ( 'NONE', #76416, #2295, #73442, .T. ) ;
#23393 = CARTESIAN_POINT ( 'NONE',  ( 0.1049643490035304938, -0.3917322834645669549, -0.4849081364829396779 ) ) ;
#23394 = CARTESIAN_POINT ( 'NONE',  ( -0.1443569553805765515, -0.3690944881889765550, -0.3153832671262227771 ) ) ;
#23395 = CARTESIAN_POINT ( 'NONE',  ( -1.003937007874015297, -0.4536011799217368745, -0.2665933059059886201 ) ) ;
#23396 = CARTESIAN_POINT ( 'NONE',  ( 1.522309711286089939, -0.6046776061558809534, -0.2411417322834644161 ) ) ;
#23397 = EDGE_CURVE ( 'NONE', #63914, #74015, #36740, .T. ) ;
#23398 = CARTESIAN_POINT ( 'NONE',  ( 0.4265091863517067039, -0.6692913385826773087, -0.1292274648535924053 ) ) ;
#23399 = CARTESIAN_POINT ( 'NONE',  ( -1.535433070866141225, -0.6692913385826771977, 8.415575281601705876E-17 ) ) ;
#23400 = CARTESIAN_POINT ( 'NONE',  ( 4.797336870675656522E-17, -0.3917322834645670104, -0.2283464566929133410 ) ) ;
#23401 = ORIENTED_EDGE ( 'NONE', *, *, #36816, .F. ) ;
#23402 = CARTESIAN_POINT ( 'NONE',  ( 1.450131233595801428, 0.2952755905511811885, 0.1292274648535926551 ) ) ;
#23403 = CARTESIAN_POINT ( 'NONE',  ( -1.586052503253845503, 2.125984251968505045, -0.1653254495020588799 ) ) ;
#23404 = CARTESIAN_POINT ( 'NONE',  ( 5.785732909357575061E-17, -0.4724409448818898682, -1.653543307086614123 ) ) ;
#23405 = CARTESIAN_POINT ( 'NONE',  ( 0.2087913723976025926, 0.2087913723976026203, 0.1248231986745541033 ) ) ;
#23406 = PLANE ( 'NONE',  #35853 ) ;
#23407 = CARTESIAN_POINT ( 'NONE',  ( -0.7808398950131222316, -0.3162353388693409650, -0.4822834645669289433 ) ) ;
#23408 = CARTESIAN_POINT ( 'NONE',  ( 1.515748031496063408, 0.1660481256975885056, 0.3530559997133364547 ) ) ;
#23410 = DIRECTION ( 'NONE',  ( 0.000000000000000000, 0.000000000000000000, 1.000000000000000000 ) ) ;
#23409 = CARTESIAN_POINT ( 'NONE',  ( -0.7186703366786194591, -2.567464376874931580E-15, -0.4445507791589072832 ) ) ;
#23411 = CARTESIAN_POINT ( 'NONE',  ( 1.587926509186352586, -0.4281496062992127816, -0.4176697321401328100 ) ) ;
#23412 = CARTESIAN_POINT ( 'NONE',  ( -0.7152230971128602510, -0.05778040916215560624, -0.4822834645669293319 ) ) ;
#23413 = CARTESIAN_POINT ( 'NONE',  ( 0.1049643490035304522, -0.3917322834645668994, -0.4802956448480821261 ) ) ;
#23414 = CARTESIAN_POINT ( 'NONE',  ( -0.01968503937007793844, -0.4536011799217367080, 0.2665933059059888421 ) ) ;
#23415 = CARTESIAN_POINT ( 'NONE',  ( -0.1958661417322834220, -0.3392501089628018884, -0.4652230971128609727 ) ) ;
#23416 = CIRCLE ( 'NONE', #47563, 1.244489337948954555 ) ;
#23417 = CARTESIAN_POINT ( 'NONE',  ( -0.1902887139107604098, 0.1771653543307087075, -0.09757992244046823083 ) ) ;
#23418 = CARTESIAN_POINT ( 'NONE',  ( 0.5971128608923890191, -0.5511811023622046335, 0.09757992244046803654 ) ) ;
#23419 = CARTESIAN_POINT ( 'NONE',  ( 0.3412073490813655186, 0.2306618581243848609, 0.2411417322834645549 ) ) ;
#23420 = CARTESIAN_POINT ( 'NONE',  ( -0.1509186351706028884, -0.2845877964562161244, -0.3641732283464567121 ) ) ;
#23421 = CARTESIAN_POINT ( 'NONE',  ( -0.1049643490035307020, 0.3917322834645669549, -2.518372703412073754 ) ) ;
#23422 = CARTESIAN_POINT ( 'NONE',  ( 1.496062992125984703, -0.1870078740157480879, -0.4822834645669291653 ) ) ;
#23423 = EDGE_CURVE ( 'NONE', #67465, #56386, #45144, .T. ) ;
#23424 = CARTESIAN_POINT ( 'NONE',  ( -1.030183727034119867, -0.3162353388693405765, 0.4822834645669290543 ) ) ;
#23425 = CARTESIAN_POINT ( 'NONE',  ( 0.3458507752293908943, 0.3458507752293908943, -0.6870078740157479213 ) ) ;
#23426 = CARTESIAN_POINT ( 'NONE',  ( -0.09842519685039295696, 0.1660481256975883668, -0.3530559997133364547 ) ) ;
#23427 = CARTESIAN_POINT ( 'NONE',  ( -0.3477690288713902178, 0.2952755905511810774, -0.1292274648535930714 ) ) ;
#23428 = CARTESIAN_POINT ( 'NONE',  ( 1.587926509186352586, -0.3690944881889765550, -0.3153832671262227771 ) ) ;
#23429 = EDGE_CURVE ( 'NONE', #80676, #4806, #65323, .T. ) ;
#23430 = CARTESIAN_POINT ( 'NONE',  ( -0.08530183727034056085, -0.08942795157528024563, -0.3641732283464568787 ) ) ;
#23431 = CARTESIAN_POINT ( 'NONE',  ( -0.3149606299212590610, -0.1870078740157479769, 0.4822834645669291653 ) ) ;
#23432 = CARTESIAN_POINT ( 'NONE',  ( -0.7283464566929126471, -0.5400638737290844871, 0.3530559997133364547 ) ) ;
#23433 = CARTESIAN_POINT ( 'NONE',  ( 1.522309711286089939, 0.1283753931104748280, 0.1820866141732283561 ) ) ;
#23434 = CARTESIAN_POINT ( 'NONE',  ( 0.09842519685039434474, 0.1660481256975885056, 0.3530559997133364547 ) ) ;
#23435 = VERTEX_POINT ( 'NONE', #56504 ) ;
#23436 = CARTESIAN_POINT ( 'NONE',  ( 0.3996062992125986035, -0.1070741851644052972, -2.078083989501312345 ) ) ;
#23437 = EDGE_CURVE ( 'NONE', #78176, #73035, #39762, .T. ) ;
#23438 = CARTESIAN_POINT ( 'NONE',  ( 0.9842519685039375910, 0.2952755905511811885, 0.000000000000000000 ) ) ;
#23439 = CARTESIAN_POINT ( 'NONE',  ( -0.4790026246719154557, -0.2845877964562159024, 0.3641732283464567677 ) ) ;
#23440 = CARTESIAN_POINT ( 'NONE',  ( -0.7677165354330699465, 0.1660481256975885056, 0.3530559997133364547 ) ) ;
#23441 = CARTESIAN_POINT ( 'NONE',  ( 1.174540682414699111, -0.3162353388693405765, 0.4822834645669290543 ) ) ;
#23442 = CARTESIAN_POINT ( 'NONE',  ( 0.7742782152230979209, 0.05413385826771626580, -0.4176697321401330321 ) ) ;
#23443 = CARTESIAN_POINT ( 'NONE',  ( -1.614173228346455824, 0.2952755905511811885, 0.000000000000000000 ) ) ;
#23444 = CARTESIAN_POINT ( 'NONE',  ( -0.9448818897637790704, -0.1870078740157479769, 0.3641732283464567677 ) ) ;
#23445 = CARTESIAN_POINT ( 'NONE',  ( -0.3460692066303957537, -0.1998031496062994405, -0.2867454068241469534 ) ) ;
#23446 = CARTESIAN_POINT ( 'NONE',  ( 0.3996062992125986035, 0.1070741851644054776, -0.5971128608923884640 ) ) ;
#23447 = CARTESIAN_POINT ( 'NONE',  ( -0.1058382717557503211, 0.3949938075777409408, 0.1509186351706036378 ) ) ;
#23448 = CARTESIAN_POINT ( 'NONE',  ( 0.03056273350766125496, -0.3973686378485505322, -8.612909436664462853E-17 ) ) ;
#23449 = CARTESIAN_POINT ( 'NONE',  ( 1.036745406824147508, -0.3690944881889765550, -0.3153832671262227771 ) ) ;
#23450 = CARTESIAN_POINT ( 'NONE',  ( 0.5052493438320215802, 0.2952755905511811885, 0.1292274648535926551 ) ) ;
#23451 = CARTESIAN_POINT ( 'NONE',  ( -1.555118110236219930, 0.1660481256975885056, 0.3530559997133364547 ) ) ;
#23452 = CARTESIAN_POINT ( 'NONE',  ( 0.2891555358219910499, -0.2891555358219909944, -0.8051181102362204856 ) ) ;
#23453 = CARTESIAN_POINT ( 'NONE',  ( 0.5971128608923891301, 0.1771653543307087075, -0.09757992244046823083 ) ) ;
#23454 = CARTESIAN_POINT ( 'NONE',  ( -0.3871391076115476282, -0.05778040916215522460, 0.4822834645669289988 ) ) ;
#23455 = CARTESIAN_POINT ( 'NONE',  ( -0.8398950131233585692, 0.2306618581243848609, 0.2411417322834645549 ) ) ;
#23456 = CARTESIAN_POINT ( 'NONE',  ( 1.253280839895013710, -0.05778040916215560624, -0.4822834645669293319 ) ) ;
#23457 = CARTESIAN_POINT ( 'NONE',  ( -0.3458507752293909498, 0.3458507752293907833, -1.279527559055118058 ) ) ;
#23458 = CARTESIAN_POINT ( 'NONE',  ( 0.1070741851644053666, 0.3996062992125986035, -2.355643044619422533 ) ) ;
#23459 = CARTESIAN_POINT ( 'NONE',  ( -0.1837270341207343505, -0.5023911411419708095, 0.1820866141732285504 ) ) ;
#23460 = VERTEX_POINT ( 'NONE', #32496 ) ;
#23461 = CARTESIAN_POINT ( 'NONE',  ( -0.3917322834645671770, 0.1049643490035302024, -0.6594681346794770693 ) ) ;
#23462 = ORIENTED_EDGE ( 'NONE', *, *, #34284, .T. ) ;
#23463 = CARTESIAN_POINT ( 'NONE',  ( -0.9973753280839886548, -0.6046776061558809534, -0.2411417322834644161 ) ) ;
#23464 = CARTESIAN_POINT ( 'NONE',  ( -0.05249343832020911260, 0.2306618581243848609, 0.2411417322834645549 ) ) ;
#23465 = CARTESIAN_POINT ( 'NONE',  ( -0.1706036745406816491, 0.05413385826771626580, -0.4176697321401330321 ) ) ;
#23466 = VECTOR ( 'NONE', #43991, 39.37007874015748143 ) ;
#23467 = CARTESIAN_POINT ( 'NONE',  ( 0.9120734908136490793, 0.2952755905511810774, -0.1292274648535930714 ) ) ;
#23468 = CARTESIAN_POINT ( 'NONE',  ( -0.5249343832020990641, 0.2306618581243848609, 0.2411417322834645549 ) ) ;
#23469 = CARTESIAN_POINT ( 'NONE',  ( -1.154855643044618851, 0.2306618581243848609, 0.2411417322834645549 ) ) ;
#23470 = CARTESIAN_POINT ( 'NONE',  ( -0.4593175853018366950, 0.05413385826771666132, 0.4176697321401328100 ) ) ;
#23471 = CARTESIAN_POINT ( 'NONE',  ( 0.5577427821522314977, -0.3162353388693409650, -0.4822834645669289433 ) ) ;
#23472 = CARTESIAN_POINT ( 'NONE',  ( 0.6102362204724416372, -0.5400638737290844871, 0.3530559997133364547 ) ) ;
#23473 = CARTESIAN_POINT ( 'NONE',  ( -0.3917322834645669549, -0.1049643490035306603, -0.9829396325459317518 ) ) ;
#23474 = CARTESIAN_POINT ( 'NONE',  ( -0.2230971128608915943, -0.004921259842519576551, 0.3153832671262227771 ) ) ;
#23475 = ORIENTED_EDGE ( 'NONE', *, *, #61940, .T. ) ;
#23476 = CARTESIAN_POINT ( 'NONE',  ( -0.3420746716998659953, -0.1974969037888706647, -1.627296587926509330 ) ) ;
#23477 = ORIENTED_EDGE ( 'NONE', *, *, #1370, .T. ) ;
#23478 = CARTESIAN_POINT ( 'NONE',  ( -1.404199475065615932, -0.004921259842519576551, 0.3153832671262227771 ) ) ;
#23479 = CARTESIAN_POINT ( 'NONE',  ( -0.4855643044619415427, 0.05413385826771626580, -0.4176697321401330321 ) ) ;
#23480 = CARTESIAN_POINT ( 'NONE',  ( 0.1070741851644054915, -0.3996062992125986035, 0.07217847769028869209 ) ) ;
#23481 = CARTESIAN_POINT ( 'NONE',  ( -0.5708661417322828946, 0.1660481256975883668, -0.3530559997133364547 ) ) ;
#23482 = CARTESIAN_POINT ( 'NONE',  ( -0.9120734908136475250, 0.2952755905511811885, 0.1292274648535926551 ) ) ;
#23483 = CARTESIAN_POINT ( 'NONE',  ( -1.305774278215222184, 0.2952755905511811885, 0.1292274648535926551 ) ) ;
#23484 = EDGE_CURVE ( 'NONE', #40183, #5969, #11816, .T. ) ;
#23485 = CARTESIAN_POINT ( 'NONE',  ( -0.4478269029167694093, 1.694792223680989363, -3.911458217027259376 ) ) ;
#23486 = AXIS2_PLACEMENT_3D ( 'NONE', #67925, #8599, #9018 ) ;
#23487 = CARTESIAN_POINT ( 'NONE',  ( 0.7939632545931766261, -0.2845877964562161244, -0.3641732283464567121 ) ) ;
#23488 = CARTESIAN_POINT ( 'NONE',  ( 0.4359958488159610956, 1.724409448818897461, 1.033875059083681158 ) ) ;
#23489 = CARTESIAN_POINT ( 'NONE',  ( -0.3917322834645669549, -0.1049643490035306603, -0.1305774278215224293 ) ) ;
#23490 = CARTESIAN_POINT ( 'NONE',  ( 0.1246719160104994284, -0.5511811023622046335, 0.09757992244046803654 ) ) ;
#23491 = CARTESIAN_POINT ( 'NONE',  ( -0.4265091863517051496, -0.6692913385826771977, 0.1292274648535927661 ) ) ;
#23492 = CARTESIAN_POINT ( 'NONE',  ( 0.006561679790026889343, -0.3162353388693409650, -0.4822834645669289433 ) ) ;
#23493 = VERTEX_POINT ( 'NONE', #13573 ) ;
#23494 = CARTESIAN_POINT ( 'NONE',  ( -0.2925321140481930704, -0.2925321140481933480, -1.948818897637795144 ) ) ;
#23495 = CARTESIAN_POINT ( 'NONE',  ( -0.5708661417322828946, 0.1012011053420775880, -0.2882089793578257453 ) ) ;
#23496 = ORIENTED_EDGE ( 'NONE', *, *, #61689, .T. ) ;
#23497 = CARTESIAN_POINT ( 'NONE',  ( -0.2925321140481930149, -0.2925321140481933480, -1.553149606299212726 ) ) ;
#23498 = CARTESIAN_POINT ( 'NONE',  ( -0.1323808228461572090, 0.2647380121165202049, 0.1574803149606299746 ) ) ;
#23499 = CARTESIAN_POINT ( 'NONE',  ( -0.8858267716535425107, 0.07958543189024071263, -0.2665933059059888421 ) ) ;
#23500 = CARTESIAN_POINT ( 'NONE',  ( -1.161417322834644716, -0.5400638737290845981, -0.3530559997133363437 ) ) ;
#23501 = CARTESIAN_POINT ( 'NONE',  ( 0.4091458600556404646, -0.2362204724409448231, -0.5774278215223097588 ) ) ;
#23502 = DIRECTION ( 'NONE',  ( -3.491481338843132961E-15, 0.000000000000000000, 1.000000000000000000 ) ) ;
#23503 = CARTESIAN_POINT ( 'NONE',  ( -9.594673741351313045E-17, 0.3917322834645670104, -2.446850393700787496 ) ) ;
#23504 = CARTESIAN_POINT ( 'NONE',  ( 1.299212598425197429, -0.6692913385826771977, 8.415575281601705876E-17 ) ) ;
#23505 = CARTESIAN_POINT ( 'NONE',  ( 0.5380577427821529035, 0.05413385826771626580, -0.4176697321401330321 ) ) ;
#23506 = CARTESIAN_POINT ( 'NONE',  ( 0.6430446194225729606, -0.4281496062992127816, -0.4176697321401328100 ) ) ;
#23507 = CARTESIAN_POINT ( 'NONE',  ( -0.8530183727034112984, -0.004921259842519576551, 0.3153832671262227771 ) ) ;
#23508 = CARTESIAN_POINT ( 'NONE',  ( -0.4986876640419942164, -0.6046776061558807314, 0.2411417322834647770 ) ) ;
#23509 = CARTESIAN_POINT ( 'NONE',  ( -0.1265901696524986964, -0.4724409448818899238, -2.511154855643044748 ) ) ;
#23510 = CARTESIAN_POINT ( 'NONE',  ( -0.2690288713910754526, 0.2952755905511810774, -0.1292274648535930714 ) ) ;
#23511 = CARTESIAN_POINT ( 'NONE',  ( -0.1974969037888706924, 0.3420746716998658843, -1.664698162729658870 ) ) ;
#23512 = CARTESIAN_POINT ( 'NONE',  ( 1.161417322834646271, 0.07958543189024071263, -0.2665933059059888421 ) ) ;
#23513 = CARTESIAN_POINT ( 'NONE',  ( -0.2296587926509179312, -0.2845877964562161244, -0.3641732283464567121 ) ) ;
#23514 = CARTESIAN_POINT ( 'NONE',  ( 1.194225721784777594, -0.004921259842519576551, 0.3153832671262227771 ) ) ;
#23515 = CARTESIAN_POINT ( 'NONE',  ( -1.115485564304461219, -0.4281496062992124485, 0.4176697321401328655 ) ) ;
#23516 = CARTESIAN_POINT ( 'NONE',  ( -1.089238845144356427, -0.3690944881889765550, -0.3153832671262227771 ) ) ;
#23517 = DIRECTION ( 'NONE',  ( -0.000000000000000000, -0.000000000000000000, -1.000000000000000000 ) ) ;
#23518 = CARTESIAN_POINT ( 'NONE',  ( -1.292650918635170010, -0.6692913385826771977, 0.1292274648535927661 ) ) ;
#23519 = CARTESIAN_POINT ( 'NONE',  ( -0.2362204724409440182, -0.1870078740157479769, 0.4822834645669291653 ) ) ;
#23520 = CARTESIAN_POINT ( 'NONE',  ( 0.4265091863517067594, 0.2952755905511811885, 0.1292274648535926551 ) ) ;
#23521 = CARTESIAN_POINT ( 'NONE',  ( -1.923433685342933241, 1.142877263639054286, 0.2639061591570278087 ) ) ;
#23522 = CARTESIAN_POINT ( 'NONE',  ( 0.4002624671916016896, -0.08942795157527998196, 0.3641732283464567121 ) ) ;
#23523 = CARTESIAN_POINT ( 'NONE',  ( -1.660104986876639543, -0.08942795157528024563, -0.3641732283464568787 ) ) ;
#23524 = CARTESIAN_POINT ( 'NONE',  ( 0.9186351706036752773, 0.2306618581243847221, -0.2411417322834647770 ) ) ;
#23525 = CARTESIAN_POINT ( 'NONE',  ( -1.548556430446193399, 0.1283753931104748280, 0.1820866141732283561 ) ) ;
#23526 = CARTESIAN_POINT ( 'NONE',  ( 1.515748031496063186, -0.4536011799217368745, -0.2665933059059886201 ) ) ;
#23527 = CARTESIAN_POINT ( 'NONE',  ( -1.076115485564303809, 0.2306618581243848609, 0.2411417322834645549 ) ) ;
#23528 = CARTESIAN_POINT ( 'NONE',  ( -0.4265091863517051496, -0.5511811023622046335, 0.09757992244046803654 ) ) ;
#23529 = DIRECTION ( 'NONE',  ( 0.000000000000000000, 0.000000000000000000, -1.000000000000000000 ) ) ;
#23530 = CARTESIAN_POINT ( 'NONE',  ( 0.2296587926509192634, -0.08942795157528024563, -0.3641732283464568787 ) ) ;
#23531 = CARTESIAN_POINT ( 'NONE',  ( 0.3996062992125986035, 2.446882876249141962E-17, -0.7480314960629921295 ) ) ;
#23532 = CARTESIAN_POINT ( 'NONE',  ( -0.2624671916010490880, -0.6046776061558807314, 0.2411417322834647770 ) ) ;
#23533 = CARTESIAN_POINT ( 'NONE',  ( -0.1998031496062991630, -0.3460692066303959202, -0.7723097112860892732 ) ) ;
#23534 = CARTESIAN_POINT ( 'NONE',  ( 0.3392501089628018329, 0.1958661417322835607, -1.948162729658792891 ) ) ;
#23535 = CARTESIAN_POINT ( 'NONE',  ( 0.6167979002624678353, -0.3690944881889763329, 0.3153832671262228327 ) ) ;
#23536 = CARTESIAN_POINT ( 'NONE',  ( 0.1115485564304470323, 0.2952755905511811885, 0.1292274648535926551 ) ) ;
#23537 = CARTESIAN_POINT ( 'NONE',  ( -0.7086614173228339419, -0.1870078740157479769, 0.4822834645669291653 ) ) ;
#23538 = CARTESIAN_POINT ( 'NONE',  ( -0.7874015748031489847, -0.1870078740157480601, -0.3641732283464567677 ) ) ;
#23539 = DIRECTION ( 'NONE',  ( 3.096699300667737957E-16, -1.000000000000000000, 0.000000000000000000 ) ) ;
#23540 = CARTESIAN_POINT ( 'NONE',  ( -0.5118110236220466680, 0.1771653543307087630, 0.000000000000000000 ) ) ;
#23541 = CARTESIAN_POINT ( 'NONE',  ( 0.04593175853018440641, -0.6692913385826771977, 0.1292274648535927661 ) ) ;
#23542 = CARTESIAN_POINT ( 'NONE',  ( -1.082677165354329896, 0.07958543189024085140, 0.2665933059059887866 ) ) ;
#23544 = CARTESIAN_POINT ( 'NONE',  ( 0.1998031496062992463, 0.3460692066303959202, -1.323490813648294129 ) ) ;
#23543 = VECTOR ( 'NONE', #67593, 39.37007874015748143 ) ;
#23545 = CARTESIAN_POINT ( 'NONE',  ( -1.423884514435694859, -0.05778040916215560624, -0.4822834645669293319 ) ) ;
#23546 = CARTESIAN_POINT ( 'NONE',  ( 0.4617417521217854204, 1.990046790791744833E-15, -0.4118477457932984698 ) ) ;
#23547 = ORIENTED_EDGE ( 'NONE', *, *, #20291, .T. ) ;
#23548 = CARTESIAN_POINT ( 'NONE',  ( -1.430446194225721390, -0.3690944881889763329, 0.3153832671262228327 ) ) ;
#23549 = CARTESIAN_POINT ( 'NONE',  ( -0.2952755905511804668, 0.1660481256975885056, 0.3530559997133364547 ) ) ;
#23550 = CARTESIAN_POINT ( 'NONE',  ( -1.003937007874014853, 0.1660481256975885056, 0.3530559997133364547 ) ) ;
#23551 = CARTESIAN_POINT ( 'NONE',  ( -0.3917322834645669549, -0.1049643490035306603, -1.705380577427821898 ) ) ;
#23552 = CARTESIAN_POINT ( 'NONE',  ( -0.5314960629921122726, 2.559055118110236560, -3.937007874015763687 ) ) ;
#23553 = CARTESIAN_POINT ( 'NONE',  ( 1.227034120734908917, 0.2952755905511810774, -0.1292274648535930714 ) ) ;
#23554 = CARTESIAN_POINT ( 'NONE',  ( 0.3280839895013130669, -0.4281496062992127816, -0.4176697321401328100 ) ) ;
#23555 = CARTESIAN_POINT ( 'NONE',  ( 1.141392835773559211, 0.3937007874015748254, 1.141392835773562764 ) ) ;
#23556 = CARTESIAN_POINT ( 'NONE',  ( -0.1070741851644051862, -0.3996062992125986035, -2.353674540682414662 ) ) ;
#23557 = CARTESIAN_POINT ( 'NONE',  ( -1.633858267716534529, -0.5400638737290845981, -0.3530559997133363437 ) ) ;
#23558 = CARTESIAN_POINT ( 'NONE',  ( -0.3996062992125986035, -0.1070741851644056997, -0.8333333333333332593 ) ) ;
#23559 = ORIENTED_EDGE ( 'NONE', *, *, #9067, .T. ) ;
#23560 = CARTESIAN_POINT ( 'NONE',  ( -0.7217847769028863381, -0.3690944881889763329, 0.3153832671262228327 ) ) ;
#23561 = CARTESIAN_POINT ( 'NONE',  ( 0.3392501089628018884, -0.1958661417322834220, -2.459317585301837195 ) ) ;
#23562 = VERTEX_POINT ( 'NONE', #70379 ) ;
#23563 = CARTESIAN_POINT ( 'NONE',  ( 0.5183727034120741983, 0.2952755905511810774, -0.1292274648535930714 ) ) ;
#23564 = CARTESIAN_POINT ( 'NONE',  ( -0.2362204724409442680, -0.1870078740157480879, -0.4822834645669291653 ) ) ;
#23565 = CARTESIAN_POINT ( 'NONE',  ( -1.135170603674539924, 0.2952755905511810774, -0.1292274648535930714 ) ) ;
#23566 = CARTESIAN_POINT ( 'NONE',  ( 0.9055118110236227702, 0.2952755905511811885, 0.000000000000000000 ) ) ;
#23567 = CARTESIAN_POINT ( 'NONE',  ( -1.279527559055116948, 0.07958543189024071263, -0.2665933059059888421 ) ) ;
#23568 = DIRECTION ( 'NONE',  ( 0.000000000000000000, 0.000000000000000000, 1.000000000000000000 ) ) ;
#23569 = CARTESIAN_POINT ( 'NONE',  ( 0.03280839895013198948, -0.6692913385826773087, -0.1292274648535924053 ) ) ;
#23570 = CARTESIAN_POINT ( 'NONE',  ( -1.259842519685038686, -0.1870078740157480879, -0.4822834645669291653 ) ) ;
#23571 = CARTESIAN_POINT ( 'NONE',  ( 0.3917322834645668994, 0.1049643490035304522, -1.936988558233908808 ) ) ;
#23572 = FACE_OUTER_BOUND ( 'NONE', #45227, .T. ) ;
#23573 = DIRECTION ( 'NONE',  ( 0.000000000000000000, 1.000000000000000000, 0.000000000000000000 ) ) ;
#23574 = CARTESIAN_POINT ( 'NONE',  ( -0.1958661417322834220, -0.3392501089628018884, 0.09973753280839900426 ) ) ;
#23575 = CARTESIAN_POINT ( 'NONE',  ( 0.9251968503937015864, 0.07958543189024071263, -0.2665933059059888421 ) ) ;
#23576 = ORIENTED_EDGE ( 'NONE', *, *, #28526, .T. ) ;
#23577 = CARTESIAN_POINT ( 'NONE',  ( 0.3949938075777409963, 2.418639510665530435E-17, -0.1181102362204724948 ) ) ;
#23578 = CARTESIAN_POINT ( 'NONE',  ( -0.9186351706036736120, -0.6046776061558809534, -0.2411417322834644161 ) ) ;
#23579 = EDGE_LOOP ( 'NONE', ( #45066, #18204, #73608, #5767 ) ) ;
#23580 = CARTESIAN_POINT ( 'NONE',  ( 0.5971128608923890191, -0.5511811023622046335, 0.09757992244046803654 ) ) ;
#23581 = CARTESIAN_POINT ( 'NONE',  ( -1.732283464566928277, -0.1870078740157479769, 0.4822834645669291653 ) ) ;
#23582 = CARTESIAN_POINT ( 'NONE',  ( 0.4790026246719167324, -0.05778040916215522460, 0.4822834645669289988 ) ) ;
#23583 = CARTESIAN_POINT ( 'NONE',  ( 0.3608923884514443348, 0.2952755905511810774, -0.1292274648535930714 ) ) ;
#23584 = EDGE_CURVE ( 'NONE', #36616, #65086, #30177, .T. ) ;
#23585 = CARTESIAN_POINT ( 'NONE',  ( -0.2427821522309703550, -0.05778040916215560624, -0.4822834645669293319 ) ) ;
#23586 = CARTESIAN_POINT ( 'NONE',  ( -0.3917322834645671770, 0.1049643490035302024, -1.289389394521996968 ) ) ;
#23587 = CARTESIAN_POINT ( 'NONE',  ( -0.5839895013123351797, -0.6692913385826771977, 0.1292274648535927661 ) ) ;
#23588 = CARTESIAN_POINT ( 'NONE',  ( -9.594673741351313045E-17, 0.3917322834645670104, -2.289370078740157410 ) ) ;
#23589 = CARTESIAN_POINT ( 'NONE',  ( 1.128608923884514947, 0.1283753931104748280, 0.1820866141732283561 ) ) ;
#23590 = CARTESIAN_POINT ( 'NONE',  ( -1.082677165354329896, -0.5400638737290845981, -0.3530559997133363437 ) ) ;
#23591 = CARTESIAN_POINT ( 'NONE',  ( 1.430446194225722500, -0.4281496062992127816, -0.4176697321401328100 ) ) ;
#23592 = CARTESIAN_POINT ( 'NONE',  ( 1.253280839895013710, -0.05778040916215560624, -0.4822834645669293319 ) ) ;
#23593 = CARTESIAN_POINT ( 'NONE',  ( 0.3460692066303959757, -0.1998031496062991907, -0.4199475065616797842 ) ) ;
#23594 = CARTESIAN_POINT ( 'NONE',  ( -0.9580052493438311334, -0.4281496062992124485, 0.4176697321401328655 ) ) ;
#23595 = CARTESIAN_POINT ( 'NONE',  ( -0.3460692066303957537, -0.1998031496062994405, -0.2867454068241469534 ) ) ;
#23596 = CARTESIAN_POINT ( 'NONE',  ( 0.3871391076115492380, -0.05778040916215560624, -0.4822834645669293319 ) ) ;
#23597 = CARTESIAN_POINT ( 'NONE',  ( 0.1070741851644053527, 0.3996062992125986590, -2.355643044619422533 ) ) ;
#23598 =( BOUNDED_CURVE ( )  B_SPLINE_CURVE ( 2, ( #44391, #19570, #43992, #64197, #45229, #32615, #63362, #44803, #5297, #51126, #82324, #31367, #6531 ),
 .UNSPECIFIED., .F., .F. ) 
 B_SPLINE_CURVE_WITH_KNOTS ( ( 3, 2, 2, 2, 2, 2, 3 ),
 ( 0.9125000000000000888, 0.9166666666666667407, 0.9208333333333333925, 0.9250000000000000444, 0.9291666666666666963, 0.9333333333333333481, 0.9375000000000000000 ),
 .UNSPECIFIED. ) 
 CURVE ( )  GEOMETRIC_REPRESENTATION_ITEM ( )  RATIONAL_B_SPLINE_CURVE ( ( 0.9999999999999991118, 0.9659258262890692004, 1.000000000000000000, 0.9659258262890683122, 1.000000000000000000, 0.9659258262890683122, 1.000000000000000000, 0.9659258262890683122, 1.000000000000000000, 0.9659258262890683122, 1.000000000000000000, 0.9659258262890683122, 1.000000000000000000 ) ) 
 REPRESENTATION_ITEM ( '' )  );
#23599 = CARTESIAN_POINT ( 'NONE',  ( -0.6955380577427815458, 0.05413385826771666132, 0.4176697321401328100 ) ) ;
#23600 = AXIS2_PLACEMENT_3D ( 'NONE', #35447, #61941, #35035 ) ;
#23601 = CARTESIAN_POINT ( 'NONE',  ( 1.568241469816273659, -0.05778040916215560624, -0.4822834645669293319 ) ) ;
#23602 = CARTESIAN_POINT ( 'NONE',  ( 0.4921259842519691285, -0.4536011799217368745, -0.2665933059059886201 ) ) ;
#23603 = CARTESIAN_POINT ( 'NONE',  ( 1.141732283464567566, 0.2952755905511811885, 0.000000000000000000 ) ) ;
#23604 = CARTESIAN_POINT ( 'NONE',  ( -0.3458507752293909498, 0.3458507752293907833, -0.8838582677165351953 ) ) ;
#23605 = CARTESIAN_POINT ( 'NONE',  ( 0.8398950131233602345, -0.5023911411419708095, 0.1820866141732285504 ) ) ;
#23606 = CARTESIAN_POINT ( 'NONE',  ( 0.8398950131233602345, 0.2306618581243847221, -0.2411417322834647770 ) ) ;
#23607 = CARTESIAN_POINT ( 'NONE',  ( -0.3949938075777409963, -7.255918531996591613E-17, -0.7460629921259843700 ) ) ;
#23608 = CARTESIAN_POINT ( 'NONE',  ( -0.6496062992125976043, -0.5400638737290844871, 0.3530559997133364547 ) ) ;
#23609 = DIRECTION ( 'NONE',  ( 0.000000000000000000, -1.000000000000000000, -0.000000000000000000 ) ) ;
#23610 = CARTESIAN_POINT ( 'NONE',  ( 0.8333333333333340365, 0.1771653543307087075, -0.09757992244046823083 ) ) ;
#23611 = CARTESIAN_POINT ( 'NONE',  ( -0.5446194225721777693, -0.3162353388693409650, -0.4822834645669289433 ) ) ;
#23612 = CARTESIAN_POINT ( 'NONE',  ( -0.02624671916010428221, -0.6046776061558807314, 0.2411417322834647770 ) ) ;
#23613 = DIRECTION ( 'NONE',  ( 0.000000000000000000, 0.000000000000000000, 1.000000000000000000 ) ) ;
#23614 = CARTESIAN_POINT ( 'NONE',  ( 0.2034120734908142214, 0.2952755905511810774, -0.1292274648535930714 ) ) ;
#23615 = CARTESIAN_POINT ( 'NONE',  ( 0.2559055118110243332, 0.07958543189024085140, 0.2665933059059887866 ) ) ;
#23616 = CARTESIAN_POINT ( 'NONE',  ( -2.829418903715950062, 1.111478976311902400, -0.2095522481616286514 ) ) ;
#23617 = CARTESIAN_POINT ( 'NONE',  ( -0.07874015748031421014, -0.1870078740157479769, 0.3641732283464567677 ) ) ;
#23618 = CARTESIAN_POINT ( 'NONE',  ( 0.6430446194225728496, -0.004921259842519576551, 0.3153832671262227771 ) ) ;
#23619 = CARTESIAN_POINT ( 'NONE',  ( 1.586052503253845281, 1.299212598425198095, 0.1653254495020587411 ) ) ;
#23620 = CARTESIAN_POINT ( 'NONE',  ( 0.3996062992125986035, -0.1070741851644052972, -1.605643044619422977 ) ) ;
#23621 = CARTESIAN_POINT ( 'NONE',  ( 0.2755905511811031494, 0.2952755905511811885, 0.000000000000000000 ) ) ;
#23622 = CARTESIAN_POINT ( 'NONE',  ( 0.3392501089628018884, -0.1958661417322834220, -1.671916010498687655 ) ) ;
#23623 = CARTESIAN_POINT ( 'NONE',  ( 0.2242874410717144995, -4.069555009745408348E-17, -0.3627989612356146698 ) ) ;
#23624 = CARTESIAN_POINT ( 'NONE',  ( -0.3588842212258053777, -0.1584414948821128155, 7.390873527593507220E-17 ) ) ;
#23625 = CARTESIAN_POINT ( 'NONE',  ( -0.3805774278215216522, -0.3690944881889765550, -0.3153832671262227771 ) ) ;
#23626 = CARTESIAN_POINT ( 'NONE',  ( -0.4658792650918627265, -0.3162353388693409650, -0.4822834645669289433 ) ) ;
#23627 = CARTESIAN_POINT ( 'NONE',  ( 0.9120734908136490793, 0.1771653543307087075, -0.09757992244046823083 ) ) ;
#23628 = CARTESIAN_POINT ( 'NONE',  ( -1.699475065616797398, 0.1771653543307087630, 0.09757992244046791164 ) ) ;
#23629 = CARTESIAN_POINT ( 'NONE',  ( -1.233595800524933894, 0.2306618581243848609, 0.2411417322834645549 ) ) ;
#23630 = CARTESIAN_POINT ( 'NONE',  ( -0.01312335958005186876, 0.05413385826771626580, -0.4176697321401330321 ) ) ;
#23631 = CARTESIAN_POINT ( 'NONE',  ( 1.194225721784777594, 0.05413385826771666132, 0.4176697321401328100 ) ) ;
#23632 = CARTESIAN_POINT ( 'NONE',  ( 0.3346456692913390985, 0.1660481256975885056, 0.3530559997133364547 ) ) ;
#23634 = CARTESIAN_POINT ( 'NONE',  ( 1.325459317585302665, -0.4281496062992124485, 0.4176697321401328655 ) ) ;
#23633 = VECTOR ( 'NONE', #25580, 39.37007874015748143 ) ;
#23635 = AXIS2_PLACEMENT_3D ( 'NONE', #53736, #77775, #52488 ) ;
#23636 = CARTESIAN_POINT ( 'NONE',  ( 0.4527559055118117182, 0.1660481256975883668, -0.3530559997133364547 ) ) ;
#23637 = CARTESIAN_POINT ( 'NONE',  ( -1.725721784776902190, -0.08942795157527998196, 0.3641732283464567121 ) ) ;
#23638 = CARTESIAN_POINT ( 'NONE',  ( 0.9186351706036752773, 0.1283753931104746893, -0.1820866141732285504 ) ) ;
#23639 = CARTESIAN_POINT ( 'NONE',  ( 1.568241469816273659, -0.05778040916215560624, -0.4822834645669293319 ) ) ;
#23640 = CARTESIAN_POINT ( 'NONE',  ( 0.2165354330708668673, 0.07958543189024071263, -0.2665933059059888421 ) ) ;
#23641 = CARTESIAN_POINT ( 'NONE',  ( -0.2624671916010490880, -0.6046776061558807314, 0.2411417322834647770 ) ) ;
#23642 = CARTESIAN_POINT ( 'NONE',  ( 0.6692913385826777528, 0.2952755905511811885, 0.000000000000000000 ) ) ;
#23643 = CARTESIAN_POINT ( 'NONE',  ( -0.4593175853018364174, -0.4281496062992127816, -0.4176697321401328100 ) ) ;
#23644 = CARTESIAN_POINT ( 'NONE',  ( 0.1049643490035304799, -0.3917322834645670104, -1.971804092684726228 ) ) ;
#23645 = CARTESIAN_POINT ( 'NONE',  ( -0.2887139107611542133, 0.1283753931104748280, 0.1820866141732283561 ) ) ;
#23646 = CARTESIAN_POINT ( 'NONE',  ( 0.7349081364829402885, -0.6046776061558809534, -0.2411417322834644161 ) ) ;
#23647 = CARTESIAN_POINT ( 'NONE',  ( 1.161417322834646493, -0.4536011799217367080, 0.2665933059059888421 ) ) ;
#23648 = CARTESIAN_POINT ( 'NONE',  ( 0.2165354330708668673, -0.5400638737290844871, 0.3530559997133364547 ) ) ;
#23649 = DIRECTION ( 'NONE',  ( 0.000000000000000000, -1.000000000000000000, -0.000000000000000000 ) ) ;
#23651 = CARTESIAN_POINT ( 'NONE',  ( 0.000000000000000000, 0.7086614173228346081, 0.2362204724409449064 ) ) ;
#23650 = CARTESIAN_POINT ( 'NONE',  ( 0.000000000000000000, 2.755905511811024056, 0.000000000000000000 ) ) ;
#23652 = CARTESIAN_POINT ( 'NONE',  ( 0.1958661417322834775, 0.3392501089628018884, -2.183727034120734878 ) ) ;
#23653 = B_SPLINE_CURVE_WITH_KNOTS ( 'NONE', 3,
 ( #68455, #37285, #36454, #55387 ),
 .UNSPECIFIED., .F., .F.,
 ( 4, 4 ),
 ( 1.999999999910059834E-07, 0.006970199999999935996 ),
 .UNSPECIFIED. ) ;
#23654 = CARTESIAN_POINT ( 'NONE',  ( -1.102362204724408601, -0.1870078740157480879, -0.4822834645669291653 ) ) ;
#23655 = CARTESIAN_POINT ( 'NONE',  ( -0.5643044619422565855, 0.05413385826771626580, -0.4176697321401330321 ) ) ;
#23656 = CARTESIAN_POINT ( 'NONE',  ( 0.4724409448818897572, -0.1265901696524988906, -0.1115485564304461719 ) ) ;
#23657 = CARTESIAN_POINT ( 'NONE',  ( -0.1974969037888703871, -0.3420746716998661063, -2.585301837270341352 ) ) ;
#23658 = VERTEX_POINT ( 'NONE', #82206 ) ;
#23659 = CARTESIAN_POINT ( 'NONE',  ( 0.3543307086614181922, -0.5511811023622047445, 6.969142054262312111E-17 ) ) ;
#23660 = CARTESIAN_POINT ( 'NONE',  ( -0.3392501089628019995, 0.1958661417322832277, -1.278215223097112885 ) ) ;
#23661 = CARTESIAN_POINT ( 'NONE',  ( 0.5905511811023629321, -0.6692913385826771977, 8.415575281601705876E-17 ) ) ;
#23662 = CARTESIAN_POINT ( 'NONE',  ( -0.2362204724409447953, -0.4091458600556404646, -2.427821522309711266 ) ) ;
#23663 = DIRECTION ( 'NONE',  ( -8.673617379884021667E-16, 1.000000000000000000, -3.028377322213054317E-30 ) ) ;
#23664 = CARTESIAN_POINT ( 'NONE',  ( -0.3018372703412066094, 0.05413385826771666132, 0.4176697321401328100 ) ) ;
#23665 = CARTESIAN_POINT ( 'NONE',  ( 1.286089238845145033, 0.1283753931104748280, 0.1820866141732283561 ) ) ;
#23666 = CARTESIAN_POINT ( 'NONE',  ( 0.4068241469816281097, 0.05413385826771666132, 0.4176697321401328100 ) ) ;
#23667 = CARTESIAN_POINT ( 'NONE',  ( -9.594673741351310580E-17, 0.3917322834645669549, -0.8674347524596309755 ) ) ;
#23668 = CARTESIAN_POINT ( 'NONE',  ( -0.4330708661417315697, -0.6692913385826771977, 8.415575281601705876E-17 ) ) ;
#23669 = CARTESIAN_POINT ( 'NONE',  ( -1.010498687664041384, -0.3690944881889765550, -0.3153832671262227771 ) ) ;
#23671 = EDGE_CURVE ( 'NONE', #13764, #66254, #64489, .T. ) ;
#23670 = CARTESIAN_POINT ( 'NONE',  ( 0.4002624671916016896, -0.3162353388693409650, -0.4822834645669289433 ) ) ;
#23672 = CARTESIAN_POINT ( 'NONE',  ( -0.06561679790026180015, -0.4281496062992127816, -0.4176697321401328100 ) ) ;
#23673 = CARTESIAN_POINT ( 'NONE',  ( -1.192200019340701855, -5.582469467804009507E-15, -0.3954985857520081360 ) ) ;
#23674 = CARTESIAN_POINT ( 'NONE',  ( 0.4606732211678724598, 1.763126522798933227, -0.5309055118110237448 ) ) ;
#23675 = CARTESIAN_POINT ( 'NONE',  ( -0.2867679344610367109, 0.2867679344610365444, -2.221147924705723753 ) ) ;
#23676 = CARTESIAN_POINT ( 'NONE',  ( 0.6627296587926517768, -0.6692913385826773087, -0.1292274648535924053 ) ) ;
#23677 = CARTESIAN_POINT ( 'NONE',  ( -0.4330708661417315697, 0.2952755905511811885, 0.000000000000000000 ) ) ;
#23678 = CARTESIAN_POINT ( 'NONE',  ( -1.325459317585300889, 0.05413385826771666132, 0.4176697321401328100 ) ) ;
#23679 = CARTESIAN_POINT ( 'NONE',  ( 0.9055118110236227702, -0.6692913385826771977, 8.415575281601705876E-17 ) ) ;
#23680 = CARTESIAN_POINT ( 'NONE',  ( 0.3740157480314966754, -0.5400638737290844871, 0.3530559997133364547 ) ) ;
#23681 = CARTESIAN_POINT ( 'NONE',  ( 0.3917322834645670104, 2.398668435337828261E-17, -0.9901574803149607584 ) ) ;
#23682 = CARTESIAN_POINT ( 'NONE',  ( -0.3018372703412066094, 0.05413385826771666132, 0.4176697321401328100 ) ) ;
#23683 = CARTESIAN_POINT ( 'NONE',  ( 0.3215223097112867578, -0.3162353388693409650, -0.4822834645669289433 ) ) ;
#23684 = CARTESIAN_POINT ( 'NONE',  ( -0.4265091863517051496, -0.6692913385826771977, 0.1292274648535927661 ) ) ;
#23685 = CARTESIAN_POINT ( 'NONE',  ( 0.2296587926509192634, -0.2845877964562159024, 0.3641732283464567677 ) ) ;
#23686 = CARTESIAN_POINT ( 'NONE',  ( 1.594488188976378673, -0.4536011799217368745, -0.2665933059059886201 ) ) ;
#23687 = DIRECTION ( 'NONE',  ( 0.000000000000000000, -1.000000000000000000, 0.000000000000000000 ) ) ;
#23688 = CARTESIAN_POINT ( 'NONE',  ( 0.2493438320209980519, -0.4281496062992127816, -0.4176697321401328100 ) ) ;
#23689 = CARTESIAN_POINT ( 'NONE',  ( -0.4724409448818898682, -8.678599364036362592E-17, -1.061023622047243986 ) ) ;
#23690 = CARTESIAN_POINT ( 'NONE',  ( 1.430446194225722500, 0.05413385826771666132, 0.4176697321401328100 ) ) ;
#23691 = CARTESIAN_POINT ( 'NONE',  ( 0.3917322834645669549, 0.1049643490035304660, -2.636482939632545985 ) ) ;
#23692 = VERTEX_POINT ( 'NONE', #6827 ) ;
#23693 = EDGE_LOOP ( 'NONE', ( #33096, #80822, #80661, #61045 ) ) ;
#23694 = AXIS2_PLACEMENT_3D ( 'NONE', #41016, #39765, #27550 ) ;
#23695 = CARTESIAN_POINT ( 'NONE',  ( 0.5183727034120741983, -0.6692913385826771977, 0.1292274648535927661 ) ) ;
#23696 = CARTESIAN_POINT ( 'NONE',  ( 0.2362204724409456558, -0.1870078740157480601, -0.3641732283464567677 ) ) ;
#23697 = AXIS2_PLACEMENT_3D ( 'NONE', #72263, #73088, #36027 ) ;
#23698 = AXIS2_PLACEMENT_3D ( 'NONE', #29617, #80988, #54034 ) ;
#23700 = CARTESIAN_POINT ( 'NONE',  ( -1.595398199321655941, 1.585328674332965315, 0.1559797534342484693 ) ) ;
#23699 = CARTESIAN_POINT ( 'NONE',  ( 0.5314960629921064994, 2.716535433070866645, 1.854472803289057836 ) ) ;
#23701 = CARTESIAN_POINT ( 'NONE',  ( 0.2867679344610365999, -0.2867679344610365444, -0.9704724409448820532 ) ) ;
#23702 = CARTESIAN_POINT ( 'NONE',  ( -0.1265901696524993347, 0.4724409448818895907, 0.2316272965879264956 ) ) ;
#23703 = FILL_AREA_STYLE ('',( #11506 ) ) ;
#23704 = CARTESIAN_POINT ( 'NONE',  ( 0.1070741851644054776, -0.3996062992125984925, -2.366797900262467280 ) ) ;
#23705 = CARTESIAN_POINT ( 'NONE',  ( 0.4986876640419954376, 0.2306618581243848609, 0.2411417322834645549 ) ) ;
#23706 = CARTESIAN_POINT ( 'NONE',  ( -0.9186351706036736120, -0.6046776061558809534, -0.2411417322834644161 ) ) ;
#23707 = CARTESIAN_POINT ( 'NONE',  ( -0.9055118110236215490, 0.2952755905511811885, 0.000000000000000000 ) ) ;
#23708 = CARTESIAN_POINT ( 'NONE',  ( 0.8858267716535438430, -0.5400638737290845981, -0.3530559997133363437 ) ) ;
#23709 = CARTESIAN_POINT ( 'NONE',  ( 1.371391076115485719, -0.6692913385826773087, -0.1292274648535924053 ) ) ;
#23710 = CARTESIAN_POINT ( 'NONE',  ( 1.194225721784777594, -0.004921259842519576551, 0.3153832671262227771 ) ) ;
#23711 = CONTEXT_DEPENDENT_SHAPE_REPRESENTATION ( #55681, #45256 ) ;
#23712 = CARTESIAN_POINT ( 'NONE',  ( 1.279527559055118724, -0.4536011799217368745, -0.2665933059059886201 ) ) ;
#23713 = CARTESIAN_POINT ( 'NONE',  ( -0.7086614173228339419, -0.1870078740157479769, 0.4822834645669291653 ) ) ;
#23714 = CARTESIAN_POINT ( 'NONE',  ( -0.1070741851644056997, 0.3996062992125984925, -0.3982939632545932085 ) ) ;
#23715 = CARTESIAN_POINT ( 'NONE',  ( 1.515748031496063408, 0.1660481256975885056, 0.3530559997133364547 ) ) ;
#23716 = CARTESIAN_POINT ( 'NONE',  ( 0.1049643490035303689, 0.3917322834645670104, -0.3005249343832020470 ) ) ;
#23717 = CARTESIAN_POINT ( 'NONE',  ( -0.4068241469816264999, -0.4281496062992124485, 0.4176697321401328655 ) ) ;
#23718 = AXIS2_PLACEMENT_3D ( 'NONE', #7356, #64601, #6936 ) ;
#23720 = FACE_OUTER_BOUND ( 'NONE', #58989, .T. ) ;
#23719 = CARTESIAN_POINT ( 'NONE',  ( 1.062992125984252745, 0.2952755905511811885, 0.000000000000000000 ) ) ;
#23721 = CARTESIAN_POINT ( 'NONE',  ( -1.194225721784776262, -0.004921259842519870586, -0.3153832671262229437 ) ) ;
#23722 = CARTESIAN_POINT ( 'NONE',  ( 0.4921259842519691285, -0.5400638737290845981, -0.3530559997133363437 ) ) ;
#23723 = CARTESIAN_POINT ( 'NONE',  ( 1.043307086614173818, -0.4536011799217368745, -0.2665933059059886201 ) ) ;
#23724 = CARTESIAN_POINT ( 'NONE',  ( 0.1049643490035304522, -0.3917322834645668994, -1.582657849572491449 ) ) ;
#23725 = CARTESIAN_POINT ( 'NONE',  ( -1.194225721784776262, -0.004921259842519870586, -0.3153832671262229437 ) ) ;
#23726 = CARTESIAN_POINT ( 'NONE',  ( 1.240157480314961314, 0.1660481256975883668, -0.3530559997133364547 ) ) ;
#23727 = DIRECTION ( 'NONE',  ( 0.000000000000000000, 0.000000000000000000, 1.000000000000000000 ) ) ;
#23728 = CARTESIAN_POINT ( 'NONE',  ( -0.2034120734908131112, -0.5511811023622048555, -0.09757992244046775898 ) ) ;
#23729 = CARTESIAN_POINT ( 'NONE',  ( -0.1706036745406816491, -0.4281496062992124485, 0.4176697321401328655 ) ) ;
#23730 = CARTESIAN_POINT ( 'NONE',  ( -1.299212598425196097, 0.1771653543307087630, 0.000000000000000000 ) ) ;
#23731 = CARTESIAN_POINT ( 'NONE',  ( -0.6364829396325453192, -0.3162353388693405765, 0.4822834645669290543 ) ) ;
#23732 = CARTESIAN_POINT ( 'NONE',  ( 1.286089238845145033, -0.6046776061558809534, -0.2411417322834644161 ) ) ;
#23733 = CARTESIAN_POINT ( 'NONE',  ( -0.1958661417322833942, -0.3392501089628018884, -0.5347962186689783071 ) ) ;
#23734 = CARTESIAN_POINT ( 'NONE',  ( -1.062992125984250968, -0.5511811023622047445, 6.969142054262312111E-17 ) ) ;
#23735 = CARTESIAN_POINT ( 'NONE',  ( 0.2017716535433070613, 0.2017716535433070613, 0.000000000000000000 ) ) ;
#23736 = CARTESIAN_POINT ( 'NONE',  ( 1.476377952755906220, 0.1660481256975883668, -0.3530559997133364547 ) ) ;
#23737 = CARTESIAN_POINT ( 'NONE',  ( -0.1265901696524986964, -0.4724409448818899238, -2.196194225721784576 ) ) ;
#23738 = CARTESIAN_POINT ( 'NONE',  ( -1.141732283464566011, -0.6692913385826771977, 8.415575281601705876E-17 ) ) ;
#23739 = CARTESIAN_POINT ( 'NONE',  ( -1.036745406824146176, -0.3690944881889763329, 0.3153832671262228327 ) ) ;
#23740 = CARTESIAN_POINT ( 'NONE',  ( -0.6758530183727028406, -0.5511811023622048555, -0.09757992244046775898 ) ) ;
#23741 = DIRECTION ( 'NONE',  ( 0.000000000000000000, 0.000000000000000000, 1.000000000000000000 ) ) ;
#23742 = CARTESIAN_POINT ( 'NONE',  ( 0.1443569553805781891, 0.05413385826771626580, -0.4176697321401330321 ) ) ;
#23743 = CARTESIAN_POINT ( 'NONE',  ( -0.2034120734908128059, 0.1771653543307087630, 0.09757992244046791164 ) ) ;
#23744 = CARTESIAN_POINT ( 'NONE',  ( -1.338582677165353729, -0.1870078740157480601, -0.3641732283464567677 ) ) ;
#23745 = CARTESIAN_POINT ( 'NONE',  ( -1.404199475065615932, 0.05413385826771666132, 0.4176697321401328100 ) ) ;
#23746 = CARTESIAN_POINT ( 'NONE',  ( 1.167979002624672580, -0.004921259842519870586, -0.3153832671262229437 ) ) ;
#23747 = CARTESIAN_POINT ( 'NONE',  ( 0.7545931758530189937, 0.2952755905511810774, -0.1292274648535930714 ) ) ;
#23748 = CARTESIAN_POINT ( 'NONE',  ( 0.04294987210466596345, 1.064862614867414070, 1.852127137687914704 ) ) ;
#23749 = CARTESIAN_POINT ( 'NONE',  ( 0.3149606299212606708, -0.1870078740157480601, -0.3641732283464567677 ) ) ;
#23750 = CARTESIAN_POINT ( 'NONE',  ( 0.7545931758530189937, 0.2952755905511810774, -0.1292274648535930714 ) ) ;
#23751 = CARTESIAN_POINT ( 'NONE',  ( 0.8333333333333340365, 0.1771653543307087075, -0.09757992244046823083 ) ) ;
#23752 = ORIENTED_EDGE ( 'NONE', *, *, #18308, .F. ) ;
#23753 = CARTESIAN_POINT ( 'NONE',  ( -1.266404199475064773, -0.05778040916215560624, -0.4822834645669293319 ) ) ;
#23754 = CARTESIAN_POINT ( 'NONE',  ( -0.8923884514435688198, -0.6046776061558807314, 0.2411417322834647770 ) ) ;
#23755 = CARTESIAN_POINT ( 'NONE',  ( -0.2493438320209966919, 0.05413385826771626580, -0.4176697321401330321 ) ) ;
#23756 = AXIS2_PLACEMENT_3D ( 'NONE', #40924, #78411, #47223 ) ;
#23757 = CARTESIAN_POINT ( 'NONE',  ( -2.170146923806554273, 1.546132656481028489, -0.4744094488188974612 ) ) ;
#23758 = CARTESIAN_POINT ( 'NONE',  ( 4.893765752498283308E-17, -0.3996062992125985480, -2.045275590551181466 ) ) ;
#23759 = CARTESIAN_POINT ( 'NONE',  ( 0.3937007874015754361, -0.1870078740157480879, -0.4822834645669291653 ) ) ;
#23760 = CARTESIAN_POINT ( 'NONE',  ( 1.364829396325459854, -0.5023911411419708095, -0.1820866141732282451 ) ) ;
#23761 = CIRCLE ( 'NONE', #78881, 1.889763779527559251 ) ;
#23762 = AXIS2_PLACEMENT_3D ( 'NONE', #49024, #73892, #67573 ) ;
#23763 = CARTESIAN_POINT ( 'NONE',  ( 0.04593175853018440641, -0.6692913385826771977, 0.1292274648535927661 ) ) ;
#23764 = CARTESIAN_POINT ( 'NONE',  ( 0.6692913385826777528, 0.2952755905511811885, 0.000000000000000000 ) ) ;
#23765 = CARTESIAN_POINT ( 'NONE',  ( -0.1998031496062991907, -0.3460692066303959757, -1.640419947506561726 ) ) ;
#23766 = CARTESIAN_POINT ( 'NONE',  ( -0.2891555358219908833, -0.2891555358219912164, -1.318897637795275912 ) ) ;
#23767 = CARTESIAN_POINT ( 'NONE',  ( 0.3460692066303959202, 0.1998031496062993295, -2.808398950131233640 ) ) ;
#23768 = DIRECTION ( 'NONE',  ( -0.000000000000000000, -1.000000000000000000, -0.000000000000000000 ) ) ;
#23769 = CARTESIAN_POINT ( 'NONE',  ( -0.3917322834645671215, 0.1049643490035301469, -0.6548556430446192955 ) ) ;
#23770 = CARTESIAN_POINT ( 'NONE',  ( -0.6102362204724400829, 0.07958543189024085140, 0.2665933059059887866 ) ) ;
#23771 = CARTESIAN_POINT ( 'NONE',  ( -0.8202099737532801971, -0.6692913385826771977, 0.1292274648535927661 ) ) ;
#23772 = CARTESIAN_POINT ( 'NONE',  ( 0.6496062992125991586, 0.1660481256975885056, 0.3530559997133364547 ) ) ;
#23773 = CARTESIAN_POINT ( 'NONE',  ( -0.1058382717557503072, 0.3949938075777408852, -1.973097112860892510 ) ) ;
#23774 = CARTESIAN_POINT ( 'NONE',  ( 0.8530183727034128527, -0.4281496062992124485, 0.4176697321401328655 ) ) ;
#23775 = CARTESIAN_POINT ( 'NONE',  ( -1.384514435695537005, -0.6692913385826773087, -0.1292274648535924053 ) ) ;
#23776 = CARTESIAN_POINT ( 'NONE',  ( 1.391076115485564868, -0.6046776061558807314, 0.2411417322834647770 ) ) ;
#23777 = CARTESIAN_POINT ( 'NONE',  ( 0.4724409448818896462, 0.1265901696524990294, -2.486876640419947382 ) ) ;
#23778 = CARTESIAN_POINT ( 'NONE',  ( -0.1998031496062994683, 0.3460692066303958092, -1.587926509186351698 ) ) ;
#23779 = CARTESIAN_POINT ( 'NONE',  ( 0.4847769261806178509, 1.968503937007873850, 0.4915354330708653907 ) ) ;
#23780 = CARTESIAN_POINT ( 'NONE',  ( 0.9251968503937015864, -0.5400638737290844871, 0.3530559997133364547 ) ) ;
#23781 = CARTESIAN_POINT ( 'NONE',  ( 0.4986876640419954376, 0.2306618581243848609, 0.2411417322834645549 ) ) ;
#23782 = CARTESIAN_POINT ( 'NONE',  ( 1.062992125984252745, -0.5511811023622047445, 6.969142054262312111E-17 ) ) ;
#23784 = CARTESIAN_POINT ( 'NONE',  ( 1.594488188976378673, 0.1660481256975885056, 0.3530559997133364547 ) ) ;
#23783 = CARTESIAN_POINT ( 'NONE',  ( -1.548556430446193399, -0.5023911411419708095, -0.1820866141732282451 ) ) ;
#23785 = CARTESIAN_POINT ( 'NONE',  ( 0.1958661417322834497, 0.3392501089628018329, -2.744075172407137497 ) ) ;
#23786 = CARTESIAN_POINT ( 'NONE',  ( 0.9317585301837276734, 0.05413385826771626580, -0.4176697321401330321 ) ) ;
#23787 = CARTESIAN_POINT ( 'NONE',  ( 1.627296587926509996, -0.5023911411419708095, 0.1820866141732285504 ) ) ;
#23788 = CARTESIAN_POINT ( 'NONE',  ( -0.6758530183727028406, -0.6692913385826773087, -0.1292274648535924053 ) ) ;
#23789 = CARTESIAN_POINT ( 'NONE',  ( -0.5446194225721777693, -0.3162353388693409650, -0.4822834645669289433 ) ) ;
#23790 = CARTESIAN_POINT ( 'NONE',  ( 1.456692913385827515, 0.2952755905511811885, 0.000000000000000000 ) ) ;
#23791 = CARTESIAN_POINT ( 'NONE',  ( -9.594673741351313045E-17, 0.3917322834645670104, -0.2421259842519686289 ) ) ;
#23792 = CARTESIAN_POINT ( 'NONE',  ( 0.3149606299212603933, -0.1870078740157479769, 0.4822834645669291653 ) ) ;
#23793 = CARTESIAN_POINT ( 'NONE',  ( 0.3917322834645669549, 0.1049643490035304660, -2.164041994750655729 ) ) ;
#23794 = CARTESIAN_POINT ( 'NONE',  ( -1.509186351706035767, -0.3690944881889763329, 0.3153832671262228327 ) ) ;
#23795 = ORIENTED_EDGE ( 'NONE', *, *, #2885, .T. ) ;
#23796 = CARTESIAN_POINT ( 'NONE',  ( -0.1058382717557497937, -0.3949938075777411628, -2.591863517060367883 ) ) ;
#23797 = ORIENTED_EDGE ( 'NONE', *, *, #81662, .T. ) ;
#23798 = CARTESIAN_POINT ( 'NONE',  ( -0.03280839895013062252, 0.2066929133858267098, -0.1054918080437494132 ) ) ;
#23799 = CARTESIAN_POINT ( 'NONE',  ( 1.220472440944882386, -0.5511811023622047445, 6.969142054262312111E-17 ) ) ;
#23800 = CARTESIAN_POINT ( 'NONE',  ( -0.3460692066303958092, -0.1998031496062994683, -0.9973753280839895430 ) ) ;
#23801 = CARTESIAN_POINT ( 'NONE',  ( 1.535433070866142558, 0.1771653543307087630, 0.000000000000000000 ) ) ;
#23802 = DIRECTION ( 'NONE',  ( 0.000000000000000000, 0.000000000000000000, 1.000000000000000000 ) ) ;
#23803 = DIRECTION ( 'NONE',  ( -0.000000000000000000, -1.000000000000000000, -0.000000000000000000 ) ) ;
#23804 = CARTESIAN_POINT ( 'NONE',  ( 0.000000000000000000, 2.165354330708661568, 0.000000000000000000 ) ) ;
#23805 = CARTESIAN_POINT ( 'NONE',  ( 0.3917322834645670104, -0.1049643490035303411, -0.3536745406824148286 ) ) ;
#23806 = CARTESIAN_POINT ( 'NONE',  ( -0.7086614173228339419, -0.1870078740157479769, 0.3641732283464567677 ) ) ;
#23807 = CARTESIAN_POINT ( 'NONE',  ( -1.404199475065615932, -0.004921259842519576551, 0.3153832671262227771 ) ) ;
#23808 = CARTESIAN_POINT ( 'NONE',  ( 1.437007874015748810, 0.1660481256975885056, 0.3530559997133364547 ) ) ;
#23809 = CARTESIAN_POINT ( 'NONE',  ( 0.5052493438320215802, 0.2952755905511811885, 0.1292274648535926551 ) ) ;
#23810 = CARTESIAN_POINT ( 'NONE',  ( -1.181102362204723644, -0.1870078740157479769, 0.4822834645669291653 ) ) ;
#23811 = CARTESIAN_POINT ( 'NONE',  ( -0.2867679344610365999, 0.2867679344610364889, -0.3267716535433070613 ) ) ;
#23812 = ORIENTED_EDGE ( 'NONE', *, *, #15671, .T. ) ;
#23813 = ADVANCED_FACE ( 'NONE', ( #5993 ), #72045, .F. ) ;
#23814 = CARTESIAN_POINT ( 'NONE',  ( -1.653543307086613234, -0.1870078740157479769, 0.4822834645669291653 ) ) ;
#23815 = CARTESIAN_POINT ( 'NONE',  ( -0.1938976377952756625, -0.1938976377952756625, 0.09542247959850377881 ) ) ;
#23816 =( CONVERSION_BASED_UNIT ( 'INCH', #36040 ) LENGTH_UNIT ( ) NAMED_UNIT ( #43771 ) );
#23817 = AXIS2_PLACEMENT_3D ( 'NONE', #6787, #13961, #71608 ) ;
#23818 = CARTESIAN_POINT ( 'NONE',  ( -0.3458507752293909498, 0.3458507752293907833, -1.751968503937007648 ) ) ;
#23819 = CARTESIAN_POINT ( 'NONE',  ( -0.2017716535433071445, -0.2017716535433071723, 0.000000000000000000 ) ) ;
#23820 = ADVANCED_FACE ( 'NONE', ( #57325 ), #11914, .T. ) ;
#23821 = VECTOR ( 'NONE', #64817, 39.37007874015748143 ) ;
#23822 = CARTESIAN_POINT ( 'NONE',  ( 0.4724409448818898682, 2.892866454678787531E-17, -0.9055118110236221041 ) ) ;
#23823 = CARTESIAN_POINT ( 'NONE',  ( -0.7283464566929126471, -0.5400638737290844871, 0.3530559997133364547 ) ) ;
#23824 = CARTESIAN_POINT ( 'NONE',  ( 0.8661417322834653598, -0.1870078740157479769, 0.4822834645669291653 ) ) ;
#23825 = CIRCLE ( 'NONE', #25118, 1.122047244094488194 ) ;
#23827 = DIRECTION ( 'NONE',  ( 0.000000000000000000, -0.4999999999999997224, -0.8660254037844388186 ) ) ;
#23826 = LINE ( 'NONE', #62543, #55662 ) ;
#23828 = CARTESIAN_POINT ( 'NONE',  ( 1.496062992125985147, -0.1870078740157479769, 0.4822834645669291653 ) ) ;
#23829 = CARTESIAN_POINT ( 'NONE',  ( -0.9317585301837263412, 0.05413385826771666132, 0.4176697321401328100 ) ) ;
#23830 = CARTESIAN_POINT ( 'NONE',  ( -9.594673741351310580E-17, 0.3917322834645669549, -0.2375134926171111049 ) ) ;
#23831 = CARTESIAN_POINT ( 'NONE',  ( -0.01312335958005186876, -0.3690944881889763329, 0.3153832671262228327 ) ) ;
#23832 = CARTESIAN_POINT ( 'NONE',  ( -0.3392501089628019995, 0.1958661417322832277, -0.2683727034120735877 ) ) ;
#23833 = CARTESIAN_POINT ( 'NONE',  ( -0.02624671916010428221, 0.1283753931104746893, -0.1820866141732285504 ) ) ;
#23834 = CARTESIAN_POINT ( 'NONE',  ( 0.6561679790026253567, 0.1283753931104748280, 0.1820866141732283561 ) ) ;
#23835 = CARTESIAN_POINT ( 'NONE',  ( 0.4265091863517067039, -0.6692913385826773087, -0.1292274648535924053 ) ) ;
#23836 = CARTESIAN_POINT ( 'NONE',  ( -0.5118110236220466680, 0.1771653543307087630, 0.000000000000000000 ) ) ;
#23837 = CARTESIAN_POINT ( 'NONE',  ( -0.3392501089628019995, 0.1958661417322832277, -2.223097112860892288 ) ) ;
#23838 = CARTESIAN_POINT ( 'NONE',  ( -1.522309711286088607, -0.6046776061558807314, 0.2411417322834647770 ) ) ;
#23839 = ADVANCED_FACE ( 'NONE', ( #75887 ), #18228, .T. ) ;
#23840 = CARTESIAN_POINT ( 'NONE',  ( -0.9580052493438311334, 0.05413385826771626580, -0.4176697321401330321 ) ) ;
#23841 = CARTESIAN_POINT ( 'NONE',  ( -0.3458507752293906723, -0.3458507752293910609, -0.7657480314960628531 ) ) ;
#23842 = CARTESIAN_POINT ( 'NONE',  ( -0.02624671916010428221, -0.6046776061558807314, 0.2411417322834647770 ) ) ;
#23843 = CARTESIAN_POINT ( 'NONE',  ( -0.5708661417322825615, -0.5400638737290844871, 0.3530559997133364547 ) ) ;
#23844 = CARTESIAN_POINT ( 'NONE',  ( 1.200787401574803681, 0.07958543189024085140, 0.2665933059059887866 ) ) ;
#23845 = CARTESIAN_POINT ( 'NONE',  ( 0.09186351706036799403, -0.3690944881889765550, -0.3153832671262227771 ) ) ;
#23846 = CARTESIAN_POINT ( 'NONE',  ( -0.1837270341207343505, -0.6046776061558807314, 0.2411417322834647770 ) ) ;
#23847 = CARTESIAN_POINT ( 'NONE',  ( -1.122047244094487306, 0.1660481256975883668, -0.3530559997133364547 ) ) ;
#23848 = DIRECTION ( 'NONE',  ( 0.000000000000000000, -1.224646799147351482E-16, 1.000000000000000000 ) ) ;
#23849 = CARTESIAN_POINT ( 'NONE',  ( 1.928577636452524918E-17, 0.000000000000000000, 0.1574803149606299746 ) ) ;
#23850 = CARTESIAN_POINT ( 'NONE',  ( 0.04593175853018440641, -0.6692913385826771977, 0.1292274648535927661 ) ) ;
#23851 = VERTEX_POINT ( 'NONE', #57741 ) ;
#23852 = CARTESIAN_POINT ( 'NONE',  ( 0.1070741851644053388, 0.3996062992125986035, -1.959973753280839892 ) ) ;
#23853 = CARTESIAN_POINT ( 'NONE',  ( 1.122047244094488860, 0.1660481256975885056, 0.3530559997133364547 ) ) ;
#23854 = CARTESIAN_POINT ( 'NONE',  ( -0.7677165354330699465, 0.07958543189024085140, 0.2665933059059887866 ) ) ;
#23855 = CARTESIAN_POINT ( 'NONE',  ( -0.4461942257217840213, 0.2306618581243848609, 0.2411417322834645549 ) ) ;
#23856 = CARTESIAN_POINT ( 'NONE',  ( 1.148293963254593875, -0.6692913385826771977, 0.1292274648535927661 ) ) ;
#23857 = CARTESIAN_POINT ( 'NONE',  ( 1.062992125984252745, 0.2952755905511811885, 0.000000000000000000 ) ) ;
#23858 = CARTESIAN_POINT ( 'NONE',  ( -1.627296587926508442, 0.2306618581243848609, 0.2411417322834645549 ) ) ;
#23859 = CARTESIAN_POINT ( 'NONE',  ( -0.8989501312335946848, 0.1771653543307087075, -0.09757992244046823083 ) ) ;
#23860 = CARTESIAN_POINT ( 'NONE',  ( 0.3996062992125984925, 0.1070741851644054499, -0.04396325459317587669 ) ) ;
#23861 = CARTESIAN_POINT ( 'NONE',  ( 0.1070741851644053527, 0.3996062992125986590, -0.6233595800524933672 ) ) ;
#23862 = CARTESIAN_POINT ( 'NONE',  ( 0.1974969037888704704, 0.3420746716998660508, 0.01312335958005243601 ) ) ;
#23863 = CARTESIAN_POINT ( 'NONE',  ( 1.509186351706037543, -0.004921259842519576551, 0.3153832671262227771 ) ) ;
#23864 = CARTESIAN_POINT ( 'NONE',  ( 0.5511811023622054106, -0.1870078740157480601, -0.3641732283464567677 ) ) ;
#23865 = CARTESIAN_POINT ( 'NONE',  ( 0.5971128608923890191, -0.6692913385826771977, 0.1292274648535927661 ) ) ;
#23866 = CARTESIAN_POINT ( 'NONE',  ( 0.4724409448818898682, 2.892866454678787531E-17, -2.399606299212598604 ) ) ;
#23867 = CARTESIAN_POINT ( 'NONE',  ( -0.3949938075777408852, -0.1058382717557502933, -0.7526246719160105680 ) ) ;
#23868 = CARTESIAN_POINT ( 'NONE',  ( 0.6364829396325465405, -0.2845877964562161244, -0.3641732283464567121 ) ) ;
#23869 = CARTESIAN_POINT ( 'NONE',  ( -0.4790026246719152336, -0.05778040916215560624, -0.4822834645669293319 ) ) ;
#23870 = CARTESIAN_POINT ( 'NONE',  ( -0.6364829396325453192, -0.05778040916215560624, -0.4822834645669293319 ) ) ;
#23871 = CARTESIAN_POINT ( 'NONE',  ( 1.135170603674541256, -0.6692913385826773087, -0.1292274648535924053 ) ) ;
#23872 = CARTESIAN_POINT ( 'NONE',  ( 0.2362204724409451007, -0.4091458600556402980, -1.351706036745406792 ) ) ;
#23873 = AXIS2_PLACEMENT_3D ( 'NONE', #64036, #64875, #58554 ) ;
#23874 = CARTESIAN_POINT ( 'NONE',  ( 0.3460692066303959202, 0.1998031496062993295, -2.178477690288713742 ) ) ;
#23875 = CARTESIAN_POINT ( 'NONE',  ( -0.1115485564304456306, 0.1771653543307087075, -0.09757992244046823083 ) ) ;
#23876 = EDGE_CURVE ( 'NONE', #39166, #34321, #32265, .T. ) ;
#23877 = ORIENTED_EDGE ( 'NONE', *, *, #9959, .F. ) ;
#23878 = CARTESIAN_POINT ( 'NONE',  ( 0.1958661417322834775, 0.3392501089628018884, -0.7710166911099232134 ) ) ;
#23879 = VERTEX_POINT ( 'NONE', #40903 ) ;
#23880 = CARTESIAN_POINT ( 'NONE',  ( -0.7742782152230965886, 0.05413385826771666132, 0.4176697321401328100 ) ) ;
#23881 = CARTESIAN_POINT ( 'NONE',  ( -0.006561679790025524116, -0.05778040916215560624, -0.4822834645669293319 ) ) ;
#23882 = CARTESIAN_POINT ( 'NONE',  ( -0.2559055118110227234, -0.5400638737290844871, 0.3530559997133364547 ) ) ;
#23883 = CARTESIAN_POINT ( 'NONE',  ( 0.3740157480314966754, -0.5400638737290844871, 0.3530559997133364547 ) ) ;
#23884 = CARTESIAN_POINT ( 'NONE',  ( -0.5905511811023613777, -0.6692913385826771977, 8.415575281601705876E-17 ) ) ;
#23885 = CARTESIAN_POINT ( 'NONE',  ( -1.351706036745406347, -0.4281496062992124485, 0.4176697321401328655 ) ) ;
#23886 = CARTESIAN_POINT ( 'NONE',  ( -0.9448818897637790704, -0.1870078740157479769, 0.4822834645669291653 ) ) ;
#23887 = CARTESIAN_POINT ( 'NONE',  ( 0.7611548556430451917, -0.6046776061558807314, 0.2411417322834647770 ) ) ;
#23888 = CARTESIAN_POINT ( 'NONE',  ( 0.4068241469816279987, -0.4281496062992127816, -0.4176697321401328100 ) ) ;
#23889 = ADVANCED_FACE ( 'NONE', ( #79642 ), #24961, .F. ) ;
#23890 = CARTESIAN_POINT ( 'NONE',  ( -0.3392501089628019995, 0.1958661417322832277, -1.120734908136482799 ) ) ;
#23891 = CARTESIAN_POINT ( 'NONE',  ( -0.3937007874015740483, -0.1870078740157479769, 0.3641732283464567677 ) ) ;
#23892 = EDGE_LOOP ( 'NONE', ( #25933, #59152, #61867, #823, #13526 ) ) ;
#23893 = CARTESIAN_POINT ( 'NONE',  ( -0.2891555358219908833, -0.2891555358219912164, -1.633858267716535195 ) ) ;
#23894 = VERTEX_POINT ( 'NONE', #77968 ) ;
#23895 = CARTESIAN_POINT ( 'NONE',  ( -1.233595800524933894, 0.1283753931104748280, 0.1820866141732283561 ) ) ;
#23896 = CARTESIAN_POINT ( 'NONE',  ( -1.062992125984250968, -0.6692913385826771977, 8.415575281601705876E-17 ) ) ;
#23897 = CARTESIAN_POINT ( 'NONE',  ( -0.6233595800524928121, -0.3162353388693409650, -0.4822834645669289433 ) ) ;
#23898 = CARTESIAN_POINT ( 'NONE',  ( 0.7770624478417551551, 1.702998256715020864E-15, -0.4281989832122454209 ) ) ;
#23899 = CARTESIAN_POINT ( 'NONE',  ( -0.5249343832020990641, -0.6046776061558809534, -0.2411417322834644161 ) ) ;
#23900 = CARTESIAN_POINT ( 'NONE',  ( -0.9711286089238838626, -0.6046776061558807314, 0.2411417322834647770 ) ) ;
#23901 = DIRECTION ( 'NONE',  ( 0.000000000000000000, 0.000000000000000000, -1.000000000000000000 ) ) ;
#23902 = DIRECTION ( 'NONE',  ( 0.000000000000000000, 1.000000000000000000, 0.000000000000000000 ) ) ;
#23903 = CARTESIAN_POINT ( 'NONE',  ( 0.8005249343832028242, -0.3690944881889765550, -0.3153832671262227771 ) ) ;
#23904 = CARTESIAN_POINT ( 'NONE',  ( 1.968503937007874072, 0.000000000000000000, 5.544487991299990703 ) ) ;
#23905 = CARTESIAN_POINT ( 'NONE',  ( 0.1049643490035304938, -0.3917322834645669549, -0.01246719160104995359 ) ) ;
#23906 = CARTESIAN_POINT ( 'NONE',  ( 0.05249343832021075018, 0.1283753931104746893, -0.1820866141732285504 ) ) ;
#23907 = CARTESIAN_POINT ( 'NONE',  ( -0.5577427821522301654, -0.3162353388693405765, 0.4822834645669290543 ) ) ;
#23908 = CARTESIAN_POINT ( 'NONE',  ( -1.614173228346456712, 2.401574803149606474, -0.1372047244094478091 ) ) ;
#23909 = CARTESIAN_POINT ( 'NONE',  ( 0.08530183727034192087, -0.05778040916215522460, 0.4822834645669289988 ) ) ;
#23910 = EDGE_LOOP ( 'NONE', ( #73509, #26482, #12083 ) ) ;
#23911 = CARTESIAN_POINT ( 'NONE',  ( 0.1998031496062994405, -0.3460692066303958092, -1.981627296587926690 ) ) ;
#23912 = CARTESIAN_POINT ( 'NONE',  ( -0.6299212598425060206, 1.724409448818897905, -3.886287458032464226 ) ) ;
#23913 = ORIENTED_EDGE ( 'NONE', *, *, #8974, .F. ) ;
#23914 = CARTESIAN_POINT ( 'NONE',  ( -0.2925321140481930149, -0.2925321140481933480, -1.395669291338582196 ) ) ;
#23915 = CARTESIAN_POINT ( 'NONE',  ( -0.1133856558944469489, 0.2726377952755905665, 0.1574803149606299191 ) ) ;
#23916 = CARTESIAN_POINT ( 'NONE',  ( -0.7545931758530177724, 0.1771653543307087630, 0.09757992244046791164 ) ) ;
#23917 = CARTESIAN_POINT ( 'NONE',  ( -0.9317585301837263412, 0.05413385826771666132, 0.4176697321401328100 ) ) ;
#23918 = CARTESIAN_POINT ( 'NONE',  ( 0.4724409448818898682, 2.892866454678787531E-17, -0.5905511811023621549 ) ) ;
#23919 = CARTESIAN_POINT ( 'NONE',  ( -0.1959442453386707195, 1.105068466360755064, 3.932155085606260148 ) ) ;
#23920 = CARTESIAN_POINT ( 'NONE',  ( -0.3917322834645671215, 0.1049643490035301469, 0.1325459317585302443 ) ) ;
#23921 = CARTESIAN_POINT ( 'NONE',  ( 1.318897637795276356, -0.5400638737290844871, 0.3530559997133364547 ) ) ;
#23922 = CARTESIAN_POINT ( 'NONE',  ( 0.2821522309711292364, -0.6692913385826771977, 0.1292274648535927661 ) ) ;
#23923 = CARTESIAN_POINT ( 'NONE',  ( 0.4461942257217856311, 0.2306618581243847221, -0.2411417322834647770 ) ) ;
#23924 = CARTESIAN_POINT ( 'NONE',  ( -0.6955380577427815458, -0.004921259842519576551, 0.3153832671262227771 ) ) ;
#23925 = CARTESIAN_POINT ( 'NONE',  ( -0.5183727034120726440, -0.6692913385826773087, -0.1292274648535924053 ) ) ;
#23926 = CARTESIAN_POINT ( 'NONE',  ( 5.785732909357575061E-17, -0.4724409448818898682, -2.360236220472441193 ) ) ;
#23927 = CARTESIAN_POINT ( 'NONE',  ( -0.7545931758530177724, 0.2952755905511811885, 0.1292274648535926551 ) ) ;
#23928 = CARTESIAN_POINT ( 'NONE',  ( 0.2891555358219910499, -0.2891555358219909944, -2.379921259842519898 ) ) ;
#23929 = CARTESIAN_POINT ( 'NONE',  ( 1.220472440944882386, -0.5511811023622047445, 6.969142054262312111E-17 ) ) ;
#23930 = CARTESIAN_POINT ( 'NONE',  ( -0.2230971128608915943, -0.3690944881889765550, -0.3153832671262227771 ) ) ;
#23931 = CARTESIAN_POINT ( 'NONE',  ( 1.036745406824147731, -0.004921259842519576551, 0.3153832671262227771 ) ) ;
#23932 = CARTESIAN_POINT ( 'NONE',  ( 1.587926509186352142, -0.004921259842519576551, 0.3153832671262227771 ) ) ;
#23933 = CARTESIAN_POINT ( 'NONE',  ( -1.259842519685038686, -0.1870078740157480601, -0.3641732283464567677 ) ) ;
#23934 = CARTESIAN_POINT ( 'NONE',  ( 0.6496062992125991586, -0.4536011799217368745, -0.2665933059059886201 ) ) ;
#23935 = CARTESIAN_POINT ( 'NONE',  ( -0.3280839895013117347, 0.05413385826771626580, -0.4176697321401330321 ) ) ;
#23936 = CARTESIAN_POINT ( 'NONE',  ( -1.947231901457312064, 1.169463170161832100, 0.3010181502270706244 ) ) ;
#23937 = CARTESIAN_POINT ( 'NONE',  ( -0.2165354330708654795, 0.07958543189024085140, 0.2665933059059887866 ) ) ;
#23938 = DIRECTION ( 'NONE',  ( 1.000000000000000000, 0.000000000000000000, 0.000000000000000000 ) ) ;
#23939 = CARTESIAN_POINT ( 'NONE',  ( 0.6167979002624679463, 0.05413385826771626580, -0.4176697321401330321 ) ) ;
#23940 = CARTESIAN_POINT ( 'NONE',  ( 0.6399301791983058596, -1.374501131054255944E-15, 0.4445507791589066726 ) ) ;
#23941 = CARTESIAN_POINT ( 'NONE',  ( 1.469816272965879911, 0.1283753931104746893, -0.1820866141732285504 ) ) ;
#23942 = CARTESIAN_POINT ( 'NONE',  ( -0.8792650918635160906, 0.05413385826771626580, -0.4176697321401330321 ) ) ;
#23943 = CARTESIAN_POINT ( 'NONE',  ( -0.3280839895013117347, -0.004921259842519870586, -0.3153832671262229437 ) ) ;
#23944 = FACE_OUTER_BOUND ( 'NONE', #56873, .T. ) ;
#23945 = CARTESIAN_POINT ( 'NONE',  ( 0.3740157480314966754, 0.07958543189024071263, -0.2665933059059888421 ) ) ;
#23946 = CARTESIAN_POINT ( 'NONE',  ( -0.4527559055118102749, -0.5400638737290845981, -0.3530559997133363437 ) ) ;
#23947 = CARTESIAN_POINT ( 'NONE',  ( 0.3996062992125986035, -0.1070741851644052972, -0.6607611548556431291 ) ) ;
#23948 = CARTESIAN_POINT ( 'NONE',  ( 0.1958661417322836440, -0.3392501089628017219, -2.066272965879265122 ) ) ;
#23949 = CARTESIAN_POINT ( 'NONE',  ( 0.6233595800524939223, -0.2845877964562159024, 0.3641732283464567677 ) ) ;
#23950 = CARTESIAN_POINT ( 'NONE',  ( -0.3149606299212590610, -0.1870078740157480879, -0.4822834645669291653 ) ) ;
#23951 = CARTESIAN_POINT ( 'NONE',  ( -0.8792650918635160906, -0.4281496062992124485, 0.4176697321401328655 ) ) ;
#23952 = CARTESIAN_POINT ( 'NONE',  ( -0.6102362204724400829, -0.4536011799217368745, -0.2665933059059886201 ) ) ;
#23953 = CARTESIAN_POINT ( 'NONE',  ( -3.913864544620323294, 1.327201601969144829, 0.4264239150993004990 ) ) ;
#23954 = CARTESIAN_POINT ( 'NONE',  ( -0.01968503937007793844, 0.1660481256975883668, -0.3530559997133364547 ) ) ;
#23955 = EDGE_CURVE ( 'NONE', #6933, #38768, #48756, .T. ) ;
#23956 = CARTESIAN_POINT ( 'NONE',  ( -1.279527559055116948, -0.4536011799217367080, 0.2665933059059888421 ) ) ;
#23957 = CARTESIAN_POINT ( 'NONE',  ( -1.443569553805773564, 0.2306618581243847221, -0.2411417322834647770 ) ) ;
#23958 = CARTESIAN_POINT ( 'NONE',  ( 0.3458507752293908943, 0.3458507752293908943, -2.185039370078739829 ) ) ;
#23959 = B_SPLINE_CURVE_WITH_KNOTS ( 'NONE', 3,
 ( #30011, #54860, #10262, #17820, #35930, #36739, #4344, #17414, #4753, #43453 ),
 .UNSPECIFIED., .F., .F.,
 ( 4, 2, 2, 2, 4 ),
 ( 0.04304707915996866530, 0.04426528421037419919, 0.04548348926077973309, 0.04670169431118526698, 0.04791989936159080088 ),
 .UNSPECIFIED. ) ;
#23960 = EDGE_LOOP ( 'NONE', ( #82490, #77946 ) ) ;
#23961 = EDGE_CURVE ( 'NONE', #33187, #27190, #76410, .T. ) ;
#23962 = CARTESIAN_POINT ( 'NONE',  ( -1.404199475065615932, -0.004921259842519576551, 0.3153832671262227771 ) ) ;
#23963 = CARTESIAN_POINT ( 'NONE',  ( -1.371391076115484831, 0.2952755905511810774, -0.1292274648535930714 ) ) ;
#23964 = CARTESIAN_POINT ( 'NONE',  ( -1.030183727034119867, -0.05778040916215560624, -0.4822834645669293319 ) ) ;
#23965 = CARTESIAN_POINT ( 'NONE',  ( -1.056430446194224881, -0.6692913385826771977, 0.1292274648535927661 ) ) ;
#23966 = CARTESIAN_POINT ( 'NONE',  ( 0.1958661417322834775, 0.3392501089628018884, -1.488845144356955252 ) ) ;
#23967 = CARTESIAN_POINT ( 'NONE',  ( 0.006303098004689107643, 0.3922539627124311812, -1.220472440944881720 ) ) ;
#23968 = CARTESIAN_POINT ( 'NONE',  ( 1.030183727034121421, -0.05778040916215522460, 0.4822834645669289988 ) ) ;
#23969 = CARTESIAN_POINT ( 'NONE',  ( 0.3215223097112867578, -0.3162353388693409650, -0.4822834645669289433 ) ) ;
#23970 = CARTESIAN_POINT ( 'NONE',  ( 1.220472440944879722, 1.496062992125984037, 0.5309055118110233007 ) ) ;
#23971 = CARTESIAN_POINT ( 'NONE',  ( 0.1998031496062992463, 0.3460692066303959202, -2.583333333333333481 ) ) ;
#23972 = CARTESIAN_POINT ( 'NONE',  ( 1.148293963254593653, 0.1771653543307087075, -0.09757992244046823083 ) ) ;
#23973 = CARTESIAN_POINT ( 'NONE',  ( -0.3460692066303958092, -0.1998031496062994683, -0.9973753280839895430 ) ) ;
#23974 = ORIENTED_EDGE ( 'NONE', *, *, #54140, .T. ) ;
#23975 = CARTESIAN_POINT ( 'NONE',  ( -0.8464566929133852113, 0.07958543189024085140, 0.2665933059059887866 ) ) ;
#23976 = CARTESIAN_POINT ( 'NONE',  ( -0.3392501089628019995, 0.1958661417322832277, -2.538057742782152015 ) ) ;
#23977 = ORIENTED_EDGE ( 'NONE', *, *, #3360, .F. ) ;
#23978 = CARTESIAN_POINT ( 'NONE',  ( 0.2099737532808405305, 0.2306618581243847221, -0.2411417322834647770 ) ) ;
#23979 = CARTESIAN_POINT ( 'NONE',  ( -0.5118110236220466680, -0.6692913385826771977, 8.415575281601705876E-17 ) ) ;
#23980 =( REPRESENTATION_RELATIONSHIP ('NONE','NONE', #79348, #48103 ) REPRESENTATION_RELATIONSHIP_WITH_TRANSFORMATION ( #6007 )SHAPE_REPRESENTATION_RELATIONSHIP( ) );
#23981 = CARTESIAN_POINT ( 'NONE',  ( -1.207349081364828436, -0.6046776061558807314, 0.2411417322834647770 ) ) ;
#23982 = CARTESIAN_POINT ( 'NONE',  ( 1.233595800524935227, 0.2306618581243847221, -0.2411417322834647770 ) ) ;
#23983 = CARTESIAN_POINT ( 'NONE',  ( 1.620734908136483465, -0.6692913385826771977, 0.1292274648535927661 ) ) ;
#23984 = CARTESIAN_POINT ( 'NONE',  ( 0.09115970038225353067, 3.421639014772782816E-16, 0.3464511005275203726 ) ) ;
#23985 = CARTESIAN_POINT ( 'NONE',  ( -0.06561679790026180015, 0.05413385826771666132, 0.4176697321401328100 ) ) ;
#23986 = CARTESIAN_POINT ( 'NONE',  ( -1.062992125984250968, -0.6692913385826771977, 8.415575281601705876E-17 ) ) ;
#23987 = CARTESIAN_POINT ( 'NONE',  ( -0.3392501089628019439, 0.1958661417322832554, -1.996043676344145146 ) ) ;
#23988 = CARTESIAN_POINT ( 'NONE',  ( -1.646981627296586703, -0.05778040916215522460, 0.4822834645669289988 ) ) ;
#23989 = CARTESIAN_POINT ( 'NONE',  ( 1.489501312335958172, -0.3162353388693405765, 0.4822834645669290543 ) ) ;
#23990 = CARTESIAN_POINT ( 'NONE',  ( 0.3917322834645670104, 2.398668435337828261E-17, -2.722440944881889369 ) ) ;
#23991 = CARTESIAN_POINT ( 'NONE',  ( 0.7414698162729663755, 0.1771653543307087630, 0.09757992244046791164 ) ) ;
#23992 = ORIENTED_EDGE ( 'NONE', *, *, #73735, .F. ) ;
#23993 = CARTESIAN_POINT ( 'NONE',  ( 0.3420746716998660508, -0.1974969037888703871, -0.2624671916010499206 ) ) ;
#23994 = CARTESIAN_POINT ( 'NONE',  ( -1.049868766404198794, -0.6046776061558807314, 0.2411417322834647770 ) ) ;
#23995 = ORIENTED_EDGE ( 'NONE', *, *, #43710, .T. ) ;
#23996 = CARTESIAN_POINT ( 'NONE',  ( -0.09842519685039295696, 0.07958543189024071263, -0.2665933059059888421 ) ) ;
#23997 = CARTESIAN_POINT ( 'NONE',  ( 0.4724409448818898682, 2.892866454678787531E-17, -0.1181102362204724532 ) ) ;
#23998 = CARTESIAN_POINT ( 'NONE',  ( 0.4199475065616803948, -0.6046776061558809534, -0.2411417322834644161 ) ) ;
#23999 = CARTESIAN_POINT ( 'NONE',  ( 0.4133858267716541968, -0.5400638737290845981, -0.3530559997133363437 ) ) ;
#24000 = CARTESIAN_POINT ( 'NONE',  ( -0.5052493438320203589, -0.6692913385826771977, 0.1292274648535927661 ) ) ;
#24001 = CARTESIAN_POINT ( 'NONE',  ( -0.3392501089628017219, -0.1958661417322836995, -1.151594118931445365 ) ) ;
#24002 = CARTESIAN_POINT ( 'NONE',  ( -0.8530183727034112984, 0.05413385826771666132, 0.4176697321401328100 ) ) ;
#24003 = CARTESIAN_POINT ( 'NONE',  ( 0.3917322834645670104, -0.1049643490035303411, -2.715879265091863726 ) ) ;
#24004 = CARTESIAN_POINT ( 'NONE',  ( 1.233595800524935227, -0.5023911411419708095, 0.1820866141732285504 ) ) ;
#24005 = CARTESIAN_POINT ( 'NONE',  ( -1.181102362204723644, -0.1870078740157479769, 0.4822834645669291653 ) ) ;
#24006 = CARTESIAN_POINT ( 'NONE',  ( 0.9711286089238851948, -0.6046776061558809534, -0.2411417322834644161 ) ) ;
#24007 = CARTESIAN_POINT ( 'NONE',  ( 1.148293963254593875, -0.6692913385826771977, 0.1292274648535927661 ) ) ;
#24008 = CARTESIAN_POINT ( 'NONE',  ( 0.1070741851644054915, -0.3996062992125986035, -0.8727034120734907807 ) ) ;
#24009 = CARTESIAN_POINT ( 'NONE',  ( -1.528871391076114250, 0.2952755905511810774, -0.1292274648535930714 ) ) ;
#24010 = CARTESIAN_POINT ( 'NONE',  ( 4.893765752498283308E-17, -0.3996062992125985480, -0.1555118110236220763 ) ) ;
#24011 = CARTESIAN_POINT ( 'NONE',  ( 0.4593175853018379162, -0.4281496062992124485, 0.4176697321401328655 ) ) ;
#24012 = CARTESIAN_POINT ( 'NONE',  ( 0.3996062992125986035, 2.446882876249141962E-17, -2.165354330708661568 ) ) ;
#24013 = CARTESIAN_POINT ( 'NONE',  ( -1.581364829396324945, -0.08942795157528024563, -0.3641732283464568787 ) ) ;
#24014 = CARTESIAN_POINT ( 'NONE',  ( 0.6036745406824154392, 0.1283753931104746893, -0.1820866141732285504 ) ) ;
#24015 = CARTESIAN_POINT ( 'NONE',  ( 0.9973753280839902091, 0.2306618581243847221, -0.2411417322834647770 ) ) ;
#24016 = CARTESIAN_POINT ( 'NONE',  ( 0.3458507752293908943, 0.3458507752293908943, -1.001968503937007871 ) ) ;
#24017 = CARTESIAN_POINT ( 'NONE',  ( 0.6824146981627303710, -0.5023911411419708095, 0.1820866141732285504 ) ) ;
#24018 = CARTESIAN_POINT ( 'NONE',  ( 0.5118110236220478892, 0.2952755905511811885, 0.000000000000000000 ) ) ;
#24019 = CARTESIAN_POINT ( 'NONE',  ( 0.3420746716998660508, -0.1974969037888704149, -1.126640419947506633 ) ) ;
#24020 = CARTESIAN_POINT ( 'NONE',  ( -0.8202099737532801971, -0.6692913385826771977, 0.1292274648535927661 ) ) ;
#24021 = CARTESIAN_POINT ( 'NONE',  ( 0.4359958488159859646, 1.724409448818897905, -3.937007874015760578 ) ) ;
#24022 = CARTESIAN_POINT ( 'NONE',  ( 1.017060367454068581, -0.08942795157528024563, -0.3641732283464568787 ) ) ;
#24023 = CARTESIAN_POINT ( 'NONE',  ( -0.07874015748031421014, -0.1870078740157480879, -0.4822834645669291653 ) ) ;
#24024 = DIRECTION ( 'NONE',  ( -0.000000000000000000, -1.000000000000000000, -0.000000000000000000 ) ) ;
#24025 = CARTESIAN_POINT ( 'NONE',  ( -0.5052493438320203589, -0.6692913385826771977, 0.1292274648535927661 ) ) ;
#24026 = CARTESIAN_POINT ( 'NONE',  ( 0.09186351706036827158, -0.004921259842519576551, 0.3153832671262227771 ) ) ;
#24027 = CARTESIAN_POINT ( 'NONE',  ( -2.593372381816044570, 1.408244132531270454, 0.4567322424080941246 ) ) ;
#24028 = CARTESIAN_POINT ( 'NONE',  ( 0.03280839895013198948, -0.5511811023622048555, -0.09757992244046775898 ) ) ;
#24029 = CARTESIAN_POINT ( 'NONE',  ( 0.7283464566929140904, -0.4536011799217368745, -0.2665933059059886201 ) ) ;
#24030 = CARTESIAN_POINT ( 'NONE',  ( 0.2925321140481932369, 0.2925321140481932369, -1.789370078740157410 ) ) ;
#24031 = CARTESIAN_POINT ( 'NONE',  ( 0.2165354330708668673, -0.5400638737290844871, 0.3530559997133364547 ) ) ;
#24032 = CARTESIAN_POINT ( 'NONE',  ( 0.3917322834645670104, -0.1049643490035303411, -1.520997375328083656 ) ) ;
#24033 = CARTESIAN_POINT ( 'NONE',  ( 1.010498687664042716, -0.3690944881889763329, 0.3153832671262228327 ) ) ;
#24034 = DIRECTION ( 'NONE',  ( -3.096699300667737957E-16, 1.000000000000000000, -0.000000000000000000 ) ) ;
#24035 = CARTESIAN_POINT ( 'NONE',  ( -0.5708661417322828946, 0.07958543189024071263, -0.2665933059059888421 ) ) ;
#24036 = CARTESIAN_POINT ( 'NONE',  ( -0.2821522309711278487, 0.1771653543307087630, 0.09757992244046791164 ) ) ;
#24037 = CARTESIAN_POINT ( 'NONE',  ( -0.4461942257217840213, -0.6046776061558809534, -0.2411417322834644161 ) ) ;
#24038 = CARTESIAN_POINT ( 'NONE',  ( 0.7808398950131241190, -0.08942795157528024563, -0.3641732283464568787 ) ) ;
#24039 = CARTESIAN_POINT ( 'NONE',  ( -0.2952755905511811885, 0.01202990275164721352, 5.879133660591332244 ) ) ;
#24040 = CARTESIAN_POINT ( 'NONE',  ( 1.417322834645670104, -0.1870078740157479769, 0.3641732283464567677 ) ) ;
#24041 = CARTESIAN_POINT ( 'NONE',  ( 0.02624671916010564918, -0.6046776061558809534, -0.2411417322834644161 ) ) ;
#24042 = CARTESIAN_POINT ( 'NONE',  ( 0.9973753280839902091, -0.6046776061558807314, 0.2411417322834647770 ) ) ;
#24043 = CARTESIAN_POINT ( 'NONE',  ( 0.2516608251556240461, 1.134091190147781925, -1.915569722591573987 ) ) ;
#24044 = CARTESIAN_POINT ( 'NONE',  ( 0.2493438320209980519, -0.4281496062992127816, -0.4176697321401328100 ) ) ;
#24045 = CARTESIAN_POINT ( 'NONE',  ( 0.3917322834645669549, 0.1049643490035304660, -1.154199475065616820 ) ) ;
#24046 = CARTESIAN_POINT ( 'NONE',  ( 1.036745406824147731, 0.05413385826771666132, 0.4176697321401328100 ) ) ;
#24047 = CARTESIAN_POINT ( 'NONE',  ( 0.7086614173228353852, -0.1870078740157479769, 0.4822834645669291653 ) ) ;
#24048 = CARTESIAN_POINT ( 'NONE',  ( -0.3771896033470157894, 1.248011834530954323, -3.918935672522287916 ) ) ;
#24049 = CARTESIAN_POINT ( 'NONE',  ( 0.7152230971128616943, -0.08942795157527998196, 0.3641732283464567121 ) ) ;
#24050 = CARTESIAN_POINT ( 'NONE',  ( 1.345144356955381593, -0.05778040916215522460, 0.4822834645669289988 ) ) ;
#24051 = EDGE_CURVE ( 'NONE', #52467, #29190, #2611, .T. ) ;
#24052 = CARTESIAN_POINT ( 'NONE',  ( 0.2559055118110243332, -0.4536011799217368745, -0.2665933059059886201 ) ) ;
#24053 = CARTESIAN_POINT ( 'NONE',  ( -0.1115485564304453947, -0.6692913385826771977, 0.1292274648535927661 ) ) ;
#24054 = CARTESIAN_POINT ( 'NONE',  ( 0.4265091863517067039, -0.6692913385826773087, -0.1292274648535924053 ) ) ;
#24055 = CARTESIAN_POINT ( 'NONE',  ( -0.6561679790026240244, 0.2306618581243847221, -0.2411417322834647770 ) ) ;
#24056 = CARTESIAN_POINT ( 'NONE',  ( -0.4461942257217840213, 0.1283753931104748280, 0.1820866141732283561 ) ) ;
#24057 = B_SPLINE_CURVE_WITH_KNOTS ( 'NONE', 3,
 ( #30213, #31868, #30633, #64273 ),
 .UNSPECIFIED., .F., .F.,
 ( 4, 4 ),
 ( 1.999999999910059834E-07, 0.006970199999999935996 ),
 .UNSPECIFIED. ) ;
#24058 = CARTESIAN_POINT ( 'NONE',  ( 0.9776902887139113929, 0.2952755905511811885, 0.1292274648535926551 ) ) ;
#24059 = CARTESIAN_POINT ( 'NONE',  ( 0.8858267716535438430, 0.07958543189024085140, 0.2665933059059887866 ) ) ;
#24060 = CARTESIAN_POINT ( 'NONE',  ( -0.01312335958005186876, 0.05413385826771626580, -0.4176697321401330321 ) ) ;
#24061 = SURFACE_SIDE_STYLE ('',( #5124 ) ) ;
#24063 = CARTESIAN_POINT ( 'NONE',  ( -0.3996062992125986035, -7.340648628747425578E-17, -1.141732283464566899 ) ) ;
#24062 = CARTESIAN_POINT ( 'NONE',  ( 3.900966923095589678, 2.755905511811024056, 0.5314960629921260393 ) ) ;
#24064 = CARTESIAN_POINT ( 'NONE',  ( 0.2952755905511810774, 0.000000000000000000, -1.929133858267716661 ) ) ;
#24065 = CARTESIAN_POINT ( 'NONE',  ( 0.1049643490035303689, 0.3917322834645670104, -2.190288713910760965 ) ) ;
#24066 = CARTESIAN_POINT ( 'NONE',  ( -1.397637795275589623, -0.5400638737290845981, -0.3530559997133363437 ) ) ;
#24067 = CARTESIAN_POINT ( 'NONE',  ( -1.003937007874015297, -0.5400638737290845981, -0.3530559997133363437 ) ) ;
#24068 = CARTESIAN_POINT ( 'NONE',  ( -0.2362204724409447953, -0.4091458600556404646, -0.3805774278215223183 ) ) ;
#24069 = CARTESIAN_POINT ( 'NONE',  ( -0.1058382717557497937, -0.3949938075777411628, -2.591863517060367883 ) ) ;
#24070 = ORIENTED_EDGE ( 'NONE', *, *, #62908, .F. ) ;
#24071 = CARTESIAN_POINT ( 'NONE',  ( 0.4593175853018380828, -0.004921259842519870586, -0.3153832671262229437 ) ) ;
#24072 = CARTESIAN_POINT ( 'NONE',  ( 0.2867679344610365999, 0.2867679344610365999, -1.389763779527558807 ) ) ;
#24073 = CARTESIAN_POINT ( 'NONE',  ( 0.5118110236220478892, 0.2952755905511811885, 0.000000000000000000 ) ) ;
#24074 = CARTESIAN_POINT ( 'NONE',  ( -0.4724409448818899238, 0.1265901696524986686, -2.552493438320210029 ) ) ;
#24075 = CARTESIAN_POINT ( 'NONE',  ( -1.157146581871515012E-16, 0.4724409448818898682, -0.8641732283464567121 ) ) ;
#24076 = CARTESIAN_POINT ( 'NONE',  ( -1.633858267716534529, -0.4536011799217368745, -0.2665933059059886201 ) ) ;
#24077 = CARTESIAN_POINT ( 'NONE',  ( 1.082677165354331228, 0.1660481256975883668, -0.3530559997133364547 ) ) ;
#24078 = CARTESIAN_POINT ( 'NONE',  ( 1.299212598425197429, 0.1771653543307087630, 0.000000000000000000 ) ) ;
#24079 = CARTESIAN_POINT ( 'NONE',  ( 0.09186351706036827158, 0.05413385826771666132, 0.4176697321401328100 ) ) ;
#24080 = CARTESIAN_POINT ( 'NONE',  ( -0.2867679344610366554, 0.2867679344610365444, -0.5721591619084497315 ) ) ;
#24081 = CARTESIAN_POINT ( 'NONE',  ( -0.5249343832020990641, 0.2306618581243848609, 0.2411417322834645549 ) ) ;
#24082 = CARTESIAN_POINT ( 'NONE',  ( -0.9973753280839886548, -0.5023911411419708095, -0.1820866141732282451 ) ) ;
#24083 = CARTESIAN_POINT ( 'NONE',  ( 0.5118110236220478892, 0.2952755905511811885, 0.000000000000000000 ) ) ;
#24084 = CARTESIAN_POINT ( 'NONE',  ( -0.6889763779527552368, -0.5400638737290845981, -0.3530559997133363437 ) ) ;
#24085 = CARTESIAN_POINT ( 'NONE',  ( 1.673228346456693494, 0.1660481256975885056, 0.3530559997133364547 ) ) ;
#24086 = CARTESIAN_POINT ( 'NONE',  ( 0.000000000000000000, 0.4374015748031496176, 1.122047244094488194 ) ) ;
#24087 = ORIENTED_EDGE ( 'NONE', *, *, #2516, .F. ) ;
#24088 = CARTESIAN_POINT ( 'NONE',  ( -0.1049643490035307158, 0.3917322834645670104, -1.893063935204411186 ) ) ;
#24089 = CARTESIAN_POINT ( 'NONE',  ( 0.5643044619422579178, 0.05413385826771666132, 0.4176697321401328100 ) ) ;
#24090 = CARTESIAN_POINT ( 'NONE',  ( -0.1837270341207343505, -0.6046776061558807314, 0.2411417322834647770 ) ) ;
#24091 = CARTESIAN_POINT ( 'NONE',  ( -1.312335958005248715, 0.2306618581243848609, 0.2411417322834645549 ) ) ;
#24092 = VECTOR ( 'NONE', #5371, 39.37007874015748854 ) ;
#24093 = CARTESIAN_POINT ( 'NONE',  ( 0.7217847769028878924, -0.4281496062992127816, -0.4176697321401328100 ) ) ;
#24094 = CARTESIAN_POINT ( 'NONE',  ( 0.2952755905511819101, 0.1660481256975883668, -0.3530559997133364547 ) ) ;
#24095 = CARTESIAN_POINT ( 'NONE',  ( -0.3392501089628017219, -0.1958661417322836718, -1.554461942257217899 ) ) ;
#24096 = CARTESIAN_POINT ( 'NONE',  ( -0.6627296587926503335, -0.6692913385826771977, 0.1292274648535927661 ) ) ;
#24097 = CARTESIAN_POINT ( 'NONE',  ( 0.3018372703412079971, 0.05413385826771626580, -0.4176697321401330321 ) ) ;
#24098 = CARTESIAN_POINT ( 'NONE',  ( -0.3083989501312330295, -0.3162353388693409650, -0.4822834645669289433 ) ) ;
#24099 = CARTESIAN_POINT ( 'NONE',  ( 0.09842519685039434474, 0.07958543189024085140, 0.2665933059059887866 ) ) ;
#24100 = CARTESIAN_POINT ( 'NONE',  ( -1.646981627296586703, -0.3162353388693409650, -0.4822834645669289433 ) ) ;
#24101 = CARTESIAN_POINT ( 'NONE',  ( -0.2797625792873952855, -0.09458053269141719621, 5.851882566737991453 ) ) ;
#24102 = CARTESIAN_POINT ( 'NONE',  ( -0.2690288713910754526, 0.2952755905511810774, -0.1292274648535930714 ) ) ;
#24103 = CARTESIAN_POINT ( 'NONE',  ( 3.912791665790199769, 1.724409448818897905, -0.4359958488159719758 ) ) ;
#24104 = CARTESIAN_POINT ( 'NONE',  ( -1.646981627296586703, -0.05778040916215522460, 0.4822834645669289988 ) ) ;
#24105 = CARTESIAN_POINT ( 'NONE',  ( 0.3917322834645670104, 2.398668435337828261E-17, -2.629921259842519898 ) ) ;
#24106 = ORIENTED_EDGE ( 'NONE', *, *, #71135, .F. ) ;
#24107 = ORIENTED_EDGE ( 'NONE', *, *, #34103, .F. ) ;
#24108 = CARTESIAN_POINT ( 'NONE',  ( 0.8792650918635177559, 0.05413385826771666132, 0.4176697321401328100 ) ) ;
#24109 = CARTESIAN_POINT ( 'NONE',  ( 0.3149606299212603933, -0.1870078740157479769, 0.3641732283464567677 ) ) ;
#24111 = LINE ( 'NONE', #17821, #47810 ) ;
#24110 = CARTESIAN_POINT ( 'NONE',  ( 1.679790026246720025, 0.1283753931104748280, 0.1820866141732283561 ) ) ;
#24112 = CARTESIAN_POINT ( 'NONE',  ( -0.1958661417322836718, 0.3392501089628017219, -0.8851706036745407014 ) ) ;
#24113 = CARTESIAN_POINT ( 'NONE',  ( 0.4724409448818897572, -0.1265901696524988906, 0.1266404199475065218 ) ) ;
#24114 = B_SPLINE_CURVE_WITH_KNOTS ( 'NONE', 3,
 ( #32386, #70695, #52569, #58049, #7985, #71116, #66060 ),
 .UNSPECIFIED., .F., .F.,
 ( 4, 3, 4 ),
 ( 3.469446951953614189E-18, 0.001246230184515548971, 0.002492489877932632051 ),
 .UNSPECIFIED. ) ;
#24115 = CARTESIAN_POINT ( 'NONE',  ( -0.3949938075777409963, -7.255918531996591613E-17, 0.1988188976377952832 ) ) ;
#24116 = CARTESIAN_POINT ( 'NONE',  ( 0.3412073490813655186, 0.2306618581243848609, 0.2411417322834645549 ) ) ;
#24117 = CARTESIAN_POINT ( 'NONE',  ( -1.030183727034119867, -0.3162353388693405765, 0.4822834645669290543 ) ) ;
#24118 = CARTESIAN_POINT ( 'NONE',  ( -1.154855643044618851, -0.6046776061558809534, -0.2411417322834644161 ) ) ;
#24119 = CARTESIAN_POINT ( 'NONE',  ( 0.8530183727034126306, 0.05413385826771626580, -0.4176697321401330321 ) ) ;
#24120 = CARTESIAN_POINT ( 'NONE',  ( 0.8858267716535438430, -0.5400638737290845981, -0.3530559997133363437 ) ) ;
#24121 = CARTESIAN_POINT ( 'NONE',  ( 1.417322834645670104, -0.1870078740157480601, -0.3641732283464567677 ) ) ;
#24122 = CARTESIAN_POINT ( 'NONE',  ( 1.056430446194226658, 0.1771653543307087630, 0.09757992244046791164 ) ) ;
#24123 = CARTESIAN_POINT ( 'NONE',  ( -0.8727034120734901146, -0.3162353388693405765, 0.4822834645669290543 ) ) ;
#24124 = CARTESIAN_POINT ( 'NONE',  ( -0.1998031496062991630, -0.3460692066303959202, -0.6148293963254594097 ) ) ;
#24125 = CARTESIAN_POINT ( 'NONE',  ( 1.686351706036745890, 0.2952755905511811885, 0.1292274648535926551 ) ) ;
#24126 = CARTESIAN_POINT ( 'NONE',  ( -0.2867679344610364334, -0.2867679344610367109, -0.2086614173228345248 ) ) ;
#24127 = CARTESIAN_POINT ( 'NONE',  ( -0.1574803149606292529, -0.1870078740157480879, -0.4822834645669291653 ) ) ;
#24129 = CARTESIAN_POINT ( 'NONE',  ( -3.908320185825791881, 1.553306296213791793, -0.4744094488188976277 ) ) ;
#24128 = CARTESIAN_POINT ( 'NONE',  ( 1.266404199475066328, -0.3162353388693409650, -0.4822834645669289433 ) ) ;
#24130 = CARTESIAN_POINT ( 'NONE',  ( 0.000000000000000000, 0.000000000000000000, 6.062992125984251857 ) ) ;
#24131 = CARTESIAN_POINT ( 'NONE',  ( 0.4330708661417329575, 0.2952755905511811885, 0.000000000000000000 ) ) ;
#24132 = CARTESIAN_POINT ( 'NONE',  ( 1.069553805774278610, -0.5511811023622046335, 0.09757992244046803654 ) ) ;
#24133 = CARTESIAN_POINT ( 'NONE',  ( -0.3917322834645670659, 0.1049643490035301607, -1.845125041173541369 ) ) ;
#24134 = CARTESIAN_POINT ( 'NONE',  ( -1.167979002624671470, -0.3690944881889765550, -0.3153832671262227771 ) ) ;
#24135 = CARTESIAN_POINT ( 'NONE',  ( 1.069553805774278832, 0.2952755905511810774, -0.1292274648535930714 ) ) ;
#24136 = CARTESIAN_POINT ( 'NONE',  ( 0.000000000000000000, 2.755905511811024056, 0.000000000000000000 ) ) ;
#24137 = CARTESIAN_POINT ( 'NONE',  ( -0.5905511811023615998, 0.1771653543307087630, 0.000000000000000000 ) ) ;
#24138 = CARTESIAN_POINT ( 'NONE',  ( -0.4593175853018366950, 0.05413385826771666132, 0.4176697321401328100 ) ) ;
#24139 = CARTESIAN_POINT ( 'NONE',  ( -1.305774278215222184, 0.1771653543307087630, 0.09757992244046791164 ) ) ;
#24140 = CARTESIAN_POINT ( 'NONE',  ( -0.7020997375328076329, -0.3162353388693409650, -0.4822834645669289433 ) ) ;
#24141 = CARTESIAN_POINT ( 'NONE',  ( 1.535433070866142558, 0.2952755905511811885, 0.000000000000000000 ) ) ;
#24142 = CARTESIAN_POINT ( 'NONE',  ( -9.594673741351313045E-17, 0.3917322834645670659, -0.7841400506899758316 ) ) ;
#24143 = CARTESIAN_POINT ( 'NONE',  ( -1.095800524934382292, -0.2845877964562161244, -0.3641732283464567121 ) ) ;
#24144 = EDGE_CURVE ( 'NONE', #28368, #43450, #74455, .T. ) ;
#24145 = CARTESIAN_POINT ( 'NONE',  ( 1.120717929797273582, 1.066111340139089814, 0.06270518838489094748 ) ) ;
#24146 = CARTESIAN_POINT ( 'NONE',  ( 1.496062992125984703, -0.1870078740157480879, -0.4822834645669291653 ) ) ;
#24147 = CARTESIAN_POINT ( 'NONE',  ( -0.3458507752293906723, -0.3458507752293910609, -1.868110236220472453 ) ) ;
#24148 = CARTESIAN_POINT ( 'NONE',  ( -1.161417322834644716, -0.5400638737290845981, -0.3530559997133363437 ) ) ;
#24149 = CARTESIAN_POINT ( 'NONE',  ( -1.391076115485563314, -0.5023911411419708095, -0.1820866141732282451 ) ) ;
#24150 = CARTESIAN_POINT ( 'NONE',  ( -0.4790026246719154557, -0.2845877964562159024, 0.3641732283464567677 ) ) ;
#24151 = DIRECTION ( 'NONE',  ( -0.000000000000000000, 1.000000000000000000, -0.000000000000000000 ) ) ;
#24152 = CARTESIAN_POINT ( 'NONE',  ( -0.4527559055118102749, -0.5400638737290845981, -0.3530559997133363437 ) ) ;
#24153 = CARTESIAN_POINT ( 'NONE',  ( 0.01312335958005323398, -0.3690944881889765550, -0.3153832671262227771 ) ) ;
#24154 = CARTESIAN_POINT ( 'NONE',  ( -1.332020997375327642, -0.2845877964562161244, -0.3641732283464567121 ) ) ;
#24155 = CARTESIAN_POINT ( 'NONE',  ( -1.345144356955379816, -0.05778040916215560624, -0.4822834645669293319 ) ) ;
#24156 = CARTESIAN_POINT ( 'NONE',  ( 1.338582677165355062, -0.1870078740157480601, -0.3641732283464567677 ) ) ;
#24157 = EDGE_CURVE ( 'NONE', #38268, #66982, #34174, .T. ) ;
#24158 = CARTESIAN_POINT ( 'NONE',  ( 0.9908136482939640111, -0.6692913385826771977, 0.1292274648535927661 ) ) ;
#24159 = CARTESIAN_POINT ( 'NONE',  ( 0.4744094488188900782, 1.537401574803149984, 2.170146923806596906 ) ) ;
#24160 = CARTESIAN_POINT ( 'NONE',  ( 0.4396325459317593221, 0.1771653543307087075, -0.09757992244046823083 ) ) ;
#24161 = CARTESIAN_POINT ( 'NONE',  ( 0.3083989501312343062, -0.05778040916215560624, -0.4822834645669293319 ) ) ;
#24162 = CARTESIAN_POINT ( 'NONE',  ( 0.8267716535433077274, 0.1771653543307087630, 0.000000000000000000 ) ) ;
#24163 = ORIENTED_EDGE ( 'NONE', *, *, #55359, .T. ) ;
#24164 = CARTESIAN_POINT ( 'NONE',  ( -1.023622047244093558, -0.1870078740157479769, 0.4822834645669291653 ) ) ;
#24165 = CARTESIAN_POINT ( 'NONE',  ( -0.8267716535433065062, 0.2952755905511811885, 0.000000000000000000 ) ) ;
#24166 = CARTESIAN_POINT ( 'NONE',  ( 0.08530183727034192087, -0.3162353388693409650, -0.4822834645669289433 ) ) ;
#24167 = CARTESIAN_POINT ( 'NONE',  ( -0.1998031496062991907, -0.3460692066303959757, -0.06561679790026248016 ) ) ;
#24168 = CARTESIAN_POINT ( 'NONE',  ( 0.3996062992125986035, -0.1070741851644052972, -2.550524934383202158 ) ) ;
#24169 = CARTESIAN_POINT ( 'NONE',  ( 0.6102362204724416372, -0.5400638737290844871, 0.3530559997133364547 ) ) ;
#24170 = CARTESIAN_POINT ( 'NONE',  ( 1.515748031496063186, -0.4536011799217368745, -0.2665933059059886201 ) ) ;
#24171 = CARTESIAN_POINT ( 'NONE',  ( 0.1181102362204730916, 0.2952755905511811885, 0.000000000000000000 ) ) ;
#24172 = CARTESIAN_POINT ( 'NONE',  ( 0.8792650918635177559, -0.4281496062992127816, -0.4176697321401328100 ) ) ;
#24173 = CARTESIAN_POINT ( 'NONE',  ( 0.3996062992125986035, 0.1070741851644054776, -2.014435695538057569 ) ) ;
#24174 = CARTESIAN_POINT ( 'NONE',  ( 0.3420746716998660508, -0.1974969037888703871, -1.364829396325459410 ) ) ;
#24175 = CARTESIAN_POINT ( 'NONE',  ( 0.2925321140481932369, -0.2925321140481932369, -2.775590551181101429 ) ) ;
#24176 = CYLINDRICAL_SURFACE ( 'NONE', #49293, 0.3149606299212598381 ) ;
#24177 = CARTESIAN_POINT ( 'NONE',  ( -0.3392501089628019995, 0.1958661417322832277, -0.8057742782152230721 ) ) ;
#24178 = CARTESIAN_POINT ( 'NONE',  ( -0.4527559055118102749, 0.07958543189024085140, 0.2665933059059887866 ) ) ;
#24179 = CARTESIAN_POINT ( 'NONE',  ( -0.9383202099737524282, -0.05778040916215522460, 0.4822834645669289988 ) ) ;
#24180 = CARTESIAN_POINT ( 'NONE',  ( 0.4396325459317590445, -0.6692913385826771977, 0.1292274648535927661 ) ) ;
#24181 = CARTESIAN_POINT ( 'NONE',  ( -9.674558042662122972E-17, 0.3949938075777409963, -2.753937007874016185 ) ) ;
#24182 = CARTESIAN_POINT ( 'NONE',  ( 0.8923884514435703741, 0.2306618581243848609, 0.2411417322834645549 ) ) ;
#24183 = CARTESIAN_POINT ( 'NONE',  ( -1.561679790026246017, -0.4281496062992127816, -0.4176697321401328100 ) ) ;
#24184 = CARTESIAN_POINT ( 'NONE',  ( 0.6036745406824153282, -0.6046776061558807314, 0.2411417322834647770 ) ) ;
#24185 = CARTESIAN_POINT ( 'NONE',  ( 5.785732909357575061E-17, -0.4724409448818898682, -2.598425196850393970 ) ) ;
#24186 = CARTESIAN_POINT ( 'NONE',  ( 0.2925321140481932369, -0.2925321140481932369, -2.303149606299212060 ) ) ;
#24187 = DIRECTION ( 'NONE',  ( 0.000000000000000000, 0.000000000000000000, -1.000000000000000000 ) ) ;
#24188 = CARTESIAN_POINT ( 'NONE',  ( 0.8464566929133865436, 0.1660481256975883668, -0.3530559997133364547 ) ) ;
#24189 = CARTESIAN_POINT ( 'NONE',  ( 0.7939632545931766261, -0.05778040916215522460, 0.4822834645669289988 ) ) ;
#24190 = CARTESIAN_POINT ( 'NONE',  ( 1.076115485564305141, -0.5023911411419708095, 0.1820866141732285504 ) ) ;
#24192 = CARTESIAN_POINT ( 'NONE',  ( 1.601049868766404982, 0.2306618581243848609, 0.2411417322834645549 ) ) ;
#24191 = CARTESIAN_POINT ( 'NONE',  ( 1.587926509186352586, -0.4281496062992127816, -0.4176697321401328100 ) ) ;
#24193 = CARTESIAN_POINT ( 'NONE',  ( 0.1049643490035303689, 0.3917322834645668994, -2.750636852197163584 ) ) ;
#24194 = CARTESIAN_POINT ( 'NONE',  ( 0.8727034120734913358, -0.05778040916215522460, 0.4822834645669289988 ) ) ;
#24195 = CARTESIAN_POINT ( 'NONE',  ( 1.509186351706037543, -0.004921259842519576551, 0.3153832671262227771 ) ) ;
#24196 = CARTESIAN_POINT ( 'NONE',  ( -0.4724409448818890911, -0.1870078740157479769, 0.4822834645669291653 ) ) ;
#24197 = CARTESIAN_POINT ( 'NONE',  ( -0.8005249343832013809, -0.4281496062992124485, 0.4176697321401328655 ) ) ;
#24198 = CARTESIAN_POINT ( 'NONE',  ( -1.541994750656167090, -0.6692913385826773087, -0.1292274648535924053 ) ) ;
#24199 = CARTESIAN_POINT ( 'NONE',  ( -0.3917322834645669549, -0.1049643490035306603, -0.6030183727034120755 ) ) ;
#24200 = CARTESIAN_POINT ( 'NONE',  ( 0.3392501089628018884, -0.1958661417322834220, -1.356955380577427928 ) ) ;
#24201 = CARTESIAN_POINT ( 'NONE',  ( -0.2867679344610364334, -0.2867679344610367109, -2.413385826771653253 ) ) ;
#24202 = CARTESIAN_POINT ( 'NONE',  ( -1.640419947506561060, -0.004921259842519576551, 0.3153832671262227771 ) ) ;
#24203 = VERTEX_POINT ( 'NONE', #52680 ) ;
#24204 = CARTESIAN_POINT ( 'NONE',  ( 0.3949938075777411073, -0.1058382717557499464, -2.631233595800525293 ) ) ;
#24205 = VERTEX_POINT ( 'NONE', #7681 ) ;
#24206 = DIRECTION ( 'NONE',  ( 0.000000000000000000, 0.000000000000000000, -1.000000000000000000 ) ) ;
#24207 = CARTESIAN_POINT ( 'NONE',  ( 1.332020997375328974, -0.08942795157528024563, -0.3641732283464568787 ) ) ;
#24208 = CARTESIAN_POINT ( 'NONE',  ( 4.893765752498283924E-17, -0.3996062992125986035, -1.653543307086614123 ) ) ;
#24209 = CARTESIAN_POINT ( 'NONE',  ( 0.03757601356357168076, -0.4709442531824368783, -4.620136098463503353E-16 ) ) ;
#24210 = CARTESIAN_POINT ( 'NONE',  ( 3.908320185825791881, 1.537401574803149984, 0.4744094488188975722 ) ) ;
#24211 = CARTESIAN_POINT ( 'NONE',  ( 0.000000000000000000, 0.000000000000000000, -2.755905511811024056 ) ) ;
#24212 = CARTESIAN_POINT ( 'NONE',  ( -0.3130349471939997685, 1.559138852304699174, 0.003046472099445048272 ) ) ;
#24213 = CARTESIAN_POINT ( 'NONE',  ( 0.3392501089628018329, 0.1958661417322835607, -0.3733595800524935338 ) ) ;
#24214 = CARTESIAN_POINT ( 'NONE',  ( -0.8792650918635160906, -0.3690944881889763329, 0.3153832671262228327 ) ) ;
#24215 = CARTESIAN_POINT ( 'NONE',  ( -1.358267716535432434, 0.07958543189024071263, -0.2665933059059888421 ) ) ;
#24216 = CARTESIAN_POINT ( 'NONE',  ( -1.332020997375327642, -0.05778040916215522460, 0.4822834645669289988 ) ) ;
#24217 = CARTESIAN_POINT ( 'NONE',  ( 0.02624671916010564918, 0.2306618581243848609, 0.2411417322834645549 ) ) ;
#24218 = CARTESIAN_POINT ( 'NONE',  ( -1.286089238845143479, 0.2306618581243847221, -0.2411417322834647770 ) ) ;
#24219 = CARTESIAN_POINT ( 'NONE',  ( -0.3917322834645670104, -7.196005306013484475E-17, -0.1889763779527558474 ) ) ;
#24220 = ORIENTED_EDGE ( 'NONE', *, *, #60997, .F. ) ;
#24221 = CARTESIAN_POINT ( 'NONE',  ( 1.607611548556431069, 0.2952755905511811885, 0.1292274648535926551 ) ) ;
#24222 = CARTESIAN_POINT ( 'NONE',  ( -1.135170603674539924, 0.2066929133858267098, -0.1054918080437494132 ) ) ;
#24223 =( NAMED_UNIT ( * ) SI_UNIT ( $, .STERADIAN. ) SOLID_ANGLE_UNIT ( ) );
#24224 = CARTESIAN_POINT ( 'NONE',  ( 0.4724409448818897572, -0.1265901696524988906, -1.843832020997375309 ) ) ;
#24225 = CARTESIAN_POINT ( 'NONE',  ( 2.165487897237717174, 1.580736828574223374, 0.4725026149319441759 ) ) ;
#24226 = CARTESIAN_POINT ( 'NONE',  ( -0.3543307086614165824, 0.1771653543307087630, 0.000000000000000000 ) ) ;
#24227 = CARTESIAN_POINT ( 'NONE',  ( -0.9711286089238838626, 0.2306618581243847221, -0.2411417322834647770 ) ) ;
#24228 = CARTESIAN_POINT ( 'NONE',  ( 0.9580052493438327987, -0.4281496062992127816, -0.4176697321401328100 ) ) ;
#24229 = ORIENTED_EDGE ( 'NONE', *, *, #52610, .F. ) ;
#24231 = CARTESIAN_POINT ( 'NONE',  ( -1.614173228346457378, 1.606230626554505658, 0.1372047244094476981 ) ) ;
#24230 = CARTESIAN_POINT ( 'NONE',  ( 1.220472440944882386, 0.000000000000000000, -0.4445507791589061175 ) ) ;
#24232 = CARTESIAN_POINT ( 'NONE',  ( 1.640419947506562393, -0.4281496062992124485, 0.4176697321401328655 ) ) ;
#24233 = CARTESIAN_POINT ( 'NONE',  ( -1.049868766404198794, 0.2306618581243847221, -0.2411417322834647770 ) ) ;
#24234 = CARTESIAN_POINT ( 'NONE',  ( -0.1049643490035301746, -0.3917322834645670659, -0.3096919703073997554 ) ) ;
#24235 = CARTESIAN_POINT ( 'NONE',  ( -0.09842519685039295696, 0.07958543189024071263, -0.2665933059059888421 ) ) ;
#24236 = CARTESIAN_POINT ( 'NONE',  ( 0.2867679344610366554, -0.2867679344610365444, -0.6555118110236221041 ) ) ;
#24237 = CARTESIAN_POINT ( 'NONE',  ( -0.05249343832020911260, 0.1283753931104748280, 0.1820866141732283561 ) ) ;
#24238 = CARTESIAN_POINT ( 'NONE',  ( 0.4790026246719167324, -0.08942795157527998196, 0.3641732283464567121 ) ) ;
#24239 = CARTESIAN_POINT ( 'NONE',  ( 0.5380577427821529035, 0.05413385826771626580, -0.4176697321401330321 ) ) ;
#24240 = CARTESIAN_POINT ( 'NONE',  ( -0.6692913385826764205, 0.1771653543307087630, 0.000000000000000000 ) ) ;
#24241 = CARTESIAN_POINT ( 'NONE',  ( -0.3392501089628019995, 0.1958661417322832277, -2.380577427821522374 ) ) ;
#24242 = CARTESIAN_POINT ( 'NONE',  ( 1.207349081364829990, -0.6046776061558809534, -0.2411417322834644161 ) ) ;
#24243 = CARTESIAN_POINT ( 'NONE',  ( -1.095800524934382292, -0.3162353388693409650, -0.4822834645669289433 ) ) ;
#24244 = CARTESIAN_POINT ( 'NONE',  ( 0.2362204724409449064, 0.4091458600556404646, -0.8510498687664042050 ) ) ;
#24245 = CARTESIAN_POINT ( 'NONE',  ( 0.01312335958005323398, 0.05413385826771666132, 0.4176697321401328100 ) ) ;
#24246 = CARTESIAN_POINT ( 'NONE',  ( -0.4527559055118102749, -0.5400638737290845981, -0.3530559997133363437 ) ) ;
#24247 = CARTESIAN_POINT ( 'NONE',  ( 1.437007874015748810, -0.4536011799217368745, -0.2665933059059886201 ) ) ;
#24248 = CARTESIAN_POINT ( 'NONE',  ( 0.05905511811023681640, 0.07958543189024071263, -0.2665933059059888421 ) ) ;
#24249 = CARTESIAN_POINT ( 'NONE',  ( -0.3280839895013117347, -0.4281496062992124485, 0.4176697321401328655 ) ) ;
#24250 = CARTESIAN_POINT ( 'NONE',  ( -1.069553805774277722, -0.6692913385826773087, -0.1292274648535924053 ) ) ;
#24251 = CARTESIAN_POINT ( 'NONE',  ( -0.5944687039322197331, 1.968503937007873850, -0.4915354330708654462 ) ) ;
#24252 = CARTESIAN_POINT ( 'NONE',  ( 1.686351706036745890, 0.1771653543307087630, 0.09757992244046791164 ) ) ;
#24253 = CARTESIAN_POINT ( 'NONE',  ( -0.4002624671916004129, -0.3162353388693405765, 0.4822834645669290543 ) ) ;
#24254 = ORIENTED_EDGE ( 'NONE', *, *, #4102, .F. ) ;
#24255 = B_SPLINE_CURVE_WITH_KNOTS ( 'NONE', 3,
 ( #75633, #17971, #69310, #11660 ),
 .UNSPECIFIED., .F., .F.,
 ( 4, 4 ),
 ( 0.000000000000000000, 0.0007402370886711635454 ),
 .UNSPECIFIED. ) ;
#24256 = CARTESIAN_POINT ( 'NONE',  ( 0.1998031496062994128, -0.3460692066303957537, -2.058398950131233640 ) ) ;
#24257 = CARTESIAN_POINT ( 'NONE',  ( 1.102362204724410155, -0.1870078740157479769, 0.4822834645669291653 ) ) ;
#24258 = CARTESIAN_POINT ( 'NONE',  ( -0.6102362204724400829, 0.07958543189024085140, 0.2665933059059887866 ) ) ;
#24259 = CARTESIAN_POINT ( 'NONE',  ( -0.4133858267716528645, 0.1660481256975883668, -0.3530559997133364547 ) ) ;
#24260 = CARTESIAN_POINT ( 'NONE',  ( 1.423884514435696413, -0.3162353388693409650, -0.4822834645669289433 ) ) ;
#24261 = CARTESIAN_POINT ( 'NONE',  ( 0.8858267716535438430, 0.1660481256975885056, 0.3530559997133364547 ) ) ;
#24262 = DIRECTION ( 'NONE',  ( 1.000000000000000000, 0.000000000000000000, 0.000000000000000000 ) ) ;
#24263 = CARTESIAN_POINT ( 'NONE',  ( -1.141732283464566011, -0.5511811023622047445, 6.969142054262312111E-17 ) ) ;
#24264 = CARTESIAN_POINT ( 'NONE',  ( 0.3996062992125985480, -0.1070741851644052972, -0.8182414698162728817 ) ) ;
#24265 = CARTESIAN_POINT ( 'NONE',  ( -0.1998031496062991907, -0.3460692066303959757, -1.010498687664042050 ) ) ;
#24266 = CARTESIAN_POINT ( 'NONE',  ( 4.837279021331060870E-17, -0.3949938075777409963, -0.3937007874015748810 ) ) ;
#24267 = CARTESIAN_POINT ( 'NONE',  ( 0.3257991949422233136, 1.192497134494935995, -1.407652438512451587 ) ) ;
#24268 = CARTESIAN_POINT ( 'NONE',  ( 1.318897637795276356, -0.4536011799217367080, 0.2665933059059888421 ) ) ;
#24269 = EDGE_CURVE ( 'NONE', #4140, #19015, #30447, .T. ) ;
#24270 = CARTESIAN_POINT ( 'NONE',  ( 0.8530183727034126306, -0.004921259842519870586, -0.3153832671262229437 ) ) ;
#24271 = CIRCLE ( 'NONE', #28313, 1.889763779527559251 ) ;
#24272 = CARTESIAN_POINT ( 'NONE',  ( 0.6299212598425204535, -0.1870078740157479769, 0.4822834645669291653 ) ) ;
#24273 = DIRECTION ( 'NONE',  ( 0.000000000000000000, -1.000000000000000000, 0.000000000000000000 ) ) ;
#24274 = CARTESIAN_POINT ( 'NONE',  ( -0.1974969037888706924, 0.3420746716998658843, -1.192257217847769279 ) ) ;
#24275 = CARTESIAN_POINT ( 'NONE',  ( 0.6561679790026253567, -0.5023911411419708095, -0.1820866141732282451 ) ) ;
#24276 = CARTESIAN_POINT ( 'NONE',  ( -0.3215223097112853146, -0.05778040916215560624, -0.4822834645669293319 ) ) ;
#24277 = CARTESIAN_POINT ( 'NONE',  ( -0.8070866141732276899, 0.1660481256975883668, -0.3530559997133364547 ) ) ;
#24278 = CARTESIAN_POINT ( 'NONE',  ( 1.450131233595801428, -0.6692913385826773087, -0.1292274648535924053 ) ) ;
#24279 = CARTESIAN_POINT ( 'NONE',  ( -0.1265901696524993347, 0.4724409448818895907, -1.108923884514435798 ) ) ;
#24280 = CARTESIAN_POINT ( 'NONE',  ( 0.1998031496062992740, 0.3460692066303959757, -2.506561679790026087 ) ) ;
#24281 = CARTESIAN_POINT ( 'NONE',  ( 0.09186351706036799403, -0.3690944881889765550, -0.3153832671262227771 ) ) ;
#24282 = EDGE_LOOP ( 'NONE', ( #10961, #49739, #74414, #55790 ) ) ;
#24283 = CARTESIAN_POINT ( 'NONE',  ( -0.3392501089628017219, -0.1958661417322836995, -0.6791531740495557745 ) ) ;
#24284 = ORIENTED_EDGE ( 'NONE', *, *, #73965, .T. ) ;
#24285 = CARTESIAN_POINT ( 'NONE',  ( -0.7414698162729651543, 0.2952755905511810774, -0.1292274648535930714 ) ) ;
#24286 = CARTESIAN_POINT ( 'NONE',  ( -0.3018372703412066094, -0.4281496062992127816, -0.4176697321401328100 ) ) ;
#24287 = CARTESIAN_POINT ( 'NONE',  ( -0.3346456692913377662, 0.1660481256975883668, -0.3530559997133364547 ) ) ;
#24288 = CARTESIAN_POINT ( 'NONE',  ( 0.4068241469816281097, 0.05413385826771666132, 0.4176697321401328100 ) ) ;
#24289 = CARTESIAN_POINT ( 'NONE',  ( -0.5314960629921250401, 0.1660481256975885056, 0.3530559997133364547 ) ) ;
#24290 = CARTESIAN_POINT ( 'NONE',  ( -1.148293963254592542, 0.2952755905511811885, 0.1292274648535926551 ) ) ;
#24291 = VECTOR ( 'NONE', #66118, 39.37007874015748143 ) ;
#24292 = CARTESIAN_POINT ( 'NONE',  ( -0.6233595800524928121, -0.05778040916215522460, 0.4822834645669289988 ) ) ;
#24293 = CARTESIAN_POINT ( 'NONE',  ( 0.6167979002624678353, -0.4281496062992124485, 0.4176697321401328655 ) ) ;
#24294 = EDGE_CURVE ( 'NONE', #4976, #52467, #43284, .T. ) ;
#24295 = CARTESIAN_POINT ( 'NONE',  ( 0.2867679344610365999, 0.2867679344610365999, -0.9173228346456693272 ) ) ;
#24296 = CARTESIAN_POINT ( 'NONE',  ( -0.2099737532808391705, 0.1283753931104748280, 0.1820866141732283561 ) ) ;
#24297 = ORIENTED_EDGE ( 'NONE', *, *, #56065, .F. ) ;
#24298 = CARTESIAN_POINT ( 'NONE',  ( -0.3949938075777409963, -7.255918531996591613E-17, -1.614173228346456934 ) ) ;
#24299 = ORIENTED_EDGE ( 'NONE', *, *, #25913, .T. ) ;
#24300 = CARTESIAN_POINT ( 'NONE',  ( -1.122047244094487306, -0.4536011799217367080, 0.2665933059059888421 ) ) ;
#24301 = CARTESIAN_POINT ( 'NONE',  ( -1.135170603674539924, 0.2952755905511810774, -0.1292274648535930714 ) ) ;
#24302 = CARTESIAN_POINT ( 'NONE',  ( -0.7217847769028863381, -0.4281496062992124485, 0.4176697321401328655 ) ) ;
#24303 = CARTESIAN_POINT ( 'NONE',  ( -1.382762875929156809, 1.274900446720740321, 0.3961663554760424533 ) ) ;
#24304 = CARTESIAN_POINT ( 'NONE',  ( -0.5052493438320203589, -0.6692913385826771977, 0.1292274648535927661 ) ) ;
#24305 = CARTESIAN_POINT ( 'NONE',  ( -0.8595800524934373854, -0.3162353388693409650, -0.4822834645669289433 ) ) ;
#24306 = CARTESIAN_POINT ( 'NONE',  ( -1.601049868766403650, 0.2306618581243847221, -0.2411417322834647770 ) ) ;
#24307 = CARTESIAN_POINT ( 'NONE',  ( -0.4744094488188834169, 1.569371252656013516, -3.908320185825794990 ) ) ;
#24308 = CARTESIAN_POINT ( 'NONE',  ( 0.7217847769028878924, -0.004921259842519576551, 0.3153832671262227771 ) ) ;
#24309 = DIRECTION ( 'NONE',  ( 1.000000000000000000, -0.000000000000000000, -0.000000000000000000 ) ) ;
#24310 = CARTESIAN_POINT ( 'NONE',  ( 0.1958661417322836440, -0.3392501089628017219, -0.01902887139107619849 ) ) ;
#24311 = CARTESIAN_POINT ( 'NONE',  ( -0.05249343832020938322, -0.5023911411419708095, -0.1820866141732282451 ) ) ;
#24312 = CARTESIAN_POINT ( 'NONE',  ( -0.1706036745406816491, 0.05413385826771626580, -0.4176697321401330321 ) ) ;
#24313 = CARTESIAN_POINT ( 'NONE',  ( 3.915517305244492707, 1.299713873440154099, 0.4108643250733345909 ) ) ;
#24314 = CARTESIAN_POINT ( 'NONE',  ( 0.1312335958005257930, 0.2306618581243847221, -0.2411417322834647770 ) ) ;
#24315 = ORIENTED_EDGE ( 'NONE', *, *, #22171, .F. ) ;
#24316 = CARTESIAN_POINT ( 'NONE',  ( 0.3996062992125986035, 0.1070741851644054776, -2.171916010498687211 ) ) ;
#24317 = CARTESIAN_POINT ( 'NONE',  ( 0.1937007874015748143, -6.342658900292320455E-18, 0.000000000000000000 ) ) ;
#24318 = VERTEX_POINT ( 'NONE', #13996 ) ;
#24319 = CARTESIAN_POINT ( 'NONE',  ( 0.3996062992125984925, 0.1070741851644054637, -1.776246719160104570 ) ) ;
#24320 = CARTESIAN_POINT ( 'NONE',  ( 1.604771003085129433, 0.4514378173630678726, -0.1466069496707749775 ) ) ;
#24322 = EDGE_CURVE ( 'NONE', #76146, #820, #47328, .T. ) ;
#24321 = CARTESIAN_POINT ( 'NONE',  ( -1.069553805774277722, 0.1771653543307087630, 0.09757992244046791164 ) ) ;
#24323 = CARTESIAN_POINT ( 'NONE',  ( -1.417322834645668772, -0.1870078740157479769, 0.4822834645669291653 ) ) ;
#24324 = CARTESIAN_POINT ( 'NONE',  ( 0.2362204724409451007, -0.4091458600556402980, -0.2493438320209973857 ) ) ;
#24325 = CARTESIAN_POINT ( 'NONE',  ( 0.2017716535433070613, -0.2017716535433070890, 0.000000000000000000 ) ) ;
#24326 = CARTESIAN_POINT ( 'NONE',  ( -0.1049643490035302024, -0.3917322834645671215, 0.09317585301837273681 ) ) ;
#24327 = CARTESIAN_POINT ( 'NONE',  ( 1.502624671916010790, -0.05778040916215522460, 0.4822834645669289988 ) ) ;
#24328 = CARTESIAN_POINT ( 'NONE',  ( 0.4986876640419954376, 0.2306618581243848609, 0.2411417322834645549 ) ) ;
#24329 = CARTESIAN_POINT ( 'NONE',  ( -0.09186351706036663400, -0.4281496062992124485, 0.4176697321401328655 ) ) ;
#24330 = CARTESIAN_POINT ( 'NONE',  ( -1.167979002624671470, -0.004921259842519576551, 0.3153832671262227771 ) ) ;
#24331 = CARTESIAN_POINT ( 'NONE',  ( -0.5577427821522301654, -0.05778040916215560624, -0.4822834645669293319 ) ) ;
#24332 = CARTESIAN_POINT ( 'NONE',  ( 5.785732909357575061E-17, -0.4724409448818898682, -2.517716535433071279 ) ) ;
#24333 = CARTESIAN_POINT ( 'NONE',  ( -0.8595800524934373854, -0.3162353388693409650, -0.4822834645669289433 ) ) ;
#24334 = CARTESIAN_POINT ( 'NONE',  ( -9.674558042662122972E-17, 0.3949938075777409963, -2.124015748031495843 ) ) ;
#24335 = CARTESIAN_POINT ( 'NONE',  ( 1.312335958005249825, 0.1283753931104746893, -0.1820866141732285504 ) ) ;
#24336 = CARTESIAN_POINT ( 'NONE',  ( -0.5118110236220466680, -0.5511811023622047445, 6.969142054262312111E-17 ) ) ;
#24337 = CARTESIAN_POINT ( 'NONE',  ( 1.023622047244095334, -0.1870078740157479769, 0.3641732283464567677 ) ) ;
#24338 = CARTESIAN_POINT ( 'NONE',  ( -1.496062992125983815, -0.1870078740157480879, -0.4822834645669291653 ) ) ;
#24339 = AXIS2_PLACEMENT_3D ( 'NONE', #76558, #32762, #791 ) ;
#24340 = CARTESIAN_POINT ( 'NONE',  ( -1.076115485564303809, -0.5023911411419708095, -0.1820866141732282451 ) ) ;
#24341 = CARTESIAN_POINT ( 'NONE',  ( 0.000000000000000000, 2.145669291338582418, 0.000000000000000000 ) ) ;
#24342 = CARTESIAN_POINT ( 'NONE',  ( 0.3937007874015754361, -0.1870078740157479769, 0.3641732283464567677 ) ) ;
#24343 = CARTESIAN_POINT ( 'NONE',  ( -0.4199475065616791736, -0.6046776061558807314, 0.2411417322834647770 ) ) ;
#24344 = CARTESIAN_POINT ( 'NONE',  ( -1.857147851633406788, 1.070284760220074460, 0.08454815954501419817 ) ) ;
#24345 = CARTESIAN_POINT ( 'NONE',  ( 0.03937007874015833325, -0.5511811023622047445, 6.969142054262312111E-17 ) ) ;
#24346 = CARTESIAN_POINT ( 'NONE',  ( -1.528871391076114250, 0.1771653543307087075, -0.09757992244046823083 ) ) ;
#24347 = CARTESIAN_POINT ( 'NONE',  ( 0.6364829396325465405, -0.3162353388693409650, -0.4822834645669289433 ) ) ;
#24348 = CARTESIAN_POINT ( 'NONE',  ( 0.000000000000000000, 0.000000000000000000, -2.755905511811024056 ) ) ;
#24349 = CARTESIAN_POINT ( 'NONE',  ( 1.246719160104987623, -0.3690944881889763329, 0.3153832671262228327 ) ) ;
#24350 = CARTESIAN_POINT ( 'NONE',  ( -1.148293963254592542, -0.6692913385826773087, -0.1292274648535924053 ) ) ;
#24351 = CARTESIAN_POINT ( 'NONE',  ( -0.2952755905511803003, -0.4536011799217368745, -0.2665933059059886201 ) ) ;
#24352 = DIRECTION ( 'NONE',  ( 0.000000000000000000, -1.000000000000000000, 0.000000000000000000 ) ) ;
#24353 = CARTESIAN_POINT ( 'NONE',  ( 0.3149606299212603933, -0.1870078740157479769, 0.3641732283464567677 ) ) ;
#24354 = VECTOR ( 'NONE', #14429, 39.37007874015748143 ) ;
#24355 = CARTESIAN_POINT ( 'NONE',  ( -1.128608923884513837, -0.6046776061558807314, 0.2411417322834647770 ) ) ;
#24356 = CARTESIAN_POINT ( 'NONE',  ( -0.5249343832020990641, 0.2306618581243848609, 0.2411417322834645549 ) ) ;
#24357 = CARTESIAN_POINT ( 'NONE',  ( 0.1070741851644053388, 0.3996062992125986035, -0.7001312335958002064 ) ) ;
#24358 = CARTESIAN_POINT ( 'NONE',  ( -0.1049643490035307020, 0.3917322834645669549, -2.138451443569553412 ) ) ;
#24359 = CARTESIAN_POINT ( 'NONE',  ( 0.7349081364829402885, -0.5023911411419708095, -0.1820866141732282451 ) ) ;
#24360 = CARTESIAN_POINT ( 'NONE',  ( -0.4002624671916004129, -0.3162353388693405765, 0.4822834645669290543 ) ) ;
#24361 = CARTESIAN_POINT ( 'NONE',  ( -0.5118110236220466680, 0.2952755905511811885, 0.000000000000000000 ) ) ;
#24362 = CARTESIAN_POINT ( 'NONE',  ( -0.9645669291338575535, 0.07958543189024071263, -0.2665933059059888421 ) ) ;
#24363 = CARTESIAN_POINT ( 'NONE',  ( -3.920816016192138154, 1.224393450447388343, 0.3568336507794432899 ) ) ;
#24364 = CARTESIAN_POINT ( 'NONE',  ( 0.1377952755905518800, 0.1660481256975883668, -0.3530559997133364547 ) ) ;
#24365 = CARTESIAN_POINT ( 'NONE',  ( -1.299212598425196097, -0.5511811023622047445, 6.969142054262312111E-17 ) ) ;
#24366 = CARTESIAN_POINT ( 'NONE',  ( -1.561679790026246017, -0.4281496062992127816, -0.4176697321401328100 ) ) ;
#24367 = CARTESIAN_POINT ( 'NONE',  ( -1.157146581871515012E-16, 0.4724409448818898682, -2.596456692913385655 ) ) ;
#24368 = VERTEX_POINT ( 'NONE', #39653 ) ;
#24369 = EDGE_CURVE ( 'NONE', #26176, #41893, #10232, .T. ) ;
#24370 = CARTESIAN_POINT ( 'NONE',  ( -1.660104986876639543, -0.08942795157528024563, -0.3641732283464568787 ) ) ;
#24371 = CARTESIAN_POINT ( 'NONE',  ( -1.207349081364828880, 0.2306618581243847221, -0.2411417322834647770 ) ) ;
#24372 = CARTESIAN_POINT ( 'NONE',  ( -0.6692913385826764205, -0.6692913385826771977, 8.415575281601705876E-17 ) ) ;
#24373 = CARTESIAN_POINT ( 'NONE',  ( 1.594488188976378673, 0.1660481256975885056, 0.3530559997133364547 ) ) ;
#24374 = CARTESIAN_POINT ( 'NONE',  ( 0.3392501089628018884, -0.1958661417322834220, -1.606955380577427928 ) ) ;
#24375 = CARTESIAN_POINT ( 'NONE',  ( -0.3204081651523081331, 0.2263583204867674892, -1.220472440944882164 ) ) ;
#24376 = CARTESIAN_POINT ( 'NONE',  ( 0.9448818897637802916, -0.1870078740157480879, -0.4822834645669291653 ) ) ;
#24377 = CARTESIAN_POINT ( 'NONE',  ( 0.5577427821522316087, -0.05778040916215522460, 0.4822834645669289988 ) ) ;
#24378 = CARTESIAN_POINT ( 'NONE',  ( -0.2952755905511810774, 3.616083068348483797E-17, -1.929133858267716661 ) ) ;
#24379 = CARTESIAN_POINT ( 'NONE',  ( -0.3996062992125984925, -0.1070741851644056719, -2.484908136482939955 ) ) ;
#24380 = CARTESIAN_POINT ( 'NONE',  ( 1.318897637795276356, 0.07958543189024071263, -0.2665933059059888421 ) ) ;
#24381 = CARTESIAN_POINT ( 'NONE',  ( 0.3996062992125986035, 2.446882876249141962E-17, -0.9055118110236221041 ) ) ;
#24382 = ORIENTED_EDGE ( 'NONE', *, *, #57238, .T. ) ;
#24383 = CARTESIAN_POINT ( 'NONE',  ( -0.9711286089238838626, 0.1283753931104746893, -0.1820866141732285504 ) ) ;
#24384 = CARTESIAN_POINT ( 'NONE',  ( -0.1049643490035307020, 0.3917322834645669549, -2.518372703412073754 ) ) ;
#24385 = VERTEX_POINT ( 'NONE', #45947 ) ;
#24386 = CARTESIAN_POINT ( 'NONE',  ( 0.5905511811023629321, -0.6692913385826771977, 8.415575281601705876E-17 ) ) ;
#24387 = CARTESIAN_POINT ( 'NONE',  ( -0.6561679790026240244, -0.6046776061558807314, 0.2411417322834647770 ) ) ;
#24388 = CARTESIAN_POINT ( 'NONE',  ( -1.364829396325458521, -0.6046776061558807314, 0.2411417322834647770 ) ) ;
#24389 = CARTESIAN_POINT ( 'NONE',  ( 1.259842519685040019, -0.1870078740157480879, -0.4822834645669291653 ) ) ;
#24390 = CARTESIAN_POINT ( 'NONE',  ( -1.574803149606298192, -0.1870078740157480601, -0.3641732283464567677 ) ) ;
#24391 = FACE_OUTER_BOUND ( 'NONE', #2384, .T. ) ;
#24392 = CARTESIAN_POINT ( 'NONE',  ( -0.2230971128608915943, 0.05413385826771666132, 0.4176697321401328100 ) ) ;
#24393 = AXIS2_PLACEMENT_3D ( 'NONE', #27533, #53190, #16170 ) ;
#24394 = CARTESIAN_POINT ( 'NONE',  ( -1.240157480314959759, -0.5400638737290845981, -0.3530559997133363437 ) ) ;
#24395 = CARTESIAN_POINT ( 'NONE',  ( 1.581364829396326277, -0.05778040916215522460, 0.4822834645669289988 ) ) ;
#24396 = CARTESIAN_POINT ( 'NONE',  ( 1.430446194225722500, -0.4281496062992127816, -0.4176697321401328100 ) ) ;
#24397 = CARTESIAN_POINT ( 'NONE',  ( 0.1049643490035304938, -0.3917322834645669549, -2.689632545931758489 ) ) ;
#24398 = CARTESIAN_POINT ( 'NONE',  ( 0.6561679790026253567, -0.5023911411419708095, -0.1820866141732282451 ) ) ;
#24399 = ORIENTED_EDGE ( 'NONE', *, *, #13121, .T. ) ;
#24400 = CARTESIAN_POINT ( 'NONE',  ( -0.3420746716998659953, -0.1974969037888706647, -0.2099737532808399476 ) ) ;
#24401 = ORIENTED_EDGE ( 'NONE', *, *, #17293, .T. ) ;
#24402 = CARTESIAN_POINT ( 'NONE',  ( 0.04593175853018440641, 0.1771653543307087075, -0.09757992244046823083 ) ) ;
#24403 = CARTESIAN_POINT ( 'NONE',  ( -1.666666666666665853, 0.05413385826771626580, -0.4176697321401330321 ) ) ;
#24404 = CARTESIAN_POINT ( 'NONE',  ( 0.4265091863517067039, -0.6692913385826773087, -0.1292274648535924053 ) ) ;
#24405 = CARTESIAN_POINT ( 'NONE',  ( 0.3740157480314966754, 0.1660481256975883668, -0.3530559997133364547 ) ) ;
#24406 = CARTESIAN_POINT ( 'NONE',  ( -0.6561679790026240244, -0.6046776061558807314, 0.2411417322834647770 ) ) ;
#24407 = CARTESIAN_POINT ( 'NONE',  ( 0.1958661417322834775, 0.3392501089628018884, -1.558418265913072309 ) ) ;
#24408 = CARTESIAN_POINT ( 'NONE',  ( -1.141732283464566011, 0.2952755905511811885, 0.000000000000000000 ) ) ;
#24409 = CARTESIAN_POINT ( 'NONE',  ( 0.1958661417322834775, 0.3392501089628018884, -2.591207349081364519 ) ) ;
#24410 = CARTESIAN_POINT ( 'NONE',  ( 1.266404199475066328, -0.08942795157527998196, 0.3641732283464567121 ) ) ;
#24411 = CARTESIAN_POINT ( 'NONE',  ( -0.9645669291338575535, 0.1660481256975883668, -0.3530559997133364547 ) ) ;
#24412 = CARTESIAN_POINT ( 'NONE',  ( 0.9645669291338591078, -0.5400638737290845981, -0.3530559997133363437 ) ) ;
#24413 = CARTESIAN_POINT ( 'NONE',  ( 1.220472440944882608, 0.2952755905511811885, 0.000000000000000000 ) ) ;
#24414 = CARTESIAN_POINT ( 'NONE',  ( -0.3460692066303958092, -0.1998031496062994683, -0.9973753280839895430 ) ) ;
#24415 = CARTESIAN_POINT ( 'NONE',  ( -1.286089238845143479, -0.6046776061558807314, 0.2411417322834647770 ) ) ;
#24416 = CARTESIAN_POINT ( 'NONE',  ( 0.3996062992125986035, -0.1070741851644052972, -0.3458005249343831244 ) ) ;
#24417 = CARTESIAN_POINT ( 'NONE',  ( 0.3543307086614179147, 0.2952755905511811885, 0.000000000000000000 ) ) ;
#24418 = CARTESIAN_POINT ( 'NONE',  ( -0.3996062992125986035, -0.1070741851644056997, -2.408136482939632561 ) ) ;
#24419 = CARTESIAN_POINT ( 'NONE',  ( 0.1049643490035304938, -0.3917322834645669549, -1.744750656167979308 ) ) ;
#24420 = CARTESIAN_POINT ( 'NONE',  ( 1.666666666666667185, 0.05413385826771666132, 0.4176697321401328100 ) ) ;
#24421 = CARTESIAN_POINT ( 'NONE',  ( 0.1706036745406830368, -0.3690944881889765550, -0.3153832671262227771 ) ) ;
#24422 = CARTESIAN_POINT ( 'NONE',  ( 0.9908136482939640111, 0.2952755905511810774, -0.1292274648535930714 ) ) ;
#24423 = CARTESIAN_POINT ( 'NONE',  ( -0.4724409448818898682, -8.678599364036362592E-17, -1.061023622047243986 ) ) ;
#24424 = CARTESIAN_POINT ( 'NONE',  ( 0.6889763779527566800, -0.4536011799217367080, 0.2665933059059888421 ) ) ;
#24425 = EDGE_CURVE ( 'NONE', #4446, #74449, #3206, .T. ) ;
#24426 = CARTESIAN_POINT ( 'NONE',  ( 0.3937007874015754361, -0.1870078740157480879, -0.4822834645669291653 ) ) ;
#24427 = CARTESIAN_POINT ( 'NONE',  ( -0.1058382717557497660, -0.3949938075777411073, -1.093832020997375309 ) ) ;
#24428 = CARTESIAN_POINT ( 'NONE',  ( -0.9383202099737524282, -0.05778040916215522460, 0.4822834645669289988 ) ) ;
#24429 = CARTESIAN_POINT ( 'NONE',  ( 0.4177787735907000366, 0.3937007874015747699, -1.361336963694947944 ) ) ;
#24430 = DIMENSIONAL_EXPONENTS ( 1.000000000000000000, 0.000000000000000000, 0.000000000000000000, 0.000000000000000000, 0.000000000000000000, 0.000000000000000000, 0.000000000000000000 ) ;
#24431 = CARTESIAN_POINT ( 'NONE',  ( 0.8070866141732288002, 0.07958543189024085140, 0.2665933059059887866 ) ) ;
#24432 = EDGE_CURVE ( 'NONE', #49328, #55671, #29010, .T. ) ;
#24433 = CARTESIAN_POINT ( 'NONE',  ( 0.1678194419220257749, 2.459406111854941508E-15, 0.4281989832122456430 ) ) ;
#24434 = CARTESIAN_POINT ( 'NONE',  ( -0.3346456692913377662, -0.5400638737290844871, 0.3530559997133364547 ) ) ;
#24435 = CARTESIAN_POINT ( 'NONE',  ( 0.1509186351706045259, -0.08942795157528024563, -0.3641732283464568787 ) ) ;
#24436 = DIRECTION ( 'NONE',  ( 0.000000000000000000, 0.000000000000000000, -1.000000000000000000 ) ) ;
#24437 = CARTESIAN_POINT ( 'NONE',  ( -0.2362204724409442680, -0.1870078740157480879, -0.4822834645669291653 ) ) ;
#24438 = CARTESIAN_POINT ( 'NONE',  ( 0.5643044619422579178, -0.3690944881889765550, -0.3153832671262227771 ) ) ;
#24439 = DIRECTION ( 'NONE',  ( -0.1923134147744552103, 0.6939076129059790210, -0.6939076129060079978 ) ) ;
#24440 = CARTESIAN_POINT ( 'NONE',  ( 0.3460692066303958092, 0.1998031496062993018, -1.782808398950131323 ) ) ;
#24441 = CARTESIAN_POINT ( 'NONE',  ( 0.1902887139107617975, -0.6692913385826773087, -0.1292274648535924053 ) ) ;
#24442 = CARTESIAN_POINT ( 'NONE',  ( 1.102362204724410155, -0.1870078740157480601, -0.3641732283464567677 ) ) ;
#24443 = CARTESIAN_POINT ( 'NONE',  ( 0.3833616679418208051, -1.283732188437465593E-15, -0.4281993546915538462 ) ) ;
#24444 = CARTESIAN_POINT ( 'NONE',  ( -0.1968503937007867743, -0.5511811023622047445, 6.969142054262312111E-17 ) ) ;
#24445 = CARTESIAN_POINT ( 'NONE',  ( -0.6102362204724400829, 0.07958543189024085140, 0.2665933059059887866 ) ) ;
#24446 = CARTESIAN_POINT ( 'NONE',  ( -0.4986876640419939388, 0.2306618581243847221, -0.2411417322834647770 ) ) ;
#24447 = CARTESIAN_POINT ( 'NONE',  ( 0.2362204724409456558, -0.1870078740157480879, -0.4822834645669291653 ) ) ;
#24448 = CARTESIAN_POINT ( 'NONE',  ( 1.148293963254593875, -0.5511811023622046335, 0.09757992244046803654 ) ) ;
#24449 = CARTESIAN_POINT ( 'NONE',  ( 0.2384209555248066326, 1.126084429615796578, -1.096744324950771121 ) ) ;
#24450 = CARTESIAN_POINT ( 'NONE',  ( -1.673228346456691717, 0.1660481256975883668, -0.3530559997133364547 ) ) ;
#24451 = AXIS2_PLACEMENT_3D ( 'NONE', #23650, #3479, #42998 ) ;
#24452 = EDGE_CURVE ( 'NONE', #50774, #60402, #57278, .T. ) ;
#24453 = CARTESIAN_POINT ( 'NONE',  ( 0.6824146981627303710, -0.6046776061558807314, 0.2411417322834647770 ) ) ;
#24454 = CARTESIAN_POINT ( 'NONE',  ( -1.614173228346457378, 1.818966223839196372, 0.1372047244094476981 ) ) ;
#24455 = CARTESIAN_POINT ( 'NONE',  ( 0.09842519685039434474, -0.5400638737290845981, -0.3530559997133363437 ) ) ;
#24456 = CARTESIAN_POINT ( 'NONE',  ( -0.1049643490035307020, 0.3917322834645669549, -1.036089238845144589 ) ) ;
#24457 = CARTESIAN_POINT ( 'NONE',  ( 0.9908136482939640111, -0.6692913385826771977, 0.1292274648535927661 ) ) ;
#24458 = CARTESIAN_POINT ( 'NONE',  ( 0.5577427821522316087, -0.05778040916215522460, 0.4822834645669289988 ) ) ;
#24459 = CARTESIAN_POINT ( 'NONE',  ( -0.5314960629921172686, 2.755905511811024056, -2.503252890251017604 ) ) ;
#24460 = CARTESIAN_POINT ( 'NONE',  ( 0.4921259842519691285, -0.4536011799217368745, -0.2665933059059886201 ) ) ;
#24461 = CARTESIAN_POINT ( 'NONE',  ( 1.023622047244095334, -0.1870078740157479769, 0.4822834645669291653 ) ) ;
#24462 = ADVANCED_FACE ( 'NONE', ( #74874 ), #74809, .F. ) ;
#24463 = CARTESIAN_POINT ( 'NONE',  ( 0.1181102362204730916, -0.5511811023622047445, 6.969142054262312111E-17 ) ) ;
#24464 = CARTESIAN_POINT ( 'NONE',  ( -0.2034120734908128059, 0.2952755905511811885, 0.1292274648535926551 ) ) ;
#24465 = CARTESIAN_POINT ( 'NONE',  ( -0.6299212598425164567, 0.000000000000000000, -0.9285414500055735321 ) ) ;
#24466 = CARTESIAN_POINT ( 'NONE',  ( 0.1246719160104994284, -0.6692913385826771977, 0.1292274648535927661 ) ) ;
#24467 = CARTESIAN_POINT ( 'NONE',  ( -0.8858267716535425107, -0.5400638737290844871, 0.3530559997133364547 ) ) ;
#24468 = CARTESIAN_POINT ( 'NONE',  ( -0.2099737532808391705, -0.5023911411419708095, -0.1820866141732282451 ) ) ;
#24469 = CARTESIAN_POINT ( 'NONE',  ( 0.4068241469816279987, -0.4281496062992127816, -0.4176697321401328100 ) ) ;
#24470 = CARTESIAN_POINT ( 'NONE',  ( 0.8398950131233602345, -0.5023911411419708095, 0.1820866141732285504 ) ) ;
#24471 = CARTESIAN_POINT ( 'NONE',  ( -0.4068241469816264999, -0.4281496062992124485, 0.4176697321401328655 ) ) ;
#24472 = ADVANCED_FACE ( 'NONE', ( #55475 ), #64024, .F. ) ;
#24473 = DIRECTION ( 'NONE',  ( 0.000000000000000000, -1.000000000000000000, -0.000000000000000000 ) ) ;
#24475 = CARTESIAN_POINT ( 'NONE',  ( 1.364829396325459854, -0.6046776061558809534, -0.2411417322834644161 ) ) ;
#24474 = DIRECTION ( 'NONE',  ( 0.000000000000000000, 0.000000000000000000, 1.000000000000000000 ) ) ;
#24476 = CARTESIAN_POINT ( 'NONE',  ( 1.496062992125985147, -0.1870078740157479769, 0.4822834645669291653 ) ) ;
#24477 = CARTESIAN_POINT ( 'NONE',  ( -0.3392501089628017219, -0.1958661417322836718, -1.934383202099737575 ) ) ;
#24478 = CARTESIAN_POINT ( 'NONE',  ( -1.272965879265091305, 0.05413385826771626580, -0.4176697321401330321 ) ) ;
#24479 = CARTESIAN_POINT ( 'NONE',  ( -0.8858267716535425107, 0.1660481256975883668, -0.3530559997133364547 ) ) ;
#24480 = CARTESIAN_POINT ( 'NONE',  ( -0.1265901696524986964, -0.4724409448818899238, -0.5446194225721783244 ) ) ;
#24481 = CARTESIAN_POINT ( 'NONE',  ( 0.3420746716998660508, -0.1974969037888703871, -2.624671916010498318 ) ) ;
#24482 = VERTEX_POINT ( 'NONE', #75692 ) ;
#24483 = CARTESIAN_POINT ( 'NONE',  ( 0.5249343832021005074, -0.5023911411419708095, 0.1820866141732285504 ) ) ;
#24484 = CARTESIAN_POINT ( 'NONE',  ( 0.3392501089628018884, -0.1958661417322834220, -1.514435695538058013 ) ) ;
#24485 = CARTESIAN_POINT ( 'NONE',  ( 0.5774278215223103139, -0.6046776061558809534, -0.2411417322834644161 ) ) ;
#24486 = CARTESIAN_POINT ( 'NONE',  ( -0.4091458600556405756, 0.2362204724409446288, -2.388451443569553856 ) ) ;
#24487 = CARTESIAN_POINT ( 'NONE',  ( -0.5615202218219585983, -1.283732188437465593E-15, -0.4281993546915544568 ) ) ;
#24488 = CARTESIAN_POINT ( 'NONE',  ( -0.6102362204724400829, -0.4536011799217368745, -0.2665933059059886201 ) ) ;
#24489 = CARTESIAN_POINT ( 'NONE',  ( -1.620734908136482577, -0.5511811023622048555, -0.09757992244046775898 ) ) ;
#24490 = CARTESIAN_POINT ( 'NONE',  ( 1.030183727034121421, -0.05778040916215522460, 0.4822834645669289988 ) ) ;
#24491 = CARTESIAN_POINT ( 'NONE',  ( 1.555118110236221041, -0.4536011799217367080, 0.2665933059059888421 ) ) ;
#24492 = CARTESIAN_POINT ( 'NONE',  ( 0.1837270341207357105, -0.6046776061558809534, -0.2411417322834644161 ) ) ;
#24493 = CARTESIAN_POINT ( 'NONE',  ( -9.594673741351310580E-17, 0.3917322834645669549, -0.7099544374990010009 ) ) ;
#24494 = CARTESIAN_POINT ( 'NONE',  ( -0.2755905511811015396, -0.6692913385826771977, 8.415575281601705876E-17 ) ) ;
#24496 = CARTESIAN_POINT ( 'NONE',  ( -1.423884514435694859, -0.2845877964562159024, 0.3641732283464567677 ) ) ;
#24495 =( BOUNDED_SURFACE ( )  B_SPLINE_SURFACE ( 1, 2, ( 
 ( #72437, #72019, #15195, #14787, #46745, #59374, #58966, #73265, #66123, #14375, #33305, #45900, #27389, #40853, #8051, #40443, #53050, #78761, #8459, #47156, #27812, #13949, #53472, #72847, #66538, #57143, #58829, #25997, #46186, #19690, #39468, #82840, #7491, #39041, #761, #57976, #37800, #64726, #77359, #78204, #33160, #70617, #71883, #13389, #20534, #31482, #50830, #63886, #25162, #12972, #64307, #71044, #70197, #63477, #38629, #71462, #5812, #19267, #52495, #65154, #7065, #1186, #32313, #76532, #18860, #45348, #44508, #32734, #44920, #26837, #12552, #38211, #58401, #6224, #31900, #57561, #26422, #20116, #52075, #83252, #77782, #45763, #6641, #25575, #51240, #13809, #341, #76939, #51654, #3396, #2571, #68207, #15623, #21919, #73274, #67793, #73697, #41280, #27819, #55129, #29471, #60632, #10130, #42096, #54730, #9299, #54308, #15203, #16037, #35794, #34137, #79189, #53479, #47163, #53889, #60221, #61461, #80839, #79603, #35381, #34969, #61046, #40863, #16451, #66546, #3809, #23152, #8879, #9710, #59798, #34555, #47581, #22337, #47998, #80019, #41683, #2152, #67376, #28230, #29059, #74521, #21505, #16868, #48821, #66966, #80435, #42505, #72855, #2983, #28648, #22745, #48405, #74105, #18901, #50461, #63522, #24386, #63111, #75338, #62703, #31529, #68605, #69013, #82887, #74937, #56374, #5852, #23563, #4212, #76165, #82477, #82073, #69431, #57185, #61871, #5042, #30711, #49646, #17685, #50057, #75752, #18093, #43727, #44551, #11784, #62280, #37437, #50873, #36202, #76573, #25207, #4618, #5449, #10544, #29876, #43315, #55538, #30289, #31110, #81248, #49234, #18502, #17282, #56777, #24793, #11365, #44145, #42910, #10945, #37022, #36602, #55955, #69837, #81668, #23978, #12187, #37844, #58873, #58446, #45808, #7956, #38255, #64768, #7107, #26040, #77402, #26469, #78669, #52120, #77828, #27296, #59281, #39087, #7536, #25618, #806, #20158, #71505, #20580, #63932, #13853, #26880, #20990, #39939, #33618, #52954, #6268, #32358, #57605, #39511, #14277, #52540, #33208, #76984, #1637, #65200, #19313, #13018, #384, #65625, #51700, #71928, #1231, #38672, #78248, #64350, #70241, #19736, #58019, #45391, #46231, #12596, #71088, #31944, #83296, #51281, #13431, #44966, #70662, #6687, #32777, #66866, #27713, #2880, #80331, #80738, #8365, #66028, #59693, #66440, #72751, #74002, #67687, #8777, #47887, #47475, #73595, #53379, #28955, #79087, #48305, #10022, #21405, #22232, #72345, #47059, #34450, #9196, #60119, #15099, #40756, #67274, #2470, #46651, #9607, #14693, #55031, #34032, #35688, #34869, #40349, #28542, #16349, #2049, #41993, #15937, #35276, #60530, #28129, #41584, #54199, #3707, #61353, #79496, #53784, #60940, #29370, #21811, #73167, #15518, #41176, #79915, #3290, #54620, #22646, #82378, #4113, #4520, #37742, #68099, #48720, #4941, #81970, #63012, #30610, #18405, #74835, #17179, #62183, #24285, #31422, #30189, #55440, #74417, #23880, #56677, #57085, #55852, #63416, #24696, #49956, #44048, #17584, #23052, #5753, #56274, #61772, #75654, #81561, #69740, #10445, #50365, #17994, #16762, #42401, #36101, #11682, #5350, #62599, #29778, #43628, #31009, #49545, #76062, #81148, #69332, #43216, #37339, #23463, #12085, #42812, #49130, #68506, #10846, #36507, #75240, #68914, #11264, #36922, #13748, #77296, #18802, #50775, #699, #25935, #12911, #14172, #76475, #44447, #70139, #70984, #51180, #7426, #13328, #45288, #64250, #38154, #33516, #64664, #76878, #12491, #20474, #6584, #39405, #25515, #52431, #38981, #52016, #32255, #51594, #46128, #57502, #57916, #71822, #63826, #7003, #78142, #6165, #31840, #65088, #71400, #32671, #58337, #39830, #83193, #19627, #26356, #38569, #280, #77722, #7850, #20051, #45704, #65519, #82781, #33097, #58763, #19209, #1126, #26776, #25102, #44857, #70556, #60431, #15843, #9920, #28857, #80234, #16248, #27191, #21304, #46543, #73067, #3193, #41492, #22133, #65927, #22550, #2782, #8264, #1949, #72649, #54519, #14999, #60841, #54101, #27611, #28442, #53274, #59178, #40656, #46957, #66341, #9507, #15416, #8679, #52855, #48212, #73908, #2370, #35180 ),
 ( #41895, #78983, #79817, #60015, #47791, #40244, #67178, #33929, #67589, #1536, #59594, #34772, #78565, #34349, #28026, #47376, #41077, #21712, #66766, #20891, #9099, #53685, #73495, #72242, #14591, #79393, #50271, #4019, #68821, #75968, #43950, #42718, #54938, #29683, #4429, #82284, #69646, #75559, #81878, #55758, #35591, #62500, #75147, #18309, #30916, #68414, #61254, #11166, #3608, #29274, #48623, #61678, #80644, #10754, #62087, #36827, #56175, #11583, #16665, #17081, #22957, #74318, #42304, #17492, #4838, #17899, #43123, #56583, #55346, #81052, #74733, #30513, #68002, #36414, #10347, #36008, #30095, #69235, #23367, #81464, #49036, #37242, #24190, #24602, #23782, #49453, #49859, #43536, #62919, #5252, #76781, #59816, #82688, #40471, #38888, #63321, #11990, #5659, #604, #77626, #51495, #21523, #19529, #21112, #70459, #66149, #47182, #58237, #6490, #26260, #31326, #34155, #6071, #8486, #2171, #46772, #56991, #70044, #77199, #83099, #12816, #51921, #32160, #25007, #50680, #13239, #38473, #25419, #27837, #76378, #18712, #44353, #183, #63732, #72463, #25836, #57816, #19113, #12398, #37644, #45186, #31745, #38055, #53499, #44762, #14812, #57407, #70889, #51084, #64157, #64567, #32575, #6904, #79207, #10148, #23580, #81265, #8897, #10561, #61063, #72874, #54747, #74540, #34574, #42524, #74123, #36219, #47599, #48015, #61888, #53908, #35398, #68227, #2589, #66564, #29488, #61479, #3414, #48424, #4229, #40882, #67393, #9727, #28666, #80036, #29076, #15222, #80453, #22762, #29893, #55556, #41700, #35813, #28248, #16469, #42114, #67811, #23170, #60242, #3828, #55147, #79622, #21939, #73293, #15641, #41298, #34986, #66984, #80858, #16886, #48839, #9316, #60650, #3000, #54327, #22355, #73715, #16054, #76588, #62719, #50888, #44160, #75354, #18517, #17702, #70561, #30727, #37038, #5057, #82902, #5464, #56389, #42927, #70258, #44567, #75767, #25222, #57200, #69852, #24402, #69447, #30306, #31126, #18917, #49251, #10962, #68622, #62298, #69030, #43330, #12613, #38271, #11381, #50476, #50072, #76180, #55972, #31544, #81685, #63948, #6285, #23996, #24809, #74954, #49664, #82088, #37452, #63126, #11799, #56793, #17300, #82493, #18109, #12203, #31961, #36620, #57622, #4635, #43742, #37861, #63537, #5868, #32794, #44984, #19754, #77843, #72361, #34047, #65641, #78684, #39526, #78263, #7123, #20172, #7552, #66044, #51298, #8382, #40364, #77418, #58887, #59710, #25635, #58463, #70680, #45408, #45822, #14709, #77001, #7971, #21006, #65214, #20594, #824, #71521, #46667, #401, #26485, #19332, #6704, #13867, #13036, #38689, #64367, #33634, #14292, #33224, #1246, #32373, #58037, #26895, #52554, #64785, #52136, #46246, #26058, #71942, #39955, #51717, #71104, #59297, #1654, #13447, #27311, #52970, #39103, #35702, #53396, #3305, #42008, #36115, #55045, #23066, #42416, #79103, #47492, #72767, #15953, #29385, #67702, #48319, #8793, #48734, #28970, #34467, #28145, #15534, #80752, #41192, #3721, #80347, #53801, #54635, #79513, #2065, #66882, #73184, #9212, #61369, #41599, #34885, #21422, #74431, #16778, #28561, #68114, #10038, #22660, #60546, #22248, #66457, #67289, #10461, #27730, #47076, #15118, #40772, #21829, #2897, #60135, #2486, #54217, #74016, #79933, #16363, #47904, #73611, #9622, #35293, #60955, #68520, #37353, #4127, #10861, #49561, #49970, #75668, #24300, #18008, #12508, #43642, #30204, #69345, #11697, #63026, #12099, #29792, #5364, #18419, #61787, #31437, #82795, #18817, #55453, #23895, #49145, #31025, #5768, #44061, #24710, #36521, #25117, #56693, #62197, #4534, #75255, #57100, #17599, #63432, #82392, #55866, #50378, #81577, #81162, #43231, #68928, #11277, #37757, #76076, #36936, #23478, #50789, #76490, #4955, #44464, #69753, #70155, #62614, #81986, #42827, #74850, #17194, #30624, #56289, #57518, #51196, #57931, #64265, #65536, #59195, #295, #39422, #38997, #65106, #19224, #20490, #44874, #39846, #1554, #70573, #13765, #63843, #12927, #25951, #26374, #52033, #715, #77738, #72258, #20069, #6599, #45721, #78581, #6181, #20907, #52871, #32271, #71418, #46560, #38169, #45305 ) ),
 .UNSPECIFIED., .F., .F., .F. ) 
 B_SPLINE_SURFACE_WITH_KNOTS ( ( 2, 2 ),
 ( 3, 2, 2, 2, 2, 2, 2, 2, 2, 2, 2, 2, 2, 2, 2, 2, 2, 2, 2, 2, 2, 2, 2, 2, 2, 2, 2, 2, 2, 2, 2, 2, 2, 2, 2, 2, 2, 2, 2, 2, 2, 2, 2, 2, 2, 2, 2, 2, 2, 2, 2, 2, 2, 2, 2, 2, 2, 2, 2, 2, 2, 2, 2, 2, 2, 2, 2, 2, 2, 2, 2, 2, 2, 2, 2, 2, 2, 2, 2, 2, 2, 2, 2, 2, 2, 2, 2, 2, 2, 2, 2, 2, 2, 2, 2, 2, 2, 2, 2, 2, 2, 2, 2, 2, 2, 2, 2, 2, 2, 2, 2, 2, 2, 2, 2, 2, 2, 2, 2, 2, 2, 2, 2, 2, 2, 2, 2, 2, 2, 2, 2, 2, 2, 2, 2, 2, 2, 2, 2, 2, 2, 2, 2, 2, 2, 2, 2, 2, 2, 2, 2, 2, 2, 2, 2, 2, 2, 2, 2, 2, 2, 2, 2, 2, 2, 2, 2, 2, 2, 2, 2, 2, 2, 2, 2, 2, 2, 2, 2, 2, 2, 2, 2, 2, 2, 2, 2, 2, 2, 2, 2, 2, 2, 2, 2, 2, 2, 2, 2, 2, 2, 2, 2, 2, 2, 2, 2, 2, 2, 2, 2, 2, 2, 2, 2, 2, 2, 2, 2, 2, 2, 2, 2, 2, 2, 2, 2, 2, 2, 2, 2, 2, 2, 2, 2, 2, 2, 2, 2, 2, 2, 2, 2, 2, 2, 2, 2, 2, 2, 2, 2, 2, 2, 2, 2, 3 ),
 ( 0.000000000000000000, 1.000000000000000000 ),
 ( 0.000000000000000000, 0.003787878787878787984, 0.007575757575757575968, 0.01136363636363636395, 0.01515151515151515194, 0.01893939393939393992, 0.02272727272727272790, 0.02651515151515151589, 0.03030303030303030387, 0.03409090909090908839, 0.03787878787878787984, 0.04166666666666666435, 0.04545454545454545581, 0.04924242424242424032, 0.05303030303030303177, 0.05681818181818181629, 0.06060606060606060774, 0.06439393939393939226, 0.06818181818181817677, 0.07196969696969697516, 0.07575757575757575968, 0.07954545454545454419, 0.08333333333333332871, 0.08712121212121212710, 0.09090909090909091161, 0.09469696969696969613, 0.09848484848484848064, 0.1022727272727272790, 0.1060606060606060635, 0.1098484848484848481, 0.1136363636363636326, 0.1174242424242424310, 0.1212121212121212155, 0.1250000000000000000, 0.1287878787878787845, 0.1325757575757575690, 0.1363636363636363535, 0.1401515151515151381, 0.1439393939393939503, 0.1477272727272727348, 0.1515151515151515194, 0.1553030303030303039, 0.1590909090909090884, 0.1628787878787878729, 0.1666666666666666574, 0.1704545454545454419, 0.1742424242424242542, 0.1780303030303030387, 0.1818181818181818232, 0.1856060606060606077, 0.1893939393939393923, 0.1931818181818181768, 0.1969696969696969613, 0.2007575757575757458, 0.2045454545454545581, 0.2083333333333333426, 0.2121212121212121271, 0.2159090909090909116, 0.2196969696969696961, 0.2234848484848484806, 0.2272727272727272652, 0.2310606060606060497, 0.2348484848484848619, 0.2386363636363636465, 0.2424242424242424310, 0.2462121212121212155, 0.2500000000000000000, 0.2537878787878787845, 0.2575757575757575690, 0.2613636363636363535, 0.2651515151515151381, 0.2689393939393939226, 0.2727272727272727071, 0.2765151515151514916, 0.2803030303030302761, 0.2840909090909091161, 0.2878787878787879007, 0.2916666666666666852, 0.2954545454545454697, 0.2992424242424242542, 0.3030303030303030387, 0.3068181818181818232, 0.3106060606060606077, 0.3143939393939393923, 0.3181818181818181768, 0.3219696969696969613, 0.3257575757575757458, 0.3295454545454545303, 0.3333333333333333148, 0.3371212121212120993, 0.3409090909090908839, 0.3446969696969697239, 0.3484848484848485084, 0.3522727272727272929, 0.3560606060606060774, 0.3598484848484848619, 0.3636363636363636465, 0.3674242424242424310, 0.3712121212121212155, 0.3750000000000000000, 0.3787878787878787845, 0.3825757575757575690, 0.3863636363636363535, 0.3901515151515151381, 0.3939393939393939226, 0.3977272727272727071, 0.4015151515151514916, 0.4053030303030302761, 0.4090909090909091161, 0.4128787878787879007, 0.4166666666666666852, 0.4204545454545454697, 0.4242424242424242542, 0.4280303030303030387, 0.4318181818181818232, 0.4356060606060606077, 0.4393939393939393923, 0.4431818181818181768, 0.4469696969696969613, 0.4507575757575757458, 0.4545454545454545303, 0.4583333333333333148, 0.4621212121212120993, 0.4659090909090908839, 0.4696969696969697239, 0.4734848484848485084, 0.4772727272727272929, 0.4810606060606060774, 0.4848484848484848619, 0.4886363636363636465, 0.4924242424242424310, 0.4962121212121212155, 0.5000000000000000000, 0.5037878787878787845, 0.5075757575757575690, 0.5113636363636363535, 0.5151515151515151381, 0.5189393939393939226, 0.5227272727272727071, 0.5265151515151514916, 0.5303030303030302761, 0.5340909090909090606, 0.5378787878787878451, 0.5416666666666666297, 0.5454545454545454142, 0.5492424242424241987, 0.5530303030303029832, 0.5568181818181817677, 0.5606060606060605522, 0.5643939393939394478, 0.5681818181818182323, 0.5719696969696970168, 0.5757575757575758013, 0.5795454545454545858, 0.5833333333333333703, 0.5871212121212121549, 0.5909090909090909394, 0.5946969696969697239, 0.5984848484848485084, 0.6022727272727272929, 0.6060606060606060774, 0.6098484848484848619, 0.6136363636363636465, 0.6174242424242424310, 0.6212121212121212155, 0.6250000000000000000, 0.6287878787878787845, 0.6325757575757575690, 0.6363636363636363535, 0.6401515151515151381, 0.6439393939393939226, 0.6477272727272727071, 0.6515151515151514916, 0.6553030303030302761, 0.6590909090909090606, 0.6628787878787878451, 0.6666666666666666297, 0.6704545454545454142, 0.6742424242424241987, 0.6780303030303029832, 0.6818181818181817677, 0.6856060606060605522, 0.6893939393939394478, 0.6931818181818182323, 0.6969696969696970168, 0.7007575757575758013, 0.7045454545454545858, 0.7083333333333333703, 0.7121212121212121549, 0.7159090909090909394, 0.7196969696969697239, 0.7234848484848485084, 0.7272727272727272929, 0.7310606060606060774, 0.7348484848484848619, 0.7386363636363636465, 0.7424242424242424310, 0.7462121212121212155, 0.7500000000000000000, 0.7537878787878787845, 0.7575757575757575690, 0.7613636363636363535, 0.7651515151515151381, 0.7689393939393939226, 0.7727272727272727071, 0.7765151515151514916, 0.7803030303030302761, 0.7840909090909090606, 0.7878787878787878451, 0.7916666666666666297, 0.7954545454545454142, 0.7992424242424241987, 0.8030303030303029832, 0.8068181818181817677, 0.8106060606060605522, 0.8143939393939394478, 0.8181818181818182323, 0.8219696969696970168, 0.8257575757575758013, 0.8295454545454545858, 0.8333333333333333703, 0.8371212121212121549, 0.8409090909090909394, 0.8446969696969697239, 0.8484848484848485084, 0.8522727272727272929, 0.8560606060606060774, 0.8598484848484848619, 0.8636363636363636465, 0.8674242424242424310, 0.8712121212121212155, 0.8750000000000000000, 0.8787878787878787845, 0.8825757575757575690, 0.8863636363636363535, 0.8901515151515151381, 0.8939393939393939226, 0.8977272727272727071, 0.9015151515151514916, 0.9053030303030302761, 0.9090909090909090606, 0.9128787878787878451, 0.9166666666666666297, 0.9204545454545454142, 0.9242424242424241987, 0.9280303030303029832, 0.9318181818181817677, 0.9356060606060605522, 0.9393939393939394478, 0.9431818181818182323, 0.9469696969696970168, 0.9507575757575758013, 0.9545454545454545858, 0.9583333333333333703, 0.9621212121212121549, 0.9659090909090909394 ),
 .UNSPECIFIED. ) 
 GEOMETRIC_REPRESENTATION_ITEM ( )  RATIONAL_B_SPLINE_SURFACE ( (
 ( 1.000000000000000000, 0.9659258262890683122, 1.000000000000000000, 0.9659258262890683122, 1.000000000000000000, 0.9659258262890683122, 1.000000000000000000, 0.9659258262890683122, 1.000000000000000000, 0.9659258262890683122, 1.000000000000000000, 0.9659258262890683122, 1.000000000000000000, 0.9659258262890683122, 1.000000000000000000, 0.9659258262890683122, 1.000000000000000000, 0.9659258262890683122, 1.000000000000000000, 0.9659258262890683122, 1.000000000000000000, 0.9659258262890683122, 1.000000000000000000, 0.9659258262890683122, 1.000000000000000000, 0.9659258262890683122, 1.000000000000000000, 0.9659258262890683122, 1.000000000000000000, 0.9659258262890683122, 1.000000000000000000, 0.9659258262890683122, 1.000000000000000000, 0.9659258262890683122, 1.000000000000000000, 0.9659258262890683122, 1.000000000000000000, 0.9659258262890683122, 1.000000000000000000, 0.9659258262890683122, 1.000000000000000000, 0.9659258262890683122, 1.000000000000000000, 0.9659258262890683122, 1.000000000000000000, 0.9659258262890683122, 1.000000000000000000, 0.9659258262890683122, 1.000000000000000000, 0.9659258262890683122, 1.000000000000000000, 0.9659258262890683122, 1.000000000000000000, 0.9659258262890683122, 1.000000000000000000, 0.9659258262890683122, 1.000000000000000000, 0.9659258262890683122, 1.000000000000000000, 0.9659258262890683122, 1.000000000000000000, 0.9659258262890683122, 1.000000000000000000, 0.9659258262890683122, 1.000000000000000000, 0.9659258262890683122, 1.000000000000000000, 0.9659258262890683122, 1.000000000000000000, 0.9659258262890683122, 1.000000000000000000, 0.9659258262890683122, 1.000000000000000000, 0.9659258262890683122, 1.000000000000000000, 0.9659258262890683122, 1.000000000000000000, 0.9659258262890683122, 1.000000000000000000, 0.9659258262890683122, 1.000000000000000000, 0.9659258262890683122, 1.000000000000000000, 0.9659258262890683122, 1.000000000000000000, 0.9659258262890683122, 1.000000000000000000, 0.9659258262890683122, 1.000000000000000000, 0.9659258262890683122, 1.000000000000000000, 0.9659258262890683122, 1.000000000000000000, 0.9659258262890683122, 1.000000000000000000, 0.9659258262890683122, 1.000000000000000000, 0.9659258262890683122, 1.000000000000000000, 0.9659258262890683122, 1.000000000000000000, 0.9659258262890683122, 1.000000000000000000, 0.9659258262890683122, 1.000000000000000000, 0.9659258262890683122, 1.000000000000000000, 0.9659258262890683122, 1.000000000000000000, 0.9659258262890683122, 1.000000000000000000, 0.9659258262890683122, 1.000000000000000000, 0.9659258262890683122, 1.000000000000000000, 0.9659258262890683122, 1.000000000000000000, 0.9659258262890683122, 1.000000000000000000, 0.9659258262890683122, 1.000000000000000000, 0.9659258262890683122, 1.000000000000000000, 0.9659258262890683122, 1.000000000000000000, 0.9659258262890683122, 1.000000000000000000, 0.9659258262890683122, 1.000000000000000000, 0.9659258262890683122, 1.000000000000000000, 0.9659258262890683122, 1.000000000000000000, 0.9659258262890683122, 1.000000000000000000, 0.9659258262890683122, 1.000000000000000000, 0.9659258262890683122, 1.000000000000000000, 0.9659258262890683122, 1.000000000000000000, 0.9659258262890683122, 1.000000000000000000, 0.9659258262890683122, 1.000000000000000000, 0.9659258262890683122, 1.000000000000000000, 0.9659258262890683122, 1.000000000000000000, 0.9659258262890683122, 1.000000000000000000, 0.9659258262890683122, 1.000000000000000000, 0.9659258262890683122, 1.000000000000000000, 0.9659258262890683122, 1.000000000000000000, 0.9659258262890683122, 1.000000000000000000, 0.9659258262890683122, 1.000000000000000000, 0.9659258262890683122, 1.000000000000000000, 0.9659258262890683122, 1.000000000000000000, 0.9659258262890683122, 1.000000000000000000, 0.9659258262890683122, 1.000000000000000000, 0.9659258262890683122, 1.000000000000000000, 0.9659258262890683122, 1.000000000000000000, 0.9659258262890683122, 1.000000000000000000, 0.9659258262890683122, 1.000000000000000000, 0.9659258262890683122, 1.000000000000000000, 0.9659258262890683122, 1.000000000000000000, 0.9659258262890683122, 1.000000000000000000, 0.9659258262890683122, 1.000000000000000000, 0.9659258262890683122, 1.000000000000000000, 0.9659258262890683122, 1.000000000000000000, 0.9659258262890683122, 1.000000000000000000, 0.9659258262890683122, 1.000000000000000000, 0.9659258262890683122, 1.000000000000000000, 0.9659258262890683122, 1.000000000000000000, 0.9659258262890683122, 1.000000000000000000, 0.9659258262890683122, 1.000000000000000000, 0.9659258262890683122, 1.000000000000000000, 0.9659258262890683122, 1.000000000000000000, 0.9659258262890683122, 1.000000000000000000, 0.9659258262890683122, 1.000000000000000000, 0.9659258262890683122, 1.000000000000000000, 0.9659258262890683122, 1.000000000000000000, 0.9659258262890683122, 1.000000000000000000, 0.9659258262890683122, 1.000000000000000000, 0.9659258262890683122, 1.000000000000000000, 0.9659258262890683122, 1.000000000000000000, 0.9659258262890683122, 1.000000000000000000, 0.9659258262890683122, 1.000000000000000000, 0.9659258262890683122, 1.000000000000000000, 0.9659258262890683122, 1.000000000000000000, 0.9659258262890683122, 1.000000000000000000, 0.9659258262890683122, 1.000000000000000000, 0.9659258262890683122, 1.000000000000000000, 0.9659258262890683122, 1.000000000000000000, 0.9659258262890683122, 1.000000000000000000, 0.9659258262890683122, 1.000000000000000000, 0.9659258262890683122, 1.000000000000000000, 0.9659258262890683122, 1.000000000000000000, 0.9659258262890683122, 1.000000000000000000, 0.9659258262890683122, 1.000000000000000000, 0.9659258262890683122, 1.000000000000000000, 0.9659258262890683122, 1.000000000000000000, 0.9659258262890683122, 1.000000000000000000, 0.9659258262890683122, 1.000000000000000000, 0.9659258262890683122, 1.000000000000000000, 0.9659258262890683122, 1.000000000000000000, 0.9659258262890683122, 1.000000000000000000, 0.9659258262890683122, 1.000000000000000000, 0.9659258262890683122, 1.000000000000000000, 0.9659258262890683122, 1.000000000000000000, 0.9659258262890683122, 1.000000000000000000, 0.9659258262890683122, 1.000000000000000000, 0.9659258262890683122, 1.000000000000000000, 0.9659258262890683122, 1.000000000000000000, 0.9659258262890683122, 1.000000000000000000, 0.9659258262890683122, 1.000000000000000000, 0.9659258262890683122, 1.000000000000000000, 0.9659258262890683122, 1.000000000000000000, 0.9659258262890683122, 1.000000000000000000, 0.9659258262890683122, 1.000000000000000000, 0.9659258262890683122, 1.000000000000000000, 0.9659258262890683122, 1.000000000000000000, 0.9659258262890683122, 1.000000000000000000, 0.9659258262890683122, 1.000000000000000000, 0.9659258262890683122, 1.000000000000000000, 0.9659258262890683122, 1.000000000000000000, 0.9659258262890683122, 1.000000000000000000, 0.9659258262890683122, 1.000000000000000000, 0.9659258262890683122, 1.000000000000000000, 0.9659258262890683122, 1.000000000000000000, 0.9659258262890683122, 1.000000000000000000, 0.9659258262890683122, 1.000000000000000000, 0.9659258262890683122, 1.000000000000000000, 0.9659258262890683122, 1.000000000000000000, 0.9659258262890683122, 1.000000000000000000, 0.9659258262890683122, 1.000000000000000000, 0.9659258262890683122, 1.000000000000000000, 0.9659258262890683122, 1.000000000000000000, 0.9659258262890683122, 1.000000000000000000, 0.9659258262890683122, 1.000000000000000000, 0.9659258262890683122, 1.000000000000000000, 0.9659258262890683122, 1.000000000000000000, 0.9659258262890683122, 1.000000000000000000, 0.9659258262890683122, 1.000000000000000000, 0.9659258262890683122, 1.000000000000000000, 0.9659258262890683122, 1.000000000000000000, 0.9659258262890683122, 1.000000000000000000, 0.9659258262890683122, 1.000000000000000000, 0.9659258262890683122, 1.000000000000000000, 0.9659258262890683122, 1.000000000000000000, 0.9659258262890683122, 1.000000000000000000, 0.9659258262890683122, 1.000000000000000000, 0.9659258262890683122, 1.000000000000000000, 0.9659258262890683122, 1.000000000000000000, 0.9659258262890683122, 1.000000000000000000, 0.9659258262890683122, 1.000000000000000000, 0.9659258262890683122, 1.000000000000000000, 0.9659258262890683122, 1.000000000000000000, 0.9659258262890683122, 1.000000000000000000, 0.9659258262890683122, 1.000000000000000000, 0.9659258262890683122, 1.000000000000000000, 0.9659258262890683122, 1.000000000000000000, 0.9659258262890683122, 1.000000000000000000, 0.9659258262890683122, 1.000000000000000000, 0.9659258262890683122, 1.000000000000000000, 0.9659258262890683122, 1.000000000000000000, 0.9659258262890683122, 1.000000000000000000, 0.9659258262890683122, 1.000000000000000000, 0.9659258262890683122, 1.000000000000000000, 0.9659258262890683122, 1.000000000000000000, 0.9659258262890683122, 1.000000000000000000, 0.9659258262890683122, 1.000000000000000000, 0.9659258262890683122, 1.000000000000000000, 0.9659258262890683122, 1.000000000000000000, 0.9659258262890683122, 1.000000000000000000, 0.9659258262890683122, 1.000000000000000000, 0.9659258262890683122, 1.000000000000000000, 0.9659258262890683122, 1.000000000000000000, 0.9659258262890683122, 1.000000000000000000, 0.9659258262890683122, 1.000000000000000000, 0.9659258262890683122, 1.000000000000000000, 0.9659258262890683122, 1.000000000000000000, 0.9659258262890683122, 1.000000000000000000, 0.9659258262890683122, 1.000000000000000000, 0.9659258262890683122, 1.000000000000000000, 0.9659258262890683122, 1.000000000000000000, 0.9659258262890683122, 1.000000000000000000, 0.9659258262890683122, 1.000000000000000000, 0.9659258262890683122, 1.000000000000000000, 0.9659258262890683122, 1.000000000000000000, 0.9659258262890683122, 1.000000000000000000, 0.9659258262890683122, 1.000000000000000000, 0.9659258262890683122, 1.000000000000000000, 0.9659258262890683122, 1.000000000000000000, 0.9659258262890683122, 1.000000000000000000, 0.9659258262890683122, 1.000000000000000000, 0.9659258262890683122, 1.000000000000000000, 0.9659258262890683122, 1.000000000000000000, 0.9659258262890683122, 1.000000000000000000, 0.9659258262890683122, 1.000000000000000000, 0.9659258262890683122, 1.000000000000000000, 0.9659258262890683122, 1.000000000000000000, 0.9659258262890683122, 1.000000000000000000, 0.9659258262890683122, 1.000000000000000000, 0.9659258262890683122, 1.000000000000000000, 0.9659258262890683122, 1.000000000000000000, 0.9659258262890683122, 1.000000000000000000, 0.9659258262890683122, 1.000000000000000000, 0.9659258262890683122, 1.000000000000000000, 0.9659258262890683122, 1.000000000000000000, 0.9659258262890683122, 1.000000000000000000, 0.9659258262890683122, 1.000000000000000000, 0.9659258262890683122, 1.000000000000000000, 0.9659258262890683122, 1.000000000000000000, 0.9659258262890683122, 1.000000000000000000, 0.9659258262890683122, 1.000000000000000000, 0.9659258262890683122, 1.000000000000000000, 0.9659258262890683122, 1.000000000000000000, 0.9659258262890683122, 1.000000000000000000, 0.9659258262890683122, 1.000000000000000000, 0.9659258262890683122, 1.000000000000000000, 0.9659258262890683122, 1.000000000000000000, 0.9659258262890683122, 1.000000000000000000, 0.9659258262890683122, 1.000000000000000000, 0.9659258262890683122, 1.000000000000000000, 0.9659258262890683122, 1.000000000000000000, 0.9659258262890683122, 1.000000000000000000, 0.9659258262890683122, 1.000000000000000000, 0.9659258262890683122, 1.000000000000000000, 0.9659258262890683122, 1.000000000000000000, 0.9659258262890683122, 1.000000000000000000),
 ( 1.000000000000000000, 0.9659258262890683122, 1.000000000000000000, 0.9659258262890683122, 1.000000000000000000, 0.9659258262890683122, 1.000000000000000000, 0.9659258262890683122, 1.000000000000000000, 0.9659258262890683122, 1.000000000000000000, 0.9659258262890683122, 1.000000000000000000, 0.9659258262890683122, 1.000000000000000000, 0.9659258262890683122, 1.000000000000000000, 0.9659258262890683122, 1.000000000000000000, 0.9659258262890683122, 1.000000000000000000, 0.9659258262890683122, 1.000000000000000000, 0.9659258262890683122, 1.000000000000000000, 0.9659258262890683122, 1.000000000000000000, 0.9659258262890683122, 1.000000000000000000, 0.9659258262890683122, 1.000000000000000000, 0.9659258262890683122, 1.000000000000000000, 0.9659258262890683122, 1.000000000000000000, 0.9659258262890683122, 1.000000000000000000, 0.9659258262890683122, 1.000000000000000000, 0.9659258262890683122, 1.000000000000000000, 0.9659258262890683122, 1.000000000000000000, 0.9659258262890683122, 1.000000000000000000, 0.9659258262890683122, 1.000000000000000000, 0.9659258262890683122, 1.000000000000000000, 0.9659258262890683122, 1.000000000000000000, 0.9659258262890683122, 1.000000000000000000, 0.9659258262890683122, 1.000000000000000000, 0.9659258262890683122, 1.000000000000000000, 0.9659258262890683122, 1.000000000000000000, 0.9659258262890683122, 1.000000000000000000, 0.9659258262890683122, 1.000000000000000000, 0.9659258262890683122, 1.000000000000000000, 0.9659258262890683122, 1.000000000000000000, 0.9659258262890683122, 1.000000000000000000, 0.9659258262890683122, 1.000000000000000000, 0.9659258262890683122, 1.000000000000000000, 0.9659258262890683122, 1.000000000000000000, 0.9659258262890683122, 1.000000000000000000, 0.9659258262890683122, 1.000000000000000000, 0.9659258262890683122, 1.000000000000000000, 0.9659258262890683122, 1.000000000000000000, 0.9659258262890683122, 1.000000000000000000, 0.9659258262890683122, 1.000000000000000000, 0.9659258262890683122, 1.000000000000000000, 0.9659258262890683122, 1.000000000000000000, 0.9659258262890683122, 1.000000000000000000, 0.9659258262890683122, 1.000000000000000000, 0.9659258262890683122, 1.000000000000000000, 0.9659258262890683122, 1.000000000000000000, 0.9659258262890683122, 1.000000000000000000, 0.9659258262890683122, 1.000000000000000000, 0.9659258262890683122, 1.000000000000000000, 0.9659258262890683122, 1.000000000000000000, 0.9659258262890683122, 1.000000000000000000, 0.9659258262890683122, 1.000000000000000000, 0.9659258262890683122, 1.000000000000000000, 0.9659258262890683122, 1.000000000000000000, 0.9659258262890683122, 1.000000000000000000, 0.9659258262890683122, 1.000000000000000000, 0.9659258262890683122, 1.000000000000000000, 0.9659258262890683122, 1.000000000000000000, 0.9659258262890683122, 1.000000000000000000, 0.9659258262890683122, 1.000000000000000000, 0.9659258262890683122, 1.000000000000000000, 0.9659258262890683122, 1.000000000000000000, 0.9659258262890683122, 1.000000000000000000, 0.9659258262890683122, 1.000000000000000000, 0.9659258262890683122, 1.000000000000000000, 0.9659258262890683122, 1.000000000000000000, 0.9659258262890683122, 1.000000000000000000, 0.9659258262890683122, 1.000000000000000000, 0.9659258262890683122, 1.000000000000000000, 0.9659258262890683122, 1.000000000000000000, 0.9659258262890683122, 1.000000000000000000, 0.9659258262890683122, 1.000000000000000000, 0.9659258262890683122, 1.000000000000000000, 0.9659258262890683122, 1.000000000000000000, 0.9659258262890683122, 1.000000000000000000, 0.9659258262890683122, 1.000000000000000000, 0.9659258262890683122, 1.000000000000000000, 0.9659258262890683122, 1.000000000000000000, 0.9659258262890683122, 1.000000000000000000, 0.9659258262890683122, 1.000000000000000000, 0.9659258262890683122, 1.000000000000000000, 0.9659258262890683122, 1.000000000000000000, 0.9659258262890683122, 1.000000000000000000, 0.9659258262890683122, 1.000000000000000000, 0.9659258262890683122, 1.000000000000000000, 0.9659258262890683122, 1.000000000000000000, 0.9659258262890683122, 1.000000000000000000, 0.9659258262890683122, 1.000000000000000000, 0.9659258262890683122, 1.000000000000000000, 0.9659258262890683122, 1.000000000000000000, 0.9659258262890683122, 1.000000000000000000, 0.9659258262890683122, 1.000000000000000000, 0.9659258262890683122, 1.000000000000000000, 0.9659258262890683122, 1.000000000000000000, 0.9659258262890683122, 1.000000000000000000, 0.9659258262890683122, 1.000000000000000000, 0.9659258262890683122, 1.000000000000000000, 0.9659258262890683122, 1.000000000000000000, 0.9659258262890683122, 1.000000000000000000, 0.9659258262890683122, 1.000000000000000000, 0.9659258262890683122, 1.000000000000000000, 0.9659258262890683122, 1.000000000000000000, 0.9659258262890683122, 1.000000000000000000, 0.9659258262890683122, 1.000000000000000000, 0.9659258262890683122, 1.000000000000000000, 0.9659258262890683122, 1.000000000000000000, 0.9659258262890683122, 1.000000000000000000, 0.9659258262890683122, 1.000000000000000000, 0.9659258262890683122, 1.000000000000000000, 0.9659258262890683122, 1.000000000000000000, 0.9659258262890683122, 1.000000000000000000, 0.9659258262890683122, 1.000000000000000000, 0.9659258262890683122, 1.000000000000000000, 0.9659258262890683122, 1.000000000000000000, 0.9659258262890683122, 1.000000000000000000, 0.9659258262890683122, 1.000000000000000000, 0.9659258262890683122, 1.000000000000000000, 0.9659258262890683122, 1.000000000000000000, 0.9659258262890683122, 1.000000000000000000, 0.9659258262890683122, 1.000000000000000000, 0.9659258262890683122, 1.000000000000000000, 0.9659258262890683122, 1.000000000000000000, 0.9659258262890683122, 1.000000000000000000, 0.9659258262890683122, 1.000000000000000000, 0.9659258262890683122, 1.000000000000000000, 0.9659258262890683122, 1.000000000000000000, 0.9659258262890683122, 1.000000000000000000, 0.9659258262890683122, 1.000000000000000000, 0.9659258262890683122, 1.000000000000000000, 0.9659258262890683122, 1.000000000000000000, 0.9659258262890683122, 1.000000000000000000, 0.9659258262890683122, 1.000000000000000000, 0.9659258262890683122, 1.000000000000000000, 0.9659258262890683122, 1.000000000000000000, 0.9659258262890683122, 1.000000000000000000, 0.9659258262890683122, 1.000000000000000000, 0.9659258262890683122, 1.000000000000000000, 0.9659258262890683122, 1.000000000000000000, 0.9659258262890683122, 1.000000000000000000, 0.9659258262890683122, 1.000000000000000000, 0.9659258262890683122, 1.000000000000000000, 0.9659258262890683122, 1.000000000000000000, 0.9659258262890683122, 1.000000000000000000, 0.9659258262890683122, 1.000000000000000000, 0.9659258262890683122, 1.000000000000000000, 0.9659258262890683122, 1.000000000000000000, 0.9659258262890683122, 1.000000000000000000, 0.9659258262890683122, 1.000000000000000000, 0.9659258262890683122, 1.000000000000000000, 0.9659258262890683122, 1.000000000000000000, 0.9659258262890683122, 1.000000000000000000, 0.9659258262890683122, 1.000000000000000000, 0.9659258262890683122, 1.000000000000000000, 0.9659258262890683122, 1.000000000000000000, 0.9659258262890683122, 1.000000000000000000, 0.9659258262890683122, 1.000000000000000000, 0.9659258262890683122, 1.000000000000000000, 0.9659258262890683122, 1.000000000000000000, 0.9659258262890683122, 1.000000000000000000, 0.9659258262890683122, 1.000000000000000000, 0.9659258262890683122, 1.000000000000000000, 0.9659258262890683122, 1.000000000000000000, 0.9659258262890683122, 1.000000000000000000, 0.9659258262890683122, 1.000000000000000000, 0.9659258262890683122, 1.000000000000000000, 0.9659258262890683122, 1.000000000000000000, 0.9659258262890683122, 1.000000000000000000, 0.9659258262890683122, 1.000000000000000000, 0.9659258262890683122, 1.000000000000000000, 0.9659258262890683122, 1.000000000000000000, 0.9659258262890683122, 1.000000000000000000, 0.9659258262890683122, 1.000000000000000000, 0.9659258262890683122, 1.000000000000000000, 0.9659258262890683122, 1.000000000000000000, 0.9659258262890683122, 1.000000000000000000, 0.9659258262890683122, 1.000000000000000000, 0.9659258262890683122, 1.000000000000000000, 0.9659258262890683122, 1.000000000000000000, 0.9659258262890683122, 1.000000000000000000, 0.9659258262890683122, 1.000000000000000000, 0.9659258262890683122, 1.000000000000000000, 0.9659258262890683122, 1.000000000000000000, 0.9659258262890683122, 1.000000000000000000, 0.9659258262890683122, 1.000000000000000000, 0.9659258262890683122, 1.000000000000000000, 0.9659258262890683122, 1.000000000000000000, 0.9659258262890683122, 1.000000000000000000, 0.9659258262890683122, 1.000000000000000000, 0.9659258262890683122, 1.000000000000000000, 0.9659258262890683122, 1.000000000000000000, 0.9659258262890683122, 1.000000000000000000, 0.9659258262890683122, 1.000000000000000000, 0.9659258262890683122, 1.000000000000000000, 0.9659258262890683122, 1.000000000000000000, 0.9659258262890683122, 1.000000000000000000, 0.9659258262890683122, 1.000000000000000000, 0.9659258262890683122, 1.000000000000000000, 0.9659258262890683122, 1.000000000000000000, 0.9659258262890683122, 1.000000000000000000, 0.9659258262890683122, 1.000000000000000000, 0.9659258262890683122, 1.000000000000000000, 0.9659258262890683122, 1.000000000000000000, 0.9659258262890683122, 1.000000000000000000, 0.9659258262890683122, 1.000000000000000000, 0.9659258262890683122, 1.000000000000000000, 0.9659258262890683122, 1.000000000000000000, 0.9659258262890683122, 1.000000000000000000, 0.9659258262890683122, 1.000000000000000000, 0.9659258262890683122, 1.000000000000000000, 0.9659258262890683122, 1.000000000000000000, 0.9659258262890683122, 1.000000000000000000, 0.9659258262890683122, 1.000000000000000000, 0.9659258262890683122, 1.000000000000000000, 0.9659258262890683122, 1.000000000000000000, 0.9659258262890683122, 1.000000000000000000, 0.9659258262890683122, 1.000000000000000000, 0.9659258262890683122, 1.000000000000000000, 0.9659258262890683122, 1.000000000000000000, 0.9659258262890683122, 1.000000000000000000, 0.9659258262890683122, 1.000000000000000000, 0.9659258262890683122, 1.000000000000000000, 0.9659258262890683122, 1.000000000000000000, 0.9659258262890683122, 1.000000000000000000, 0.9659258262890683122, 1.000000000000000000, 0.9659258262890683122, 1.000000000000000000, 0.9659258262890683122, 1.000000000000000000, 0.9659258262890683122, 1.000000000000000000, 0.9659258262890683122, 1.000000000000000000, 0.9659258262890683122, 1.000000000000000000, 0.9659258262890683122, 1.000000000000000000, 0.9659258262890683122, 1.000000000000000000, 0.9659258262890683122, 1.000000000000000000, 0.9659258262890683122, 1.000000000000000000, 0.9659258262890683122, 1.000000000000000000, 0.9659258262890683122, 1.000000000000000000, 0.9659258262890683122, 1.000000000000000000, 0.9659258262890683122, 1.000000000000000000, 0.9659258262890683122, 1.000000000000000000, 0.9659258262890683122, 1.000000000000000000, 0.9659258262890683122, 1.000000000000000000, 0.9659258262890683122, 1.000000000000000000, 0.9659258262890683122, 1.000000000000000000, 0.9659258262890683122, 1.000000000000000000, 0.9659258262890683122, 1.000000000000000000, 0.9659258262890683122, 1.000000000000000000, 0.9659258262890683122, 1.000000000000000000, 0.9659258262890683122, 1.000000000000000000, 0.9659258262890683122, 1.000000000000000000, 0.9659258262890683122, 1.000000000000000000, 0.9659258262890683122, 1.000000000000000000, 0.9659258262890683122, 1.000000000000000000, 0.9659258262890683122, 1.000000000000000000) ) ) 
 REPRESENTATION_ITEM ( '' )  SURFACE ( )  );
#24497 = CARTESIAN_POINT ( 'NONE',  ( -0.6299212598425188991, -0.1870078740157479769, 0.4822834645669291653 ) ) ;
#24498 = CARTESIAN_POINT ( 'NONE',  ( 0.6889763779527560139, 0.000000000000000000, 0.1181102362204724116 ) ) ;
#24499 = CARTESIAN_POINT ( 'NONE',  ( -0.2886821576726690264, 1.160628398849495868, -1.939323366023511852 ) ) ;
#24500 = VERTEX_POINT ( 'NONE', #63458 ) ;
#24501 = CARTESIAN_POINT ( 'NONE',  ( -0.1958661417322836995, 0.3392501089628017219, -1.899625614994437495 ) ) ;
#24502 = CARTESIAN_POINT ( 'NONE',  ( 0.3346456692913393205, -0.5400638737290845981, -0.3530559997133363437 ) ) ;
#24503 = VERTEX_POINT ( 'NONE', #24325 ) ;
#24504 = CARTESIAN_POINT ( 'NONE',  ( -0.5118110236220466680, -0.6692913385826771977, 8.415575281601705876E-17 ) ) ;
#24505 = CARTESIAN_POINT ( 'NONE',  ( -1.391076115485563314, -0.6046776061558809534, -0.2411417322834644161 ) ) ;
#24506 = CARTESIAN_POINT ( 'NONE',  ( 0.5708661417322841158, -0.5400638737290845981, -0.3530559997133363437 ) ) ;
#24507 = CARTESIAN_POINT ( 'NONE',  ( -0.09186351706036663400, -0.4281496062992124485, 0.4176697321401328655 ) ) ;
#24508 = CARTESIAN_POINT ( 'NONE',  ( -0.1958661417322836718, 0.3392501089628017219, -1.357611548556430625 ) ) ;
#24509 = CARTESIAN_POINT ( 'NONE',  ( -0.6561679790026240244, -0.6046776061558807314, 0.2411417322834647770 ) ) ;
#24510 = CARTESIAN_POINT ( 'NONE',  ( 0.3674540682414705883, -0.6046776061558807314, 0.2411417322834647770 ) ) ;
#24511 = CARTESIAN_POINT ( 'NONE',  ( -0.3805774278215216522, 0.05413385826771666132, 0.4176697321401328100 ) ) ;
#24512 = CARTESIAN_POINT ( 'NONE',  ( 0.2362204724409456558, -0.1870078740157479769, 0.3641732283464567677 ) ) ;
#24513 = CARTESIAN_POINT ( 'NONE',  ( -0.2405540237485361554, -0.1712599301372657035, 5.748856329247442609 ) ) ;
#24514 = CARTESIAN_POINT ( 'NONE',  ( 0.09186351706036799403, -0.4281496062992127816, -0.4176697321401328100 ) ) ;
#24515 = VECTOR ( 'NONE', #35049, 39.37007874015748143 ) ;
#24516 = CARTESIAN_POINT ( 'NONE',  ( -0.7080320533160963103, 1.900312960331933976, -0.5309055118110235227 ) ) ;
#24517 = CARTESIAN_POINT ( 'NONE',  ( 1.548556430446194954, -0.6046776061558807314, 0.2411417322834647770 ) ) ;
#24518 = CARTESIAN_POINT ( 'NONE',  ( -0.1049643490035302024, -0.3917322834645671215, -2.741469816272964710 ) ) ;
#24519 = ORIENTED_EDGE ( 'NONE', *, *, #82130, .F. ) ;
#24520 = ORIENTED_EDGE ( 'NONE', *, *, #28027, .F. ) ;
#24521 = CARTESIAN_POINT ( 'NONE',  ( 0.8070866141732289112, -0.5400638737290845981, -0.3530559997133363437 ) ) ;
#24522 = CARTESIAN_POINT ( 'NONE',  ( 0.1574803149606306130, -0.1870078740157479769, 0.3641732283464567677 ) ) ;
#24524 = CARTESIAN_POINT ( 'NONE',  ( -2.795275590551183242, 1.614173228346456712, -1.327125379919507468E-16 ) ) ;
#24523 = DIRECTION ( 'NONE',  ( 0.000000000000000000, 0.000000000000000000, 1.000000000000000000 ) ) ;
#24525 = CARTESIAN_POINT ( 'NONE',  ( -0.1049643490035302024, -0.3917322834645671215, -1.101706036745407014 ) ) ;
#24526 = CARTESIAN_POINT ( 'NONE',  ( 0.4091458600556403535, 0.2362204724409449896, 0.1069553805774278027 ) ) ;
#24527 = SURFACE_SIDE_STYLE ('',( #37162 ) ) ;
#24528 = EDGE_CURVE ( 'NONE', #43552, #9013, #30649, .T. ) ;
#24529 = CARTESIAN_POINT ( 'NONE',  ( 4.837279021331061486E-17, -0.3949938075777409963, 0.1594488188976377896 ) ) ;
#24530 = CARTESIAN_POINT ( 'NONE',  ( 0.3740157480314966754, 0.1660481256975883668, -0.3530559997133364547 ) ) ;
#24531 = CARTESIAN_POINT ( 'NONE',  ( -1.095800524934382292, -0.3162353388693409650, -0.4822834645669289433 ) ) ;
#24532 = CARTESIAN_POINT ( 'NONE',  ( -1.246719160104986512, 0.05413385826771666132, 0.4176697321401328100 ) ) ;
#24533 = CARTESIAN_POINT ( 'NONE',  ( 0.2362204724409456558, -0.1870078740157480879, -0.4822834645669291653 ) ) ;
#24534 = CARTESIAN_POINT ( 'NONE',  ( 0.9317585301837276734, -0.4281496062992124485, 0.4176697321401328655 ) ) ;
#24535 = CARTESIAN_POINT ( 'NONE',  ( 1.502624671916010790, -0.08942795157527998196, 0.3641732283464567121 ) ) ;
#24536 = ITEM_DEFINED_TRANSFORMATION ( 'NONE', 'NONE', #18137,  #22098 ) ;
#24537 = CARTESIAN_POINT ( 'NONE',  ( 1.194225721784777594, -0.004921259842519576551, 0.3153832671262227771 ) ) ;
#24538 = CARTESIAN_POINT ( 'NONE',  ( -0.7611548556430438595, -0.6046776061558809534, -0.2411417322834644161 ) ) ;
#24539 = CARTESIAN_POINT ( 'NONE',  ( 4.893765752498283308E-17, -0.3996062992125985480, -0.6279527559055118058 ) ) ;
#24540 = CARTESIAN_POINT ( 'NONE',  ( -1.555118110236219930, -0.4536011799217368745, -0.2665933059059886201 ) ) ;
#24541 = B_SPLINE_CURVE_WITH_KNOTS ( 'NONE', 3,
 ( #43474, #34616, #14017, #45552 ),
 .UNSPECIFIED., .F., .F.,
 ( 4, 4 ),
 ( 0.09865403381126973403, 0.1000779257405593758 ),
 .UNSPECIFIED. ) ;
#24542 = CARTESIAN_POINT ( 'NONE',  ( -0.3392501089628019995, 0.1958661417322832277, -0.3333333333333333148 ) ) ;
#24543 = CARTESIAN_POINT ( 'NONE',  ( -0.2034120734908128059, 0.2952755905511811885, 0.1292274648535926551 ) ) ;
#24545 = FACE_OUTER_BOUND ( 'NONE', #31509, .T. ) ;
#24544 = CARTESIAN_POINT ( 'NONE',  ( 0.9580052493438327987, -0.4281496062992127816, -0.4176697321401328100 ) ) ;
#24546 = CARTESIAN_POINT ( 'NONE',  ( -1.423884514435694859, -0.2845877964562159024, 0.3641732283464567677 ) ) ;
#24547 = CARTESIAN_POINT ( 'NONE',  ( -0.08530183727034056085, -0.3162353388693405765, 0.4822834645669290543 ) ) ;
#24548 = CARTESIAN_POINT ( 'NONE',  ( 0.7480314960629927956, -0.5511811023622047445, 6.969142054262312111E-17 ) ) ;
#24549 = CARTESIAN_POINT ( 'NONE',  ( -1.535433070866141225, 0.1771653543307087630, 0.000000000000000000 ) ) ;
#24550 = CARTESIAN_POINT ( 'NONE',  ( 1.148293963254593875, -0.6692913385826771977, 0.1292274648535927661 ) ) ;
#24551 = LINE ( 'NONE', #50217, #34409 ) ;
#24552 = CARTESIAN_POINT ( 'NONE',  ( -0.4396325459317579898, 0.1771653543307087630, 0.09757992244046791164 ) ) ;
#24553 = CARTESIAN_POINT ( 'NONE',  ( -0.4658792650918627265, -0.05778040916215522460, 0.4822834645669289988 ) ) ;
#24554 = CARTESIAN_POINT ( 'NONE',  ( -1.640419947506561060, -0.004921259842519576551, 0.3153832671262227771 ) ) ;
#24555 = CARTESIAN_POINT ( 'NONE',  ( -1.279527559055116948, -0.5400638737290844871, 0.3530559997133364547 ) ) ;
#24556 = CARTESIAN_POINT ( 'NONE',  ( 1.272965879265092637, -0.4281496062992127816, -0.4176697321401328100 ) ) ;
#24557 = CARTESIAN_POINT ( 'NONE',  ( -0.3917322834645670104, -0.1049643490035307020, -0.9875521241807894146 ) ) ;
#24558 = CARTESIAN_POINT ( 'NONE',  ( -1.377952755905511140, -0.5511811023622047445, 6.969142054262312111E-17 ) ) ;
#24559 = CARTESIAN_POINT ( 'NONE',  ( 1.111560454228161632, 1.088337758531439992, -0.1537820215174434957 ) ) ;
#24560 = CARTESIAN_POINT ( 'NONE',  ( 1.469816272965879911, 0.2306618581243847221, -0.2411417322834647770 ) ) ;
#24561 = CARTESIAN_POINT ( 'NONE',  ( -0.4091458600556402980, -0.2362204724409451284, -1.861548556430446144 ) ) ;
#24562 = CARTESIAN_POINT ( 'NONE',  ( -1.437007874015747477, -0.5400638737290844871, 0.3530559997133364547 ) ) ;
#24563 = CARTESIAN_POINT ( 'NONE',  ( 1.633858267716535639, -0.5400638737290844871, 0.3530559997133364547 ) ) ;
#24564 = CARTESIAN_POINT ( 'NONE',  ( -1.017060367454067249, -0.2845877964562161244, -0.3641732283464567121 ) ) ;
#24565 = CARTESIAN_POINT ( 'NONE',  ( -0.5380577427821514602, 0.05413385826771666132, 0.4176697321401328100 ) ) ;
#24566 = CARTESIAN_POINT ( 'NONE',  ( -0.07874015748031421014, -0.1870078740157479769, 0.3641732283464567677 ) ) ;
#24567 = CARTESIAN_POINT ( 'NONE',  ( -1.200787401574802349, 0.07958543189024071263, -0.2665933059059888421 ) ) ;
#24568 = CARTESIAN_POINT ( 'NONE',  ( 1.351706036745407458, -0.3690944881889765550, -0.3153832671262227771 ) ) ;
#24569 = CIRCLE ( 'NONE', #59481, 0.1771653543307085410 ) ;
#24570 = CARTESIAN_POINT ( 'NONE',  ( 0.8727034120734913358, -0.05778040916215522460, 0.4822834645669289988 ) ) ;
#24571 = CARTESIAN_POINT ( 'NONE',  ( 1.601049868766404982, 0.2306618581243848609, 0.2411417322834645549 ) ) ;
#24572 = CARTESIAN_POINT ( 'NONE',  ( 0.5249343832021005074, -0.5023911411419708095, 0.1820866141732285504 ) ) ;
#24573 = CARTESIAN_POINT ( 'NONE',  ( 0.4199475065616805614, 0.2306618581243848609, 0.2411417322834645549 ) ) ;
#24574 = CARTESIAN_POINT ( 'NONE',  ( 0.7808398950131240079, -0.2845877964562159024, 0.3641732283464567677 ) ) ;
#24575 = VERTEX_POINT ( 'NONE', #18842 ) ;
#24576 = CARTESIAN_POINT ( 'NONE',  ( 1.548556430446194954, -0.6046776061558807314, 0.2411417322834647770 ) ) ;
#24577 = CARTESIAN_POINT ( 'NONE',  ( -1.187664041994749731, -0.3162353388693405765, 0.4822834645669290543 ) ) ;
#24578 = CARTESIAN_POINT ( 'NONE',  ( 0.07217847769028949700, -0.05778040916215560624, -0.4822834645669293319 ) ) ;
#24579 = CARTESIAN_POINT ( 'NONE',  ( 0.5387615594602676028, 2.409604939980833412E-17, -0.3464511005275205946 ) ) ;
#24580 = CARTESIAN_POINT ( 'NONE',  ( -0.1998031496062994405, 0.3460692066303957537, -2.452099737532808188 ) ) ;
#24581 = CARTESIAN_POINT ( 'NONE',  ( 0.6233595800524939223, -0.3162353388693405765, 0.4822834645669290543 ) ) ;
#24582 = CARTESIAN_POINT ( 'NONE',  ( 1.299212598425197429, 0.1771653543307087630, 0.000000000000000000 ) ) ;
#24583 = CARTESIAN_POINT ( 'NONE',  ( -0.1640419947506553400, -0.05778040916215560624, -0.4822834645669293319 ) ) ;
#24584 = CARTESIAN_POINT ( 'NONE',  ( 0.2427821522309716595, -0.3162353388693409650, -0.4822834645669289433 ) ) ;
#24585 = CARTESIAN_POINT ( 'NONE',  ( -0.3460692066303958092, -0.1998031496062994683, -2.257217847769029007 ) ) ;
#24586 = CARTESIAN_POINT ( 'NONE',  ( 0.3949938075777409408, 0.1058382717557500574, -1.699475065616798064 ) ) ;
#24587 = CARTESIAN_POINT ( 'NONE',  ( -0.3573726498115010752, 1.223876645116869000, 1.063858708914491524 ) ) ;
#24588 = CARTESIAN_POINT ( 'NONE',  ( 0.4091458600556403535, 0.2362204724409449896, -2.493438320209973469 ) ) ;
#24589 = CARTESIAN_POINT ( 'NONE',  ( 0.3392501089628018884, -0.1958661417322834220, -0.5695538057742781657 ) ) ;
#24590 = CARTESIAN_POINT ( 'NONE',  ( -0.6167979002624665030, -0.004921259842519576551, 0.3153832671262227771 ) ) ;
#24591 = CARTESIAN_POINT ( 'NONE',  ( -0.8858267716535425107, 0.1660481256975883668, -0.3530559997133364547 ) ) ;
#24592 = CARTESIAN_POINT ( 'NONE',  ( 0.5708661417322841158, -0.5400638737290845981, -0.3530559997133363437 ) ) ;
#24593 = CARTESIAN_POINT ( 'NONE',  ( 0.3949938075777409408, -0.1058382717557499186, -2.393044619422572072 ) ) ;
#24594 = CARTESIAN_POINT ( 'NONE',  ( 0.7545931758530189937, 0.2952755905511810774, -0.1292274648535930714 ) ) ;
#24595 = CARTESIAN_POINT ( 'NONE',  ( -1.587926509186350810, 0.05413385826771626580, -0.4176697321401330321 ) ) ;
#24596 = CARTESIAN_POINT ( 'NONE',  ( 0.8727034120734912248, -0.3162353388693409650, -0.4822834645669289433 ) ) ;
#24597 = CARTESIAN_POINT ( 'NONE',  ( 0.4091458600556403535, 0.2362204724409449896, -2.808398950131233640 ) ) ;
#24598 = CARTESIAN_POINT ( 'NONE',  ( 0.3996062992125986035, 0.1070741851644054776, -2.329396325459317296 ) ) ;
#24599 = CARTESIAN_POINT ( 'NONE',  ( -0.7426113562971994320, 2.199547029021313715, 0.5309055118110236338 ) ) ;
#24600 = CARTESIAN_POINT ( 'NONE',  ( 0.8530183727034126306, 0.05413385826771626580, -0.4176697321401330321 ) ) ;
#24601 = CARTESIAN_POINT ( 'NONE',  ( 0.5249343832021003964, 0.2306618581243847221, -0.2411417322834647770 ) ) ;
#24602 = CARTESIAN_POINT ( 'NONE',  ( 1.069553805774278610, -0.5511811023622046335, 0.09757992244046803654 ) ) ;
#24603 = CARTESIAN_POINT ( 'NONE',  ( 1.594488188976378673, -0.5400638737290845981, -0.3530559997133363437 ) ) ;
#24604 = CARTESIAN_POINT ( 'NONE',  ( 0.3392501089628018884, -0.1958661417322834220, -0.1896325459317586282 ) ) ;
#24605 = FACE_OUTER_BOUND ( 'NONE', #45084, .T. ) ;
#24606 = CARTESIAN_POINT ( 'NONE',  ( 0.6233595800524942554, -0.05778040916215560624, -0.4822834645669293319 ) ) ;
#24607 = VECTOR ( 'NONE', #41860, 39.37007874015748143 ) ;
#24608 = CARTESIAN_POINT ( 'NONE',  ( 0.4724409448818898682, 2.892866454678787531E-17, -2.007874015748031482 ) ) ;
#24609 = CARTESIAN_POINT ( 'NONE',  ( -0.5446194225721777693, -0.3162353388693409650, -0.4822834645669289433 ) ) ;
#24610 = CARTESIAN_POINT ( 'NONE',  ( -1.062992125984250968, 0.2952755905511811885, 0.000000000000000000 ) ) ;
#24611 = CARTESIAN_POINT ( 'NONE',  ( 1.325459317585302665, 0.05413385826771626580, -0.4176697321401330321 ) ) ;
#24612 = CARTESIAN_POINT ( 'NONE',  ( -0.1958661417322834220, -0.3392501089628018884, -0.6227034120734910028 ) ) ;
#24613 = CARTESIAN_POINT ( 'NONE',  ( -0.3917322834645671215, 0.1049643490035301469, -1.599737532808399143 ) ) ;
#24614 = CARTESIAN_POINT ( 'NONE',  ( -0.1049643490035307020, 0.3917322834645669549, -2.833333333333333037 ) ) ;
#24615 = CARTESIAN_POINT ( 'NONE',  ( 1.555118110236221041, 0.1660481256975883668, -0.3530559997133364547 ) ) ;
#24616 = VERTEX_POINT ( 'NONE', #36544 ) ;
#24617 = CARTESIAN_POINT ( 'NONE',  ( 0.1058382717557499880, 0.3949938075777411073, -2.513123359580052174 ) ) ;
#24618 = EDGE_LOOP ( 'NONE', ( #56304, #27225, #54969, #65436, #21826, #6615, #82996, #11137, #13136, #40688, #74849, #70590, #49901, #37618, #77313, #75271, #61478, #68226, #61135, #74198, #68505, #28558, #1888, #56649, #79951, #17555, #25298, #70152, #66764, #45943, #1465, #38688, #59278, #62179, #60501, #73710 ) ) ;
#24619 = DIRECTION ( 'NONE',  ( 0.000000000000000000, -1.000000000000000000, -0.000000000000000000 ) ) ;
#24620 = CARTESIAN_POINT ( 'NONE',  ( 1.469816272965879911, 0.1283753931104746893, -0.1820866141732285504 ) ) ;
#24621 = CARTESIAN_POINT ( 'NONE',  ( -0.1998031496062994683, 0.3460692066303958092, -1.272965879265091749 ) ) ;
#24622 = CARTESIAN_POINT ( 'NONE',  ( 1.476377952755906442, -0.4536011799217367080, 0.2665933059059888421 ) ) ;
#24623 = CARTESIAN_POINT ( 'NONE',  ( -0.4091458600556402980, -0.2362204724409451284, -0.7591863517060367661 ) ) ;
#24624 = CARTESIAN_POINT ( 'NONE',  ( 0.3836918680457899744, 8.471767977567108961E-16, -0.4445507791589058955 ) ) ;
#24625 = DIRECTION ( 'NONE',  ( -1.000000000000000000, 0.000000000000000000, -3.491481338843132961E-15 ) ) ;
#24626 = CARTESIAN_POINT ( 'NONE',  ( -0.3392501089628019995, 0.1958661417322832277, -0.5833333333333334814 ) ) ;
#24627 = EDGE_CURVE ( 'NONE', #50308, #61368, #69369, .T. ) ;
#24628 = CARTESIAN_POINT ( 'NONE',  ( -0.7874015748031489847, -0.1870078740157480601, -0.3641732283464567677 ) ) ;
#24629 = CARTESIAN_POINT ( 'NONE',  ( -1.227034120734907585, 0.1771653543307087630, 0.09757992244046791164 ) ) ;
#24630 = CARTESIAN_POINT ( 'NONE',  ( -1.397637795275589623, -0.5400638737290845981, -0.3530559997133363437 ) ) ;
#24631 = CARTESIAN_POINT ( 'NONE',  ( 0.1837270341207354329, 0.2306618581243848609, 0.2411417322834645549 ) ) ;
#24632 = CARTESIAN_POINT ( 'NONE',  ( 1.528871391076116026, -0.6692913385826773087, -0.1292274648535924053 ) ) ;
#24633 = ORIENTED_EDGE ( 'NONE', *, *, #37682, .F. ) ;
#24634 = CARTESIAN_POINT ( 'NONE',  ( 1.456692913385827515, 0.2952755905511811885, 0.000000000000000000 ) ) ;
#24635 = CARTESIAN_POINT ( 'NONE',  ( -1.614173228346457378, 0.2753471884572480932, 0.1372047244094471985 ) ) ;
#24636 = CARTESIAN_POINT ( 'NONE',  ( -0.1265901696524993347, 0.4724409448818895907, -2.211286089238845065 ) ) ;
#24637 = FACE_OUTER_BOUND ( 'NONE', #30203, .T. ) ;
#24638 = CARTESIAN_POINT ( 'NONE',  ( -0.3149606299212590610, -0.1870078740157480601, -0.3641732283464567677 ) ) ;
#24639 = CARTESIAN_POINT ( 'NONE',  ( -1.338582677165353729, -0.1870078740157479769, 0.4822834645669291653 ) ) ;
#24640 = CARTESIAN_POINT ( 'NONE',  ( 1.082677165354331228, 0.1660481256975883668, -0.3530559997133364547 ) ) ;
#24641 = ORIENTED_EDGE ( 'NONE', *, *, #1862, .T. ) ;
#24643 = CYLINDRICAL_SURFACE ( 'NONE', #27728, 0.3937007874015748254 ) ;
#24642 = CARTESIAN_POINT ( 'NONE',  ( -1.220472440944882386, -0.1870078740157480046, 1.254653134982923898E-17 ) ) ;
#24644 = CARTESIAN_POINT ( 'NONE',  ( 1.561679790026247350, 0.05413385826771626580, -0.4176697321401330321 ) ) ;
#24645 = CARTESIAN_POINT ( 'NONE',  ( -1.089238845144356427, 0.05413385826771666132, 0.4176697321401328100 ) ) ;
#24646 = CARTESIAN_POINT ( 'NONE',  ( 0.3917322834645669549, 2.398668435337827645E-17, -0.5131040437982135050 ) ) ;
#24647 = CARTESIAN_POINT ( 'NONE',  ( -0.3674540682414692561, -0.5023911411419708095, -0.1820866141732282451 ) ) ;
#24648 = CARTESIAN_POINT ( 'NONE',  ( 0.1049643490035303689, 0.3917322834645670104, -0.8654855643044619962 ) ) ;
#24649 = CARTESIAN_POINT ( 'NONE',  ( -0.5839895013123351797, -0.5511811023622046335, 0.09757992244046803654 ) ) ;
#24650 = CARTESIAN_POINT ( 'NONE',  ( 0.3871391076115492380, -0.08942795157528024563, -0.3641732283464568787 ) ) ;
#24651 = CARTESIAN_POINT ( 'NONE',  ( 0.6889763779527563470, 0.1660481256975883668, -0.3530559997133364547 ) ) ;
#24652 = CARTESIAN_POINT ( 'NONE',  ( -0.6233595800524928121, -0.2845877964562161244, -0.3641732283464567121 ) ) ;
#24653 = CARTESIAN_POINT ( 'NONE',  ( -0.2867679344610364334, -0.2867679344610367109, -2.728346456692912536 ) ) ;
#24654 = CARTESIAN_POINT ( 'NONE',  ( 1.364829396325459854, -0.6046776061558809534, -0.2411417322834644161 ) ) ;
#24655 = CARTESIAN_POINT ( 'NONE',  ( -1.200787401574802349, -0.5400638737290844871, 0.3530559997133364547 ) ) ;
#24656 = CARTESIAN_POINT ( 'NONE',  ( 0.3458507752293908943, -0.3458507752293908943, -0.9625984251968502381 ) ) ;
#24657 = CARTESIAN_POINT ( 'NONE',  ( -0.3477690288713905509, -0.6692913385826771977, 0.1292274648535927661 ) ) ;
#24658 = CARTESIAN_POINT ( 'NONE',  ( -0.5314960629921250401, 0.1660481256975885056, 0.3530559997133364547 ) ) ;
#24659 = CARTESIAN_POINT ( 'NONE',  ( 1.122047244094488860, -0.4536011799217368745, -0.2665933059059886201 ) ) ;
#24660 = CARTESIAN_POINT ( 'NONE',  ( 0.2230971128608929543, -0.004921259842519870586, -0.3153832671262229437 ) ) ;
#24661 = CARTESIAN_POINT ( 'NONE',  ( -0.2034120734908131112, -0.6692913385826773087, -0.1292274648535924053 ) ) ;
#24662 = CARTESIAN_POINT ( 'NONE',  ( -1.187664041994749731, -0.3162353388693405765, 0.4822834645669290543 ) ) ;
#24663 = DIRECTION ( 'NONE',  ( -0.000000000000000000, 1.000000000000000000, -0.000000000000000000 ) ) ;
#24664 = CARTESIAN_POINT ( 'NONE',  ( -1.013282927784338705, 2.320010949979154579E-15, 0.4281993546915509041 ) ) ;
#24665 = VECTOR ( 'NONE', #11329, 39.37007874015748143 ) ;
#24666 = CARTESIAN_POINT ( 'NONE',  ( -0.3149606299212590610, -0.1870078740157480879, -0.4822834645669291653 ) ) ;
#24667 = CARTESIAN_POINT ( 'NONE',  ( -0.8989501312335946848, 0.2952755905511810774, -0.1292274648535930714 ) ) ;
#24668 = ORIENTED_EDGE ( 'NONE', *, *, #51709, .T. ) ;
#24669 = CARTESIAN_POINT ( 'NONE',  ( -0.3996062992125986590, 0.1070741851644051723, -2.156824146981627166 ) ) ;
#24670 = CARTESIAN_POINT ( 'NONE',  ( 1.115485564304462551, 0.05413385826771666132, 0.4176697321401328100 ) ) ;
#24671 = CARTESIAN_POINT ( 'NONE',  ( -0.5774278215223089816, 0.1283753931104746893, -0.1820866141732285504 ) ) ;
#24672 = CARTESIAN_POINT ( 'NONE',  ( -0.6364829396325453192, -0.3162353388693405765, 0.4822834645669290543 ) ) ;
#24673 = CARTESIAN_POINT ( 'NONE',  ( 1.299212598425197429, -0.6692913385826771977, 8.415575281601705876E-17 ) ) ;
#24674 = CARTESIAN_POINT ( 'NONE',  ( 1.017060367454068803, -0.3162353388693405765, 0.4822834645669290543 ) ) ;
#24675 = CARTESIAN_POINT ( 'NONE',  ( 1.509186351706037543, -0.4281496062992127816, -0.4176697321401328100 ) ) ;
#24676 = CARTESIAN_POINT ( 'NONE',  ( -1.049868766404198794, 0.1283753931104746893, -0.1820866141732285504 ) ) ;
#24677 = CARTESIAN_POINT ( 'NONE',  ( 4.893765752498283308E-17, -0.3996062992125985480, -0.7854330708661416693 ) ) ;
#24678 = CARTESIAN_POINT ( 'NONE',  ( -0.2925321140481932924, 0.2925321140481931814, -0.8070866141732284671 ) ) ;
#24679 = AXIS2_PLACEMENT_3D ( 'NONE', #43838, #64044, #11889 ) ;
#24680 = CARTESIAN_POINT ( 'NONE',  ( -0.1058382717557503211, 0.3949938075777409408, -0.3215223097112862027 ) ) ;
#24681 = CARTESIAN_POINT ( 'NONE',  ( 0.3841287887292355596, 0.08106202739151233128, -1.220472440944881942 ) ) ;
#24682 = CARTESIAN_POINT ( 'NONE',  ( 1.272965879265092637, -0.3690944881889765550, -0.3153832671262227771 ) ) ;
#24683 = CARTESIAN_POINT ( 'NONE',  ( 0.7152230971128614723, -0.2845877964562161244, -0.3641732283464567121 ) ) ;
#24684 = CARTESIAN_POINT ( 'NONE',  ( 0.6233595800524939223, -0.3162353388693405765, 0.4822834645669290543 ) ) ;
#24685 = CARTESIAN_POINT ( 'NONE',  ( 1.528871391076116026, -0.6692913385826773087, -0.1292274648535924053 ) ) ;
#24686 = CARTESIAN_POINT ( 'NONE',  ( 0.2891555358219910499, -0.2891555358219909944, -1.435039370078739829 ) ) ;
#24687 = CARTESIAN_POINT ( 'NONE',  ( 0.9448818897637802916, -0.1870078740157480601, -0.3641732283464567677 ) ) ;
#24688 = CARTESIAN_POINT ( 'NONE',  ( -0.3608923884514428360, 0.2952755905511811885, 0.1292274648535926551 ) ) ;
#24689 = CARTESIAN_POINT ( 'NONE',  ( -1.108923884514435132, -0.05778040916215560624, -0.4822834645669293319 ) ) ;
#24690 = CARTESIAN_POINT ( 'NONE',  ( 1.167979002624672580, -0.4281496062992124485, 0.4176697321401328655 ) ) ;
#24691 = CARTESIAN_POINT ( 'NONE',  ( 0.1265901696524989462, 0.4724409448818897572, -1.725721784776903078 ) ) ;
#24692 = CARTESIAN_POINT ( 'NONE',  ( -0.1070741851644051862, -0.3996062992125986590, -2.591863517060367439 ) ) ;
#24693 = CARTESIAN_POINT ( 'NONE',  ( -0.04593175853018302557, -0.5511811023622048555, -0.09757992244046775898 ) ) ;
#24694 = EDGE_LOOP ( 'NONE', ( #14261, #2708, #54030, #7106 ) ) ;
#24695 = ORIENTED_EDGE ( 'NONE', *, *, #11333, .T. ) ;
#24696 = CARTESIAN_POINT ( 'NONE',  ( -0.8070866141732276899, -0.5400638737290844871, 0.3530559997133364547 ) ) ;
#24697 = CARTESIAN_POINT ( 'NONE',  ( -0.7939632545931750718, -0.05778040916215560624, -0.4822834645669293319 ) ) ;
#24698 = CARTESIAN_POINT ( 'NONE',  ( -0.1837270341207340729, 0.2306618581243847221, -0.2411417322834647770 ) ) ;
#24699 = CARTESIAN_POINT ( 'NONE',  ( 0.4855643044619430415, -0.4281496062992127816, -0.4176697321401328100 ) ) ;
#24700 = CARTESIAN_POINT ( 'NONE',  ( -0.3215223097112853146, -0.05778040916215560624, -0.4822834645669293319 ) ) ;
#24701 = CARTESIAN_POINT ( 'NONE',  ( -1.358267716535432434, -0.5400638737290844871, 0.3530559997133364547 ) ) ;
#24702 = CARTESIAN_POINT ( 'NONE',  ( -0.7939632545931754048, -0.3162353388693405765, 0.4822834645669290543 ) ) ;
#24703 = CARTESIAN_POINT ( 'NONE',  ( 0.7874015748031503170, -0.1870078740157479769, 0.4822834645669291653 ) ) ;
#24704 = EDGE_CURVE ( 'NONE', #20803, #19838, #57125, .T. ) ;
#24705 = CARTESIAN_POINT ( 'NONE',  ( -0.3917322834645671215, 0.1049643490035301469, -1.284776902887139194 ) ) ;
#24706 = CARTESIAN_POINT ( 'NONE',  ( -0.4790026246719152336, -0.08942795157528024563, -0.3641732283464568787 ) ) ;
#24707 = VERTEX_POINT ( 'NONE', #49995 ) ;
#24708 = CARTESIAN_POINT ( 'NONE',  ( 0.2891555358219910499, -0.2891555358219909944, -1.358267716535433101 ) ) ;
#24709 = ORIENTED_EDGE ( 'NONE', *, *, #44487, .T. ) ;
#24710 = CARTESIAN_POINT ( 'NONE',  ( -1.266404199475064773, -0.2845877964562159024, 0.3641732283464567677 ) ) ;
#24711 = CARTESIAN_POINT ( 'NONE',  ( -0.8989501312335946848, -0.6692913385826771977, 0.1292274648535927661 ) ) ;
#24712 = CARTESIAN_POINT ( 'NONE',  ( -0.6955380577427815458, 0.05413385826771666132, 0.4176697321401328100 ) ) ;
#24713 = CARTESIAN_POINT ( 'NONE',  ( -0.1070741851644056997, 0.3996062992125986035, -0.1640419947506561726 ) ) ;
#24714 = CARTESIAN_POINT ( 'NONE',  ( -0.9317585301837263412, 0.05413385826771666132, 0.4176697321401328100 ) ) ;
#24715 = CARTESIAN_POINT ( 'NONE',  ( -0.6299212598425188991, -0.1870078740157479769, 0.4822834645669291653 ) ) ;
#24716 = CARTESIAN_POINT ( 'NONE',  ( -1.627296587926508442, 0.2306618581243848609, 0.2411417322834645549 ) ) ;
#24717 = CARTESIAN_POINT ( 'NONE',  ( -1.686351706036744558, 0.2952755905511810774, -0.1292274648535930714 ) ) ;
#24718 = CARTESIAN_POINT ( 'NONE',  ( 0.4068241469816281097, -0.004921259842519576551, 0.3153832671262227771 ) ) ;
#24719 = CARTESIAN_POINT ( 'NONE',  ( 0.000000000000000000, 2.755905511811024056, 0.000000000000000000 ) ) ;
#24720 = CARTESIAN_POINT ( 'NONE',  ( 4.797336870675656522E-17, -0.3917322834645670104, -0.005905511811023714773 ) ) ;
#24721 = CARTESIAN_POINT ( 'NONE',  ( 0.09186351706036799403, -0.3690944881889765550, -0.3153832671262227771 ) ) ;
#24722 = AXIS2_PLACEMENT_3D ( 'NONE', #1323, #28221, #59790 ) ;
#24723 = CARTESIAN_POINT ( 'NONE',  ( -0.5118110236220466680, 0.2952755905511811885, 0.000000000000000000 ) ) ;
#24724 = CARTESIAN_POINT ( 'NONE',  ( 1.338582677165355062, -0.1870078740157480879, -0.4822834645669291653 ) ) ;
#24725 = CARTESIAN_POINT ( 'NONE',  ( -0.1377952755905504645, -0.5400638737290845981, -0.3530559997133363437 ) ) ;
#24726 = ORIENTED_EDGE ( 'NONE', *, *, #7531, .T. ) ;
#24727 = CARTESIAN_POINT ( 'NONE',  ( -0.3460692066303960868, 0.1998031496062990242, -2.073490813648294129 ) ) ;
#24728 = CARTESIAN_POINT ( 'NONE',  ( -0.8533690079452078692, 0.004960608223778821026, 0.3437734562760189072 ) ) ;
#24729 = ORIENTED_EDGE ( 'NONE', *, *, #19143, .T. ) ;
#24730 = CARTESIAN_POINT ( 'NONE',  ( -0.3996062992125984925, -0.1070741851644056858, -1.382545931758530022 ) ) ;
#24731 = CARTESIAN_POINT ( 'NONE',  ( 1.122047244094488860, 0.1660481256975885056, 0.3530559997133364547 ) ) ;
#24732 = CARTESIAN_POINT ( 'NONE',  ( -1.102362204724408601, -0.1870078740157479769, 0.3641732283464567677 ) ) ;
#24733 = CARTESIAN_POINT ( 'NONE',  ( -1.587926509186350810, -0.4281496062992124485, 0.4176697321401328655 ) ) ;
#24734 = CARTESIAN_POINT ( 'NONE',  ( 0.3458507752293908943, -0.3458507752293908943, -1.043307086614173151 ) ) ;
#24735 = DIRECTION ( 'NONE',  ( 0.000000000000000000, 0.000000000000000000, -1.000000000000000000 ) ) ;
#24736 = CARTESIAN_POINT ( 'NONE',  ( -0.3392501089628019995, 0.1958661417322832277, -0.01837270341207344546 ) ) ;
#24737 = CARTESIAN_POINT ( 'NONE',  ( 1.397637795275591177, 0.1660481256975883668, -0.3530559997133364547 ) ) ;
#24738 = CARTESIAN_POINT ( 'NONE',  ( -0.2867679344610366554, 0.2867679344610365444, -1.994094488188976388 ) ) ;
#24739 = CARTESIAN_POINT ( 'NONE',  ( 0.2690288713910767848, 0.2952755905511811885, 0.1292274648535926551 ) ) ;
#24740 = CARTESIAN_POINT ( 'NONE',  ( -1.279527559055116948, 0.07958543189024071263, -0.2665933059059888421 ) ) ;
#24741 = CARTESIAN_POINT ( 'NONE',  ( -0.3543307086614165824, -0.6692913385826771977, 8.415575281601705876E-17 ) ) ;
#24742 = CARTESIAN_POINT ( 'NONE',  ( 4.893765752498283308E-17, -0.3996062992125985480, 0.1594488188976377896 ) ) ;
#24743 = CARTESIAN_POINT ( 'NONE',  ( -1.069553805774277722, 0.2952755905511811885, 0.1292274648535926551 ) ) ;
#24744 = AXIS2_PLACEMENT_3D ( 'NONE', #44138, #17274, #4609 ) ;
#24745 = CARTESIAN_POINT ( 'NONE',  ( -0.1974969037888706924, 0.3420746716998658843, -2.452099737532808632 ) ) ;
#24746 = CARTESIAN_POINT ( 'NONE',  ( 1.174540682414699111, -0.08942795157528024563, -0.3641732283464568787 ) ) ;
#24747 = CARTESIAN_POINT ( 'NONE',  ( -0.4133858267716528645, 0.07958543189024071263, -0.2665933059059888421 ) ) ;
#24748 = CARTESIAN_POINT ( 'NONE',  ( 0.7808398950131241190, -0.08942795157528024563, -0.3641732283464568787 ) ) ;
#24749 = CARTESIAN_POINT ( 'NONE',  ( -1.423884514435694859, -0.3162353388693405765, 0.4822834645669290543 ) ) ;
#24750 = CARTESIAN_POINT ( 'NONE',  ( 0.6299212598425204535, -0.1870078740157480601, -0.3641732283464567677 ) ) ;
#24751 = CARTESIAN_POINT ( 'NONE',  ( -0.7874015748031489847, -0.1870078740157480879, -0.4822834645669291653 ) ) ;
#24752 = CARTESIAN_POINT ( 'NONE',  ( 0.4177787735907000366, 0.3937007874015747699, -1.757006255033530806 ) ) ;
#24753 = CARTESIAN_POINT ( 'NONE',  ( 0.09186351706036827158, -0.004921259842519576551, 0.3153832671262227771 ) ) ;
#24754 = CARTESIAN_POINT ( 'NONE',  ( 0.000000000000000000, 0.000000000000000000, -2.755905511811024056 ) ) ;
#24755 = CARTESIAN_POINT ( 'NONE',  ( 0.6955380577427828781, -0.4281496062992124485, 0.4176697321401328655 ) ) ;
#24756 = CYLINDRICAL_SURFACE ( 'NONE', #15614, 0.4724409448818898682 ) ;
#24757 = CARTESIAN_POINT ( 'NONE',  ( 1.581364829396326277, -0.08942795157527998196, 0.3641732283464567121 ) ) ;
#24758 = CARTESIAN_POINT ( 'NONE',  ( -1.161417322834644716, -0.5400638737290845981, -0.3530559997133363437 ) ) ;
#24759 = CARTESIAN_POINT ( 'NONE',  ( -0.4133858267716528645, -0.4536011799217367080, 0.2665933059059888421 ) ) ;
#24760 = CARTESIAN_POINT ( 'NONE',  ( -3.224202737261815166, 2.716535433070866645, 0.5314960629921260393 ) ) ;
#24761 = CARTESIAN_POINT ( 'NONE',  ( 0.06561679790026316017, -0.004921259842519870586, -0.3153832671262229437 ) ) ;
#24762 = CARTESIAN_POINT ( 'NONE',  ( -1.299212598425196097, -0.6692913385826771977, 8.415575281601705876E-17 ) ) ;
#24763 = CARTESIAN_POINT ( 'NONE',  ( -0.6561679790026240244, 0.2306618581243847221, -0.2411417322834647770 ) ) ;
#24764 = CARTESIAN_POINT ( 'NONE',  ( -0.3996062992125984925, -0.1070741851644056858, -0.9101049868766404316 ) ) ;
#24765 = CARTESIAN_POINT ( 'NONE',  ( -9.594673741351313045E-17, 0.3917322834645670104, -2.131889763779527769 ) ) ;
#24766 = CARTESIAN_POINT ( 'NONE',  ( 0.6299212598425204535, -0.1870078740157479769, 0.3641732283464567677 ) ) ;
#24767 = CARTESIAN_POINT ( 'NONE',  ( -0.2952755905511803003, -0.5400638737290845981, -0.3530559997133363437 ) ) ;
#24768 = CARTESIAN_POINT ( 'NONE',  ( -0.8661417322834640276, -0.1870078740157479769, 0.4822834645669291653 ) ) ;
#24769 = CARTESIAN_POINT ( 'NONE',  ( -0.7808398950131222316, -0.2845877964562161244, -0.3641732283464567121 ) ) ;
#24770 = CARTESIAN_POINT ( 'NONE',  ( -3.927306557984919344, 1.151598356332751871, 0.2765182861327670771 ) ) ;
#24771 = CARTESIAN_POINT ( 'NONE',  ( -0.09842519685039295696, -0.5400638737290844871, 0.3530559997133364547 ) ) ;
#24772 = CARTESIAN_POINT ( 'NONE',  ( 1.114781747626347963, 3.405574981839577511E-16, 0.3464511005275203726 ) ) ;
#24773 = CARTESIAN_POINT ( 'NONE',  ( -1.646981627296586703, -0.05778040916215522460, 0.4822834645669289988 ) ) ;
#24774 = DIRECTION ( 'NONE',  ( 0.000000000000000000, 1.000000000000000000, 0.000000000000000000 ) ) ;
#24775 = ORIENTED_EDGE ( 'NONE', *, *, #73731, .F. ) ;
#24776 = CIRCLE ( 'NONE', #47626, 1.220472440944881942 ) ;
#24777 = CARTESIAN_POINT ( 'NONE',  ( -1.646051170424378096, 0.000000000000000000, 0.3464511005275205946 ) ) ;
#24778 = CARTESIAN_POINT ( 'NONE',  ( -1.489501312335957062, -0.3162353388693409650, -0.4822834645669289433 ) ) ;
#24779 = CARTESIAN_POINT ( 'NONE',  ( -1.010498687664041384, -0.4281496062992127816, -0.4176697321401328100 ) ) ;
#24780 = CARTESIAN_POINT ( 'NONE',  ( -1.463254593175852492, 0.2952755905511811885, 0.1292274648535926551 ) ) ;
#24781 = CARTESIAN_POINT ( 'NONE',  ( 0.1049643490035303689, 0.3917322834645670104, -1.967847769028871374 ) ) ;
#24782 = FACE_OUTER_BOUND ( 'NONE', #38069, .T. ) ;
#24783 = CARTESIAN_POINT ( 'NONE',  ( 0.7677165354330716118, 0.1660481256975883668, -0.3530559997133364547 ) ) ;
#24784 = CARTESIAN_POINT ( 'NONE',  ( 0.2230971128608932319, -0.4281496062992124485, 0.4176697321401328655 ) ) ;
#24785 = CARTESIAN_POINT ( 'NONE',  ( -0.4724409448818904234, 0.1265901696524979470, -0.5052493438320210251 ) ) ;
#24786 = CARTESIAN_POINT ( 'NONE',  ( -0.6889763779527551257, 0.1660481256975885056, 0.3530559997133364547 ) ) ;
#24787 = CARTESIAN_POINT ( 'NONE',  ( 1.246719160104987623, -0.3690944881889763329, 0.3153832671262228327 ) ) ;
#24788 = CARTESIAN_POINT ( 'NONE',  ( 0.3460692066303959757, -0.1998031496062991907, -0.7349081364829396223 ) ) ;
#24789 = EDGE_LOOP ( 'NONE', ( #23812, #28647, #66413, #44058 ) ) ;
#24791 = CARTESIAN_POINT ( 'NONE',  ( 0.3917322834645670104, 2.398668435337828261E-17, -2.787401574803149096 ) ) ;
#24790 = CIRCLE ( 'NONE', #70458, 0.3149606299212598381 ) ;
#24792 = VERTEX_POINT ( 'NONE', #37379 ) ;
#24793 = CARTESIAN_POINT ( 'NONE',  ( 0.2755905511811031494, -0.6692913385826771977, 8.415575281601705876E-17 ) ) ;
#24794 = CARTESIAN_POINT ( 'NONE',  ( -0.7874015748031489847, -0.1870078740157479769, 0.4822834645669291653 ) ) ;
#24795 = CARTESIAN_POINT ( 'NONE',  ( -1.515748031496062076, -0.5400638737290844871, 0.3530559997133364547 ) ) ;
#24796 = CARTESIAN_POINT ( 'NONE',  ( 0.7349081364829403995, 0.2306618581243848609, 0.2411417322834645549 ) ) ;
#24797 = CARTESIAN_POINT ( 'NONE',  ( 1.496062992125985147, -0.1870078740157479769, 0.4822834645669291653 ) ) ;
#24798 = CARTESIAN_POINT ( 'NONE',  ( 1.561679790026247350, -0.4281496062992124485, 0.4176697321401328655 ) ) ;
#24799 = CARTESIAN_POINT ( 'NONE',  ( -0.2755905511811015396, -0.6692913385826771977, 8.415575281601705876E-17 ) ) ;
#24800 = CARTESIAN_POINT ( 'NONE',  ( -1.076115485564303809, -0.6046776061558809534, -0.2411417322834644161 ) ) ;
#24801 = CARTESIAN_POINT ( 'NONE',  ( 0.3492006680983059663, 0.3045572308828553565, -0.01849200668098333403 ) ) ;
#24802 = CARTESIAN_POINT ( 'NONE',  ( 1.456692913385827515, -0.6692913385826771977, 8.415575281601705876E-17 ) ) ;
#24803 =( BOUNDED_SURFACE ( )  B_SPLINE_SURFACE ( 1, 2, ( 
 ( #2520, #79136, #28178, #8825, #9247, #54670, #21862, #59744, #40395, #22282, #8003, #35328, #29004, #67324, #78715, #2098, #54253, #79969, #60991, #33667, #27763, #47110, #47527, #73218, #1685, #15568, #53428, #41228, #66077, #80381, #47942, #3340, #65676, #66915, #59329, #28596, #8413, #73645, #39986, #72800, #22694, #27344, #14328, #53002, #21040, #15149, #72392, #40806, #56325, #37391, #68965, #74050, #36973, #18046, #55489, #82024, #4571, #49183, #48769, #61405, #50007, #68151, #62233, #35737, #81199, #48353, #74886, #75292, #29826, #43267, #3754, #74468, #30242, #23101, #10896, #55905, #23514, #17232, #75705, #69382, #11736, #82429, #68555, #42044, #42862, #36149, #62653, #36556, #29418, #11314, #43679, #4994, #63063, #5400, #31063, #61821, #55077, #81617, #80785, #30662, #23931, #16815, #24337, #56731, #16398, #67740, #42451, #49598, #17635, #4161, #10073, #10495, #58395, #58823, #69792, #44099, #44914, #70192, #13382, #45342, #82835, #12547, #44502, #57968, #57555, #25569, #20109, #76115, #51648, #38205, #12138, #63879, #335, #70611, #83246, #63472, #25157, #39035, #19261, #24748, #6635, #18855, #37794, #5807, #13803, #64718, #71038, #51234, #31477, #77776, #50415, #18456, #12966, #57138, #19684, #50825, #32307, #76527, #39461, #7059, #755, #32728, #25990, #45757, #6218, #76933, #65148, #31894, #38623, #26416, #52069, #77352, #71454, #7484, #64301, #33154, #20942, #34400, #15470, #65573, #66818, #47010, #47427, #28079, #7907, #27246, #46600, #73119, #40707, #72704, #52905, #60481, #65979, #53329, #46180, #72296, #59645, #66392, #8730, #14226, #15051, #8316, #2423, #78619, #41540, #2832, #54153, #78197, #60068, #20528, #53737, #14642, #9151, #52489, #33983, #79445, #71877, #79868, #33568, #67229, #40298, #21357, #59230, #34824, #73548, #21764, #26831, #41127, #22185, #2001, #28493, #47842, #27663, #1591, #39886, #15891, #79038, #9559, #35229, #1180, #60893, #4064, #29731, #36055, #17538, #49083, #43583, #28908, #54571, #11631, #10398, #80285, #74783, #3661, #56228, #41944, #17134, #81511, #43170, #42766, #68051, #10800, #23833, #36875, #67640, #81100, #24237, #61303, #61727, #29324, #36460, #68866, #48673, #55393, #35643, #3244, #42353, #11215, #80693, #9973, #55805, #81926, #62553, #62134, #68462, #49910, #49501, #23417, #30562, #4888, #75607, #54985, #17946, #4474, #30144, #75194, #23006, #69284, #22598, #48259, #16302, #73955, #74369, #16713, #44398, #25466, #31790, #57865, #20003, #51132, #82733, #63368, #70937, #56630, #650, #77673, #32622, #44000, #25052, #19577, #45237, #26307, #77248, #64614, #38520, #76014, #71349, #13282, #76826, #70090, #19159, #57453, #232, #45654, #44809, #50727, #5702, #38934, #82331, #51965, #37291, #58284, #69693, #76426, #6952, #62966, #5304, #24649, #18754, #12444, #70505, #12863, #50317, #64203, #38103, #6537, #31374, #30963, #18356, #12036, #37693, #32207, #57039, #25883, #63779, #6118, #83146, #51544, #53219, #58710, #66711, #78091, #54048, #39773, #33878, #46075, #21662, #2727, #34299, #39352, #2316, #9044, #20838, #47322, #78929, #14543, #14121, #26728, #15364, #33467, #27560, #1075, #46490, #13696, #40195, #65878, #72185, #53634, #1899, #79762, #65036, #7372, #47738, #8213, #33041, #21251, #65468, #34719, #20422, #46906, #59960, #79342, #72601, #59544, #14947, #27976, #73013, #71768, #40606, #60379, #7802, #66289, #59129, #8628, #41025, #1486, #28388, #27140, #52382, #78514, #22079, #52804, #80182, #68369, #68770, #30043, #23317, #55294, #62447, #62038, #35959, #43073, #17443, #81413, #73855, #55705, #48986, #29633, #81003, #48160, #28805, #74685, #48570, #29223, #17031, #4783, #23730, #24139, #35123, #9452, #10292, #35539, #4375, #10707, #16196, #61201, #9870, #42670, #22903, #74268, #11114, #41438, #36363, #3558, #60789, #54890, #49401, #61628, #16611, #54469, #41842, #75095, #67949, #73436, #36771, #67532, #3142, #22497, #30459, #56123, #81829, #42254, #80595, #15786, #67122, #3970, #12350, #37187, #44713, #30867, #31693, #18255, #64518, #12766, #25787, #64105, #57352, #70841, #24554, #24952, #38839 ),
 ( #56532, #70410, #45137, #6440, #83048, #25371, #6855, #38423, #38006, #19484, #77152, #57770, #50220, #32112, #51034, #6022, #76733, #75916, #132, #13190, #19065, #5203, #557, #51449, #63684, #56942, #32525, #44304, #58188, #49809, #75510, #11940, #43897, #17849, #69179, #43483, #11530, #62866, #82235, #37595, #69594, #63268, #5609, #31277, #82639, #50625, #76330, #18660, #69995, #15582, #8839, #28608, #21466, #34515, #79562, #28191, #54266, #60180, #22294, #64938, #53441, #41240, #2112, #73231, #66928, #2533, #53849, #29018, #48365, #74064, #61417, #47541, #19910, #21876, #15163, #16000, #9260, #7278, #47955, #22707, #41647, #16410, #42056, #67752, #40820, #13602, #34932, #34094, #9671, #60595, #27777, #73658, #10086, #61004, #26210, #59757, #79981, #2944, #66505, #67338, #35751, #3353, #51872, #71256, #45560, #35341, #72814, #54684, #80395, #79149, #77578, #47124, #39256, #36565, #4580, #82437, #55089, #30673, #23524, #74480, #49194, #36984, #49606, #62242, #42463, #4173, #75714, #81628, #3767, #68974, #81209, #48782, #16827, #76123, #18055, #50016, #30251, #68163, #56740, #29431, #80798, #75301, #10506, #82033, #36159, #11324, #55500, #18465, #43688, #63073, #69393, #62663, #24755, #61833, #55915, #44108, #29837, #10907, #11745, #37401, #56334, #24347, #5410, #74895, #23939, #17243, #5003, #31072, #42872, #50423, #17645, #69800, #12147, #68565, #43277, #37804, #23115, #19695, #26001, #6229, #39472, #57147, #14237, #12977, #82846, #51659, #31904, #58833, #44513, #77363, #765, #45767, #45352, #70621, #13393, #26427, #65159, #70201, #345, #26840, #63890, #38633, #57565, #39046, #71466, #51243, #64311, #38215, #63482, #44924, #13814, #83257, #12556, #58406, #1191, #20120, #64731, #71049, #52499, #52079, #7069, #33165, #7496, #78208, #25579, #20540, #32738, #77787, #46191, #76945, #71887, #5815, #31486, #18864, #25167, #50836, #76536, #6645, #19271, #57980, #32318, #22608, #28091, #2012, #65990, #73557, #59241, #3254, #80294, #35239, #46611, #27676, #22195, #47853, #28916, #1600, #53341, #15062, #21775, #15901, #20954, #27256, #41550, #39896, #78630, #41138, #40718, #79050, #79458, #54584, #67238, #73966, #52915, #72307, #60080, #21368, #28506, #60492, #14654, #47023, #59656, #73130, #72715, #66403, #60903, #7917, #66828, #8741, #40311, #34412, #15481, #2434, #53748, #8328, #33994, #54163, #47437, #65584, #9161, #34833, #2842, #79877, #48268, #9568, #33578, #74796, #54994, #69294, #50326, #49919, #30153, #23427, #4485, #10809, #36885, #82340, #55815, #61736, #42364, #75617, #35652, #62975, #56639, #11643, #23016, #4073, #81935, #24246, #5314, #61315, #29740, #17143, #37301, #48683, #67649, #36064, #81110, #17547, #10407, #24658, #17955, #30972, #9985, #81523, #3670, #23843, #68063, #43592, #29333, #49092, #49510, #80702, #16311, #74379, #41955, #55404, #36469, #16722, #42775, #68471, #62562, #62144, #4901, #75203, #43179, #68876, #11225, #30572, #56238, #5713, #77683, #12453, #6546, #63377, #25475, #76024, #19170, #44818, #51142, #32633, #64212, #58723, #44009, #69703, #26738, #76836, #12046, #32217, #18764, #71360, #57048, #57875, #13291, #58296, #242, #83156, #25894, #38943, #51978, #82742, #12872, #39362, #76435, #70515, #44407, #51554, #661, #63788, #38531, #50737, #18369, #57462, #26317, #38114, #25063, #70946, #13708, #20013, #77257, #19587, #65047, #64626, #45249, #45664, #7384, #33052, #70101, #1086, #6962, #37704, #31383, #6127, #31802, #79773, #53646, #7812, #9462, #65889, #39785, #59971, #33478, #34730, #2330, #60390, #59140, #65480, #2740, #52392, #1498, #79354, #27571, #8224, #8638, #41449, #28400, #3152, #14132, #71778, #72611, #14554, #41035, #73024, #27150, #40206, #72201, #27986, #1909, #53229, #47749, #20432, #21673, #33888, #52814, #59554, #47334, #14959, #78945, #78525, #20848, #66721, #46918, #78101, #34309, #46501, #21263, #40616, #67133, #9058, #15374, #66299, #54058, #22089, #46086, #73448, #15798, #35136, #60798, #9880, #10718, #80604, #43495, #75108, #4794, #43084, #36375, #49821, #3567, #3980, #17860, #35549, #35969 ) ),
 .UNSPECIFIED., .F., .F., .F. ) 
 B_SPLINE_SURFACE_WITH_KNOTS ( ( 2, 2 ),
 ( 3, 2, 2, 2, 2, 2, 2, 2, 2, 2, 2, 2, 2, 2, 2, 2, 2, 2, 2, 2, 2, 2, 2, 2, 2, 2, 2, 2, 2, 2, 2, 2, 2, 2, 2, 2, 2, 2, 2, 2, 2, 2, 2, 2, 2, 2, 2, 2, 2, 2, 2, 2, 2, 2, 2, 2, 2, 2, 2, 2, 2, 2, 2, 2, 2, 2, 2, 2, 2, 2, 2, 2, 2, 2, 2, 2, 2, 2, 2, 2, 2, 2, 2, 2, 2, 2, 2, 2, 2, 2, 2, 2, 2, 2, 2, 2, 2, 2, 2, 2, 2, 2, 2, 2, 2, 2, 2, 2, 2, 2, 2, 2, 2, 2, 2, 2, 2, 2, 2, 2, 2, 2, 2, 2, 2, 2, 2, 2, 2, 2, 2, 2, 2, 2, 2, 2, 2, 2, 2, 2, 2, 2, 2, 2, 2, 2, 2, 2, 2, 2, 2, 2, 2, 2, 2, 2, 2, 2, 2, 2, 2, 2, 2, 2, 2, 2, 2, 2, 2, 2, 2, 2, 2, 2, 2, 2, 2, 2, 2, 2, 2, 2, 2, 2, 2, 2, 2, 2, 2, 2, 2, 2, 2, 2, 2, 2, 2, 2, 2, 2, 2, 2, 2, 2, 2, 2, 2, 2, 2, 2, 2, 2, 2, 2, 2, 2, 2, 2, 2, 2, 2, 2, 2, 2, 2, 2, 2, 2, 2, 2, 2, 2, 2, 2, 2, 2, 2, 2, 2, 2, 2, 2, 2, 2, 2, 2, 2, 2, 2, 2, 2, 2, 2, 2, 2, 3 ),
 ( 0.000000000000000000, 1.000000000000000000 ),
 ( 0.000000000000000000, 0.003787878787878787984, 0.007575757575757575968, 0.01136363636363636395, 0.01515151515151515194, 0.01893939393939393992, 0.02272727272727272790, 0.02651515151515151589, 0.03030303030303030387, 0.03409090909090908839, 0.03787878787878787984, 0.04166666666666666435, 0.04545454545454545581, 0.04924242424242424032, 0.05303030303030303177, 0.05681818181818181629, 0.06060606060606060774, 0.06439393939393939226, 0.06818181818181817677, 0.07196969696969697516, 0.07575757575757575968, 0.07954545454545454419, 0.08333333333333332871, 0.08712121212121212710, 0.09090909090909091161, 0.09469696969696969613, 0.09848484848484848064, 0.1022727272727272790, 0.1060606060606060635, 0.1098484848484848481, 0.1136363636363636326, 0.1174242424242424310, 0.1212121212121212155, 0.1250000000000000000, 0.1287878787878787845, 0.1325757575757575690, 0.1363636363636363535, 0.1401515151515151381, 0.1439393939393939503, 0.1477272727272727348, 0.1515151515151515194, 0.1553030303030303039, 0.1590909090909090884, 0.1628787878787878729, 0.1666666666666666574, 0.1704545454545454419, 0.1742424242424242542, 0.1780303030303030387, 0.1818181818181818232, 0.1856060606060606077, 0.1893939393939393923, 0.1931818181818181768, 0.1969696969696969613, 0.2007575757575757458, 0.2045454545454545581, 0.2083333333333333426, 0.2121212121212121271, 0.2159090909090909116, 0.2196969696969696961, 0.2234848484848484806, 0.2272727272727272652, 0.2310606060606060497, 0.2348484848484848619, 0.2386363636363636465, 0.2424242424242424310, 0.2462121212121212155, 0.2500000000000000000, 0.2537878787878787845, 0.2575757575757575690, 0.2613636363636363535, 0.2651515151515151381, 0.2689393939393939226, 0.2727272727272727071, 0.2765151515151514916, 0.2803030303030302761, 0.2840909090909091161, 0.2878787878787879007, 0.2916666666666666852, 0.2954545454545454697, 0.2992424242424242542, 0.3030303030303030387, 0.3068181818181818232, 0.3106060606060606077, 0.3143939393939393923, 0.3181818181818181768, 0.3219696969696969613, 0.3257575757575757458, 0.3295454545454545303, 0.3333333333333333148, 0.3371212121212120993, 0.3409090909090908839, 0.3446969696969697239, 0.3484848484848485084, 0.3522727272727272929, 0.3560606060606060774, 0.3598484848484848619, 0.3636363636363636465, 0.3674242424242424310, 0.3712121212121212155, 0.3750000000000000000, 0.3787878787878787845, 0.3825757575757575690, 0.3863636363636363535, 0.3901515151515151381, 0.3939393939393939226, 0.3977272727272727071, 0.4015151515151514916, 0.4053030303030302761, 0.4090909090909091161, 0.4128787878787879007, 0.4166666666666666852, 0.4204545454545454697, 0.4242424242424242542, 0.4280303030303030387, 0.4318181818181818232, 0.4356060606060606077, 0.4393939393939393923, 0.4431818181818181768, 0.4469696969696969613, 0.4507575757575757458, 0.4545454545454545303, 0.4583333333333333148, 0.4621212121212120993, 0.4659090909090908839, 0.4696969696969697239, 0.4734848484848485084, 0.4772727272727272929, 0.4810606060606060774, 0.4848484848484848619, 0.4886363636363636465, 0.4924242424242424310, 0.4962121212121212155, 0.5000000000000000000, 0.5037878787878787845, 0.5075757575757575690, 0.5113636363636363535, 0.5151515151515151381, 0.5189393939393939226, 0.5227272727272727071, 0.5265151515151514916, 0.5303030303030302761, 0.5340909090909090606, 0.5378787878787878451, 0.5416666666666666297, 0.5454545454545454142, 0.5492424242424241987, 0.5530303030303029832, 0.5568181818181817677, 0.5606060606060605522, 0.5643939393939394478, 0.5681818181818182323, 0.5719696969696970168, 0.5757575757575758013, 0.5795454545454545858, 0.5833333333333333703, 0.5871212121212121549, 0.5909090909090909394, 0.5946969696969697239, 0.5984848484848485084, 0.6022727272727272929, 0.6060606060606060774, 0.6098484848484848619, 0.6136363636363636465, 0.6174242424242424310, 0.6212121212121212155, 0.6250000000000000000, 0.6287878787878787845, 0.6325757575757575690, 0.6363636363636363535, 0.6401515151515151381, 0.6439393939393939226, 0.6477272727272727071, 0.6515151515151514916, 0.6553030303030302761, 0.6590909090909090606, 0.6628787878787878451, 0.6666666666666666297, 0.6704545454545454142, 0.6742424242424241987, 0.6780303030303029832, 0.6818181818181817677, 0.6856060606060605522, 0.6893939393939394478, 0.6931818181818182323, 0.6969696969696970168, 0.7007575757575758013, 0.7045454545454545858, 0.7083333333333333703, 0.7121212121212121549, 0.7159090909090909394, 0.7196969696969697239, 0.7234848484848485084, 0.7272727272727272929, 0.7310606060606060774, 0.7348484848484848619, 0.7386363636363636465, 0.7424242424242424310, 0.7462121212121212155, 0.7500000000000000000, 0.7537878787878787845, 0.7575757575757575690, 0.7613636363636363535, 0.7651515151515151381, 0.7689393939393939226, 0.7727272727272727071, 0.7765151515151514916, 0.7803030303030302761, 0.7840909090909090606, 0.7878787878787878451, 0.7916666666666666297, 0.7954545454545454142, 0.7992424242424241987, 0.8030303030303029832, 0.8068181818181817677, 0.8106060606060605522, 0.8143939393939394478, 0.8181818181818182323, 0.8219696969696970168, 0.8257575757575758013, 0.8295454545454545858, 0.8333333333333333703, 0.8371212121212121549, 0.8409090909090909394, 0.8446969696969697239, 0.8484848484848485084, 0.8522727272727272929, 0.8560606060606060774, 0.8598484848484848619, 0.8636363636363636465, 0.8674242424242424310, 0.8712121212121212155, 0.8750000000000000000, 0.8787878787878787845, 0.8825757575757575690, 0.8863636363636363535, 0.8901515151515151381, 0.8939393939393939226, 0.8977272727272727071, 0.9015151515151514916, 0.9053030303030302761, 0.9090909090909090606, 0.9128787878787878451, 0.9166666666666666297, 0.9204545454545454142, 0.9242424242424241987, 0.9280303030303029832, 0.9318181818181817677, 0.9356060606060605522, 0.9393939393939394478, 0.9431818181818182323, 0.9469696969696970168, 0.9507575757575758013, 0.9545454545454545858, 0.9583333333333333703, 0.9621212121212121549, 0.9659090909090909394 ),
 .UNSPECIFIED. ) 
 GEOMETRIC_REPRESENTATION_ITEM ( )  RATIONAL_B_SPLINE_SURFACE ( (
 ( 1.000000000000000000, 0.9659258262890683122, 1.000000000000000000, 0.9659258262890683122, 1.000000000000000000, 0.9659258262890683122, 1.000000000000000000, 0.9659258262890683122, 1.000000000000000000, 0.9659258262890683122, 1.000000000000000000, 0.9659258262890683122, 1.000000000000000000, 0.9659258262890683122, 1.000000000000000000, 0.9659258262890683122, 1.000000000000000000, 0.9659258262890683122, 1.000000000000000000, 0.9659258262890683122, 1.000000000000000000, 0.9659258262890683122, 1.000000000000000000, 0.9659258262890683122, 1.000000000000000000, 0.9659258262890683122, 1.000000000000000000, 0.9659258262890683122, 1.000000000000000000, 0.9659258262890683122, 1.000000000000000000, 0.9659258262890683122, 1.000000000000000000, 0.9659258262890683122, 1.000000000000000000, 0.9659258262890683122, 1.000000000000000000, 0.9659258262890683122, 1.000000000000000000, 0.9659258262890683122, 1.000000000000000000, 0.9659258262890683122, 1.000000000000000000, 0.9659258262890683122, 1.000000000000000000, 0.9659258262890683122, 1.000000000000000000, 0.9659258262890683122, 1.000000000000000000, 0.9659258262890683122, 1.000000000000000000, 0.9659258262890683122, 1.000000000000000000, 0.9659258262890683122, 1.000000000000000000, 0.9659258262890683122, 1.000000000000000000, 0.9659258262890683122, 1.000000000000000000, 0.9659258262890683122, 1.000000000000000000, 0.9659258262890683122, 1.000000000000000000, 0.9659258262890683122, 1.000000000000000000, 0.9659258262890683122, 1.000000000000000000, 0.9659258262890683122, 1.000000000000000000, 0.9659258262890683122, 1.000000000000000000, 0.9659258262890683122, 1.000000000000000000, 0.9659258262890683122, 1.000000000000000000, 0.9659258262890683122, 1.000000000000000000, 0.9659258262890683122, 1.000000000000000000, 0.9659258262890683122, 1.000000000000000000, 0.9659258262890683122, 1.000000000000000000, 0.9659258262890683122, 1.000000000000000000, 0.9659258262890683122, 1.000000000000000000, 0.9659258262890683122, 1.000000000000000000, 0.9659258262890683122, 1.000000000000000000, 0.9659258262890683122, 1.000000000000000000, 0.9659258262890683122, 1.000000000000000000, 0.9659258262890683122, 1.000000000000000000, 0.9659258262890683122, 1.000000000000000000, 0.9659258262890683122, 1.000000000000000000, 0.9659258262890683122, 1.000000000000000000, 0.9659258262890683122, 1.000000000000000000, 0.9659258262890683122, 1.000000000000000000, 0.9659258262890683122, 1.000000000000000000, 0.9659258262890683122, 1.000000000000000000, 0.9659258262890683122, 1.000000000000000000, 0.9659258262890683122, 1.000000000000000000, 0.9659258262890683122, 1.000000000000000000, 0.9659258262890683122, 1.000000000000000000, 0.9659258262890683122, 1.000000000000000000, 0.9659258262890683122, 1.000000000000000000, 0.9659258262890683122, 1.000000000000000000, 0.9659258262890683122, 1.000000000000000000, 0.9659258262890683122, 1.000000000000000000, 0.9659258262890683122, 1.000000000000000000, 0.9659258262890683122, 1.000000000000000000, 0.9659258262890683122, 1.000000000000000000, 0.9659258262890683122, 1.000000000000000000, 0.9659258262890683122, 1.000000000000000000, 0.9659258262890683122, 1.000000000000000000, 0.9659258262890683122, 1.000000000000000000, 0.9659258262890683122, 1.000000000000000000, 0.9659258262890683122, 1.000000000000000000, 0.9659258262890683122, 1.000000000000000000, 0.9659258262890683122, 1.000000000000000000, 0.9659258262890683122, 1.000000000000000000, 0.9659258262890683122, 1.000000000000000000, 0.9659258262890683122, 1.000000000000000000, 0.9659258262890683122, 1.000000000000000000, 0.9659258262890683122, 1.000000000000000000, 0.9659258262890683122, 1.000000000000000000, 0.9659258262890683122, 1.000000000000000000, 0.9659258262890683122, 1.000000000000000000, 0.9659258262890683122, 1.000000000000000000, 0.9659258262890683122, 1.000000000000000000, 0.9659258262890683122, 1.000000000000000000, 0.9659258262890683122, 1.000000000000000000, 0.9659258262890683122, 1.000000000000000000, 0.9659258262890683122, 1.000000000000000000, 0.9659258262890683122, 1.000000000000000000, 0.9659258262890683122, 1.000000000000000000, 0.9659258262890683122, 1.000000000000000000, 0.9659258262890683122, 1.000000000000000000, 0.9659258262890683122, 1.000000000000000000, 0.9659258262890683122, 1.000000000000000000, 0.9659258262890683122, 1.000000000000000000, 0.9659258262890683122, 1.000000000000000000, 0.9659258262890683122, 1.000000000000000000, 0.9659258262890683122, 1.000000000000000000, 0.9659258262890683122, 1.000000000000000000, 0.9659258262890683122, 1.000000000000000000, 0.9659258262890683122, 1.000000000000000000, 0.9659258262890683122, 1.000000000000000000, 0.9659258262890683122, 1.000000000000000000, 0.9659258262890683122, 1.000000000000000000, 0.9659258262890683122, 1.000000000000000000, 0.9659258262890683122, 1.000000000000000000, 0.9659258262890683122, 1.000000000000000000, 0.9659258262890683122, 1.000000000000000000, 0.9659258262890683122, 1.000000000000000000, 0.9659258262890683122, 1.000000000000000000, 0.9659258262890683122, 1.000000000000000000, 0.9659258262890683122, 1.000000000000000000, 0.9659258262890683122, 1.000000000000000000, 0.9659258262890683122, 1.000000000000000000, 0.9659258262890683122, 1.000000000000000000, 0.9659258262890683122, 1.000000000000000000, 0.9659258262890683122, 1.000000000000000000, 0.9659258262890683122, 1.000000000000000000, 0.9659258262890683122, 1.000000000000000000, 0.9659258262890683122, 1.000000000000000000, 0.9659258262890683122, 1.000000000000000000, 0.9659258262890683122, 1.000000000000000000, 0.9659258262890683122, 1.000000000000000000, 0.9659258262890683122, 1.000000000000000000, 0.9659258262890683122, 1.000000000000000000, 0.9659258262890683122, 1.000000000000000000, 0.9659258262890683122, 1.000000000000000000, 0.9659258262890683122, 1.000000000000000000, 0.9659258262890683122, 1.000000000000000000, 0.9659258262890683122, 1.000000000000000000, 0.9659258262890683122, 1.000000000000000000, 0.9659258262890683122, 1.000000000000000000, 0.9659258262890683122, 1.000000000000000000, 0.9659258262890683122, 1.000000000000000000, 0.9659258262890683122, 1.000000000000000000, 0.9659258262890683122, 1.000000000000000000, 0.9659258262890683122, 1.000000000000000000, 0.9659258262890683122, 1.000000000000000000, 0.9659258262890683122, 1.000000000000000000, 0.9659258262890683122, 1.000000000000000000, 0.9659258262890683122, 1.000000000000000000, 0.9659258262890683122, 1.000000000000000000, 0.9659258262890683122, 1.000000000000000000, 0.9659258262890683122, 1.000000000000000000, 0.9659258262890683122, 1.000000000000000000, 0.9659258262890683122, 1.000000000000000000, 0.9659258262890683122, 1.000000000000000000, 0.9659258262890683122, 1.000000000000000000, 0.9659258262890683122, 1.000000000000000000, 0.9659258262890683122, 1.000000000000000000, 0.9659258262890683122, 1.000000000000000000, 0.9659258262890683122, 1.000000000000000000, 0.9659258262890683122, 1.000000000000000000, 0.9659258262890683122, 1.000000000000000000, 0.9659258262890683122, 1.000000000000000000, 0.9659258262890683122, 1.000000000000000000, 0.9659258262890683122, 1.000000000000000000, 0.9659258262890683122, 1.000000000000000000, 0.9659258262890683122, 1.000000000000000000, 0.9659258262890683122, 1.000000000000000000, 0.9659258262890683122, 1.000000000000000000, 0.9659258262890683122, 1.000000000000000000, 0.9659258262890683122, 1.000000000000000000, 0.9659258262890683122, 1.000000000000000000, 0.9659258262890683122, 1.000000000000000000, 0.9659258262890683122, 1.000000000000000000, 0.9659258262890683122, 1.000000000000000000, 0.9659258262890683122, 1.000000000000000000, 0.9659258262890683122, 1.000000000000000000, 0.9659258262890683122, 1.000000000000000000, 0.9659258262890683122, 1.000000000000000000, 0.9659258262890683122, 1.000000000000000000, 0.9659258262890683122, 1.000000000000000000, 0.9659258262890683122, 1.000000000000000000, 0.9659258262890683122, 1.000000000000000000, 0.9659258262890683122, 1.000000000000000000, 0.9659258262890683122, 1.000000000000000000, 0.9659258262890683122, 1.000000000000000000, 0.9659258262890683122, 1.000000000000000000, 0.9659258262890683122, 1.000000000000000000, 0.9659258262890683122, 1.000000000000000000, 0.9659258262890683122, 1.000000000000000000, 0.9659258262890683122, 1.000000000000000000, 0.9659258262890683122, 1.000000000000000000, 0.9659258262890683122, 1.000000000000000000, 0.9659258262890683122, 1.000000000000000000, 0.9659258262890683122, 1.000000000000000000, 0.9659258262890683122, 1.000000000000000000, 0.9659258262890683122, 1.000000000000000000, 0.9659258262890683122, 1.000000000000000000, 0.9659258262890683122, 1.000000000000000000, 0.9659258262890683122, 1.000000000000000000, 0.9659258262890683122, 1.000000000000000000, 0.9659258262890683122, 1.000000000000000000, 0.9659258262890683122, 1.000000000000000000, 0.9659258262890683122, 1.000000000000000000, 0.9659258262890683122, 1.000000000000000000, 0.9659258262890683122, 1.000000000000000000, 0.9659258262890683122, 1.000000000000000000, 0.9659258262890683122, 1.000000000000000000, 0.9659258262890683122, 1.000000000000000000, 0.9659258262890683122, 1.000000000000000000, 0.9659258262890683122, 1.000000000000000000, 0.9659258262890683122, 1.000000000000000000, 0.9659258262890683122, 1.000000000000000000, 0.9659258262890683122, 1.000000000000000000, 0.9659258262890683122, 1.000000000000000000, 0.9659258262890683122, 1.000000000000000000, 0.9659258262890683122, 1.000000000000000000, 0.9659258262890683122, 1.000000000000000000, 0.9659258262890683122, 1.000000000000000000, 0.9659258262890683122, 1.000000000000000000, 0.9659258262890683122, 1.000000000000000000, 0.9659258262890683122, 1.000000000000000000, 0.9659258262890683122, 1.000000000000000000, 0.9659258262890683122, 1.000000000000000000, 0.9659258262890683122, 1.000000000000000000, 0.9659258262890683122, 1.000000000000000000, 0.9659258262890683122, 1.000000000000000000, 0.9659258262890683122, 1.000000000000000000, 0.9659258262890683122, 1.000000000000000000, 0.9659258262890683122, 1.000000000000000000, 0.9659258262890683122, 1.000000000000000000, 0.9659258262890683122, 1.000000000000000000, 0.9659258262890683122, 1.000000000000000000, 0.9659258262890683122, 1.000000000000000000, 0.9659258262890683122, 1.000000000000000000, 0.9659258262890683122, 1.000000000000000000, 0.9659258262890683122, 1.000000000000000000, 0.9659258262890683122, 1.000000000000000000, 0.9659258262890683122, 1.000000000000000000, 0.9659258262890683122, 1.000000000000000000, 0.9659258262890683122, 1.000000000000000000, 0.9659258262890683122, 1.000000000000000000, 0.9659258262890683122, 1.000000000000000000, 0.9659258262890683122, 1.000000000000000000, 0.9659258262890683122, 1.000000000000000000, 0.9659258262890683122, 1.000000000000000000, 0.9659258262890683122, 1.000000000000000000, 0.9659258262890683122, 1.000000000000000000, 0.9659258262890683122, 1.000000000000000000, 0.9659258262890683122, 1.000000000000000000, 0.9659258262890683122, 1.000000000000000000, 0.9659258262890683122, 1.000000000000000000, 0.9659258262890683122, 1.000000000000000000, 0.9659258262890683122, 1.000000000000000000, 0.9659258262890683122, 1.000000000000000000, 0.9659258262890683122, 1.000000000000000000, 0.9659258262890683122, 1.000000000000000000, 0.9659258262890683122, 1.000000000000000000, 0.9659258262890683122, 1.000000000000000000, 0.9659258262890683122, 1.000000000000000000, 0.9659258262890683122, 1.000000000000000000, 0.9659258262890683122, 1.000000000000000000),
 ( 1.000000000000000000, 0.9659258262890683122, 1.000000000000000000, 0.9659258262890683122, 1.000000000000000000, 0.9659258262890683122, 1.000000000000000000, 0.9659258262890683122, 1.000000000000000000, 0.9659258262890683122, 1.000000000000000000, 0.9659258262890683122, 1.000000000000000000, 0.9659258262890683122, 1.000000000000000000, 0.9659258262890683122, 1.000000000000000000, 0.9659258262890683122, 1.000000000000000000, 0.9659258262890683122, 1.000000000000000000, 0.9659258262890683122, 1.000000000000000000, 0.9659258262890683122, 1.000000000000000000, 0.9659258262890683122, 1.000000000000000000, 0.9659258262890683122, 1.000000000000000000, 0.9659258262890683122, 1.000000000000000000, 0.9659258262890683122, 1.000000000000000000, 0.9659258262890683122, 1.000000000000000000, 0.9659258262890683122, 1.000000000000000000, 0.9659258262890683122, 1.000000000000000000, 0.9659258262890683122, 1.000000000000000000, 0.9659258262890683122, 1.000000000000000000, 0.9659258262890683122, 1.000000000000000000, 0.9659258262890683122, 1.000000000000000000, 0.9659258262890683122, 1.000000000000000000, 0.9659258262890683122, 1.000000000000000000, 0.9659258262890683122, 1.000000000000000000, 0.9659258262890683122, 1.000000000000000000, 0.9659258262890683122, 1.000000000000000000, 0.9659258262890683122, 1.000000000000000000, 0.9659258262890683122, 1.000000000000000000, 0.9659258262890683122, 1.000000000000000000, 0.9659258262890683122, 1.000000000000000000, 0.9659258262890683122, 1.000000000000000000, 0.9659258262890683122, 1.000000000000000000, 0.9659258262890683122, 1.000000000000000000, 0.9659258262890683122, 1.000000000000000000, 0.9659258262890683122, 1.000000000000000000, 0.9659258262890683122, 1.000000000000000000, 0.9659258262890683122, 1.000000000000000000, 0.9659258262890683122, 1.000000000000000000, 0.9659258262890683122, 1.000000000000000000, 0.9659258262890683122, 1.000000000000000000, 0.9659258262890683122, 1.000000000000000000, 0.9659258262890683122, 1.000000000000000000, 0.9659258262890683122, 1.000000000000000000, 0.9659258262890683122, 1.000000000000000000, 0.9659258262890683122, 1.000000000000000000, 0.9659258262890683122, 1.000000000000000000, 0.9659258262890683122, 1.000000000000000000, 0.9659258262890683122, 1.000000000000000000, 0.9659258262890683122, 1.000000000000000000, 0.9659258262890683122, 1.000000000000000000, 0.9659258262890683122, 1.000000000000000000, 0.9659258262890683122, 1.000000000000000000, 0.9659258262890683122, 1.000000000000000000, 0.9659258262890683122, 1.000000000000000000, 0.9659258262890683122, 1.000000000000000000, 0.9659258262890683122, 1.000000000000000000, 0.9659258262890683122, 1.000000000000000000, 0.9659258262890683122, 1.000000000000000000, 0.9659258262890683122, 1.000000000000000000, 0.9659258262890683122, 1.000000000000000000, 0.9659258262890683122, 1.000000000000000000, 0.9659258262890683122, 1.000000000000000000, 0.9659258262890683122, 1.000000000000000000, 0.9659258262890683122, 1.000000000000000000, 0.9659258262890683122, 1.000000000000000000, 0.9659258262890683122, 1.000000000000000000, 0.9659258262890683122, 1.000000000000000000, 0.9659258262890683122, 1.000000000000000000, 0.9659258262890683122, 1.000000000000000000, 0.9659258262890683122, 1.000000000000000000, 0.9659258262890683122, 1.000000000000000000, 0.9659258262890683122, 1.000000000000000000, 0.9659258262890683122, 1.000000000000000000, 0.9659258262890683122, 1.000000000000000000, 0.9659258262890683122, 1.000000000000000000, 0.9659258262890683122, 1.000000000000000000, 0.9659258262890683122, 1.000000000000000000, 0.9659258262890683122, 1.000000000000000000, 0.9659258262890683122, 1.000000000000000000, 0.9659258262890683122, 1.000000000000000000, 0.9659258262890683122, 1.000000000000000000, 0.9659258262890683122, 1.000000000000000000, 0.9659258262890683122, 1.000000000000000000, 0.9659258262890683122, 1.000000000000000000, 0.9659258262890683122, 1.000000000000000000, 0.9659258262890683122, 1.000000000000000000, 0.9659258262890683122, 1.000000000000000000, 0.9659258262890683122, 1.000000000000000000, 0.9659258262890683122, 1.000000000000000000, 0.9659258262890683122, 1.000000000000000000, 0.9659258262890683122, 1.000000000000000000, 0.9659258262890683122, 1.000000000000000000, 0.9659258262890683122, 1.000000000000000000, 0.9659258262890683122, 1.000000000000000000, 0.9659258262890683122, 1.000000000000000000, 0.9659258262890683122, 1.000000000000000000, 0.9659258262890683122, 1.000000000000000000, 0.9659258262890683122, 1.000000000000000000, 0.9659258262890683122, 1.000000000000000000, 0.9659258262890683122, 1.000000000000000000, 0.9659258262890683122, 1.000000000000000000, 0.9659258262890683122, 1.000000000000000000, 0.9659258262890683122, 1.000000000000000000, 0.9659258262890683122, 1.000000000000000000, 0.9659258262890683122, 1.000000000000000000, 0.9659258262890683122, 1.000000000000000000, 0.9659258262890683122, 1.000000000000000000, 0.9659258262890683122, 1.000000000000000000, 0.9659258262890683122, 1.000000000000000000, 0.9659258262890683122, 1.000000000000000000, 0.9659258262890683122, 1.000000000000000000, 0.9659258262890683122, 1.000000000000000000, 0.9659258262890683122, 1.000000000000000000, 0.9659258262890683122, 1.000000000000000000, 0.9659258262890683122, 1.000000000000000000, 0.9659258262890683122, 1.000000000000000000, 0.9659258262890683122, 1.000000000000000000, 0.9659258262890683122, 1.000000000000000000, 0.9659258262890683122, 1.000000000000000000, 0.9659258262890683122, 1.000000000000000000, 0.9659258262890683122, 1.000000000000000000, 0.9659258262890683122, 1.000000000000000000, 0.9659258262890683122, 1.000000000000000000, 0.9659258262890683122, 1.000000000000000000, 0.9659258262890683122, 1.000000000000000000, 0.9659258262890683122, 1.000000000000000000, 0.9659258262890683122, 1.000000000000000000, 0.9659258262890683122, 1.000000000000000000, 0.9659258262890683122, 1.000000000000000000, 0.9659258262890683122, 1.000000000000000000, 0.9659258262890683122, 1.000000000000000000, 0.9659258262890683122, 1.000000000000000000, 0.9659258262890683122, 1.000000000000000000, 0.9659258262890683122, 1.000000000000000000, 0.9659258262890683122, 1.000000000000000000, 0.9659258262890683122, 1.000000000000000000, 0.9659258262890683122, 1.000000000000000000, 0.9659258262890683122, 1.000000000000000000, 0.9659258262890683122, 1.000000000000000000, 0.9659258262890683122, 1.000000000000000000, 0.9659258262890683122, 1.000000000000000000, 0.9659258262890683122, 1.000000000000000000, 0.9659258262890683122, 1.000000000000000000, 0.9659258262890683122, 1.000000000000000000, 0.9659258262890683122, 1.000000000000000000, 0.9659258262890683122, 1.000000000000000000, 0.9659258262890683122, 1.000000000000000000, 0.9659258262890683122, 1.000000000000000000, 0.9659258262890683122, 1.000000000000000000, 0.9659258262890683122, 1.000000000000000000, 0.9659258262890683122, 1.000000000000000000, 0.9659258262890683122, 1.000000000000000000, 0.9659258262890683122, 1.000000000000000000, 0.9659258262890683122, 1.000000000000000000, 0.9659258262890683122, 1.000000000000000000, 0.9659258262890683122, 1.000000000000000000, 0.9659258262890683122, 1.000000000000000000, 0.9659258262890683122, 1.000000000000000000, 0.9659258262890683122, 1.000000000000000000, 0.9659258262890683122, 1.000000000000000000, 0.9659258262890683122, 1.000000000000000000, 0.9659258262890683122, 1.000000000000000000, 0.9659258262890683122, 1.000000000000000000, 0.9659258262890683122, 1.000000000000000000, 0.9659258262890683122, 1.000000000000000000, 0.9659258262890683122, 1.000000000000000000, 0.9659258262890683122, 1.000000000000000000, 0.9659258262890683122, 1.000000000000000000, 0.9659258262890683122, 1.000000000000000000, 0.9659258262890683122, 1.000000000000000000, 0.9659258262890683122, 1.000000000000000000, 0.9659258262890683122, 1.000000000000000000, 0.9659258262890683122, 1.000000000000000000, 0.9659258262890683122, 1.000000000000000000, 0.9659258262890683122, 1.000000000000000000, 0.9659258262890683122, 1.000000000000000000, 0.9659258262890683122, 1.000000000000000000, 0.9659258262890683122, 1.000000000000000000, 0.9659258262890683122, 1.000000000000000000, 0.9659258262890683122, 1.000000000000000000, 0.9659258262890683122, 1.000000000000000000, 0.9659258262890683122, 1.000000000000000000, 0.9659258262890683122, 1.000000000000000000, 0.9659258262890683122, 1.000000000000000000, 0.9659258262890683122, 1.000000000000000000, 0.9659258262890683122, 1.000000000000000000, 0.9659258262890683122, 1.000000000000000000, 0.9659258262890683122, 1.000000000000000000, 0.9659258262890683122, 1.000000000000000000, 0.9659258262890683122, 1.000000000000000000, 0.9659258262890683122, 1.000000000000000000, 0.9659258262890683122, 1.000000000000000000, 0.9659258262890683122, 1.000000000000000000, 0.9659258262890683122, 1.000000000000000000, 0.9659258262890683122, 1.000000000000000000, 0.9659258262890683122, 1.000000000000000000, 0.9659258262890683122, 1.000000000000000000, 0.9659258262890683122, 1.000000000000000000, 0.9659258262890683122, 1.000000000000000000, 0.9659258262890683122, 1.000000000000000000, 0.9659258262890683122, 1.000000000000000000, 0.9659258262890683122, 1.000000000000000000, 0.9659258262890683122, 1.000000000000000000, 0.9659258262890683122, 1.000000000000000000, 0.9659258262890683122, 1.000000000000000000, 0.9659258262890683122, 1.000000000000000000, 0.9659258262890683122, 1.000000000000000000, 0.9659258262890683122, 1.000000000000000000, 0.9659258262890683122, 1.000000000000000000, 0.9659258262890683122, 1.000000000000000000, 0.9659258262890683122, 1.000000000000000000, 0.9659258262890683122, 1.000000000000000000, 0.9659258262890683122, 1.000000000000000000, 0.9659258262890683122, 1.000000000000000000, 0.9659258262890683122, 1.000000000000000000, 0.9659258262890683122, 1.000000000000000000, 0.9659258262890683122, 1.000000000000000000, 0.9659258262890683122, 1.000000000000000000, 0.9659258262890683122, 1.000000000000000000, 0.9659258262890683122, 1.000000000000000000, 0.9659258262890683122, 1.000000000000000000, 0.9659258262890683122, 1.000000000000000000, 0.9659258262890683122, 1.000000000000000000, 0.9659258262890683122, 1.000000000000000000, 0.9659258262890683122, 1.000000000000000000, 0.9659258262890683122, 1.000000000000000000, 0.9659258262890683122, 1.000000000000000000, 0.9659258262890683122, 1.000000000000000000, 0.9659258262890683122, 1.000000000000000000, 0.9659258262890683122, 1.000000000000000000, 0.9659258262890683122, 1.000000000000000000, 0.9659258262890683122, 1.000000000000000000, 0.9659258262890683122, 1.000000000000000000, 0.9659258262890683122, 1.000000000000000000, 0.9659258262890683122, 1.000000000000000000, 0.9659258262890683122, 1.000000000000000000, 0.9659258262890683122, 1.000000000000000000, 0.9659258262890683122, 1.000000000000000000, 0.9659258262890683122, 1.000000000000000000, 0.9659258262890683122, 1.000000000000000000, 0.9659258262890683122, 1.000000000000000000, 0.9659258262890683122, 1.000000000000000000, 0.9659258262890683122, 1.000000000000000000, 0.9659258262890683122, 1.000000000000000000, 0.9659258262890683122, 1.000000000000000000, 0.9659258262890683122, 1.000000000000000000, 0.9659258262890683122, 1.000000000000000000, 0.9659258262890683122, 1.000000000000000000, 0.9659258262890683122, 1.000000000000000000, 0.9659258262890683122, 1.000000000000000000, 0.9659258262890683122, 1.000000000000000000, 0.9659258262890683122, 1.000000000000000000, 0.9659258262890683122, 1.000000000000000000) ) ) 
 REPRESENTATION_ITEM ( '' )  SURFACE ( )  );
#24804 = CARTESIAN_POINT ( 'NONE',  ( 0.1958661417322836440, -0.3392501089628017219, -2.696194225721784576 ) ) ;
#24805 = CARTESIAN_POINT ( 'NONE',  ( 0.7152230971128616943, -0.08942795157527998196, 0.3641732283464567121 ) ) ;
#24806 = VERTEX_POINT ( 'NONE', #50812 ) ;
#24807 = CARTESIAN_POINT ( 'NONE',  ( 4.837279021331060870E-17, -0.3949938075777409963, -0.2362204724409449619 ) ) ;
#24808 = VERTEX_POINT ( 'NONE', #82819 ) ;
#24809 = CARTESIAN_POINT ( 'NONE',  ( -0.1049868766404193215, 0.1283753931104746893, -0.1820866141732285504 ) ) ;
#24810 = CARTESIAN_POINT ( 'NONE',  ( 2.776658174029195347, 1.170105060311650069, -0.3006284332565901662 ) ) ;
#24811 = CARTESIAN_POINT ( 'NONE',  ( 0.7545931758530188826, -0.6692913385826771977, 0.1292274648535927661 ) ) ;
#24812 = CARTESIAN_POINT ( 'NONE',  ( 0.2427821522309716595, -0.3162353388693409650, -0.4822834645669289433 ) ) ;
#24813 = CARTESIAN_POINT ( 'NONE',  ( -0.5774278215223089816, 0.2306618581243847221, -0.2411417322834647770 ) ) ;
#24814 = CARTESIAN_POINT ( 'NONE',  ( -0.3917322834645671770, 0.1049643490035302024, -1.761830339403886336 ) ) ;
#24815 = CARTESIAN_POINT ( 'NONE',  ( -1.220472440944881054, -0.6692913385826771977, 8.415575281601705876E-17 ) ) ;
#24816 = CARTESIAN_POINT ( 'NONE',  ( -0.3917322834645669549, -0.1049643490035306603, -2.492782152230970993 ) ) ;
#24817 = CARTESIAN_POINT ( 'NONE',  ( 1.338582677165355062, -0.1870078740157480601, -0.3641732283464567677 ) ) ;
#24818 = CARTESIAN_POINT ( 'NONE',  ( -1.509186351706035767, -0.4281496062992124485, 0.4176697321401328655 ) ) ;
#24819 = CARTESIAN_POINT ( 'NONE',  ( 0.8989501312335964611, 0.2952755905511811885, 0.1292274648535926551 ) ) ;
#24820 = CARTESIAN_POINT ( 'NONE',  ( 1.154855643044620184, -0.6046776061558807314, 0.2411417322834647770 ) ) ;
#24821 = CARTESIAN_POINT ( 'NONE',  ( 0.1998031496062994405, -0.3460692066303958092, -0.8792650918635170898 ) ) ;
#24822 = CARTESIAN_POINT ( 'NONE',  ( -1.345144356955379816, -0.05778040916215560624, -0.4822834645669293319 ) ) ;
#24823 = CARTESIAN_POINT ( 'NONE',  ( -9.787531504996566615E-17, 0.3996062992125985480, -0.3917322834645669549 ) ) ;
#24824 = CARTESIAN_POINT ( 'NONE',  ( -0.2624671916010490880, 0.2306618581243847221, -0.2411417322834647770 ) ) ;
#24825 = CARTESIAN_POINT ( 'NONE',  ( -0.3996062992125987146, 0.1070741851644051862, -2.395013123359580387 ) ) ;
#24826 = CARTESIAN_POINT ( 'NONE',  ( -0.3917322834645671215, 0.1049643490035301469, -1.849737532808399143 ) ) ;
#24827 = CARTESIAN_POINT ( 'NONE',  ( 1.377952755905512472, 0.2952755905511811885, 0.000000000000000000 ) ) ;
#24828 = CARTESIAN_POINT ( 'NONE',  ( 0.05905511811023709395, -0.4536011799217367080, 0.2665933059059888421 ) ) ;
#24829 = CARTESIAN_POINT ( 'NONE',  ( 0.7939632545931766261, -0.05778040916215522460, 0.4822834645669289988 ) ) ;
#24830 = CARTESIAN_POINT ( 'NONE',  ( -0.2362204724409447953, -0.4091458600556404646, -0.9297900262467192478 ) ) ;
#24831 = CARTESIAN_POINT ( 'NONE',  ( 0.6496062992125991586, -0.4536011799217368745, -0.2665933059059886201 ) ) ;
#24832 = CARTESIAN_POINT ( 'NONE',  ( 0.2230971128608929543, 0.05413385826771626580, -0.4176697321401330321 ) ) ;
#24833 = CARTESIAN_POINT ( 'NONE',  ( -0.1974969037888706924, 0.3420746716998658843, -1.192257217847769279 ) ) ;
#24834 = CARTESIAN_POINT ( 'NONE',  ( -0.9645669291338575535, -0.5400638737290844871, 0.3530559997133364547 ) ) ;
#24835 = CARTESIAN_POINT ( 'NONE',  ( -0.1902887139107604098, 0.2952755905511810219, -0.1292274648535930437 ) ) ;
#24836 = AXIS2_PLACEMENT_3D ( 'NONE', #62535, #83131, #30949 ) ;
#24837 = CARTESIAN_POINT ( 'NONE',  ( 0.7808398950131240079, -0.2845877964562159024, 0.3641732283464567677 ) ) ;
#24838 = DIRECTION ( 'NONE',  ( 1.000000000000000000, 0.000000000000000000, 0.000000000000000000 ) ) ;
#24840 = ADVANCED_FACE ( 'NONE', ( #81185 ), #18444, .F. ) ;
#24839 = CARTESIAN_POINT ( 'NONE',  ( -0.3871391076115479057, -0.3162353388693409650, -0.4822834645669289433 ) ) ;
#24841 = CARTESIAN_POINT ( 'NONE',  ( 0.1837270341207357105, -0.5023911411419708095, -0.1820866141732282451 ) ) ;
#24842 = CARTESIAN_POINT ( 'NONE',  ( -2.558820304884324326, 1.494558157769224183, 0.4725443725032419939 ) ) ;
#24843 = CARTESIAN_POINT ( 'NONE',  ( -0.1574803149606292529, -0.1870078740157479769, 0.4822834645669291653 ) ) ;
#24844 = CARTESIAN_POINT ( 'NONE',  ( 0.4068241469816279987, -0.3690944881889765550, -0.3153832671262227771 ) ) ;
#24845 = CARTESIAN_POINT ( 'NONE',  ( -0.1998031496062991630, -0.3460692066303959202, -1.874671916010498762 ) ) ;
#24846 = CARTESIAN_POINT ( 'NONE',  ( 0.4330708661417329575, 0.2952755905511811885, 0.000000000000000000 ) ) ;
#24847 = EDGE_CURVE ( 'NONE', #7338, #24368, #72398, .T. ) ;
#24848 = CARTESIAN_POINT ( 'NONE',  ( 1.122047244094488860, -0.4536011799217368745, -0.2665933059059886201 ) ) ;
#24849 = CARTESIAN_POINT ( 'NONE',  ( 0.1690661813110321821, 0.02791078216816225699, 0.4328096321851905293 ) ) ;
#24850 = CARTESIAN_POINT ( 'NONE',  ( -0.5971128608923877978, 0.1771653543307087630, 0.09757992244046791164 ) ) ;
#24851 = CARTESIAN_POINT ( 'NONE',  ( -0.8464566929133852113, -0.4536011799217368745, -0.2665933059059886201 ) ) ;
#24852 = CARTESIAN_POINT ( 'NONE',  ( -0.2755905511811015396, -0.6692913385826771977, 8.415575281601705876E-17 ) ) ;
#24853 = CARTESIAN_POINT ( 'NONE',  ( 0.1115485564304467270, -0.6692913385826773087, -0.1292274648535924053 ) ) ;
#24854 = CARTESIAN_POINT ( 'NONE',  ( 0.9580052493438327987, -0.3690944881889765550, -0.3153832671262227771 ) ) ;
#24855 = CARTESIAN_POINT ( 'NONE',  ( 0.1539095575340513611, 1.088378732996000631, -1.111543816720518274 ) ) ;
#24856 = CARTESIAN_POINT ( 'NONE',  ( 1.568241469816273437, -0.2845877964562159024, 0.3641732283464567677 ) ) ;
#24857 = CARTESIAN_POINT ( 'NONE',  ( 0.6889763779527566800, -0.5400638737290844871, 0.3530559997133364547 ) ) ;
#24858 = EDGE_CURVE ( 'NONE', #36386, #24503, #55891, .T. ) ;
#24859 = CARTESIAN_POINT ( 'NONE',  ( -1.614173228346456712, 1.818966223839196816, -0.1372047244094478091 ) ) ;
#24860 = CARTESIAN_POINT ( 'NONE',  ( -0.2493438320209966919, 0.05413385826771626580, -0.4176697321401330321 ) ) ;
#24861 = CARTESIAN_POINT ( 'NONE',  ( 0.1049643490035304938, -0.3917322834645669549, -1.114829396325459410 ) ) ;
#24862 = CARTESIAN_POINT ( 'NONE',  ( 0.8398950131233602345, -0.6046776061558807314, 0.2411417322834647770 ) ) ;
#24863 = CARTESIAN_POINT ( 'NONE',  ( 0.4133858267716541968, 0.1660481256975885056, 0.3530559997133364547 ) ) ;
#24864 = EDGE_CURVE ( 'NONE', #82812, #1879, #44488, .T. ) ;
#24865 = DIRECTION ( 'NONE',  ( 1.000000000000000000, -0.000000000000000000, -0.000000000000000000 ) ) ;
#24866 = CARTESIAN_POINT ( 'NONE',  ( 0.4855643044619430415, -0.3690944881889765550, -0.3153832671262227771 ) ) ;
#24867 = CARTESIAN_POINT ( 'NONE',  ( 1.076115485564305141, 0.2306618581243847221, -0.2411417322834647770 ) ) ;
#24868 = CARTESIAN_POINT ( 'NONE',  ( -0.3543307086614165824, -0.5511811023622047445, 6.969142054262312111E-17 ) ) ;
#24869 = CARTESIAN_POINT ( 'NONE',  ( -0.3674540682414689785, 0.2306618581243848609, 0.2411417322834645549 ) ) ;
#24870 = CARTESIAN_POINT ( 'NONE',  ( 0.1265901696524990572, -0.4724409448818897017, -2.604986876640420057 ) ) ;
#24871 = CARTESIAN_POINT ( 'NONE',  ( 0.2230971128608929543, 0.05413385826771626580, -0.4176697321401330321 ) ) ;
#24872 = CARTESIAN_POINT ( 'NONE',  ( -0.8727034120734901146, -0.3162353388693405765, 0.4822834645669290543 ) ) ;
#24873 = CARTESIAN_POINT ( 'NONE',  ( -0.6758530183727028406, -0.5511811023622048555, -0.09757992244046775898 ) ) ;
#24874 = CARTESIAN_POINT ( 'NONE',  ( 0.4265091863517067039, -0.6692913385826773087, -0.1292274648535924053 ) ) ;
#24875 = CARTESIAN_POINT ( 'NONE',  ( -1.148293963254592542, -0.6692913385826773087, -0.1292274648535924053 ) ) ;
#24876 = CARTESIAN_POINT ( 'NONE',  ( -0.3149606299212590610, -0.1870078740157480879, -0.4822834645669291653 ) ) ;
#24877 = CARTESIAN_POINT ( 'NONE',  ( 5.785732909357575061E-17, -0.4724409448818898682, -0.5511811023622047445 ) ) ;
#24879 = CARTESIAN_POINT ( 'NONE',  ( 1.522309711286089939, -0.6046776061558809534, -0.2411417322834644161 ) ) ;
#24878 = CARTESIAN_POINT ( 'NONE',  ( -0.9341826970036740674, -2.609244250047836720E-15, 0.4118477457933002461 ) ) ;
#24880 = CARTESIAN_POINT ( 'NONE',  ( 1.633858267716535639, -0.5400638737290844871, 0.3530559997133364547 ) ) ;
#24881 = CARTESIAN_POINT ( 'NONE',  ( 4.797336870675656522E-17, -0.3917322834645670104, -1.960629921259842368 ) ) ;
#24882 = FACE_OUTER_BOUND ( 'NONE', #74316, .T. ) ;
#24883 = CARTESIAN_POINT ( 'NONE',  ( -1.089238845144356427, 0.05413385826771666132, 0.4176697321401328100 ) ) ;
#24884 = CARTESIAN_POINT ( 'NONE',  ( -0.3458507752293909498, 0.3458507752293907833, -0.4921259842519684624 ) ) ;
#24885 = CARTESIAN_POINT ( 'NONE',  ( -0.3420746716998659953, -0.1974969037888706647, -2.572178477690288734 ) ) ;
#24886 = ORIENTED_EDGE ( 'NONE', *, *, #56212, .F. ) ;
#24887 = CARTESIAN_POINT ( 'NONE',  ( 0.1837270341207357105, -0.5023911411419708095, -0.1820866141732282451 ) ) ;
#24888 = CARTESIAN_POINT ( 'NONE',  ( 4.797336870675656522E-17, -0.3917322834645670104, -1.173228346456692828 ) ) ;
#24889 = CARTESIAN_POINT ( 'NONE',  ( 0.5708661417322841158, -0.5400638737290845981, -0.3530559997133363437 ) ) ;
#24890 = CARTESIAN_POINT ( 'NONE',  ( -0.4724409448818899238, 0.1265901696524986686, -2.867454068241469756 ) ) ;
#24891 = LINE ( 'NONE', #76263, #30546 ) ;
#24892 = CARTESIAN_POINT ( 'NONE',  ( -0.4593175853018364174, -0.3690944881889765550, -0.3153832671262227771 ) ) ;
#24893 = CARTESIAN_POINT ( 'NONE',  ( -0.2624671916010490880, 0.2306618581243847221, -0.2411417322834647770 ) ) ;
#24894 = CARTESIAN_POINT ( 'NONE',  ( 1.292650918635171564, -0.6692913385826773087, -0.1292274648535924053 ) ) ;
#24895 = CARTESIAN_POINT ( 'NONE',  ( 0.9580052493438326877, -0.004921259842519576551, 0.3153832671262227771 ) ) ;
#24896 = CARTESIAN_POINT ( 'NONE',  ( 0.1771653543307093182, -0.5400638737290845981, -0.3530559997133363437 ) ) ;
#24897 = CARTESIAN_POINT ( 'NONE',  ( -0.1958661417322836440, 0.3392501089628016664, -0.8805581120396831496 ) ) ;
#24898 = CARTESIAN_POINT ( 'NONE',  ( -0.4986876640419939388, 0.2306618581243847221, -0.2411417322834647770 ) ) ;
#24899 = CARTESIAN_POINT ( 'NONE',  ( -1.312335958005248715, -0.5023911411419708095, -0.1820866141732282451 ) ) ;
#24900 = CARTESIAN_POINT ( 'NONE',  ( -0.4396325459317579898, 0.2952755905511811885, 0.1292274648535926551 ) ) ;
#24901 = CARTESIAN_POINT ( 'NONE',  ( 1.692913385826772421, 0.2952755905511811885, 0.000000000000000000 ) ) ;
#24902 = CARTESIAN_POINT ( 'NONE',  ( 0.6410189441372368124, -2.592014407703319119E-15, 0.3954974714151467952 ) ) ;
#24903 = EDGE_LOOP ( 'NONE', ( #78683, #22872, #46098, #58115 ) ) ;
#24904 = CARTESIAN_POINT ( 'NONE',  ( 0.3392501089628018884, -0.1958661417322833942, -2.148969447015434575 ) ) ;
#24905 = CARTESIAN_POINT ( 'NONE',  ( 0.2296587926509192634, -0.3162353388693405765, 0.4822834645669290543 ) ) ;
#24906 = ORIENTED_EDGE ( 'NONE', *, *, #82137, .T. ) ;
#24907 = AXIS2_PLACEMENT_3D ( 'NONE', #46820, #33379, #72511 ) ;
#24908 = CARTESIAN_POINT ( 'NONE',  ( -0.5511811023622041894, -0.1870078740157480879, -0.4822834645669291653 ) ) ;
#24909 = CARTESIAN_POINT ( 'NONE',  ( -1.358267716535432434, -0.5400638737290844871, 0.3530559997133364547 ) ) ;
#24910 = CARTESIAN_POINT ( 'NONE',  ( 0.7808398950131240079, -0.3162353388693405765, 0.4822834645669290543 ) ) ;
#24911 = CARTESIAN_POINT ( 'NONE',  ( 0.2034120734908144990, -0.6692913385826771977, 0.1292274648535927661 ) ) ;
#24912 = CARTESIAN_POINT ( 'NONE',  ( 0.2867679344610365999, 0.2867679344610365999, -1.324803149606299302 ) ) ;
#24913 = CARTESIAN_POINT ( 'NONE',  ( -0.6364829396325453192, -0.3162353388693405765, 0.4822834645669290543 ) ) ;
#24914 = CARTESIAN_POINT ( 'NONE',  ( -0.2821522309711278487, -0.6692913385826773087, -0.1292274648535924053 ) ) ;
#24915 = CARTESIAN_POINT ( 'NONE',  ( -0.7283464566929126471, -0.5400638737290844871, 0.3530559997133364547 ) ) ;
#24916 = CARTESIAN_POINT ( 'NONE',  ( 0.4855643044619430415, -0.3690944881889765550, -0.3153832671262227771 ) ) ;
#24917 = CARTESIAN_POINT ( 'NONE',  ( -0.2371198560983138193, -0.1759840215932895469, 5.725591907046409190 ) ) ;
#24918 = CARTESIAN_POINT ( 'NONE',  ( -0.2755905511811018171, 0.2952755905511811885, 0.000000000000000000 ) ) ;
#24919 = DIRECTION ( 'NONE',  ( 0.000000000000000000, 0.000000000000000000, 1.000000000000000000 ) ) ;
#24920 = EDGE_CURVE ( 'NONE', #48388, #49969, #74487, .T. ) ;
#24921 = CARTESIAN_POINT ( 'NONE',  ( 1.115485564304462551, 0.05413385826771666132, 0.4176697321401328100 ) ) ;
#24922 = CARTESIAN_POINT ( 'NONE',  ( 0.2867679344610365999, 0.2867679344610365999, -2.807086614173227357 ) ) ;
#24923 = ORIENTED_EDGE ( 'NONE', *, *, #80068, .F. ) ;
#24924 = ORIENTED_EDGE ( 'NONE', *, *, #37615, .T. ) ;
#24925 = CARTESIAN_POINT ( 'NONE',  ( 0.2690288713910767848, 0.2952755905511811885, 0.1292274648535926551 ) ) ;
#24926 = CARTESIAN_POINT ( 'NONE',  ( -0.02624671916010428221, -0.5023911411419708095, 0.1820866141732285504 ) ) ;
#24927 = CARTESIAN_POINT ( 'NONE',  ( 1.653543307086614789, -0.1870078740157479769, 0.3641732283464567677 ) ) ;
#24928 = CARTESIAN_POINT ( 'NONE',  ( -0.1958661417322836718, 0.3392501089628017219, -1.200131233595800540 ) ) ;
#24929 = CARTESIAN_POINT ( 'NONE',  ( -0.4724409448818895907, -0.1265901696524993070, 0.03477690288713909672 ) ) ;
#24930 = CARTESIAN_POINT ( 'NONE',  ( 0.1058382717557500852, -0.3949938075777408852, 0.1528871391076115638 ) ) ;
#24931 = CARTESIAN_POINT ( 'NONE',  ( 0.2559055118110243332, -0.5400638737290845981, -0.3530559997133363437 ) ) ;
#24932 = CARTESIAN_POINT ( 'NONE',  ( -1.200787401574802349, -0.5400638737290844871, 0.3530559997133364547 ) ) ;
#24933 = CARTESIAN_POINT ( 'NONE',  ( -1.141732283464566011, -0.6692913385826771977, 8.415575281601705876E-17 ) ) ;
#24934 = CARTESIAN_POINT ( 'NONE',  ( 0.1574803149606306130, -0.1870078740157479769, 0.4822834645669291653 ) ) ;
#24935 = CARTESIAN_POINT ( 'NONE',  ( 0.9908136482939640111, 0.2952755905511810774, -0.1292274648535930714 ) ) ;
#24936 = CARTESIAN_POINT ( 'NONE',  ( 1.555118110236221041, 0.07958543189024071263, -0.2665933059059888421 ) ) ;
#24937 = CARTESIAN_POINT ( 'NONE',  ( 0.7283464566929143125, 0.07958543189024085140, 0.2665933059059887866 ) ) ;
#24938 = CARTESIAN_POINT ( 'NONE',  ( -0.7283464566929126471, -0.5400638737290844871, 0.3530559997133364547 ) ) ;
#24939 = CARTESIAN_POINT ( 'NONE',  ( -0.1998031496062994405, 0.3460692066303957537, -0.4048556430446194621 ) ) ;
#24940 = CARTESIAN_POINT ( 'NONE',  ( 1.469816272965879911, -0.6046776061558807314, 0.2411417322834647770 ) ) ;
#24941 = CARTESIAN_POINT ( 'NONE',  ( -0.3917322834645669549, -0.1049643490035306603, -0.3530183727034120755 ) ) ;
#24943 = CARTESIAN_POINT ( 'NONE',  ( -6.686372609646914991E-25, 1.062992125984252745, 1.850393700787401619 ) ) ;
#24942 = CARTESIAN_POINT ( 'NONE',  ( 1.312335958005250269, -0.6046776061558807314, 0.2411417322834647770 ) ) ;
#24944 = CARTESIAN_POINT ( 'NONE',  ( -1.719160104986876103, -0.004921259842519576551, 0.3153832671262227771 ) ) ;
#24945 = CARTESIAN_POINT ( 'NONE',  ( -0.01968503937007793844, 0.1660481256975883668, -0.3530559997133364547 ) ) ;
#24946 = CARTESIAN_POINT ( 'NONE',  ( 0.7808398950131240079, -0.2845877964562159024, 0.3641732283464567677 ) ) ;
#24947 = CARTESIAN_POINT ( 'NONE',  ( -1.699475065616797398, 0.1771653543307087630, 0.09757992244046791164 ) ) ;
#24948 = CARTESIAN_POINT ( 'NONE',  ( 1.056430446194226658, 0.2952755905511811885, 0.1292274648535926551 ) ) ;
#24949 = FACE_OUTER_BOUND ( 'NONE', #31355, .T. ) ;
#24950 = CARTESIAN_POINT ( 'NONE',  ( -0.5774278215223089816, 0.1283753931104746893, -0.1820866141732285504 ) ) ;
#24951 = CARTESIAN_POINT ( 'NONE',  ( -0.6102362204724400829, 0.1660481256975885056, 0.3530559997133364547 ) ) ;
#24952 = CARTESIAN_POINT ( 'NONE',  ( -1.646981627296586703, -0.08942795157527998196, 0.3641732283464567121 ) ) ;
#24953 = CARTESIAN_POINT ( 'NONE',  ( -1.286089238845143479, -0.6046776061558807314, 0.2411417322834647770 ) ) ;
#24954 = CARTESIAN_POINT ( 'NONE',  ( 1.187664041994751285, -0.05778040916215522460, 0.4822834645669289988 ) ) ;
#24955 = CARTESIAN_POINT ( 'NONE',  ( 4.797336870675656522E-17, -0.3917322834645670659, -0.7053998932096606778 ) ) ;
#24956 = CARTESIAN_POINT ( 'NONE',  ( -1.364829396325458521, -0.5023911411419708095, 0.1820866141732285504 ) ) ;
#24957 = EDGE_CURVE ( 'NONE', #43450, #49642, #70762, .T. ) ;
#24958 = CARTESIAN_POINT ( 'NONE',  ( 1.024231438423351292, 1.413526771164698159, 0.4582195470708000373 ) ) ;
#24959 = CARTESIAN_POINT ( 'NONE',  ( 1.030183727034121421, -0.3162353388693409650, -0.4822834645669289433 ) ) ;
#24960 = CARTESIAN_POINT ( 'NONE',  ( -0.4724409448818895907, -0.1265901696524993070, -2.327427821522309426 ) ) ;
#24961 = CONICAL_SURFACE ( 'NONE', #69328, 1.968503937007874072, 0.7853981633974500554 ) ;
#24962 = CARTESIAN_POINT ( 'NONE',  ( -1.601049868766403650, -0.6046776061558807314, 0.2411417322834647770 ) ) ;
#24963 = CARTESIAN_POINT ( 'NONE',  ( -1.450131233595799651, 0.1771653543307087075, -0.09757992244046823083 ) ) ;
#24964 = CARTESIAN_POINT ( 'NONE',  ( -1.049868766404198794, 0.1283753931104746893, -0.1820866141732285504 ) ) ;
#24965 = CARTESIAN_POINT ( 'NONE',  ( 1.627296587926509996, -0.5023911411419708095, 0.1820866141732285504 ) ) ;
#24966 = CARTESIAN_POINT ( 'NONE',  ( -0.3477690288713902178, 0.2952755905511810774, -0.1292274648535930714 ) ) ;
#24967 = CARTESIAN_POINT ( 'NONE',  ( 0.1968503937007881344, -0.5511811023622047445, 6.969142054262312111E-17 ) ) ;
#24968 = CARTESIAN_POINT ( 'NONE',  ( -1.482939632545930975, -0.3690944881889765550, -0.3153832671262227771 ) ) ;
#24969 = CARTESIAN_POINT ( 'NONE',  ( 1.266404199475066328, -0.08942795157527998196, 0.3641732283464567121 ) ) ;
#24970 = CARTESIAN_POINT ( 'NONE',  ( 1.030183727034121421, -0.05778040916215522460, 0.4822834645669289988 ) ) ;
#24971 = CARTESIAN_POINT ( 'NONE',  ( 1.423884514435696191, -0.05778040916215522460, 0.4822834645669289988 ) ) ;
#24972 = CARTESIAN_POINT ( 'NONE',  ( -0.01968503937007793844, 0.07958543189024071263, -0.2665933059059888421 ) ) ;
#24973 = CARTESIAN_POINT ( 'NONE',  ( 0.2821522309711292364, 0.2952755905511810774, -0.1292274648535930714 ) ) ;
#24974 = CARTESIAN_POINT ( 'NONE',  ( 0.9251968503937015864, -0.4536011799217367080, 0.2665933059059888421 ) ) ;
#24975 = ORIENTED_EDGE ( 'NONE', *, *, #63009, .F. ) ;
#24976 = CARTESIAN_POINT ( 'NONE',  ( -1.502624671916009680, -0.3162353388693405765, 0.4822834645669290543 ) ) ;
#24977 =( BOUNDED_CURVE ( )  B_SPLINE_CURVE ( 2, ( #10413, #11649, #36070, #30978, #44015, #61742, #4907, #23022, #29746, #68477, #17553, #68882, #75209 ),
 .UNSPECIFIED., .F., .F. ) 
 B_SPLINE_CURVE_WITH_KNOTS ( ( 3, 2, 2, 2, 2, 2, 3 ),
 ( 0.1375000000000000111, 0.1416666666666666630, 0.1458333333333333426, 0.1499999999999999944, 0.1541666666666666741, 0.1583333333333333259, 0.1625000000000000056 ),
 .UNSPECIFIED. ) 
 CURVE ( )  GEOMETRIC_REPRESENTATION_ITEM ( )  RATIONAL_B_SPLINE_CURVE ( ( 1.000000000000000000, 0.9659258262890683122, 1.000000000000000000, 0.9659258262890683122, 1.000000000000000000, 0.9659258262890683122, 1.000000000000000000, 0.9659258262890683122, 1.000000000000000000, 0.9659258262890683122, 1.000000000000000000, 0.9659258262890683122, 1.000000000000000000 ) ) 
 REPRESENTATION_ITEM ( '' )  );
#24978 = CARTESIAN_POINT ( 'NONE',  ( -1.318897637795274802, 0.1660481256975885056, 0.3530559997133364547 ) ) ;
#24979 = CARTESIAN_POINT ( 'NONE',  ( 0.05249343832021075018, 0.2306618581243847221, -0.2411417322834647770 ) ) ;
#24980 = CARTESIAN_POINT ( 'NONE',  ( -0.3460692066303960868, 0.1998031496062990242, -0.1837270341207349333 ) ) ;
#24981 = CARTESIAN_POINT ( 'NONE',  ( -0.2925321140481930149, -0.2925321140481933480, -2.812992125984251857 ) ) ;
#24982 = CARTESIAN_POINT ( 'NONE',  ( 0.5446194225721792126, -0.05778040916215560624, -0.4822834645669293319 ) ) ;
#24983 = CARTESIAN_POINT ( 'NONE',  ( 0.9973753280839902091, 0.1283753931104746893, -0.1820866141732285504 ) ) ;
#24984 = CARTESIAN_POINT ( 'NONE',  ( -0.4133858267716528645, -0.5400638737290844871, 0.3530559997133364547 ) ) ;
#24985 = CARTESIAN_POINT ( 'NONE',  ( 0.5052493438320215802, 0.2952755905511811885, 0.1292274648535926551 ) ) ;
#24986 = EDGE_CURVE ( 'NONE', #30946, #8463, #70179, .T. ) ;
#24987 = CARTESIAN_POINT ( 'NONE',  ( 0.1998031496062994405, -0.3460692066303958092, -2.139107611548556331 ) ) ;
#24988 = CARTESIAN_POINT ( 'NONE',  ( -0.2891555358219908833, -0.2891555358219912164, -1.633858267716535195 ) ) ;
#24989 = CARTESIAN_POINT ( 'NONE',  ( 0.3996062992125986590, -0.1070741851644053111, -2.946194225721785465 ) ) ;
#24990 = CARTESIAN_POINT ( 'NONE',  ( 0.3249695492770460770, 1.223219560026271499E-15, 0.4445507791589056734 ) ) ;
#24991 = CARTESIAN_POINT ( 'NONE',  ( -0.1049643490035301885, -0.3917322834645671215, -0.5367454068241467313 ) ) ;
#24992 = EDGE_CURVE ( 'NONE', #3121, #76416, #31762, .T. ) ;
#24993 = CARTESIAN_POINT ( 'NONE',  ( -0.6692913385826764205, -0.5511811023622047445, 6.969142054262312111E-17 ) ) ;
#24994 = CARTESIAN_POINT ( 'NONE',  ( -0.6824146981627291497, -0.6046776061558809534, -0.2411417322834644161 ) ) ;
#24995 = CARTESIAN_POINT ( 'NONE',  ( 0.1058382717557499880, 0.3949938075777409408, -2.432414698162729927 ) ) ;
#24996 = CARTESIAN_POINT ( 'NONE',  ( 0.6889763779527566800, -0.5400638737290844871, 0.3530559997133364547 ) ) ;
#24997 = CARTESIAN_POINT ( 'NONE',  ( -1.607611548556429737, 0.2952755905511810774, -0.1292274648535930714 ) ) ;
#24998 = CARTESIAN_POINT ( 'NONE',  ( 0.6233595800524939223, -0.3162353388693405765, 0.4822834645669290543 ) ) ;
#24999 = CARTESIAN_POINT ( 'NONE',  ( -0.4091458600556402980, -0.2362204724409451284, -2.887139107611548461 ) ) ;
#25000 = AXIS2_PLACEMENT_3D ( 'NONE', #6112, #31784, #57447 ) ;
#25001 = CARTESIAN_POINT ( 'NONE',  ( 0.1998031496062994405, -0.3460692066303958092, -1.981627296587926690 ) ) ;
#25002 = DIRECTION ( 'NONE',  ( 0.000000000000000000, 0.000000000000000000, 1.000000000000000000 ) ) ;
#25003 = CONICAL_SURFACE ( 'NONE', #59992, 2.165354330708661568, 0.7853981633974500554 ) ;
#25004 = AXIS2_PLACEMENT_3D ( 'NONE', #18252, #31274, #56939 ) ;
#25005 = CARTESIAN_POINT ( 'NONE',  ( 1.115485564304462551, 0.05413385826771666132, 0.4176697321401328100 ) ) ;
#25006 = CARTESIAN_POINT ( 'NONE',  ( 0.5774278215223103139, -0.6046776061558809534, -0.2411417322834644161 ) ) ;
#25007 = CARTESIAN_POINT ( 'NONE',  ( 0.8070866141732288002, 0.07958543189024085140, 0.2665933059059887866 ) ) ;
#25008 = CARTESIAN_POINT ( 'NONE',  ( 1.213910761154856299, 0.2952755905511811885, 0.1292274648535926551 ) ) ;
#25009 = CARTESIAN_POINT ( 'NONE',  ( -0.3917322834645671215, 0.1049643490035301469, -0.1174540682414699083 ) ) ;
#25010 = CARTESIAN_POINT ( 'NONE',  ( -1.604771003085129433, 2.104981124449682106, 0.1466069496707750608 ) ) ;
#25011 = CARTESIAN_POINT ( 'NONE',  ( 0.7152230971128616943, -0.05778040916215522460, 0.4822834645669289988 ) ) ;
#25012 = CARTESIAN_POINT ( 'NONE',  ( 1.496062992125985147, -0.1870078740157479769, 0.3641732283464567677 ) ) ;
#25013 = CARTESIAN_POINT ( 'NONE',  ( -0.8858267716535425107, 0.1660481256975883668, -0.3530559997133364547 ) ) ;
#25014 = CARTESIAN_POINT ( 'NONE',  ( -0.9580052493438311334, -0.4281496062992124485, 0.4176697321401328655 ) ) ;
#25015 = CARTESIAN_POINT ( 'NONE',  ( 1.253280839895013710, -0.3162353388693405765, 0.4822834645669290543 ) ) ;
#25016 = CARTESIAN_POINT ( 'NONE',  ( -0.1049643490035307020, 0.3917322834645669549, -0.7211286089238846397 ) ) ;
#25017 = CARTESIAN_POINT ( 'NONE',  ( 0.3392501089628018884, -0.1958661417322834220, -1.514435695538058013 ) ) ;
#25018 = CARTESIAN_POINT ( 'NONE',  ( -0.2867679344610365999, 0.2867679344610364889, -2.531496062992125484 ) ) ;
#25019 = ORIENTED_EDGE ( 'NONE', *, *, #56144, .T. ) ;
#25020 = CARTESIAN_POINT ( 'NONE',  ( -9.787531504996567848E-17, 0.3996062992125986035, -1.920830620545185230E-17 ) ) ;
#25021 = ORIENTED_EDGE ( 'NONE', *, *, #13910, .F. ) ;
#25022 = CARTESIAN_POINT ( 'NONE',  ( -0.03937007874015669567, 0.2066929133858268208, 0.000000000000000000 ) ) ;
#25023 = AXIS2_PLACEMENT_3D ( 'NONE', #30228, #43667, #24735 ) ;
#25024 = CARTESIAN_POINT ( 'NONE',  ( 1.305774278215223960, 0.1771653543307087075, -0.09757992244046823083 ) ) ;
#25025 = CARTESIAN_POINT ( 'NONE',  ( -0.1998031496062994683, 0.3460692066303958092, -1.587926509186351698 ) ) ;
#25026 = CARTESIAN_POINT ( 'NONE',  ( 1.318897637795276356, -0.4536011799217367080, 0.2665933059059888421 ) ) ;
#25027 = CARTESIAN_POINT ( 'NONE',  ( -0.1938976377952756625, 0.1938976377952755792, -0.3740157480314971750 ) ) ;
#25028 = DIRECTION ( 'NONE',  ( 0.000000000000000000, 0.000000000000000000, -1.000000000000000000 ) ) ;
#25029 = CARTESIAN_POINT ( 'NONE',  ( 0.1406185367545949583, 0.000000000000000000, -1.409564117849439802 ) ) ;
#25030 = CARTESIAN_POINT ( 'NONE',  ( 0.1049643490035304938, -0.3917322834645669549, -0.3274278215223098143 ) ) ;
#25031 = CARTESIAN_POINT ( 'NONE',  ( -0.6036745406824141069, -0.5023911411419708095, -0.1820866141732282451 ) ) ;
#25032 = CARTESIAN_POINT ( 'NONE',  ( -1.607611548556429737, -0.5511811023622046335, 0.09757992244046803654 ) ) ;
#25033 = CARTESIAN_POINT ( 'NONE',  ( -1.450131233595799651, 0.2952755905511810774, -0.1292274648535930714 ) ) ;
#25034 = CARTESIAN_POINT ( 'NONE',  ( -0.02624671916010428221, -0.6046776061558807314, 0.2411417322834647770 ) ) ;
#25035 = CARTESIAN_POINT ( 'NONE',  ( -1.548556430446193399, -0.6046776061558809534, -0.2411417322834644161 ) ) ;
#25036 = ORIENTED_EDGE ( 'NONE', *, *, #51779, .T. ) ;
#25037 = DIRECTION ( 'NONE',  ( -1.000000000000000000, -0.000000000000000000, -0.000000000000000000 ) ) ;
#25038 =( NAMED_UNIT ( * ) PLANE_ANGLE_UNIT ( ) SI_UNIT ( $, .RADIAN. ) );
#25039 = CARTESIAN_POINT ( 'NONE',  ( -0.4724409448818898682, -8.678599364036362592E-17, -2.244094488188976388 ) ) ;
#25040 = CARTESIAN_POINT ( 'NONE',  ( -1.604771003085130099, 1.553800022087478583, 0.1466069496707745334 ) ) ;
#25041 = CARTESIAN_POINT ( 'NONE',  ( -0.3346456692913377662, 0.07958543189024071263, -0.2665933059059888421 ) ) ;
#25042 = CARTESIAN_POINT ( 'NONE',  ( -1.279527559055116948, 0.1660481256975883668, -0.3530559997133364547 ) ) ;
#25043 = CARTESIAN_POINT ( 'NONE',  ( 1.043307086614173818, 0.1660481256975885056, 0.3530559997133364547 ) ) ;
#25044 = EDGE_LOOP ( 'NONE', ( #22567, #4228, #49955, #640 ) ) ;
#25046 = FACE_OUTER_BOUND ( 'NONE', #80231, .T. ) ;
#25045 = CARTESIAN_POINT ( 'NONE',  ( 0.4724409448818898682, 2.892866454678787531E-17, -2.322834645669291209 ) ) ;
#25047 = CARTESIAN_POINT ( 'NONE',  ( 1.089238845144357759, 0.05413385826771626580, -0.4176697321401330321 ) ) ;
#25048 = CARTESIAN_POINT ( 'NONE',  ( -1.115485564304461219, -0.4281496062992124485, 0.4176697321401328655 ) ) ;
#25049 = CARTESIAN_POINT ( 'NONE',  ( 0.1958661417322836162, -0.3392501089628018329, -0.4868573246381086017 ) ) ;
#25050 = CARTESIAN_POINT ( 'NONE',  ( -0.3149606299212590610, -0.1870078740157479769, 0.3641732283464567677 ) ) ;
#25051 = CARTESIAN_POINT ( 'NONE',  ( 0.3392501089628018329, 0.1958661417322835607, -0.8458005249343831800 ) ) ;
#25052 = CARTESIAN_POINT ( 'NONE',  ( -0.3937007874015740483, -0.1870078740157479769, 0.3641732283464567677 ) ) ;
#25053 = CARTESIAN_POINT ( 'NONE',  ( 0.3280839895013130669, -0.004921259842519576551, 0.3153832671262227771 ) ) ;
#25054 = CARTESIAN_POINT ( 'NONE',  ( 0.2099737532808405305, 0.2306618581243847221, -0.2411417322834647770 ) ) ;
#25055 = CARTESIAN_POINT ( 'NONE',  ( -0.7086614173228339419, -0.1870078740157479769, 0.3641732283464567677 ) ) ;
#25056 = CARTESIAN_POINT ( 'NONE',  ( 0.3917322834645670104, 2.398668435337828261E-17, -2.944881889763779181 ) ) ;
#25057 = CARTESIAN_POINT ( 'NONE',  ( 1.345144356955381593, -0.3162353388693409650, -0.4822834645669289433 ) ) ;
#25058 = AXIS2_PLACEMENT_3D ( 'NONE', #41429, #35114, #29214 ) ;
#25059 = CARTESIAN_POINT ( 'NONE',  ( -1.437007874015747477, 0.1660481256975883668, -0.3530559997133364547 ) ) ;
#25060 = CARTESIAN_POINT ( 'NONE',  ( -0.2362204724409447953, -0.4091458600556404646, -1.402230971128609172 ) ) ;
#25061 = CIRCLE ( 'NONE', #23698, 1.181102362204724310 ) ;
#25062 = CARTESIAN_POINT ( 'NONE',  ( -0.3215223097112853146, -0.3162353388693405765, 0.4822834645669290543 ) ) ;
#25063 = CARTESIAN_POINT ( 'NONE',  ( -1.023622047244093558, -0.1870078740157479769, 0.4822834645669291653 ) ) ;
#25064 = CARTESIAN_POINT ( 'NONE',  ( 1.332020997375329197, -0.2845877964562159024, 0.3641732283464567677 ) ) ;
#25065 = CARTESIAN_POINT ( 'NONE',  ( -0.4330708661417315697, 0.1771653543307087630, 0.000000000000000000 ) ) ;
#25066 = CARTESIAN_POINT ( 'NONE',  ( -0.7414698162729651543, 0.2952755905511810774, -0.1292274648535930714 ) ) ;
#25067 = CARTESIAN_POINT ( 'NONE',  ( -1.095800524934382292, -0.3162353388693409650, -0.4822834645669289433 ) ) ;
#25068 = CARTESIAN_POINT ( 'NONE',  ( -0.4047984445375523710, 5.961526036605507449E-15, -0.3954985857520045833 ) ) ;
#25069 = CARTESIAN_POINT ( 'NONE',  ( 1.141732283464567788, -0.5511811023622047445, 6.969142054262312111E-17 ) ) ;
#25070 = CARTESIAN_POINT ( 'NONE',  ( -0.3346456692913377662, 0.1660481256975883668, -0.3530559997133364547 ) ) ;
#25071 = CARTESIAN_POINT ( 'NONE',  ( -0.9186351706036736120, 0.2306618581243848609, 0.2411417322834645549 ) ) ;
#25072 = ORIENTED_EDGE ( 'NONE', *, *, #36983, .T. ) ;
#25073 = CARTESIAN_POINT ( 'NONE',  ( -0.3460692066303960313, 0.1998031496062989965, -2.465223097112860806 ) ) ;
#25074 = CARTESIAN_POINT ( 'NONE',  ( -0.9973753280839886548, 0.1283753931104748280, 0.1820866141732283561 ) ) ;
#25075 = CARTESIAN_POINT ( 'NONE',  ( 1.338582677165355062, -0.1870078740157480879, -0.4822834645669291653 ) ) ;
#25076 = CARTESIAN_POINT ( 'NONE',  ( -1.181102362204723644, -0.1870078740157480601, -0.3641732283464567677 ) ) ;
#25077 = CARTESIAN_POINT ( 'NONE',  ( -0.1998031496062991630, -0.3460692066303959202, -1.559711286089239035 ) ) ;
#25078 = CARTESIAN_POINT ( 'NONE',  ( -1.043307086614172707, 0.1660481256975883668, -0.3530559997133364547 ) ) ;
#25079 = CARTESIAN_POINT ( 'NONE',  ( 1.391076115485564868, 0.2306618581243847221, -0.2411417322834647770 ) ) ;
#25080 = CARTESIAN_POINT ( 'NONE',  ( 0.8005249343832028242, -0.4281496062992127816, -0.4176697321401328100 ) ) ;
#25081 = CARTESIAN_POINT ( 'NONE',  ( 1.348312163386739426, 0.2755905511811023723, 0.7386866130305692613 ) ) ;
#25082 = CARTESIAN_POINT ( 'NONE',  ( -1.174540682414697335, -0.2845877964562161244, -0.3641732283464567121 ) ) ;
#25084 = EDGE_CURVE ( 'NONE', #69331, #81942, #62659, .T. ) ;
#25083 = CARTESIAN_POINT ( 'NONE',  ( 0.3460692066303959202, -0.1998031496062991630, -0.4967191601049869010 ) ) ;
#25085 = CARTESIAN_POINT ( 'NONE',  ( -0.2925321140481932924, 0.2925321140481931814, -1.122047244094488194 ) ) ;
#25086 = CARTESIAN_POINT ( 'NONE',  ( -0.1058382717557503211, 0.3949938075777409408, -0.1640419947506562559 ) ) ;
#25087 = CARTESIAN_POINT ( 'NONE',  ( 0.3165050273377052470, 1.183948952745706995, -1.413700202057344590 ) ) ;
#25088 = CARTESIAN_POINT ( 'NONE',  ( 1.332020997375329197, -0.2845877964562159024, 0.3641732283464567677 ) ) ;
#25089 = CARTESIAN_POINT ( 'NONE',  ( 0.6627296587926515548, 0.1771653543307087630, 0.09757992244046791164 ) ) ;
#25090 = CARTESIAN_POINT ( 'NONE',  ( 0.5118110236220478892, 0.2952755905511811885, 0.000000000000000000 ) ) ;
#25091 = CARTESIAN_POINT ( 'NONE',  ( -0.4724409448818898682, -8.678599364036362592E-17, -2.320866141732283783 ) ) ;
#25092 = B_SPLINE_CURVE_WITH_KNOTS ( 'NONE', 3,
 ( #83219, #69763, #82804, #50388, #70583, #55875, #44883 ),
 .UNSPECIFIED., .F., .F.,
 ( 4, 3, 4 ),
 ( 1.908195823574488112E-17, 0.001246230184515590604, 0.002492489877932652868 ),
 .UNSPECIFIED. ) ;
#25093 = CARTESIAN_POINT ( 'NONE',  ( -0.3949938075777408852, -0.1058382717557502933, -1.225065616797900159 ) ) ;
#25094 = CARTESIAN_POINT ( 'NONE',  ( 0.8005249343832028242, -0.3690944881889765550, -0.3153832671262227771 ) ) ;
#25095 = CARTESIAN_POINT ( 'NONE',  ( -0.4593175853018364174, -0.4281496062992127816, -0.4176697321401328100 ) ) ;
#25096 = CARTESIAN_POINT ( 'NONE',  ( -1.194225721784776262, -0.4281496062992124485, 0.4176697321401328655 ) ) ;
#25097 = CARTESIAN_POINT ( 'NONE',  ( 0.8792650918635177559, 0.05413385826771666132, 0.4176697321401328100 ) ) ;
#25098 = CARTESIAN_POINT ( 'NONE',  ( 0.2362204724409449064, 0.4091458600556404646, -1.561679790026246684 ) ) ;
#25099 = CARTESIAN_POINT ( 'NONE',  ( -0.3460692066303960868, 0.1998031496062990242, -2.703412073490813583 ) ) ;
#25100 = ORIENTED_EDGE ( 'NONE', *, *, #30797, .F. ) ;
#25101 = ORIENTED_EDGE ( 'NONE', *, *, #37233, .F. ) ;
#25102 = CARTESIAN_POINT ( 'NONE',  ( -1.469816272965878357, -0.6046776061558809534, -0.2411417322834644161 ) ) ;
#25103 = CARTESIAN_POINT ( 'NONE',  ( -0.6364829396325453192, -0.05778040916215560624, -0.4822834645669293319 ) ) ;
#25105 = CARTESIAN_POINT ( 'NONE',  ( -0.8727034120734901146, -0.3162353388693405765, 0.4822834645669290543 ) ) ;
#25104 = CARTESIAN_POINT ( 'NONE',  ( -0.7808398950131222316, -0.2845877964562161244, -0.3641732283464567121 ) ) ;
#25106 = CARTESIAN_POINT ( 'NONE',  ( 0.3543307086614181922, -0.6692913385826771977, 8.415575281601705876E-17 ) ) ;
#25107 = CARTESIAN_POINT ( 'NONE',  ( -0.5183727034120726440, 0.2952755905511811885, 0.1292274648535926551 ) ) ;
#25108 = CARTESIAN_POINT ( 'NONE',  ( -1.181102362204723644, -0.1870078740157479769, 0.4822834645669291653 ) ) ;
#25109 = CARTESIAN_POINT ( 'NONE',  ( -0.8464566929133852113, -0.5400638737290845981, -0.3530559997133363437 ) ) ;
#25110 = CARTESIAN_POINT ( 'NONE',  ( 0.6561679790026253567, 0.2306618581243848609, 0.2411417322834645549 ) ) ;
#25111 = VECTOR ( 'NONE', #69728, 39.37007874015748143 ) ;
#25112 = CARTESIAN_POINT ( 'NONE',  ( -0.1049643490035307020, 0.3917322834645669549, -1.258530183727033958 ) ) ;
#25113 = CARTESIAN_POINT ( 'NONE',  ( -0.9514435695538050464, -0.08942795157528024563, -0.3641732283464568787 ) ) ;
#25114 = VERTEX_POINT ( 'NONE', #19666 ) ;
#25115 = CARTESIAN_POINT ( 'NONE',  ( -0.2891555358219911054, 0.2891555358219909388, -2.066929133858268042 ) ) ;
#25116 = ORIENTED_EDGE ( 'NONE', *, *, #26304, .F. ) ;
#25117 = CARTESIAN_POINT ( 'NONE',  ( -1.279527559055116948, -0.4536011799217367080, 0.2665933059059888421 ) ) ;
#25118 = AXIS2_PLACEMENT_3D ( 'NONE', #82198, #77113, #36732 ) ;
#25119 = AXIS2_PLACEMENT_3D ( 'NONE', #43660, #50396, #76093 ) ;
#25120 = CARTESIAN_POINT ( 'NONE',  ( -1.148293963254592542, 0.2952755905511811885, 0.1292274648535926551 ) ) ;
#25121 = CARTESIAN_POINT ( 'NONE',  ( -0.8595800524934373854, -0.05778040916215522460, 0.4822834645669289988 ) ) ;
#25122 = CARTESIAN_POINT ( 'NONE',  ( -0.1070741851644051862, -0.3996062992125987146, -0.2296587926509186250 ) ) ;
#25123 = CARTESIAN_POINT ( 'NONE',  ( -0.9120734908136475250, 0.2952755905511811885, 0.1292274648535926551 ) ) ;
#25124 = CARTESIAN_POINT ( 'NONE',  ( -1.443569553805773564, -0.6046776061558807314, 0.2411417322834647770 ) ) ;
#25125 = CARTESIAN_POINT ( 'NONE',  ( -1.607611548556429737, 0.2952755905511810774, -0.1292274648535930714 ) ) ;
#25126 = CARTESIAN_POINT ( 'NONE',  ( -1.633858267716534529, -0.5400638737290845981, -0.3530559997133363437 ) ) ;
#25127 = CARTESIAN_POINT ( 'NONE',  ( 0.4724409448818904789, -0.1870078740157480601, -0.3641732283464567677 ) ) ;
#25128 = DIRECTION ( 'NONE',  ( 1.000000000000000000, -0.000000000000000000, -0.000000000000000000 ) ) ;
#25129 = CARTESIAN_POINT ( 'NONE',  ( -0.3917322834645671215, 0.1049643490035301469, -0.1174540682414699083 ) ) ;
#25130 = CARTESIAN_POINT ( 'NONE',  ( -0.05905511811023545637, -0.4536011799217368745, -0.2665933059059886201 ) ) ;
#25131 = CARTESIAN_POINT ( 'NONE',  ( -0.2887139107611542133, -0.6046776061558809534, -0.2411417322834644161 ) ) ;
#25132 = CARTESIAN_POINT ( 'NONE',  ( 1.391076115485564868, -0.6046776061558807314, 0.2411417322834647770 ) ) ;
#25133 = CARTESIAN_POINT ( 'NONE',  ( -0.3083989501312330295, -0.3162353388693409650, -0.4822834645669289433 ) ) ;
#25134 = ORIENTED_EDGE ( 'NONE', *, *, #60455, .F. ) ;
#25135 = CARTESIAN_POINT ( 'NONE',  ( -0.5639538267004599037, 0.004960608223778500969, -0.3437734562760191848 ) ) ;
#25136 = VERTEX_POINT ( 'NONE', #70597 ) ;
#25137 = CARTESIAN_POINT ( 'NONE',  ( -0.1998031496062991630, -0.3460692066303959202, -1.402230971128609172 ) ) ;
#25138 = CARTESIAN_POINT ( 'NONE',  ( -0.4921259842519677963, 0.1660481256975883668, -0.3530559997133364547 ) ) ;
#25139 = CARTESIAN_POINT ( 'NONE',  ( 1.410761154855643795, -0.3162353388693405765, 0.4822834645669290543 ) ) ;
#25140 = CARTESIAN_POINT ( 'NONE',  ( -1.010498687664041384, -0.3690944881889765550, -0.3153832671262227771 ) ) ;
#25141 = CARTESIAN_POINT ( 'NONE',  ( -1.200787401574802349, 0.1660481256975883668, -0.3530559997133364547 ) ) ;
#25142 = CARTESIAN_POINT ( 'NONE',  ( 0.4724409448818897572, -0.1265901696524988906, -1.056430446194225992 ) ) ;
#25143 = B_SPLINE_CURVE_WITH_KNOTS ( 'NONE', 3,
 ( #73971, #80707, #3675, #30577 ),
 .UNSPECIFIED., .F., .F.,
 ( 4, 4 ),
 ( 3.210432057704302528E-07, 0.001287787053612143027 ),
 .UNSPECIFIED. ) ;
#25144 = DIRECTION ( 'NONE',  ( -1.000000000000000000, 0.000000000000000000, -3.491481338843132961E-15 ) ) ;
#25145 = CARTESIAN_POINT ( 'NONE',  ( 0.3917322834645670104, 2.398668435337828261E-17, -2.879921259842519454 ) ) ;
#25146 = CARTESIAN_POINT ( 'NONE',  ( 1.312335958005250269, -0.6046776061558807314, 0.2411417322834647770 ) ) ;
#25147 = CARTESIAN_POINT ( 'NONE',  ( 0.3392501089628018884, -0.1958661417322834220, -2.079396325459317740 ) ) ;
#25148 = CARTESIAN_POINT ( 'NONE',  ( 0.01968503937007957949, -0.5400638737290845981, -0.3530559997133363437 ) ) ;
#25149 = CARTESIAN_POINT ( 'NONE',  ( -1.187664041994749731, -0.2845877964562159024, 0.3641732283464567677 ) ) ;
#25150 = CARTESIAN_POINT ( 'NONE',  ( -0.2952755905511804668, 0.1660481256975885056, 0.3530559997133364547 ) ) ;
#25151 = CARTESIAN_POINT ( 'NONE',  ( 0.3458507752293908943, -0.3458507752293908943, -2.694881889763780070 ) ) ;
#25152 = CARTESIAN_POINT ( 'NONE',  ( -0.9186351706036736120, 0.2306618581243848609, 0.2411417322834645549 ) ) ;
#25153 = CARTESIAN_POINT ( 'NONE',  ( -1.181102362204723644, -0.1870078740157480879, -0.4822834645669291653 ) ) ;
#25154 = CARTESIAN_POINT ( 'NONE',  ( 0.1974969037888706092, -0.3420746716998660508, -2.215879265091863726 ) ) ;
#25155 = CARTESIAN_POINT ( 'NONE',  ( 0.9645669291338588858, 0.07958543189024085140, 0.2665933059059887866 ) ) ;
#25156 = CARTESIAN_POINT ( 'NONE',  ( -0.1181102362204717315, 0.1771653543307087630, 0.000000000000000000 ) ) ;
#25157 = CARTESIAN_POINT ( 'NONE',  ( 0.8005249343832028242, -0.3690944881889765550, -0.3153832671262227771 ) ) ;
#25158 = CARTESIAN_POINT ( 'NONE',  ( -1.587926509186350810, -0.4281496062992124485, 0.4176697321401328655 ) ) ;
#25159 = CARTESIAN_POINT ( 'NONE',  ( 1.423884514435696191, -0.05778040916215522460, 0.4822834645669289988 ) ) ;
#25160 = CARTESIAN_POINT ( 'NONE',  ( 0.4593175853018380828, -0.004921259842519870586, -0.3153832671262229437 ) ) ;
#25161 = CARTESIAN_POINT ( 'NONE',  ( -0.6692913385826764205, 0.2952755905511811885, 0.000000000000000000 ) ) ;
#25162 = CARTESIAN_POINT ( 'NONE',  ( 1.299212598425197429, 0.2952755905511811885, 0.000000000000000000 ) ) ;
#25163 = CARTESIAN_POINT ( 'NONE',  ( -1.157146581871515012E-16, 0.4724409448818898682, 0.2381889763779527491 ) ) ;
#25164 = CARTESIAN_POINT ( 'NONE',  ( -0.1902887139107604098, 0.1771653543307087075, -0.09757992244046823083 ) ) ;
#25165 = CARTESIAN_POINT ( 'NONE',  ( 1.614173228346457378, 0.7794589730111999293, 0.1372047244094478369 ) ) ;
#25166 =( BOUNDED_CURVE ( )  B_SPLINE_CURVE ( 3, ( #31625, #52227, #57286, #19418 ),
 .UNSPECIFIED., .F., .F. ) 
 B_SPLINE_CURVE_WITH_KNOTS ( ( 4, 4 ),
 ( 2.516398611174360145, 3.141592653589793116 ),
 .UNSPECIFIED. ) 
 CURVE ( )  GEOMETRIC_REPRESENTATION_ITEM ( )  RATIONAL_B_SPLINE_CURVE ( ( 1.000000000000000000, 0.9676920770090844393, 0.9676920770090844393, 1.000000000000000000 ) ) 
 REPRESENTATION_ITEM ( '' )  );
#25167 = CARTESIAN_POINT ( 'NONE',  ( 0.1574803149606306130, -0.1870078740157480879, -0.4822834645669291653 ) ) ;
#25168 = DIRECTION ( 'NONE',  ( 1.000000000000000000, 0.000000000000000000, 0.000000000000000000 ) ) ;
#25169 = CARTESIAN_POINT ( 'NONE',  ( 1.555118110236221041, -0.4536011799217367080, 0.2665933059059888421 ) ) ;
#25170 = CARTESIAN_POINT ( 'NONE',  ( 0.07874015748031558404, -0.1870078740157480601, -0.3641732283464567677 ) ) ;
#25171 = CARTESIAN_POINT ( 'NONE',  ( -1.522309711286088607, 0.2306618581243847221, -0.2411417322834647770 ) ) ;
#25172 = CARTESIAN_POINT ( 'NONE',  ( -0.7808398950131222316, -0.2845877964562161244, -0.3641732283464567121 ) ) ;
#25173 = DIRECTION ( 'NONE',  ( 1.000000000000000000, 3.083952846180990281E-16, 0.000000000000000000 ) ) ;
#25174 = CARTESIAN_POINT ( 'NONE',  ( -1.174540682414697335, -0.3162353388693409650, -0.4822834645669289433 ) ) ;
#25175 = CARTESIAN_POINT ( 'NONE',  ( -0.5905511811023613777, -0.6692913385826771977, 8.415575281601705876E-17 ) ) ;
#25176 = CARTESIAN_POINT ( 'NONE',  ( 0.3460692066303958092, 0.1998031496062993018, -0.6804461942257218343 ) ) ;
#25177 = EDGE_CURVE ( 'NONE', #42693, #5361, #21102, .T. ) ;
#25178 = CARTESIAN_POINT ( 'NONE',  ( -9.594673741351313045E-17, 0.3917322834645670104, -2.446850393700787496 ) ) ;
#25179 = CARTESIAN_POINT ( 'NONE',  ( 0.7677165354330716118, -0.4536011799217367080, 0.2665933059059888421 ) ) ;
#25181 = CIRCLE ( 'NONE', #29230, 2.401574803149606474 ) ;
#25180 = CARTESIAN_POINT ( 'NONE',  ( -0.2099737532808391705, 0.2306618581243848609, 0.2411417322834645549 ) ) ;
#25182 = CARTESIAN_POINT ( 'NONE',  ( -0.6167979002624665030, -0.4281496062992127816, -0.4176697321401328100 ) ) ;
#25183 = CARTESIAN_POINT ( 'NONE',  ( -0.8792650918635160906, -0.3690944881889763329, 0.3153832671262228327 ) ) ;
#25184 = CARTESIAN_POINT ( 'NONE',  ( -3.918068336532610108, 1.260885577041682248, 0.3858078592113795557 ) ) ;
#25185 = CARTESIAN_POINT ( 'NONE',  ( 0.07874015748031558404, -0.1870078740157479769, 0.4822834645669291653 ) ) ;
#25186 = CARTESIAN_POINT ( 'NONE',  ( -1.456692913385826182, -0.5511811023622047445, 6.969142054262312111E-17 ) ) ;
#25187 = CARTESIAN_POINT ( 'NONE',  ( 1.312335958005249825, 0.2306618581243847221, -0.2411417322834647770 ) ) ;
#25188 = DIRECTION ( 'NONE',  ( 0.000000000000000000, 0.000000000000000000, 1.000000000000000000 ) ) ;
#25189 = EDGE_CURVE ( 'NONE', #67810, #68995, #43816, .T. ) ;
#25190 = CARTESIAN_POINT ( 'NONE',  ( -0.1049643490035302301, -0.3917322834645671770, -2.273641363025933781 ) ) ;
#25191 = EDGE_LOOP ( 'NONE', ( #1736, #80838, #9421, #81480 ) ) ;
#25192 = CARTESIAN_POINT ( 'NONE',  ( -0.2251228153049663061, -4.992347309556208597E-15, 0.3954985857520076920 ) ) ;
#25193 = CARTESIAN_POINT ( 'NONE',  ( -1.364829396325458521, 0.2306618581243847221, -0.2411417322834647770 ) ) ;
#25194 = CARTESIAN_POINT ( 'NONE',  ( -0.7742782152230965886, 0.05413385826771666132, 0.4176697321401328100 ) ) ;
#25195 = CARTESIAN_POINT ( 'NONE',  ( 1.548556430446194954, -0.6046776061558807314, 0.2411417322834647770 ) ) ;
#25196 = CARTESIAN_POINT ( 'NONE',  ( 0.3392501089628018884, -0.1958661417322834220, -2.079396325459317740 ) ) ;
#25197 = CARTESIAN_POINT ( 'NONE',  ( -0.02544847934398350789, 0.3910482532979367432, -1.220472440944882164 ) ) ;
#25198 = CARTESIAN_POINT ( 'NONE',  ( 1.069553805774278832, 0.2952755905511810774, -0.1292274648535930714 ) ) ;
#25199 = CARTESIAN_POINT ( 'NONE',  ( 0.1640419947506569498, -0.3162353388693409650, -0.4822834645669289433 ) ) ;
#25200 = LINE ( 'NONE', #82470, #5932 ) ;
#25201 = CARTESIAN_POINT ( 'NONE',  ( 0.3996062992125984925, 0.1070741851644054499, -2.721128608923884862 ) ) ;
#25202 = CARTESIAN_POINT ( 'NONE',  ( 1.023622047244095112, -0.1870078740157480601, -0.3641732283464567677 ) ) ;
#25203 = CARTESIAN_POINT ( 'NONE',  ( -0.3460692066303960868, 0.1998031496062990242, -1.443569553805774230 ) ) ;
#25204 = ORIENTED_EDGE ( 'NONE', *, *, #67559, .T. ) ;
#25205 = CARTESIAN_POINT ( 'NONE',  ( -0.1049643490035307158, 0.3917322834645670104, 0.1541801592837776513 ) ) ;
#25206 = EDGE_LOOP ( 'NONE', ( #25036, #49928, #24401, #58970 ) ) ;
#25207 = CARTESIAN_POINT ( 'NONE',  ( 0.3674540682414705883, 0.2306618581243847221, -0.2411417322834647770 ) ) ;
#25208 = CARTESIAN_POINT ( 'NONE',  ( -0.8858267716535425107, 0.1660481256975883668, -0.3530559997133364547 ) ) ;
#25209 = CARTESIAN_POINT ( 'NONE',  ( -1.627296587926508442, 0.2306618581243848609, 0.2411417322834645549 ) ) ;
#25210 = CARTESIAN_POINT ( 'NONE',  ( 0.4855643044619430415, -0.4281496062992127816, -0.4176697321401328100 ) ) ;
#25211 = CARTESIAN_POINT ( 'NONE',  ( -1.555118110236219930, -0.4536011799217368745, -0.2665933059059886201 ) ) ;
#25212 = CARTESIAN_POINT ( 'NONE',  ( 1.489501312335958172, -0.05778040916215560624, -0.4822834645669293319 ) ) ;
#25213 = CARTESIAN_POINT ( 'NONE',  ( 0.06561679790026316017, -0.4281496062992124485, 0.4176697321401328655 ) ) ;
#25214 = CARTESIAN_POINT ( 'NONE',  ( -1.397637795275589623, -0.5400638737290845981, -0.3530559997133363437 ) ) ;
#25215 = CARTESIAN_POINT ( 'NONE',  ( 1.279527559055118724, 0.1660481256975885056, 0.3530559997133364547 ) ) ;
#25216 = CARTESIAN_POINT ( 'NONE',  ( 0.4567483893478956336, 1.408297760469685356, -2.593341242975145899 ) ) ;
#25217 = CARTESIAN_POINT ( 'NONE',  ( -0.3917322834645671215, 0.1049643490035301469, -0.02493438320209968861 ) ) ;
#25218 = CARTESIAN_POINT ( 'NONE',  ( 0.9120734908136490793, 0.1771653543307087075, -0.09757992244046823083 ) ) ;
#25219 = VERTEX_POINT ( 'NONE', #33137 ) ;
#25220 = CARTESIAN_POINT ( 'NONE',  ( 0.3949938075777411073, -0.1058382717557499464, -0.1115485564304462551 ) ) ;
#25221 = ORIENTED_EDGE ( 'NONE', *, *, #56394, .F. ) ;
#25222 = CARTESIAN_POINT ( 'NONE',  ( 0.06561679790026316017, -0.004921259842519870586, -0.3153832671262229437 ) ) ;
#25223 = LINE ( 'NONE', #50889, #60987 ) ;
#25224 = B_SPLINE_CURVE_WITH_KNOTS ( 'NONE', 3,
 ( #4299, #41367, #75022, #16119 ),
 .UNSPECIFIED., .F., .F.,
 ( 4, 4 ),
 ( 9.989667305668851654E-07, 0.001428340232518097606 ),
 .UNSPECIFIED. ) ;
#25225 = CARTESIAN_POINT ( 'NONE',  ( 0.1049868766404206816, -0.6046776061558809534, -0.2411417322834644161 ) ) ;
#25226 = CARTESIAN_POINT ( 'NONE',  ( 0.3805774278215230400, 0.05413385826771626580, -0.4176697321401330321 ) ) ;
#25227 = CARTESIAN_POINT ( 'NONE',  ( -0.5905511811023615998, 0.2952755905511811885, 0.000000000000000000 ) ) ;
#25228 = CARTESIAN_POINT ( 'NONE',  ( -9.594673741351313045E-17, 0.3917322834645670659, -1.886502255414385099 ) ) ;
#25229 = CARTESIAN_POINT ( 'NONE',  ( -1.312335958005248715, 0.2306618581243848609, 0.2411417322834645549 ) ) ;
#25230 = CARTESIAN_POINT ( 'NONE',  ( -0.1958661417322836718, 0.3392501089628017219, -2.617454068241469756 ) ) ;
#25231 = CARTESIAN_POINT ( 'NONE',  ( 1.312335958005249825, 0.1283753931104746893, -0.1820866141732285504 ) ) ;
#25232 = CARTESIAN_POINT ( 'NONE',  ( 0.7545931758530189937, 0.2952755905511810774, -0.1292274648535930714 ) ) ;
#25233 = CARTESIAN_POINT ( 'NONE',  ( 0.5774278215223104249, 0.2306618581243848609, 0.2411417322834645549 ) ) ;
#25234 = CARTESIAN_POINT ( 'NONE',  ( -0.3996062992125986035, -7.340648628747425578E-17, -0.9842519685039369248 ) ) ;
#25235 = CARTESIAN_POINT ( 'NONE',  ( -1.450131233595799651, -0.6692913385826771977, 0.1292274648535927661 ) ) ;
#25236 = CARTESIAN_POINT ( 'NONE',  ( 0.3996062992125984925, 0.1070741851644054637, -0.5164041994750655507 ) ) ;
#25237 = CARTESIAN_POINT ( 'NONE',  ( 0.2925321140481932369, -0.2925321140481931814, -0.01771653543307089712 ) ) ;
#25238 = CARTESIAN_POINT ( 'NONE',  ( -0.2165354330708654795, -0.5400638737290845981, -0.3530559997133363437 ) ) ;
#25239 = CARTESIAN_POINT ( 'NONE',  ( -0.3460692066303958092, -0.1998031496062994683, -2.729658792650918375 ) ) ;
#25240 = CARTESIAN_POINT ( 'NONE',  ( -0.3392501089628019995, 0.1958661417322832277, -1.843175853018372834 ) ) ;
#25241 = CARTESIAN_POINT ( 'NONE',  ( 1.200787401574803681, -0.5400638737290845981, -0.3530559997133363437 ) ) ;
#25242 = AXIS2_PLACEMENT_3D ( 'NONE', #68581, #23539, #29447 ) ;
#25243 = CARTESIAN_POINT ( 'NONE',  ( 1.548556430446194954, 0.2306618581243847221, -0.2411417322834647770 ) ) ;
#25244 = CARTESIAN_POINT ( 'NONE',  ( -0.01968503937007793844, 0.07958543189024071263, -0.2665933059059888421 ) ) ;
#25245 = CARTESIAN_POINT ( 'NONE',  ( 1.010498687664042716, 0.05413385826771626580, -0.4176697321401330321 ) ) ;
#25246 = CARTESIAN_POINT ( 'NONE',  ( -1.157146581871515012E-16, 0.4724409448818898682, -1.494094488188976388 ) ) ;
#25247 = CARTESIAN_POINT ( 'NONE',  ( 0.5511811023622055217, -0.1870078740157479769, 0.3641732283464567677 ) ) ;
#25248 = CARTESIAN_POINT ( 'NONE',  ( 0.2034120734908142214, 0.2952755905511810774, -0.1292274648535930714 ) ) ;
#25249 = CARTESIAN_POINT ( 'NONE',  ( -0.1058382717557503072, 0.3949938075777408852, -1.028215223097112885 ) ) ;
#25250 = EDGE_CURVE ( 'NONE', #13252, #28229, #1166, .T. ) ;
#25251 = CARTESIAN_POINT ( 'NONE',  ( -1.358267716535432434, 0.1660481256975883668, -0.3530559997133364547 ) ) ;
#25252 = CARTESIAN_POINT ( 'NONE',  ( 0.8661417322834652488, -0.1870078740157480601, -0.3641732283464567677 ) ) ;
#25253 = CARTESIAN_POINT ( 'NONE',  ( -2.556694656352302530, 1.572145545125843924, -0.4734416007054419451 ) ) ;
#25254 = CARTESIAN_POINT ( 'NONE',  ( -0.3805774278215216522, -0.4281496062992127816, -0.4176697321401328100 ) ) ;
#25255 = CARTESIAN_POINT ( 'NONE',  ( 0.01968503937007957949, -0.4536011799217368745, -0.2665933059059886201 ) ) ;
#25256 = DIRECTION ( 'NONE',  ( -0.000000000000000000, -1.000000000000000000, -0.000000000000000000 ) ) ;
#25257 = CARTESIAN_POINT ( 'NONE',  ( -0.3346456692913377662, -0.5400638737290844871, 0.3530559997133364547 ) ) ;
#25258 = CARTESIAN_POINT ( 'NONE',  ( 0.1771653543307093182, 0.07958543189024085140, 0.2665933059059887866 ) ) ;
#25259 = CARTESIAN_POINT ( 'NONE',  ( -0.3460692066303960313, 0.1998031496062989965, -1.992782152230971437 ) ) ;
#25260 = CARTESIAN_POINT ( 'NONE',  ( -0.2099737532808391705, 0.2306618581243848609, 0.2411417322834645549 ) ) ;
#25261 = CARTESIAN_POINT ( 'NONE',  ( 1.233595800524935227, 0.1283753931104746893, -0.1820866141732285504 ) ) ;
#25262 = CARTESIAN_POINT ( 'NONE',  ( 0.2246346060905436703, 0.02791078216816508459, -0.4328096321851889194 ) ) ;
#25263 = CARTESIAN_POINT ( 'NONE',  ( -0.1902887139107604098, -0.5511811023622046335, 0.09757992244046803654 ) ) ;
#25264 = CARTESIAN_POINT ( 'NONE',  ( -0.7020997375328076329, -0.2845877964562161244, -0.3641732283464567121 ) ) ;
#25265 = CARTESIAN_POINT ( 'NONE',  ( -0.1443569553805765515, -0.4281496062992127816, -0.4176697321401328100 ) ) ;
#25266 = CARTESIAN_POINT ( 'NONE',  ( 0.07874015748031558404, -0.1870078740157480879, -0.4822834645669291653 ) ) ;
#25267 = CARTESIAN_POINT ( 'NONE',  ( 1.122047244094488860, -0.4536011799217368745, -0.2665933059059886201 ) ) ;
#25268 = CARTESIAN_POINT ( 'NONE',  ( 0.2112933010598323225, 1.111520798820692990, -1.102352278213539316 ) ) ;
#25269 = CARTESIAN_POINT ( 'NONE',  ( 1.535433070866142335, -0.5511811023622047445, 6.969142054262312111E-17 ) ) ;
#25270 = CARTESIAN_POINT ( 'NONE',  ( 0.5511811023622055217, -0.1870078740157479769, 0.4822834645669291653 ) ) ;
#25271 = CARTESIAN_POINT ( 'NONE',  ( 0.3006999498584591590, 1.170162153792016158, -1.947802021145076168 ) ) ;
#25272 = CARTESIAN_POINT ( 'NONE',  ( -0.2755905511811018171, 0.2952755905511811885, 0.000000000000000000 ) ) ;
#25273 = CARTESIAN_POINT ( 'NONE',  ( -0.3917322834645670104, -7.196005306013484475E-17, -0.9114173228346457156 ) ) ;
#25274 = CARTESIAN_POINT ( 'NONE',  ( 0.9055118110236227702, 0.2952755905511811885, 0.000000000000000000 ) ) ;
#25275 = CARTESIAN_POINT ( 'NONE',  ( 0.5839895013123367340, 0.2952755905511811885, 0.1292274648535926551 ) ) ;
#25276 = CARTESIAN_POINT ( 'NONE',  ( 1.854472803289052507, 2.716535433070866645, -0.5314960629921260393 ) ) ;
#25277 = CARTESIAN_POINT ( 'NONE',  ( 0.2887139107611556010, 0.1283753931104746893, -0.1820866141732285504 ) ) ;
#25278 = CARTESIAN_POINT ( 'NONE',  ( 1.233595800524935227, 0.2306618581243847221, -0.2411417322834647770 ) ) ;
#25279 = CARTESIAN_POINT ( 'NONE',  ( -0.4527559055118102749, 0.07958543189024085140, 0.2665933059059887866 ) ) ;
#25280 = CARTESIAN_POINT ( 'NONE',  ( -0.6233595800524928121, -0.3162353388693409650, -0.4822834645669289433 ) ) ;
#25281 = DIRECTION ( 'NONE',  ( 0.000000000000000000, -1.000000000000000000, -0.000000000000000000 ) ) ;
#25282 = CARTESIAN_POINT ( 'NONE',  ( 0.1902887139107617975, 0.2952755905511811885, 0.1292274648535926551 ) ) ;
#25283 = CARTESIAN_POINT ( 'NONE',  ( -0.9120734908136475250, -0.6692913385826773087, -0.1292274648535924053 ) ) ;
#25284 = CARTESIAN_POINT ( 'NONE',  ( -0.4921259842519677963, -0.4536011799217367080, 0.2665933059059888421 ) ) ;
#25285 = CARTESIAN_POINT ( 'NONE',  ( 0.3937007874015754361, -0.1870078740157480879, -0.4822834645669291653 ) ) ;
#25286 = CARTESIAN_POINT ( 'NONE',  ( -1.095800524934382292, -0.05778040916215522460, 0.4822834645669289988 ) ) ;
#25287 = CARTESIAN_POINT ( 'NONE',  ( -0.5052493438320203589, 0.2952755905511810774, -0.1292274648535930714 ) ) ;
#25288 =( BOUNDED_CURVE ( )  B_SPLINE_CURVE ( 2, ( #72496, #28701, #21557, #35850, #46805, #73330, #80075, #14845, #61519, #59854, #2206, #79242, #47218 ),
 .UNSPECIFIED., .F., .F. ) 
 B_SPLINE_CURVE_WITH_KNOTS ( ( 3, 2, 2, 2, 2, 2, 3 ),
 ( 0.1853969023887781231, 0.1856060606060606633, 0.1893939393939394478, 0.1931818181818182323, 0.1969696969696970168, 0.2007575757575758013, 0.2009667339748583414 ),
 .UNSPECIFIED. ) 
 CURVE ( )  GEOMETRIC_REPRESENTATION_ITEM ( )  RATIONAL_B_SPLINE_CURVE ( ( 0.9964447847208416364, 0.9981185001348089614, 1.000000000000000000, 0.9659258262890683122, 1.000000000000000000, 0.9659258262890683122, 1.000000000000000000, 0.9659258262890683122, 1.000000000000000000, 0.9659258262890683122, 1.000000000000000000, 0.9981185001348089614, 0.9964447847208417475 ) ) 
 REPRESENTATION_ITEM ( '' )  );
#25289 = CARTESIAN_POINT ( 'NONE',  ( -0.2362204724409447953, -0.4091458600556404646, -0.5380577427821522374 ) ) ;
#25291 = CARTESIAN_POINT ( 'NONE',  ( 1.515748031496063186, -0.5400638737290845981, -0.3530559997133363437 ) ) ;
#25290 = DIRECTION ( 'NONE',  ( 0.000000000000000000, -0.000000000000000000, -1.000000000000000000 ) ) ;
#25292 = CARTESIAN_POINT ( 'NONE',  ( 1.220472440944882608, 0.2952755905511811885, 0.000000000000000000 ) ) ;
#25293 = CARTESIAN_POINT ( 'NONE',  ( -0.2867679344610364334, -0.2867679344610367109, -2.098425196850393970 ) ) ;
#25294 = CARTESIAN_POINT ( 'NONE',  ( 0.4177787735907000366, 1.299212598425196985, -1.559171609364239375 ) ) ;
#25295 = CARTESIAN_POINT ( 'NONE',  ( -1.102362204724408601, -0.1870078740157479769, 0.4822834645669291653 ) ) ;
#25296 = CARTESIAN_POINT ( 'NONE',  ( 0.4724409448818898682, 2.892866454678787531E-17, -0.2755905511811023723 ) ) ;
#25297 = CARTESIAN_POINT ( 'NONE',  ( 4.837279021331060870E-17, -0.3949938075777409963, -2.598425196850393970 ) ) ;
#25298 = ORIENTED_EDGE ( 'NONE', *, *, #47465, .T. ) ;
#25299 = CARTESIAN_POINT ( 'NONE',  ( -0.09842519685039295696, -0.4536011799217367080, 0.2665933059059888421 ) ) ;
#25300 = CARTESIAN_POINT ( 'NONE',  ( 0.3917322834645670104, -0.1049643490035303411, -1.520997375328083656 ) ) ;
#25301 = B_SPLINE_CURVE_WITH_KNOTS ( 'NONE', 3,
 ( #40241, #78138, #47372, #33093 ),
 .UNSPECIFIED., .F., .F.,
 ( 4, 4 ),
 ( 1.999999999910059834E-07, 0.006970199999999934261 ),
 .UNSPECIFIED. ) ;
#25302 = CARTESIAN_POINT ( 'NONE',  ( 0.5511811023622054106, -0.1870078740157480879, -0.4822834645669291653 ) ) ;
#25303 = CARTESIAN_POINT ( 'NONE',  ( -0.02190130575838357754, 0.3959418824714266427, -2.755905511811024500 ) ) ;
#25304 = CARTESIAN_POINT ( 'NONE',  ( -3.924389226575468737, 2.165354330708661568, 0.3149606299212595606 ) ) ;
#25305 = CARTESIAN_POINT ( 'NONE',  ( -0.5446194225721777693, -0.08942795157527998196, 0.3641732283464567121 ) ) ;
#25306 = CARTESIAN_POINT ( 'NONE',  ( -9.787531504996567848E-17, 0.3996062992125986035, -1.920830620545185230E-17 ) ) ;
#25307 = CARTESIAN_POINT ( 'NONE',  ( 1.318897637795276356, -0.5400638737290844871, 0.3530559997133364547 ) ) ;
#25308 = EDGE_CURVE ( 'NONE', #10444, #58992, #65231, .T. ) ;
#25309 = CARTESIAN_POINT ( 'NONE',  ( 1.049868766404200127, -0.5023911411419708095, -0.1820866141732282451 ) ) ;
#25310 = CARTESIAN_POINT ( 'NONE',  ( -0.1312335958005241554, -0.6046776061558809534, -0.2411417322834644161 ) ) ;
#25311 = CARTESIAN_POINT ( 'NONE',  ( -0.1958661417322836440, 0.3392501089628016664, -0.5655974821184234225 ) ) ;
#25312 = CARTESIAN_POINT ( 'NONE',  ( -0.5446194225721777693, -0.05778040916215522460, 0.4822834645669289988 ) ) ;
#25313 = CARTESIAN_POINT ( 'NONE',  ( -1.174540682414697335, -0.2845877964562161244, -0.3641732283464567121 ) ) ;
#25314 = CARTESIAN_POINT ( 'NONE',  ( -0.5446194225721777693, -0.3162353388693409650, -0.4822834645669289433 ) ) ;
#25315 = DIRECTION ( 'NONE',  ( 0.000000000000000000, 9.738798461624180871E-16, 1.000000000000000000 ) ) ;
#25316 = CARTESIAN_POINT ( 'NONE',  ( -0.2017716535433071445, -0.2017716535433071445, -0.3937007874015748254 ) ) ;
#25317 = VERTEX_POINT ( 'NONE', #79853 ) ;
#25318 = CARTESIAN_POINT ( 'NONE',  ( -0.1958661417322836995, 0.3392501089628017219, -2.057105929955067580 ) ) ;
#25319 = CARTESIAN_POINT ( 'NONE',  ( 0.4921259842519691285, -0.5400638737290845981, -0.3530559997133363437 ) ) ;
#25320 = EDGE_LOOP ( 'NONE', ( #41596, #33031 ) ) ;
#25321 = CARTESIAN_POINT ( 'NONE',  ( -0.9448818897637790704, -0.1870078740157479769, 0.4822834645669291653 ) ) ;
#25322 = CARTESIAN_POINT ( 'NONE',  ( 1.213910761154856299, -0.6692913385826773087, -0.1292274648535924053 ) ) ;
#25323 = CARTESIAN_POINT ( 'NONE',  ( 0.8661417322834652488, -0.1870078740157480879, -0.4822834645669291653 ) ) ;
#25324 = CARTESIAN_POINT ( 'NONE',  ( 0.03937007874015833325, -0.6692913385826771977, 8.415575281601705876E-17 ) ) ;
#25325 = CARTESIAN_POINT ( 'NONE',  ( 0.1958661417322834775, 0.3392501089628018884, -1.331364829396325611 ) ) ;
#25326 = CARTESIAN_POINT ( 'NONE',  ( -0.5905511811023615998, 0.2952755905511811885, 0.000000000000000000 ) ) ;
#25327 = CARTESIAN_POINT ( 'NONE',  ( -0.1902887139107604098, 0.2952755905511810774, -0.1292274648535930714 ) ) ;
#25328 = CARTESIAN_POINT ( 'NONE',  ( -1.049868766404198794, -0.6046776061558807314, 0.2411417322834647770 ) ) ;
#25329 = CARTESIAN_POINT ( 'NONE',  ( -0.09186351706036663400, -0.3690944881889763329, 0.3153832671262228327 ) ) ;
#25330 = CARTESIAN_POINT ( 'NONE',  ( 1.912049360642951330E-20, 1.062992125984252745, -2.874015748031495843 ) ) ;
#25331 = CARTESIAN_POINT ( 'NONE',  ( -0.1837270341207343505, -0.6046776061558807314, 0.2411417322834647770 ) ) ;
#25332 = DIRECTION ( 'NONE',  ( 0.000000000000000000, -1.000000000000000000, 1.408710688920637755E-15 ) ) ;
#25333 = ADVANCED_FACE ( 'NONE', ( #53312 ), #16288, .F. ) ;
#25334 = CARTESIAN_POINT ( 'NONE',  ( 1.286089238845145033, 0.2306618581243848609, 0.2411417322834645549 ) ) ;
#25335 = CARTESIAN_POINT ( 'NONE',  ( 0.1958661417322834775, 0.3392501089628018884, -2.813648293963254776 ) ) ;
#25336 = ORIENTED_EDGE ( 'NONE', *, *, #24369, .T. ) ;
#25337 = EDGE_CURVE ( 'NONE', #38567, #13837, #2819, .T. ) ;
#25338 = ORIENTED_EDGE ( 'NONE', *, *, #66088, .T. ) ;
#25339 = CARTESIAN_POINT ( 'NONE',  ( 0.1049868766404206816, 0.2306618581243848609, 0.2411417322834645549 ) ) ;
#25340 = CARTESIAN_POINT ( 'NONE',  ( -0.3740157480314953431, -0.4536011799217368745, -0.2665933059059886201 ) ) ;
#25342 = DIRECTION ( 'NONE',  ( 1.000000000000000000, 0.000000000000000000, -0.000000000000000000 ) ) ;
#25341 = CARTESIAN_POINT ( 'NONE',  ( 1.325459317585302665, -0.3690944881889763329, 0.3153832671262228327 ) ) ;
#25343 = CARTESIAN_POINT ( 'NONE',  ( 4.797336870675656522E-17, -0.3917322834645670104, -1.265748031496062964 ) ) ;
#25344 = CARTESIAN_POINT ( 'NONE',  ( 0.3458507752293908943, 0.3458507752293908943, -0.2145669291338583029 ) ) ;
#25345 = CARTESIAN_POINT ( 'NONE',  ( 1.555118110236221041, 0.07958543189024071263, -0.2665933059059888421 ) ) ;
#25346 = CARTESIAN_POINT ( 'NONE',  ( 1.587926509186352142, 0.05413385826771666132, 0.4176697321401328100 ) ) ;
#25347 = CARTESIAN_POINT ( 'NONE',  ( -0.1998031496062994405, 0.3460692066303957537, -2.767060367454068359 ) ) ;
#25348 = CARTESIAN_POINT ( 'NONE',  ( 0.6430446194225728496, 0.05413385826771666132, 0.4176697321401328100 ) ) ;
#25349 = CARTESIAN_POINT ( 'NONE',  ( -1.233595800524933894, -0.6046776061558809534, -0.2411417322834644161 ) ) ;
#25350 = CARTESIAN_POINT ( 'NONE',  ( -1.305774278215222184, -0.6692913385826773087, -0.1292274648535924053 ) ) ;
#25351 = CARTESIAN_POINT ( 'NONE',  ( 0.3018372703412079971, -0.4281496062992124485, 0.4176697321401328655 ) ) ;
#25352 = CARTESIAN_POINT ( 'NONE',  ( 0.3949938075777408852, 0.1058382717557500435, -0.04396325459317585588 ) ) ;
#25353 = CARTESIAN_POINT ( 'NONE',  ( -1.607611548556429737, 0.1771653543307087075, -0.09757992244046823083 ) ) ;
#25354 = CARTESIAN_POINT ( 'NONE',  ( 0.9973753280839902091, 0.2306618581243847221, -0.2411417322834647770 ) ) ;
#25355 = CARTESIAN_POINT ( 'NONE',  ( 1.397637795275591177, 0.07958543189024071263, -0.2665933059059888421 ) ) ;
#25356 = CARTESIAN_POINT ( 'NONE',  ( -0.4724409448818898682, -8.678599364036362592E-17, -0.9842519685039369248 ) ) ;
#25357 = CARTESIAN_POINT ( 'NONE',  ( 0.8530183727034128527, -0.3690944881889763329, 0.3153832671262228327 ) ) ;
#25358 = CARTESIAN_POINT ( 'NONE',  ( -0.9448818897637790704, -0.1870078740157480879, -0.4822834645669291653 ) ) ;
#25359 = CARTESIAN_POINT ( 'NONE',  ( 0.3996062992125985480, 2.446882876249141654E-17, -0.3523622047244094335 ) ) ;
#25360 = CARTESIAN_POINT ( 'NONE',  ( 1.522309711286089939, 0.2306618581243848609, 0.2411417322834645549 ) ) ;
#25361 = CARTESIAN_POINT ( 'NONE',  ( 0.3392501089628018329, 0.1958661417322835607, -0.2808398950131232863 ) ) ;
#25363 = CARTESIAN_POINT ( 'NONE',  ( -0.4425803288943545577, 1.365943002350755053, 2.104928023556738914 ) ) ;
#25362 = CARTESIAN_POINT ( 'NONE',  ( 0.6299212598425204535, -0.1870078740157480879, -0.4822834645669291653 ) ) ;
#25364 = CARTESIAN_POINT ( 'NONE',  ( -1.482939632545930975, -0.3690944881889765550, -0.3153832671262227771 ) ) ;
#25365 = CARTESIAN_POINT ( 'NONE',  ( -0.01312335958005186876, 0.05413385826771626580, -0.4176697321401330321 ) ) ;
#25366 = CARTESIAN_POINT ( 'NONE',  ( 1.049868766404200127, -0.5023911411419708095, -0.1820866141732282451 ) ) ;
#25367 = CARTESIAN_POINT ( 'NONE',  ( 0.9317585301837276734, 0.05413385826771626580, -0.4176697321401330321 ) ) ;
#25368 = DIRECTION ( 'NONE',  ( 1.000000000000000000, -0.000000000000000000, -0.000000000000000000 ) ) ;
#25369 = CARTESIAN_POINT ( 'NONE',  ( -0.3346456692913377662, -0.4536011799217367080, 0.2665933059059888421 ) ) ;
#25370 = CARTESIAN_POINT ( 'NONE',  ( -0.5577427821522301654, -0.05778040916215560624, -0.4822834645669293319 ) ) ;
#25371 = CARTESIAN_POINT ( 'NONE',  ( 1.660104986876641320, -0.05778040916215522460, 0.4822834645669289988 ) ) ;
#25372 = CARTESIAN_POINT ( 'NONE',  ( -1.010498687664041384, -0.4281496062992127816, -0.4176697321401328100 ) ) ;
#25373 = CARTESIAN_POINT ( 'NONE',  ( 1.030183727034121421, -0.05778040916215522460, 0.4822834645669289988 ) ) ;
#25374 = CARTESIAN_POINT ( 'NONE',  ( -0.2867679344610367109, 0.2867679344610365444, -0.8038250900600545368 ) ) ;
#25375 = CARTESIAN_POINT ( 'NONE',  ( -1.469816272965878357, 0.1283753931104748280, 0.1820866141732283561 ) ) ;
#25376 = CARTESIAN_POINT ( 'NONE',  ( -0.7426113562971995430, 1.972848275015057995, -0.5309055118110235227 ) ) ;
#25377 = CARTESIAN_POINT ( 'NONE',  ( 1.128608923884514947, 0.2306618581243848609, 0.2411417322834645549 ) ) ;
#25378 = CARTESIAN_POINT ( 'NONE',  ( 0.3458507752293908943, 0.3458507752293908943, -2.419291338582676865 ) ) ;
#25379 = CARTESIAN_POINT ( 'NONE',  ( -1.489501312335957062, -0.3162353388693409650, -0.4822834645669289433 ) ) ;
#25380 = CARTESIAN_POINT ( 'NONE',  ( 1.614173228346457378, -0.6692913385826771977, 8.415575281601705876E-17 ) ) ;
#25381 = CARTESIAN_POINT ( 'NONE',  ( -1.154855643044618851, -0.5023911411419708095, -0.1820866141732282451 ) ) ;
#25382 = CARTESIAN_POINT ( 'NONE',  ( 1.581364829396326277, -0.2845877964562161244, -0.3641732283464567121 ) ) ;
#25383 = CARTESIAN_POINT ( 'NONE',  ( -0.4265091863517051496, -0.6692913385826771977, 0.1292274648535927661 ) ) ;
#25384 = CARTESIAN_POINT ( 'NONE',  ( -0.2952755905511803003, -0.4536011799217368745, -0.2665933059059886201 ) ) ;
#25385 = CARTESIAN_POINT ( 'NONE',  ( -1.692913385826770645, 0.1771653543307087630, 0.000000000000000000 ) ) ;
#25386 = CARTESIAN_POINT ( 'NONE',  ( 1.023622047244095112, -0.1870078740157480601, -0.3641732283464567677 ) ) ;
#25387 = CARTESIAN_POINT ( 'NONE',  ( 0.9383202099737538715, -0.05778040916215560624, -0.4822834645669293319 ) ) ;
#25388 = CARTESIAN_POINT ( 'NONE',  ( 1.404199475065617264, -0.4281496062992124485, 0.4176697321401328655 ) ) ;
#25389 = CARTESIAN_POINT ( 'NONE',  ( 0.1443569553805781891, -0.004921259842519870586, -0.3153832671262229437 ) ) ;
#25390 = CARTESIAN_POINT ( 'NONE',  ( 0.6299212598425204535, -0.1870078740157480879, -0.4822834645669291653 ) ) ;
#25391 = CARTESIAN_POINT ( 'NONE',  ( 0.5183727034120741983, 0.1771653543307087075, -0.09757992244046823083 ) ) ;
#25392 = CARTESIAN_POINT ( 'NONE',  ( 1.489501312335958172, -0.05778040916215560624, -0.4822834645669293319 ) ) ;
#25393 = ADVANCED_FACE ( 'NONE', ( #60052 ), #18326, .T. ) ;
#25394 = CARTESIAN_POINT ( 'NONE',  ( -1.253280839895012377, -0.3162353388693409650, -0.4822834645669289433 ) ) ;
#25395 = CARTESIAN_POINT ( 'NONE',  ( -0.4855643044619415427, -0.4281496062992124485, 0.4176697321401328655 ) ) ;
#25396 = CARTESIAN_POINT ( 'NONE',  ( -0.2925321140481932369, 0.2925321140481931814, -0.4921259842519684624 ) ) ;
#25397 = CARTESIAN_POINT ( 'NONE',  ( 0.1070741851644054776, -0.3996062992125984925, -2.839238845144356649 ) ) ;
#25398 = CARTESIAN_POINT ( 'NONE',  ( 0.5774278215223103139, -0.6046776061558809534, -0.2411417322834644161 ) ) ;
#25399 = CARTESIAN_POINT ( 'NONE',  ( 0.9580052493438326877, -0.004921259842519576551, 0.3153832671262227771 ) ) ;
#25400 = CARTESIAN_POINT ( 'NONE',  ( -0.4527559055118102749, -0.5400638737290845981, -0.3530559997133363437 ) ) ;
#25402 = VECTOR ( 'NONE', #39854, 39.37007874015748143 ) ;
#25401 = CARTESIAN_POINT ( 'NONE',  ( 0.3215223097112867578, -0.05778040916215522460, 0.4822834645669289988 ) ) ;
#25403 = CARTESIAN_POINT ( 'NONE',  ( 0.3996062992125986035, 0.1070741851644054776, -2.171916010498687211 ) ) ;
#25404 = CARTESIAN_POINT ( 'NONE',  ( 0.3420746716998660508, -0.1974969037888703871, -1.522309711286089273 ) ) ;
#25405 = CARTESIAN_POINT ( 'NONE',  ( -0.3996062992125986035, -7.340648628747425578E-17, -2.874015748031495843 ) ) ;
#25406 = CARTESIAN_POINT ( 'NONE',  ( -0.5120078740157480990, -0.3045572308828553565, -0.01849200668098333056 ) ) ;
#25407 = CARTESIAN_POINT ( 'NONE',  ( -0.2867679344610364334, -0.2867679344610367109, -0.8385826771653541734 ) ) ;
#25408 = CARTESIAN_POINT ( 'NONE',  ( -1.043307086614172707, 0.07958543189024071263, -0.2665933059059888421 ) ) ;
#25409 = CARTESIAN_POINT ( 'NONE',  ( -1.358267716535432434, 0.1660481256975883668, -0.3530559997133364547 ) ) ;
#25410 = CARTESIAN_POINT ( 'NONE',  ( 0.2891555358219910499, -0.2891555358219909944, -2.537401574803150428 ) ) ;
#25411 = CARTESIAN_POINT ( 'NONE',  ( 0.7939632545931766261, -0.3162353388693409650, -0.4822834645669289433 ) ) ;
#25412 = CARTESIAN_POINT ( 'NONE',  ( 1.338582677165355062, -0.1870078740157480879, -0.4822834645669291653 ) ) ;
#25413 = CARTESIAN_POINT ( 'NONE',  ( 0.9317585301837276734, -0.4281496062992124485, 0.4176697321401328655 ) ) ;
#25414 = CARTESIAN_POINT ( 'NONE',  ( -0.1265901696524986964, -0.4724409448818899238, -2.906824146981627610 ) ) ;
#25415 = CARTESIAN_POINT ( 'NONE',  ( 0.1998031496062992740, 0.3460692066303959757, -2.034120734908136718 ) ) ;
#25416 = CARTESIAN_POINT ( 'NONE',  ( 1.666666666666667185, 0.05413385826771666132, 0.4176697321401328100 ) ) ;
#25417 = CARTESIAN_POINT ( 'NONE',  ( 0.4265091863517067039, -0.6692913385826773087, -0.1292274648535924053 ) ) ;
#25418 = CARTESIAN_POINT ( 'NONE',  ( 0.5708661417322841158, -0.5400638737290845981, -0.3530559997133363437 ) ) ;
#25419 = CARTESIAN_POINT ( 'NONE',  ( 0.7808398950131240079, -0.2845877964562159024, 0.3641732283464567677 ) ) ;
#25420 = CARTESIAN_POINT ( 'NONE',  ( 1.509186351706037543, 0.05413385826771666132, 0.4176697321401328100 ) ) ;
#25421 = CARTESIAN_POINT ( 'NONE',  ( -0.1049643490035307020, 0.3917322834645669549, -0.09120734908136493568 ) ) ;
#25422 = CARTESIAN_POINT ( 'NONE',  ( 0.6036745406824153282, -0.6046776061558807314, 0.2411417322834647770 ) ) ;
#25423 = CARTESIAN_POINT ( 'NONE',  ( 1.148293963254593875, -0.6692913385826771977, 0.1292274648535927661 ) ) ;
#25424 = CARTESIAN_POINT ( 'NONE',  ( 0.2427821522309719648, -0.05778040916215522460, 0.4822834645669289988 ) ) ;
#25425 = CARTESIAN_POINT ( 'NONE',  ( 1.345144356955381593, -0.08942795157527998196, 0.3641732283464567121 ) ) ;
#25426 = CARTESIAN_POINT ( 'NONE',  ( -0.7545931758530177724, 0.2952755905511811885, 0.1292274648535926551 ) ) ;
#25427 = CARTESIAN_POINT ( 'NONE',  ( -0.9908136482939626788, -0.6692913385826773087, -0.1292274648535924053 ) ) ;
#25428 = CARTESIAN_POINT ( 'NONE',  ( 1.187664041994751285, -0.3162353388693409650, -0.4822834645669289433 ) ) ;
#25429 = CARTESIAN_POINT ( 'NONE',  ( -0.3392501089628019995, 0.1958661417322832277, -0.4258530183727035068 ) ) ;
#25430 = CARTESIAN_POINT ( 'NONE',  ( -0.3917322834645669549, -0.1049643490035306603, -1.612860892388451539 ) ) ;
#25431 = CARTESIAN_POINT ( 'NONE',  ( -0.3392501089628019995, 0.1958661417322832277, -2.538057742782152015 ) ) ;
#25432 = VERTEX_POINT ( 'NONE', #54556 ) ;
#25433 = CARTESIAN_POINT ( 'NONE',  ( -0.3996062992125987146, 0.1070741851644051862, -0.03280839895013124702 ) ) ;
#25434 = ORIENTED_EDGE ( 'NONE', *, *, #33217, .T. ) ;
#25435 = CARTESIAN_POINT ( 'NONE',  ( 1.489501312335958172, -0.3162353388693405765, 0.4822834645669290543 ) ) ;
#25436 = CARTESIAN_POINT ( 'NONE',  ( 1.259842519685040019, -0.1870078740157479769, 0.3641732283464567677 ) ) ;
#25437 = CARTESIAN_POINT ( 'NONE',  ( -0.3996062992125986035, -7.340648628747425578E-17, -1.614173228346456712 ) ) ;
#25438 = CARTESIAN_POINT ( 'NONE',  ( 1.496062992125985147, -0.1870078740157479769, 0.3641732283464567677 ) ) ;
#25439 = DIRECTION ( 'NONE',  ( 0.000000000000000000, 0.000000000000000000, -1.000000000000000000 ) ) ;
#25440 = CARTESIAN_POINT ( 'NONE',  ( -0.09032602383071618168, 0.02791078216816508459, -0.4328096321851889194 ) ) ;
#25441 = CARTESIAN_POINT ( 'NONE',  ( 0.3808816823641231752, -0.09156050430092187165, -1.929133858267716661 ) ) ;
#25442 = CARTESIAN_POINT ( 'NONE',  ( -0.1958661417322836718, 0.3392501089628017219, -0.8851706036745407014 ) ) ;
#25443 = CARTESIAN_POINT ( 'NONE',  ( -0.5839895013123351797, -0.5511811023622046335, 0.09757992244046803654 ) ) ;
#25444 = CARTESIAN_POINT ( 'NONE',  ( -1.535433070866141225, 0.1771653543307087630, 0.000000000000000000 ) ) ;
#25445 = EDGE_CURVE ( 'NONE', #37037, #25602, #79025, .T. ) ;
#25446 = CARTESIAN_POINT ( 'NONE',  ( -1.187664041994749731, -0.3162353388693405765, 0.4822834645669290543 ) ) ;
#25447 = CARTESIAN_POINT ( 'NONE',  ( 0.1246719160104994284, -0.6692913385826771977, 0.1292274648535927661 ) ) ;
#25448 = CARTESIAN_POINT ( 'NONE',  ( 1.515748031496063186, -0.5400638737290845981, -0.3530559997133363437 ) ) ;
#25449 = ORIENTED_EDGE ( 'NONE', *, *, #43371, .F. ) ;
#25450 = CARTESIAN_POINT ( 'NONE',  ( -1.167979002624671248, 0.009842519685039467087, 0.3409548833797002021 ) ) ;
#25451 = CARTESIAN_POINT ( 'NONE',  ( -0.2362204724409447953, -0.4091458600556404646, -1.955380577427821454 ) ) ;
#25452 = CARTESIAN_POINT ( 'NONE',  ( -1.614173228346457378, 1.543375672658094944, 0.1372047244094476981 ) ) ;
#25453 = CARTESIAN_POINT ( 'NONE',  ( -0.6824146981627288167, 0.1283753931104748280, 0.1820866141732283561 ) ) ;
#25454 = CARTESIAN_POINT ( 'NONE',  ( -1.305774278215222184, 0.2952755905511811885, 0.1292274648535926551 ) ) ;
#25455 = CARTESIAN_POINT ( 'NONE',  ( 1.213910761154856299, 0.2952755905511811885, 0.1292274648535926551 ) ) ;
#25456 = ORIENTED_EDGE ( 'NONE', *, *, #38303, .T. ) ;
#25458 = DIRECTION ( 'NONE',  ( 0.000000000000000000, 0.000000000000000000, -1.000000000000000000 ) ) ;
#25457 = CARTESIAN_POINT ( 'NONE',  ( -0.08874907683609993547, 8.471767977567108961E-16, -0.4445507791589058955 ) ) ;
#25459 = EDGE_CURVE ( 'NONE', #26586, #48126, #61326, .T. ) ;
#25460 = CARTESIAN_POINT ( 'NONE',  ( 1.069553805774278832, 0.2952755905511810774, -0.1292274648535930714 ) ) ;
#25461 = CARTESIAN_POINT ( 'NONE',  ( -1.417322834645668772, -0.1870078740157479769, 0.4822834645669291653 ) ) ;
#25462 = CARTESIAN_POINT ( 'NONE',  ( 0.1958661417322834497, 0.3392501089628018329, -1.011791707840208332 ) ) ;
#25463 = CARTESIAN_POINT ( 'NONE',  ( -0.4658792650918627265, -0.08942795157527998196, 0.3641732283464567121 ) ) ;
#25464 = CARTESIAN_POINT ( 'NONE',  ( 0.3917322834645670104, 2.398668435337828261E-17, -0.6751968503937009203 ) ) ;
#25465 = ADVANCED_FACE ( 'NONE', ( #54139 ), #15879, .T. ) ;
#25466 = CARTESIAN_POINT ( 'NONE',  ( -0.3083989501312330295, -0.2845877964562161244, -0.3641732283464567121 ) ) ;
#25467 = CARTESIAN_POINT ( 'NONE',  ( 0.02624671916010564918, 0.1283753931104748280, 0.1820866141732283561 ) ) ;
#25468 = CARTESIAN_POINT ( 'NONE',  ( -0.05249343832020938322, -0.6046776061558809534, -0.2411417322834644161 ) ) ;
#25469 = CARTESIAN_POINT ( 'NONE',  ( -0.8070866141732276899, 0.07958543189024071263, -0.2665933059059888421 ) ) ;
#25470 = CARTESIAN_POINT ( 'NONE',  ( 0.3917322834645670104, -0.1049643490035303411, -2.623359580052493367 ) ) ;
#25471 = CARTESIAN_POINT ( 'NONE',  ( 1.161417322834646271, 0.1660481256975883668, -0.3530559997133364547 ) ) ;
#25472 = CARTESIAN_POINT ( 'NONE',  ( -1.292650918635170010, 0.2952755905511810774, -0.1292274648535930714 ) ) ;
#25473 = CARTESIAN_POINT ( 'NONE',  ( 0.2362204724409451007, -0.4091458600556402980, -1.113517060367454015 ) ) ;
#25474 = CARTESIAN_POINT ( 'NONE',  ( -0.4002624671916004129, -0.05778040916215560624, -0.4822834645669293319 ) ) ;
#25475 = CARTESIAN_POINT ( 'NONE',  ( -0.7611548556430438595, -0.6046776061558809534, -0.2411417322834644161 ) ) ;
#25476 = CARTESIAN_POINT ( 'NONE',  ( 1.069553805774278832, 0.1771653543307087075, -0.09757992244046823083 ) ) ;
#25477 = CARTESIAN_POINT ( 'NONE',  ( -0.4396325459317579898, 0.1771653543307087630, 0.09757992244046791164 ) ) ;
#25478 = CARTESIAN_POINT ( 'NONE',  ( -0.5905511811023615998, 0.2952755905511811885, 0.000000000000000000 ) ) ;
#25479 = CARTESIAN_POINT ( 'NONE',  ( -1.305774278215222184, 0.2952755905511811885, 0.1292274648535926551 ) ) ;
#25480 = CARTESIAN_POINT ( 'NONE',  ( 0.000000000000000000, 0.000000000000000000, -2.755905511811024056 ) ) ;
#25481 = CARTESIAN_POINT ( 'NONE',  ( 1.128608923884515169, -0.5023911411419708095, -0.1820866141732282451 ) ) ;
#25482 = CARTESIAN_POINT ( 'NONE',  ( -0.3280839895013117347, 0.05413385826771626580, -0.4176697321401330321 ) ) ;
#25483 = CARTESIAN_POINT ( 'NONE',  ( -1.358267716535432434, 0.1660481256975883668, -0.3530559997133364547 ) ) ;
#25484 = ORIENTED_EDGE ( 'NONE', *, *, #46415, .F. ) ;
#25485 = EDGE_CURVE ( 'NONE', #77295, #21005, #69245, .T. ) ;
#25486 = CARTESIAN_POINT ( 'NONE',  ( 0.2925321140481932369, -0.2925321140481931814, -2.379921259842520342 ) ) ;
#25487 = CARTESIAN_POINT ( 'NONE',  ( -0.9383202099737524282, -0.2845877964562161244, -0.3641732283464567121 ) ) ;
#25488 = CARTESIAN_POINT ( 'NONE',  ( 0.8792650918635177559, -0.4281496062992127816, -0.4176697321401328100 ) ) ;
#25489 = CARTESIAN_POINT ( 'NONE',  ( -0.8989501312335946848, 0.1771653543307087075, -0.09757992244046823083 ) ) ;
#25490 = CARTESIAN_POINT ( 'NONE',  ( -9.787531504996566615E-17, 0.3996062992125985480, -1.494094488188976610 ) ) ;
#25491 = CARTESIAN_POINT ( 'NONE',  ( -1.108923884514435132, -0.3162353388693405765, 0.4822834645669290543 ) ) ;
#25492 = CARTESIAN_POINT ( 'NONE',  ( 0.8005249343832028242, -0.4281496062992127816, -0.4176697321401328100 ) ) ;
#25493 = CARTESIAN_POINT ( 'NONE',  ( 0.2952755905511819101, 0.1660481256975883668, -0.3530559997133364547 ) ) ;
#25494 = CARTESIAN_POINT ( 'NONE',  ( 1.502624671916010790, -0.3162353388693409650, -0.4822834645669289433 ) ) ;
#25495 = CARTESIAN_POINT ( 'NONE',  ( -1.548556430446193399, 0.1283753931104748280, 0.1820866141732283561 ) ) ;
#25496 = CARTESIAN_POINT ( 'NONE',  ( 0.1070741851644053527, 0.3996062992125985480, -0.7001312335958003175 ) ) ;
#25498 = EDGE_CURVE ( 'NONE', #18348, #21842, #40284, .T. ) ;
#25497 = CARTESIAN_POINT ( 'NONE',  ( -0.1070741851644051862, -0.3996062992125987146, -0.8595800524934383846 ) ) ;
#25499 = CARTESIAN_POINT ( 'NONE',  ( -0.3949938075777411628, 0.1058382717557497937, -0.1902887139107612702 ) ) ;
#25500 = CARTESIAN_POINT ( 'NONE',  ( -0.03443470937339728616, 0.2755905511811023723, -1.753551325310622078 ) ) ;
#25501 = CARTESIAN_POINT ( 'NONE',  ( 1.161417322834646493, -0.4536011799217367080, 0.2665933059059888421 ) ) ;
#25502 = CARTESIAN_POINT ( 'NONE',  ( 0.5905511811023629321, -0.5511811023622047445, 6.969142054262312111E-17 ) ) ;
#25503 = CARTESIAN_POINT ( 'NONE',  ( 0.1509186351706042484, -0.3162353388693405765, 0.4822834645669290543 ) ) ;
#25504 = CARTESIAN_POINT ( 'NONE',  ( 0.2087913723976025926, -0.2087913723976025926, 0.1248231986745540617 ) ) ;
#25505 = CARTESIAN_POINT ( 'NONE',  ( 0.1058382717557500852, -0.3949938075777408852, -1.421916010498688099 ) ) ;
#25506 = CARTESIAN_POINT ( 'NONE',  ( 0.3280839895013130669, -0.3690944881889765550, -0.3153832671262227771 ) ) ;
#25507 = EDGE_CURVE ( 'NONE', #51592, #10444, #984, .T. ) ;
#25508 = CARTESIAN_POINT ( 'NONE',  ( -0.7152230971128602510, -0.3162353388693405765, 0.4822834645669290543 ) ) ;
#25509 = CARTESIAN_POINT ( 'NONE',  ( -1.167979002624671470, 0.05413385826771666132, 0.4176697321401328100 ) ) ;
#25510 = CARTESIAN_POINT ( 'NONE',  ( 0.7217847769028878924, 0.05413385826771666132, 0.4176697321401328100 ) ) ;
#25511 = CARTESIAN_POINT ( 'NONE',  ( -0.4091458600556402980, -0.2362204724409451284, -1.469816272965879245 ) ) ;
#25512 = CARTESIAN_POINT ( 'NONE',  ( -0.1998031496062991907, -0.3460692066303959757, -2.585301837270341352 ) ) ;
#25513 = ORIENTED_EDGE ( 'NONE', *, *, #32216, .T. ) ;
#25514 = ORIENTED_EDGE ( 'NONE', *, *, #49009, .F. ) ;
#25515 = CARTESIAN_POINT ( 'NONE',  ( -1.233595800524933894, 0.2306618581243848609, 0.2411417322834645549 ) ) ;
#25516 = CARTESIAN_POINT ( 'NONE',  ( -0.4330708661417315697, -0.6692913385826771977, 8.415575281601705876E-17 ) ) ;
#25518 = CARTESIAN_POINT ( 'NONE',  ( -0.8398950131233585692, 0.2306618581243848609, 0.2411417322834645549 ) ) ;
#25517 = CARTESIAN_POINT ( 'NONE',  ( -0.7545931758530176614, -0.5511811023622048555, -0.09757992244046775898 ) ) ;
#25519 = CARTESIAN_POINT ( 'NONE',  ( -0.3392501089628019439, 0.1958661417322832554, -1.838563361383515504 ) ) ;
#25520 = DIRECTION ( 'NONE',  ( 0.000000000000000000, 1.000000000000000000, -0.000000000000000000 ) ) ;
#25521 = CARTESIAN_POINT ( 'NONE',  ( 1.456692913385827515, -0.6692913385826771977, 8.415575281601705876E-17 ) ) ;
#25522 = CARTESIAN_POINT ( 'NONE',  ( 1.338582677165355062, -0.1870078740157480879, -0.4822834645669291653 ) ) ;
#25523 = CARTESIAN_POINT ( 'NONE',  ( -0.7611548556430438595, 0.2306618581243848609, 0.2411417322834645549 ) ) ;
#25524 = CARTESIAN_POINT ( 'NONE',  ( 0.4133858267716541968, -0.5400638737290845981, -0.3530559997133363437 ) ) ;
#25525 = CARTESIAN_POINT ( 'NONE',  ( -0.9251968503937002541, -0.5400638737290845981, -0.3530559997133363437 ) ) ;
#25526 = CARTESIAN_POINT ( 'NONE',  ( -0.3917322834645669549, -0.1049643490035306603, -1.612860892388451539 ) ) ;
#25527 = CARTESIAN_POINT ( 'NONE',  ( -0.8398950131233585692, 0.1283753931104748280, 0.1820866141732283561 ) ) ;
#25528 = ORIENTED_EDGE ( 'NONE', *, *, #36242, .F. ) ;
#25529 = CARTESIAN_POINT ( 'NONE',  ( 0.3420746716998659953, 0.1974969037888705536, -1.706036745406824151 ) ) ;
#25530 = ORIENTED_EDGE ( 'NONE', *, *, #37828, .F. ) ;
#25531 = LINE ( 'NONE', #58354, #51561 ) ;
#25532 = CARTESIAN_POINT ( 'NONE',  ( -0.9711286089238838626, 0.2306618581243847221, -0.2411417322834647770 ) ) ;
#25533 = CARTESIAN_POINT ( 'NONE',  ( -1.076115485564303809, -0.6046776061558809534, -0.2411417322834644161 ) ) ;
#25534 = CARTESIAN_POINT ( 'NONE',  ( -0.3996062992125986035, -0.1070741851644056997, -0.2034120734908136108 ) ) ;
#25535 = CARTESIAN_POINT ( 'NONE',  ( -1.187664041994750175, -0.05778040916215560624, -0.4822834645669293319 ) ) ;
#25536 = CARTESIAN_POINT ( 'NONE',  ( -1.187664041994750175, -0.05778040916215560624, -0.4822834645669293319 ) ) ;
#25537 = CARTESIAN_POINT ( 'NONE',  ( -1.653543307086613234, -0.1870078740157479769, 0.4822834645669291653 ) ) ;
#25538 = FACE_OUTER_BOUND ( 'NONE', #50054, .T. ) ;
#25539 = CARTESIAN_POINT ( 'NONE',  ( 0.7283464566929143125, 0.07958543189024085140, 0.2665933059059887866 ) ) ;
#25540 = CARTESIAN_POINT ( 'NONE',  ( 0.4687364453272602205, 1.550612376216559563, 0.5180075785468909455 ) ) ;
#25541 = CARTESIAN_POINT ( 'NONE',  ( 0.1049643490035303689, 0.3917322834645670104, -0.3930446194225722945 ) ) ;
#25542 = CARTESIAN_POINT ( 'NONE',  ( -0.4002624671916004129, -0.08942795157528024563, -0.3641732283464568787 ) ) ;
#25543 = CARTESIAN_POINT ( 'NONE',  ( -0.6102362204724400829, -0.5400638737290845981, -0.3530559997133363437 ) ) ;
#25544 = CARTESIAN_POINT ( 'NONE',  ( 1.417322834645670104, -0.1870078740157479769, 0.4822834645669291653 ) ) ;
#25545 = CARTESIAN_POINT ( 'NONE',  ( -0.2952755905511803003, -0.5400638737290845981, -0.3530559997133363437 ) ) ;
#25546 = EDGE_LOOP ( 'NONE', ( #13866, #7639, #69444, #70525 ) ) ;
#25547 = VERTEX_POINT ( 'NONE', #82317 ) ;
#25548 = CARTESIAN_POINT ( 'NONE',  ( -0.1998031496062994405, 0.3460692066303957537, -1.822178477690288512 ) ) ;
#25549 = CARTESIAN_POINT ( 'NONE',  ( -0.7480314960629914633, -0.6692913385826771977, 8.415575281601705876E-17 ) ) ;
#25550 = CARTESIAN_POINT ( 'NONE',  ( 1.305774278215223960, 0.2952755905511810774, -0.1292274648535930714 ) ) ;
#25551 = CARTESIAN_POINT ( 'NONE',  ( -1.305774278215222184, -0.5511811023622048555, -0.09757992244046775898 ) ) ;
#25552 = CARTESIAN_POINT ( 'NONE',  ( -1.194225721784776262, 0.05413385826771626580, -0.4176697321401330321 ) ) ;
#25553 = CARTESIAN_POINT ( 'NONE',  ( -0.3458507752293909498, 0.3458507752293907833, -0.9645669291338579976 ) ) ;
#25554 = CARTESIAN_POINT ( 'NONE',  ( 1.947751274789685016, 1.170105060311642742, 0.3006284332565817285 ) ) ;
#25555 = CARTESIAN_POINT ( 'NONE',  ( -0.1958661417322836718, 0.3392501089628017219, 0.1522309711286089495 ) ) ;
#25556 = CARTESIAN_POINT ( 'NONE',  ( -0.3392501089628017219, -0.1958661417322836718, -2.026902887139107712 ) ) ;
#25557 = CARTESIAN_POINT ( 'NONE',  ( 0.2559055118110243332, 0.1660481256975885056, 0.3530559997133364547 ) ) ;
#25558 = CARTESIAN_POINT ( 'NONE',  ( -1.049868766404198794, -0.5023911411419708095, 0.1820866141732285504 ) ) ;
#25559 = CARTESIAN_POINT ( 'NONE',  ( -0.9186351706036736120, 0.2306618581243848609, 0.2411417322834645549 ) ) ;
#25560 = CARTESIAN_POINT ( 'NONE',  ( 0.4724409448818898682, 2.892866454678787531E-17, -2.714566929133858331 ) ) ;
#25561 = CARTESIAN_POINT ( 'NONE',  ( -0.9514435695538050464, -0.3162353388693405765, 0.4822834645669290543 ) ) ;
#25562 = EDGE_CURVE ( 'NONE', #43155, #74503, #43133, .T. ) ;
#25563 = CARTESIAN_POINT ( 'NONE',  ( -1.030183727034119867, -0.05778040916215560624, -0.4822834645669293319 ) ) ;
#25564 = CARTESIAN_POINT ( 'NONE',  ( 0.1049868766404206816, -0.6046776061558809534, -0.2411417322834644161 ) ) ;
#25565 = CARTESIAN_POINT ( 'NONE',  ( -0.3949938075777409963, -7.255918531996591613E-17, -2.635826771653543954 ) ) ;
#25566 = CARTESIAN_POINT ( 'NONE',  ( 0.7545931758530188826, -0.5511811023622046335, 0.09757992244046803654 ) ) ;
#25567 = APPLICATION_CONTEXT ( 'automotive_design' ) ;
#25568 = CARTESIAN_POINT ( 'NONE',  ( -0.8267716535433065062, -0.5511811023622047445, 6.969142054262312111E-17 ) ) ;
#25569 = CARTESIAN_POINT ( 'NONE',  ( 0.8727034120734913358, -0.08942795157527998196, 0.3641732283464567121 ) ) ;
#25570 = CARTESIAN_POINT ( 'NONE',  ( 1.371391076115485719, -0.5511811023622048555, -0.09757992244046775898 ) ) ;
#25571 = CARTESIAN_POINT ( 'NONE',  ( 1.476377952755906220, 0.1660481256975883668, -0.3530559997133364547 ) ) ;
#25572 = CARTESIAN_POINT ( 'NONE',  ( 0.3674540682414705883, -0.5023911411419708095, 0.1820866141732285504 ) ) ;
#25573 = CARTESIAN_POINT ( 'NONE',  ( 0.1958661417322834775, 0.3392501089628018884, -1.396325459317585338 ) ) ;
#25574 = CARTESIAN_POINT ( 'NONE',  ( -0.6824146981627288167, 0.2306618581243848609, 0.2411417322834645549 ) ) ;
#25575 = CARTESIAN_POINT ( 'NONE',  ( 1.069553805774278610, -0.6692913385826771977, 0.1292274648535927661 ) ) ;
#25576 = CARTESIAN_POINT ( 'NONE',  ( 0.4724409448818898682, 2.892866454678787531E-17, -0.03740157480314962313 ) ) ;
#25577 = CARTESIAN_POINT ( 'NONE',  ( -0.1837270341207340729, 0.1283753931104746893, -0.1820866141732285504 ) ) ;
#25578 = CARTESIAN_POINT ( 'NONE',  ( -0.1938976377952756625, 0.1938976377952755792, 0.07874015748031495954 ) ) ;
#25579 = CARTESIAN_POINT ( 'NONE',  ( 0.2230971128608932319, -0.4281496062992124485, 0.4176697321401328655 ) ) ;
#25580 = DIRECTION ( 'NONE',  ( 3.096699300667737957E-16, -1.000000000000000000, 0.000000000000000000 ) ) ;
#25581 = CARTESIAN_POINT ( 'NONE',  ( 0.9580052493438326877, -0.004921259842519576551, 0.3153832671262227771 ) ) ;
#25582 = CARTESIAN_POINT ( 'NONE',  ( 0.2362204724409456558, -0.1870078740157480601, -0.3641732283464567677 ) ) ;
#25583 = CARTESIAN_POINT ( 'NONE',  ( 0.1443569553805781891, 0.05413385826771626580, -0.4176697321401330321 ) ) ;
#25584 = CARTESIAN_POINT ( 'NONE',  ( -1.299212598425196097, -0.6692913385826771977, 8.415575281601705876E-17 ) ) ;
#25585 = CARTESIAN_POINT ( 'NONE',  ( -0.8858267716535425107, -0.4536011799217367080, 0.2665933059059888421 ) ) ;
#25586 = FACE_OUTER_BOUND ( 'NONE', #53601, .T. ) ;
#25587 = B_SPLINE_CURVE_WITH_KNOTS ( 'NONE', 3,
 ( #71191, #489, #5956, #31626 ),
 .UNSPECIFIED., .F., .F.,
 ( 4, 4 ),
 ( 3.210432057671751052E-07, 0.001287787053611966735 ),
 .UNSPECIFIED. ) ;
#25588 = CARTESIAN_POINT ( 'NONE',  ( -0.4986876640419939388, 0.2306618581243847221, -0.2411417322834647770 ) ) ;
#25589 = CARTESIAN_POINT ( 'NONE',  ( 0.2925321140481932369, 0.2925321140481932369, -1.001968503937007871 ) ) ;
#25590 = CARTESIAN_POINT ( 'NONE',  ( 4.797336870675656522E-17, -0.3917322834645670104, -2.368110236220472675 ) ) ;
#25591 = CARTESIAN_POINT ( 'NONE',  ( 0.06561679790026316017, -0.004921259842519870586, -0.3153832671262229437 ) ) ;
#25592 = CARTESIAN_POINT ( 'NONE',  ( -0.4461942257217840213, -0.6046776061558809534, -0.2411417322834644161 ) ) ;
#25593 = CARTESIAN_POINT ( 'NONE',  ( -1.286089238845143479, 0.2306618581243847221, -0.2411417322834647770 ) ) ;
#25594 = CARTESIAN_POINT ( 'NONE',  ( -1.220472440944881054, -0.5511811023622047445, 6.969142054262312111E-17 ) ) ;
#25595 = CARTESIAN_POINT ( 'NONE',  ( -3.915444394612497714, 1.299891025107167364, 0.4118628028680341169 ) ) ;
#25596 = CARTESIAN_POINT ( 'NONE',  ( -0.6036745406824141069, -0.6046776061558809534, -0.2411417322834644161 ) ) ;
#25597 = CARTESIAN_POINT ( 'NONE',  ( -1.043307086614172041, -0.4536011799217367080, 0.2665933059059888421 ) ) ;
#25598 = CARTESIAN_POINT ( 'NONE',  ( -1.640419947506561060, -0.3690944881889765550, -0.3153832671262227771 ) ) ;
#25599 = CARTESIAN_POINT ( 'NONE',  ( 1.167979002624672580, 0.05413385826771626580, -0.4176697321401330321 ) ) ;
#25600 = CARTESIAN_POINT ( 'NONE',  ( 2.795275590551181466, 2.204724409448820310, 0.000000000000000000 ) ) ;
#25601 = CARTESIAN_POINT ( 'NONE',  ( -9.594673741351313045E-17, 0.3917322834645670659, -2.043982570375014962 ) ) ;
#25602 = VERTEX_POINT ( 'NONE', #23819 ) ;
#25603 = CARTESIAN_POINT ( 'NONE',  ( 1.614173228346457378, 1.055049524192302357, 0.1372047244094478369 ) ) ;
#25604 = CARTESIAN_POINT ( 'NONE',  ( -1.535433070866141225, 0.2952755905511811885, 0.000000000000000000 ) ) ;
#25605 = CARTESIAN_POINT ( 'NONE',  ( -0.9973753280839886548, -0.6046776061558809534, -0.2411417322834644161 ) ) ;
#25606 = CARTESIAN_POINT ( 'NONE',  ( 1.522309711286089939, -0.6046776061558809534, -0.2411417322834644161 ) ) ;
#25607 = CARTESIAN_POINT ( 'NONE',  ( -0.3917322834645670104, -7.196005306013484475E-17, -2.013779527559055094 ) ) ;
#25608 = CARTESIAN_POINT ( 'NONE',  ( -0.1778467755331564759, 0.3496712940256280211, -1.220472440944882164 ) ) ;
#25609 = CARTESIAN_POINT ( 'NONE',  ( 1.135170603674541256, -0.6692913385826773087, -0.1292274648535924053 ) ) ;
#25610 = CARTESIAN_POINT ( 'NONE',  ( -0.09842519685039295696, -0.5400638737290844871, 0.3530559997133364547 ) ) ;
#25611 = CARTESIAN_POINT ( 'NONE',  ( 0.4724409448818898682, 2.892866454678787531E-17, -2.557086614173228689 ) ) ;
#25612 = CARTESIAN_POINT ( 'NONE',  ( 0.1998031496062994128, -0.3460692066303957537, -2.688320209973753538 ) ) ;
#25613 = CARTESIAN_POINT ( 'NONE',  ( 1.049868766404200127, -0.5023911411419708095, -0.1820866141732282451 ) ) ;
#25614 = CARTESIAN_POINT ( 'NONE',  ( -9.787531504996567848E-17, 0.3996062992125986035, -1.259842519685039353 ) ) ;
#25615 = ORIENTED_EDGE ( 'NONE', *, *, #78000, .T. ) ;
#25616 = CARTESIAN_POINT ( 'NONE',  ( -0.2867679344610364334, -0.2867679344610367109, -2.885826771653543066 ) ) ;
#25617 = ORIENTED_EDGE ( 'NONE', *, *, #30136, .T. ) ;
#25618 = CARTESIAN_POINT ( 'NONE',  ( 0.07874015748031558404, -0.1870078740157480879, -0.4822834645669291653 ) ) ;
#25619 = CARTESIAN_POINT ( 'NONE',  ( -0.7086614173228339419, -0.1870078740157480879, -0.4822834645669291653 ) ) ;
#25620 = CARTESIAN_POINT ( 'NONE',  ( -1.371391076115484609, -0.6692913385826771977, 0.1292274648535927661 ) ) ;
#25621 = CARTESIAN_POINT ( 'NONE',  ( 0.5577427821522316087, -0.05778040916215522460, 0.4822834645669289988 ) ) ;
#25622 = CARTESIAN_POINT ( 'NONE',  ( 1.430446194225722500, -0.4281496062992127816, -0.4176697321401328100 ) ) ;
#25623 = CARTESIAN_POINT ( 'NONE',  ( 1.318897637795276356, 0.1660481256975883668, -0.3530559997133364547 ) ) ;
#25624 = CARTESIAN_POINT ( 'NONE',  ( -0.5643044619422565855, -0.4281496062992124485, 0.4176697321401328655 ) ) ;
#25625 = CARTESIAN_POINT ( 'NONE',  ( 0.6036745406824153282, -0.6046776061558807314, 0.2411417322834647770 ) ) ;
#25626 = CARTESIAN_POINT ( 'NONE',  ( 1.555118110236221041, -0.5400638737290844871, 0.3530559997133364547 ) ) ;
#25627 = CARTESIAN_POINT ( 'NONE',  ( 1.423884514435696191, -0.05778040916215522460, 0.4822834645669289988 ) ) ;
#25628 = CARTESIAN_POINT ( 'NONE',  ( 1.443569553805774897, -0.6046776061558809534, -0.2411417322834644161 ) ) ;
#25629 = CARTESIAN_POINT ( 'NONE',  ( -0.1837270341207343505, -0.6046776061558807314, 0.2411417322834647770 ) ) ;
#25630 = CARTESIAN_POINT ( 'NONE',  ( 0.3917322834645670104, -0.1049643490035303411, -0.1036745406824146343 ) ) ;
#25631 = CARTESIAN_POINT ( 'NONE',  ( 0.3149606299212606708, -0.1870078740157480601, -0.3641732283464567677 ) ) ;
#25632 = VERTEX_POINT ( 'NONE', #68855 ) ;
#25633 = CARTESIAN_POINT ( 'NONE',  ( -0.2891555358219911054, 0.2891555358219909388, -0.6496062992125984925 ) ) ;
#25634 = ORIENTED_EDGE ( 'NONE', *, *, #40829, .F. ) ;
#25635 = CARTESIAN_POINT ( 'NONE',  ( -0.3674540682414692561, -0.5023911411419708095, -0.1820866141732282451 ) ) ;
#25636 = DIRECTION ( 'NONE',  ( 1.000000000000000000, -0.000000000000000000, 3.491481338843132961E-15 ) ) ;
#25637 = CARTESIAN_POINT ( 'NONE',  ( 0.3346456692913390985, 0.1660481256975885056, 0.3530559997133364547 ) ) ;
#25638 = CARTESIAN_POINT ( 'NONE',  ( 0.1181102362204730916, -0.6692913385826771977, 8.415575281601705876E-17 ) ) ;
#25639 = B_SPLINE_CURVE_WITH_KNOTS ( 'NONE', 3,
 ( #4727, #31221, #56889, #63217 ),
 .UNSPECIFIED., .F., .F.,
 ( 4, 4 ),
 ( 3.210432057682506253E-07, 0.001287787053612032872 ),
 .UNSPECIFIED. ) ;
#25640 = CARTESIAN_POINT ( 'NONE',  ( -0.3805774278215216522, -0.4281496062992127816, -0.4176697321401328100 ) ) ;
#25641 = CARTESIAN_POINT ( 'NONE',  ( 0.3392501089628018884, -0.1958661417322833942, -1.676528502133545206 ) ) ;
#25642 = CARTESIAN_POINT ( 'NONE',  ( -1.259842519685038686, -0.1870078740157480879, -0.4822834645669291653 ) ) ;
#25643 = CARTESIAN_POINT ( 'NONE',  ( -0.1049643490035307020, 0.3917322834645669549, -2.610892388451443225 ) ) ;
#25644 = CARTESIAN_POINT ( 'NONE',  ( 0.6889763779527563470, 0.07958543189024071263, -0.2665933059059888421 ) ) ;
#25645 = CARTESIAN_POINT ( 'NONE',  ( 0.6167979002624679463, 0.05413385826771626580, -0.4176697321401330321 ) ) ;
#25646 = CARTESIAN_POINT ( 'NONE',  ( 0.9448818897637802916, -0.1870078740157480879, -0.4822834645669291653 ) ) ;
#25647 = CIRCLE ( 'NONE', #80846, 3.937007874015748143 ) ;
#25648 = CARTESIAN_POINT ( 'NONE',  ( 0.3460692066303959202, 0.1998031496062993295, -0.7611548556430446366 ) ) ;
#25649 = CARTESIAN_POINT ( 'NONE',  ( -1.463254593175852492, -0.6692913385826773087, -0.1292274648535924053 ) ) ;
#25650 = CARTESIAN_POINT ( 'NONE',  ( 0.3460692066303958092, 0.1998031496062993018, -0.8379265091863516979 ) ) ;
#25651 = CARTESIAN_POINT ( 'NONE',  ( -0.1998031496062994405, 0.3460692066303957537, 0.06758530183727032292 ) ) ;
#25652 = CARTESIAN_POINT ( 'NONE',  ( 0.07874015748031558404, -0.1870078740157480879, -0.4822834645669291653 ) ) ;
#25653 = CARTESIAN_POINT ( 'NONE',  ( -0.1998031496062994683, 0.3460692066303958092, -2.532808398950130879 ) ) ;
#25654 = CARTESIAN_POINT ( 'NONE',  ( 0.1958661417322834775, 0.3392501089628018884, -1.803805774278215202 ) ) ;
#25655 = CARTESIAN_POINT ( 'NONE',  ( -1.069553805774277722, -0.5511811023622048555, -0.09757992244046775898 ) ) ;
#25656 = CARTESIAN_POINT ( 'NONE',  ( 1.227034120734908917, -0.6692913385826771977, 0.1292274648535927661 ) ) ;
#25657 = CARTESIAN_POINT ( 'NONE',  ( 1.463254593175853824, -0.6692913385826771977, 0.1292274648535927661 ) ) ;
#25658 = CARTESIAN_POINT ( 'NONE',  ( 0.3083989501312343062, -0.08942795157528024563, -0.3641732283464568787 ) ) ;
#25659 = CARTESIAN_POINT ( 'NONE',  ( 0.9842519685039375910, 0.2952755905511811885, 0.000000000000000000 ) ) ;
#25660 = CARTESIAN_POINT ( 'NONE',  ( 5.785732909357575061E-17, -0.4724409448818898682, -1.415354330708661346 ) ) ;
#25661 = CARTESIAN_POINT ( 'NONE',  ( 0.5183727034120741983, -0.5511811023622046335, 0.09757992244046803654 ) ) ;
#25662 =( BOUNDED_CURVE ( )  B_SPLINE_CURVE ( 1, ( #49973, #49564 ),
 .UNSPECIFIED., .F., .F. ) 
 B_SPLINE_CURVE_WITH_KNOTS ( ( 2, 2 ),
 ( 5.204170427930421283E-18, 0.002000000000000005246 ),
 .UNSPECIFIED. ) 
 CURVE ( )  GEOMETRIC_REPRESENTATION_ITEM ( )  RATIONAL_B_SPLINE_CURVE ( ( 0.9875488213027523443, 0.9875488213027523443 ) ) 
 REPRESENTATION_ITEM ( '' )  );
#25663 = CARTESIAN_POINT ( 'NONE',  ( 0.5905511811023629321, -0.6692913385826771977, 8.415575281601705876E-17 ) ) ;
#25664 = CARTESIAN_POINT ( 'NONE',  ( -9.674558042662122972E-17, 0.3949938075777409963, -1.021653543307086798 ) ) ;
#25665 = CARTESIAN_POINT ( 'NONE',  ( -1.108923884514435132, -0.3162353388693405765, 0.4822834645669290543 ) ) ;
#25666 = CARTESIAN_POINT ( 'NONE',  ( 0.3215223097112867578, -0.08942795157527998196, 0.3641732283464567121 ) ) ;
#25667 = AXIS2_PLACEMENT_3D ( 'NONE', #44135, #37427, #43304 ) ;
#25668 = CARTESIAN_POINT ( 'NONE',  ( -1.948818897637795367, 2.169649841009080787E-17, 5.524802951929911998 ) ) ;
#25669 = CARTESIAN_POINT ( 'NONE',  ( -0.1706036745406816491, -0.4281496062992124485, 0.4176697321401328655 ) ) ;
#25670 = CARTESIAN_POINT ( 'NONE',  ( -0.2099737532808391705, 0.1283753931104748280, 0.1820866141732283561 ) ) ;
#25671 = CARTESIAN_POINT ( 'NONE',  ( 1.076935383196057749, -5.463695987328518425E-17, -0.3149606299212591720 ) ) ;
#25672 = CARTESIAN_POINT ( 'NONE',  ( -0.4068241469816267775, 0.05413385826771626580, -0.4176697321401330321 ) ) ;
#25673 = CARTESIAN_POINT ( 'NONE',  ( 0.2165354330708668673, 0.07958543189024071263, -0.2665933059059888421 ) ) ;
#25674 = CARTESIAN_POINT ( 'NONE',  ( -0.3460692066303957537, -0.1998031496062994405, -2.176509186351706315 ) ) ;
#25675 = CARTESIAN_POINT ( 'NONE',  ( -0.1837270341207340729, 0.2306618581243847221, -0.2411417322834647770 ) ) ;
#25676 = CARTESIAN_POINT ( 'NONE',  ( -0.3917322834645668994, -0.1049643490035306742, -1.700768085792964346 ) ) ;
#25677 = CARTESIAN_POINT ( 'NONE',  ( 1.082677165354331228, 0.07958543189024071263, -0.2665933059059888421 ) ) ;
#25678 = CARTESIAN_POINT ( 'NONE',  ( 0.3836918680457899744, 8.471767977567108961E-16, -0.4445507791589058955 ) ) ;
#25679 = CARTESIAN_POINT ( 'NONE',  ( -0.7217847769028863381, -0.004921259842519870586, -0.3153832671262229437 ) ) ;
#25680 = CARTESIAN_POINT ( 'NONE',  ( -0.8858267716535425107, 0.07958543189024071263, -0.2665933059059888421 ) ) ;
#25681 = CARTESIAN_POINT ( 'NONE',  ( -0.8333333333333323711, 0.2952755905511811885, 0.1292274648535926551 ) ) ;
#25682 = CARTESIAN_POINT ( 'NONE',  ( -0.3083989501312330295, -0.05778040916215522460, 0.4822834645669289988 ) ) ;
#25683 = CARTESIAN_POINT ( 'NONE',  ( 0.6692913385826778638, -0.5511811023622047445, 6.969142054262312111E-17 ) ) ;
#25684 = CARTESIAN_POINT ( 'NONE',  ( -0.2943720246490709735, 0.02382778696830940499, 5.526312367533047443 ) ) ;
#25685 = CARTESIAN_POINT ( 'NONE',  ( 1.345144356955381593, -0.2845877964562161244, -0.3641732283464567121 ) ) ;
#25686 = CARTESIAN_POINT ( 'NONE',  ( 0.9514435695538062676, -0.3162353388693409650, -0.4822834645669289433 ) ) ;
#25687 = CARTESIAN_POINT ( 'NONE',  ( 0.3460692066303958092, 0.1998031496062993018, -0.05052493438320210251 ) ) ;
#25688 = CARTESIAN_POINT ( 'NONE',  ( -0.4068241469816267775, 0.05413385826771626580, -0.4176697321401330321 ) ) ;
#25689 = CARTESIAN_POINT ( 'NONE',  ( -0.3917322834645669549, -0.1049643490035306603, -0.9179790026246721357 ) ) ;
#25690 = CARTESIAN_POINT ( 'NONE',  ( 1.443569553805774897, 0.1283753931104748280, 0.1820866141732283561 ) ) ;
#25691 = CARTESIAN_POINT ( 'NONE',  ( 1.069553805774278832, 0.2952755905511810774, -0.1292274648535930714 ) ) ;
#25692 = CARTESIAN_POINT ( 'NONE',  ( 0.1377952755905518800, 0.1660481256975883668, -0.3530559997133364547 ) ) ;
#25693 = CARTESIAN_POINT ( 'NONE',  ( -0.1959128669332750872, 1.105054483805734566, -3.932156628022151157 ) ) ;
#25694 = CARTESIAN_POINT ( 'NONE',  ( 0.5052493438320218022, -0.5511811023622048555, -0.09757992244046775898 ) ) ;
#25695 = CARTESIAN_POINT ( 'NONE',  ( 1.128608923884515169, -0.6046776061558809534, -0.2411417322834644161 ) ) ;
#25696 = CARTESIAN_POINT ( 'NONE',  ( -0.3412073490813641308, -0.5023911411419708095, 0.1820866141732285504 ) ) ;
#25697 = CARTESIAN_POINT ( 'NONE',  ( -0.9055118110236215490, -0.6692913385826771977, 8.415575281601705876E-17 ) ) ;
#25698 = CARTESIAN_POINT ( 'NONE',  ( 1.868118594278514344, 2.729653106663536555, 0.5314960629921260393 ) ) ;
#25699 = CARTESIAN_POINT ( 'NONE',  ( 0.2755905511811031494, -0.6692913385826771977, 8.415575281601705876E-17 ) ) ;
#25700 = CARTESIAN_POINT ( 'NONE',  ( -0.9973753280839886548, 0.2306618581243848609, 0.2411417322834645549 ) ) ;
#25701 = CARTESIAN_POINT ( 'NONE',  ( -0.7283464566929126471, 0.07958543189024071263, -0.2665933059059888421 ) ) ;
#25702 = VECTOR ( 'NONE', #5178, 39.37007874015748143 ) ;
#25703 = CARTESIAN_POINT ( 'NONE',  ( 0.5052493438320215802, 0.2952755905511811885, 0.1292274648535926551 ) ) ;
#25704 = CARTESIAN_POINT ( 'NONE',  ( -1.049868766404198794, 0.2306618581243847221, -0.2411417322834647770 ) ) ;
#25705 = CARTESIAN_POINT ( 'NONE',  ( -0.3674540682414689785, 0.2306618581243848609, 0.2411417322834645549 ) ) ;
#25706 = FILL_AREA_STYLE ('',( #57690 ) ) ;
#25708 = CARTESIAN_POINT ( 'NONE',  ( 1.318897637795276356, 0.1660481256975883668, -0.3530559997133364547 ) ) ;
#25707 = CARTESIAN_POINT ( 'NONE',  ( -0.9337842054690626004, -2.609244250047836720E-15, 0.3954974714151479609 ) ) ;
#25709 = CARTESIAN_POINT ( 'NONE',  ( 1.332020997375329197, -0.3162353388693405765, 0.4822834645669290543 ) ) ;
#25710 = CARTESIAN_POINT ( 'NONE',  ( 0.3392501089628018884, -0.1958661417322834220, -2.616797900262466836 ) ) ;
#25711 = CARTESIAN_POINT ( 'NONE',  ( -1.502624671916009680, -0.3162353388693405765, 0.4822834645669290543 ) ) ;
#25712 = CARTESIAN_POINT ( 'NONE',  ( -0.8464566929133852113, -0.5400638737290845981, -0.3530559997133363437 ) ) ;
#25713 = CARTESIAN_POINT ( 'NONE',  ( 0.3458507752293908943, 0.3458507752293908943, -0.9251968503937008093 ) ) ;
#25714 = CARTESIAN_POINT ( 'NONE',  ( 0.2925321140481932369, 0.2925321140481932369, 0.01968503937007872254 ) ) ;
#25715 = ORIENTED_EDGE ( 'NONE', *, *, #24847, .F. ) ;
#25716 = CARTESIAN_POINT ( 'NONE',  ( -0.2034120734908128059, 0.1771653543307087630, 0.09757992244046791164 ) ) ;
#25717 = CARTESIAN_POINT ( 'NONE',  ( -0.2867679344610365999, 0.2867679344610364889, -1.744094488188976610 ) ) ;
#25718 = VERTEX_POINT ( 'NONE', #49489 ) ;
#25719 = CARTESIAN_POINT ( 'NONE',  ( 0.4396325459317590445, -0.6692913385826771977, 0.1292274648535927661 ) ) ;
#25720 = CARTESIAN_POINT ( 'NONE',  ( -0.2362204724409447953, -0.4091458600556404646, -2.742782152230971437 ) ) ;
#25721 = CARTESIAN_POINT ( 'NONE',  ( -1.604771003085129655, 1.871396828306225224, -0.1466069496707748387 ) ) ;
#25722 = CARTESIAN_POINT ( 'NONE',  ( -0.5577427821522301654, -0.2845877964562159024, 0.3641732283464567677 ) ) ;
#25723 = CARTESIAN_POINT ( 'NONE',  ( 0.3280839895013130669, 0.05413385826771666132, 0.4176697321401328100 ) ) ;
#25724 = CARTESIAN_POINT ( 'NONE',  ( 1.207349081364829990, 0.2306618581243848609, 0.2411417322834645549 ) ) ;
#25725 = CARTESIAN_POINT ( 'NONE',  ( 1.082677165354331228, -0.4536011799217367080, 0.2665933059059888421 ) ) ;
#25726 = CARTESIAN_POINT ( 'NONE',  ( 0.1049868766404206816, 0.2306618581243848609, 0.2411417322834645549 ) ) ;
#25727 = CARTESIAN_POINT ( 'NONE',  ( 0.3392501089628018329, -0.1958661417322834497, -0.9724216291000506995 ) ) ;
#25728 = CARTESIAN_POINT ( 'NONE',  ( -0.8989501312335946848, -0.6692913385826771977, 0.1292274648535927661 ) ) ;
#25729 = CARTESIAN_POINT ( 'NONE',  ( -1.450131233595799651, -0.5511811023622046335, 0.09757992244046803654 ) ) ;
#25730 = CARTESIAN_POINT ( 'NONE',  ( -0.6102362204724400829, 0.1660481256975885056, 0.3530559997133364547 ) ) ;
#25731 = CARTESIAN_POINT ( 'NONE',  ( 0.000000000000000000, 2.755905511811024056, 0.000000000000000000 ) ) ;
#25732 = CARTESIAN_POINT ( 'NONE',  ( 1.666666666666667185, -0.004921259842519576551, 0.3153832671262227771 ) ) ;
#25733 = ORIENTED_EDGE ( 'NONE', *, *, #64478, .T. ) ;
#25734 = CARTESIAN_POINT ( 'NONE',  ( -0.3917322834645671770, 0.1049643490035302024, -2.391751599246406457 ) ) ;
#25735 = CARTESIAN_POINT ( 'NONE',  ( 0.2165354330708668673, -0.5400638737290844871, 0.3530559997133364547 ) ) ;
#25736 = ORIENTED_EDGE ( 'NONE', *, *, #15160, .T. ) ;
#25737 = CARTESIAN_POINT ( 'NONE',  ( -0.6627296587926503335, -0.6692913385826771977, 0.1292274648535927661 ) ) ;
#25738 = CARTESIAN_POINT ( 'NONE',  ( 1.338582677165355062, -0.1870078740157480879, -0.4822834645669291653 ) ) ;
#25739 = CARTESIAN_POINT ( 'NONE',  ( 1.115485564304462551, 0.05413385826771666132, 0.4176697321401328100 ) ) ;
#25740 = CARTESIAN_POINT ( 'NONE',  ( 0.8595800524934390507, -0.05778040916215560624, -0.4822834645669293319 ) ) ;
#25741 = CARTESIAN_POINT ( 'NONE',  ( 0.1115485564304470323, 0.2952755905511811885, 0.1292274648535926551 ) ) ;
#25742 = CARTESIAN_POINT ( 'NONE',  ( 4.797336870675656522E-17, -0.3917322834645670104, -1.423228346456693050 ) ) ;
#25743 = CARTESIAN_POINT ( 'NONE',  ( -1.095800524934382292, -0.05778040916215522460, 0.4822834645669289988 ) ) ;
#25744 = CARTESIAN_POINT ( 'NONE',  ( -0.3477690288713902178, 0.2952755905511810774, -0.1292274648535930714 ) ) ;
#25745 = CARTESIAN_POINT ( 'NONE',  ( -0.08530183727034056085, -0.2845877964562159024, 0.3641732283464567677 ) ) ;
#25746 = CARTESIAN_POINT ( 'NONE',  ( -0.001150535885505079474, 0.3985446848723406821, -3.148631409696655085E-18 ) ) ;
#25747 = CARTESIAN_POINT ( 'NONE',  ( 0.01312335958005323398, 0.05413385826771666132, 0.4176697321401328100 ) ) ;
#25748 = FACE_OUTER_BOUND ( 'NONE', #76795, .T. ) ;
#25749 = CARTESIAN_POINT ( 'NONE',  ( 1.076115485564305141, -0.6046776061558807314, 0.2411417322834647770 ) ) ;
#25750 = LINE ( 'NONE', #13566, #9338 ) ;
#25751 = ORIENTED_EDGE ( 'NONE', *, *, #18704, .F. ) ;
#25752 = ADVANCED_FACE ( 'NONE', ( #24637 ), #55794, .F. ) ;
#25753 = VERTEX_POINT ( 'NONE', #48659 ) ;
#25754 = CARTESIAN_POINT ( 'NONE',  ( 0.2296587926509192634, -0.3162353388693405765, 0.4822834645669290543 ) ) ;
#25755 = CARTESIAN_POINT ( 'NONE',  ( -0.1509186351706028884, -0.08942795157527998196, 0.3641732283464567121 ) ) ;
#25757 = CARTESIAN_POINT ( 'NONE',  ( -0.06724401132814883386, -3.915482057279200494E-15, 0.3791483426435196535 ) ) ;
#25756 = CARTESIAN_POINT ( 'NONE',  ( 1.332020997375329197, -0.2845877964562159024, 0.3641732283464567677 ) ) ;
#25758 = CARTESIAN_POINT ( 'NONE',  ( -0.2867679344610365999, 0.2867679344610364889, -1.049212598425196763 ) ) ;
#25759 = CARTESIAN_POINT ( 'NONE',  ( -0.1265901696524993347, 0.4724409448818895907, -0.3982939632545932085 ) ) ;
#25760 = CARTESIAN_POINT ( 'NONE',  ( 1.541994750656168645, 0.1771653543307087075, -0.09757992244046823083 ) ) ;
#25761 = CARTESIAN_POINT ( 'NONE',  ( -1.502624671916009680, -0.3162353388693405765, 0.4822834645669290543 ) ) ;
#25762 = CARTESIAN_POINT ( 'NONE',  ( -9.674558042662122972E-17, 0.3949938075777409963, 0.08070866141732281618 ) ) ;
#25763 = PRODUCT ( 'Cast Iron Heavy Chuck Body', 'Cast Iron Heavy Chuck Body', '', ( #68350 ) ) ;
#25764 = CARTESIAN_POINT ( 'NONE',  ( 0.01968503937007930540, 0.1660481256975885056, 0.3530559997133364547 ) ) ;
#25765 = CARTESIAN_POINT ( 'NONE',  ( -1.404199475065615932, -0.4281496062992127816, -0.4176697321401328100 ) ) ;
#25766 = CARTESIAN_POINT ( 'NONE',  ( -0.9973753280839886548, -0.6046776061558809534, -0.2411417322834644161 ) ) ;
#25767 = CARTESIAN_POINT ( 'NONE',  ( 0.1509186351706042484, -0.3162353388693405765, 0.4822834645669290543 ) ) ;
#25768 = CARTESIAN_POINT ( 'NONE',  ( 0.3420746716998660508, -0.1974969037888704149, -0.1817585301837270073 ) ) ;
#25769 = CARTESIAN_POINT ( 'NONE',  ( -1.568241469816272105, -0.2845877964562161244, -0.3641732283464567121 ) ) ;
#25770 = CARTESIAN_POINT ( 'NONE',  ( 0.9580052493438326877, 0.05413385826771666132, 0.4176697321401328100 ) ) ;
#25771 = CARTESIAN_POINT ( 'NONE',  ( 0.9251968503937015864, 0.07958543189024071263, -0.2665933059059888421 ) ) ;
#25772 = CARTESIAN_POINT ( 'NONE',  ( -0.06873123812452887338, -2.191421614605370878E-15, 0.4445507791589071167 ) ) ;
#25773 = CARTESIAN_POINT ( 'NONE',  ( 0.9776902887139113929, -0.5511811023622048555, -0.09757992244046775898 ) ) ;
#25774 = CARTESIAN_POINT ( 'NONE',  ( -1.299212598425196097, 0.2952755905511811885, 0.000000000000000000 ) ) ;
#25775 = CARTESIAN_POINT ( 'NONE',  ( -9.787531504996566615E-17, 0.3996062992125985480, -0.8641732283464567121 ) ) ;
#25776 = CARTESIAN_POINT ( 'NONE',  ( 1.049868766404200349, 0.2306618581243848609, 0.2411417322834645549 ) ) ;
#25777 = CARTESIAN_POINT ( 'NONE',  ( -0.2867679344610364334, -0.2867679344610367109, -0.6811023622047243098 ) ) ;
#25779 = CARTESIAN_POINT ( 'NONE',  ( -0.08477834984147802899, 1.070319560067209963, 1.857180095838086631 ) ) ;
#25778 = CARTESIAN_POINT ( 'NONE',  ( 0.6824146981627303710, -0.6046776061558807314, 0.2411417322834647770 ) ) ;
#25780 = FACE_OUTER_BOUND ( 'NONE', #4050, .T. ) ;
#25781 = CARTESIAN_POINT ( 'NONE',  ( 0.1443569553805781891, 0.05413385826771626580, -0.4176697321401330321 ) ) ;
#25782 = CARTESIAN_POINT ( 'NONE',  ( 0.2493438320209980519, -0.3690944881889765550, -0.3153832671262227771 ) ) ;
#25783 = CARTESIAN_POINT ( 'NONE',  ( 0.7808398950131241190, -0.05778040916215560624, -0.4822834645669293319 ) ) ;
#25784 = CARTESIAN_POINT ( 'NONE',  ( 0.7742782152230979209, 0.009842519685039147898, -0.3409548833797004797 ) ) ;
#25785 = CARTESIAN_POINT ( 'NONE',  ( -0.5708661417322828946, 0.07958543189024071263, -0.2665933059059888421 ) ) ;
#25786 = CARTESIAN_POINT ( 'NONE',  ( -0.7939632545931754048, -0.3162353388693405765, 0.4822834645669290543 ) ) ;
#25787 = CARTESIAN_POINT ( 'NONE',  ( -1.614173228346455824, 0.1771653543307087630, 0.000000000000000000 ) ) ;
#25788 = ADVANCED_FACE ( 'NONE', ( #29720 ), #17527, .F. ) ;
#25789 = CARTESIAN_POINT ( 'NONE',  ( -1.338582677165353729, -0.1870078740157480879, -0.4822834645669291653 ) ) ;
#25790 = CARTESIAN_POINT ( 'NONE',  ( 1.141732283464567788, -0.6692913385826771977, 8.415575281601705876E-17 ) ) ;
#25791 = CARTESIAN_POINT ( 'NONE',  ( -1.528871391076114250, -0.5511811023622046335, 0.09757992244046803654 ) ) ;
#25792 =( BOUNDED_CURVE ( )  B_SPLINE_CURVE ( 1, ( #77974, #14836 ),
 .UNSPECIFIED., .F., .F. ) 
 B_SPLINE_CURVE_WITH_KNOTS ( ( 2, 2 ),
 ( 1.734723475976807094E-18, 0.002000000000000003511 ),
 .UNSPECIFIED. ) 
 CURVE ( )  GEOMETRIC_REPRESENTATION_ITEM ( )  RATIONAL_B_SPLINE_CURVE ( ( 0.9875488213027523443, 0.9875488213027523443 ) ) 
 REPRESENTATION_ITEM ( '' )  );
#25793 = CARTESIAN_POINT ( 'NONE',  ( 1.077480042006655703, 1.180860146545615885, 0.3133340167985102509 ) ) ;
#25794 = CARTESIAN_POINT ( 'NONE',  ( 1.187664041994751285, -0.3162353388693409650, -0.4822834645669289433 ) ) ;
#25795 = CARTESIAN_POINT ( 'NONE',  ( 0.4724409448818896462, 0.1265901696524990294, -2.406167979002624246 ) ) ;
#25796 = CARTESIAN_POINT ( 'NONE',  ( -1.522309711286088607, 0.2306618581243847221, -0.2411417322834647770 ) ) ;
#25797 = CARTESIAN_POINT ( 'NONE',  ( -1.581364829396324945, -0.08942795157528024563, -0.3641732283464568787 ) ) ;
#25798 = CARTESIAN_POINT ( 'NONE',  ( -0.8595800524934373854, -0.2845877964562161244, -0.3641732283464567121 ) ) ;
#25799 = CARTESIAN_POINT ( 'NONE',  ( 1.489501312335958172, -0.2845877964562159024, 0.3641732283464567677 ) ) ;
#25800 = CARTESIAN_POINT ( 'NONE',  ( -0.2559055118110227234, -0.5400638737290844871, 0.3530559997133364547 ) ) ;
#25801 = CARTESIAN_POINT ( 'NONE',  ( -0.3477690288713902178, 0.1771653543307087075, -0.09757992244046823083 ) ) ;
#25802 = CARTESIAN_POINT ( 'NONE',  ( -1.614173228346456268, -0.5511811023622047445, 6.969142054262312111E-17 ) ) ;
#25803 = CARTESIAN_POINT ( 'NONE',  ( 0.8989501312335963501, -0.5511811023622048555, -0.09757992244046775898 ) ) ;
#25804 = CARTESIAN_POINT ( 'NONE',  ( 0.4461942257217856311, 0.2306618581243847221, -0.2411417322834647770 ) ) ;
#25805 = CARTESIAN_POINT ( 'NONE',  ( 0.6299212598424784870, 2.165354330708661568, 3.937007874015796105 ) ) ;
#25806 = CARTESIAN_POINT ( 'NONE',  ( 0.6692913385826778638, -0.6692913385826771977, 8.415575281601705876E-17 ) ) ;
#25807 = CARTESIAN_POINT ( 'NONE',  ( 0.6036745406824153282, -0.5023911411419708095, 0.1820866141732285504 ) ) ;
#25808 = CARTESIAN_POINT ( 'NONE',  ( -1.548556430446193399, -0.6046776061558809534, -0.2411417322834644161 ) ) ;
#25809 = EDGE_CURVE ( 'NONE', #64186, #2910, #11601, .T. ) ;
#25810 = CARTESIAN_POINT ( 'NONE',  ( -1.430446194225720724, 0.05413385826771626580, -0.4176697321401330321 ) ) ;
#25811 = CARTESIAN_POINT ( 'NONE',  ( -0.4002624671916004129, -0.05778040916215560624, -0.4822834645669293319 ) ) ;
#25812 = CARTESIAN_POINT ( 'NONE',  ( -0.1070741851644057135, 0.3996062992125985480, -0.1640419947506562004 ) ) ;
#25813 = CARTESIAN_POINT ( 'NONE',  ( -0.1998031496062991630, -0.3460692066303959202, -2.662073490813648746 ) ) ;
#25814 = CARTESIAN_POINT ( 'NONE',  ( 0.09842519685039434474, -0.5400638737290845981, -0.3530559997133363437 ) ) ;
#25815 = CARTESIAN_POINT ( 'NONE',  ( 1.010498687664042716, -0.004921259842519870586, -0.3153832671262229437 ) ) ;
#25816 = CARTESIAN_POINT ( 'NONE',  ( -0.5249343832020990641, 0.2306618581243848609, 0.2411417322834645549 ) ) ;
#25817 = CARTESIAN_POINT ( 'NONE',  ( 0.4461942257217855201, -0.6046776061558807314, 0.2411417322834647770 ) ) ;
#25818 = CARTESIAN_POINT ( 'NONE',  ( -0.3460692066303958092, -0.1998031496062994683, -2.099737532808398921 ) ) ;
#25819 = CARTESIAN_POINT ( 'NONE',  ( 0.2891555358219910499, -0.2891555358219909944, -1.988188976377952777 ) ) ;
#25820 = CARTESIAN_POINT ( 'NONE',  ( -0.3917322834645669549, -0.1049643490035306603, -0.3530183727034120755 ) ) ;
#25821 = CARTESIAN_POINT ( 'NONE',  ( 0.4177787735907000366, 0.3937007874015748254, -1.559171609364239375 ) ) ;
#25822 = CARTESIAN_POINT ( 'NONE',  ( -0.1049643490035301885, -0.3917322834645671215, -1.009186351706036433 ) ) ;
#25823 = CARTESIAN_POINT ( 'NONE',  ( -0.8530183727034112984, -0.3690944881889765550, -0.3153832671262227771 ) ) ;
#25824 = CARTESIAN_POINT ( 'NONE',  ( -1.279527559055116948, -0.5400638737290844871, 0.3530559997133364547 ) ) ;
#25825 = AXIS2_PLACEMENT_3D ( 'NONE', #4274, #11005, #16928 ) ;
#25826 = CARTESIAN_POINT ( 'NONE',  ( -0.2891555358219911054, 0.2891555358219909388, -2.458661417322835163 ) ) ;
#25827 = CARTESIAN_POINT ( 'NONE',  ( 0.3215223097112867578, -0.3162353388693409650, -0.4822834645669289433 ) ) ;
#25828 = CARTESIAN_POINT ( 'NONE',  ( 1.187664041994751285, -0.3162353388693409650, -0.4822834645669289433 ) ) ;
#25829 = CARTESIAN_POINT ( 'NONE',  ( 0.7677165354330716118, -0.5400638737290844871, 0.3530559997133364547 ) ) ;
#25830 = CARTESIAN_POINT ( 'NONE',  ( -0.2362204724409451284, 0.4091458600556402425, -2.690288713910760965 ) ) ;
#25831 = CARTESIAN_POINT ( 'NONE',  ( 0.1998031496062992740, 0.3460692066303959757, -2.191601049868766360 ) ) ;
#25832 = CARTESIAN_POINT ( 'NONE',  ( 0.3392501089628018329, 0.1958661417322835607, -0.6004130165692406207 ) ) ;
#25833 = CARTESIAN_POINT ( 'NONE',  ( 1.535433070866142558, 0.2952755905511811885, 0.000000000000000000 ) ) ;
#25834 = CARTESIAN_POINT ( 'NONE',  ( 0.3477690288713918276, 0.2952755905511811885, 0.1292274648535926551 ) ) ;
#25835 = CARTESIAN_POINT ( 'NONE',  ( 0.07874015748031558404, -0.1870078740157480879, -0.4822834645669291653 ) ) ;
#25836 = CARTESIAN_POINT ( 'NONE',  ( 0.7283464566929140904, -0.4536011799217368745, -0.2665933059059886201 ) ) ;
#25837 = CARTESIAN_POINT ( 'NONE',  ( 1.318897637795276356, -0.5400638737290844871, 0.3530559997133364547 ) ) ;
#25838 = CARTESIAN_POINT ( 'NONE',  ( 0.1049643490035304938, -0.3917322834645669549, -0.3274278215223098143 ) ) ;
#25839 = CARTESIAN_POINT ( 'NONE',  ( 0.5577427821522314977, -0.3162353388693409650, -0.4822834645669289433 ) ) ;
#25840 = CARTESIAN_POINT ( 'NONE',  ( 0.9448818897637802916, -0.1870078740157480879, -0.4822834645669291653 ) ) ;
#25841 = CARTESIAN_POINT ( 'NONE',  ( 0.1837270341207357105, -0.6046776061558809534, -0.2411417322834644161 ) ) ;
#25842 = CARTESIAN_POINT ( 'NONE',  ( 1.056430446194226658, 0.1771653543307087630, 0.09757992244046791164 ) ) ;
#25843 = CARTESIAN_POINT ( 'NONE',  ( -1.036745406824146176, 0.05413385826771626580, -0.4176697321401330321 ) ) ;
#25844 = CARTESIAN_POINT ( 'NONE',  ( -1.108923884514435132, -0.3162353388693405765, 0.4822834645669290543 ) ) ;
#25845 = CARTESIAN_POINT ( 'NONE',  ( 1.227034120734908917, -0.6692913385826771977, 0.1292274648535927661 ) ) ;
#25846 = CARTESIAN_POINT ( 'NONE',  ( -0.3917322834645669549, -0.1049643490035306603, -0.7604986876640419391 ) ) ;
#25847 = CARTESIAN_POINT ( 'NONE',  ( 4.797336870675656522E-17, -0.3917322834645670104, -1.488188976377952777 ) ) ;
#25848 = CARTESIAN_POINT ( 'NONE',  ( -0.3917322834645670104, -7.196005306013484475E-17, -2.866141732283464361 ) ) ;
#25849 = VERTEX_POINT ( 'NONE', #81088 ) ;
#25850 = CARTESIAN_POINT ( 'NONE',  ( -0.3996062992125986035, -0.1070741851644056997, -0.04593175853018374721 ) ) ;
#25851 = VERTEX_POINT ( 'NONE', #62537 ) ;
#25852 = CARTESIAN_POINT ( 'NONE',  ( 1.410761154855643795, -0.05778040916215560624, -0.4822834645669293319 ) ) ;
#25853 = CARTESIAN_POINT ( 'NONE',  ( 0.9580052493438326877, -0.004921259842519576551, 0.3153832671262227771 ) ) ;
#25854 = CARTESIAN_POINT ( 'NONE',  ( -0.2925321140481932924, 0.2925321140481931814, -1.437007874015747921 ) ) ;
#25855 = CARTESIAN_POINT ( 'NONE',  ( 1.207349081364829990, 0.1283753931104748280, 0.1820866141732283561 ) ) ;
#25856 = CARTESIAN_POINT ( 'NONE',  ( 0.8761506516392508770, -4.927456884911482678E-16, 0.4445507791589062840 ) ) ;
#25857 = CLOSED_SHELL ( 'NONE', ( #74348, #75100, #71156, #69191, #33473, #11941, #82590, #12134, #60173, #18684, #61504, #22635, #70074, #62024, #63467, #8043, #55189, #36506, #35461, #41549, #27491, #80719, #47069, #11624, #28941, #30648, #77956, #13717, #12143, #51550, #5872, #46293, #8117, #71640, #19724, #40121, #36166, #65122, #45547, #30331, #68450, #34686, #38163, #75824, #14043, #71282, #995, #31168, #47984, #48514, #38323, #10452, #62411, #30668, #31175, #21981, #29986, #67090, #18794, #61336, #28474, #44546, #44736, #53424, #8523, #26537, #77668, #28093, #74389, #72528, #64894, #75484, #4827, #65316, #63425, #52596, #4176, #33389, #40464, #36257, #60304, #73876, #39944, #36194, #72439, #29137, #4673, #5428, #12182, #64484, #67221, #74186, #76043, #72658, #53265, #19748, #59438, #26870, #49957, #44444, #26046, #49179, #23889, #55290, #16951, #5061, #56282, #27094, #70686, #55749, #11406, #23337, #76267, #13813, #37367, #74057, #42342, #29106, #80571, #20648, #54159, #9057, #10898, #9532, #11732, #8303, #21883, #13194, #29568, #7468, #51124, #22913, #33047, #79109, #9822, #73241, #78873, #28938, #50679, #47621, #68661, #12761, #73395, #9472, #56234, #1837, #58771, #49657, #16811, #74795, #60552, #32317, #59116, #28336, #7861, #24840, #56841, #13237, #55020, #18148, #34742, #4371, #15112, #7893, #69392, #58291, #53257, #64340, #1705, #72691, #35600, #59970, #71759, #64110, #79061, #2735, #1770, #52837, #54723, #790, #57483, #74831, #64625, #34263, #56077, #64633, #18709, #10373, #40934, #8356, #39351, #59497, #47329, #28632, #15084, #8910, #19785, #75418, #43999, #65582, #9254, #4804 ) ) ;
#25858 = CARTESIAN_POINT ( 'NONE',  ( -0.4124503923812501971, 1.301275207309029014, 2.666248201964647180 ) ) ;
#25859 = CARTESIAN_POINT ( 'NONE',  ( -0.1265901696524986964, -0.4724409448818899238, -1.174540682414698445 ) ) ;
#25860 = CARTESIAN_POINT ( 'NONE',  ( 0.3917322834645670104, 2.398668435337828261E-17, -0.8326771653543307838 ) ) ;
#25861 = CARTESIAN_POINT ( 'NONE',  ( -0.9908136482939626788, 0.1771653543307087630, 0.09757992244046791164 ) ) ;
#25862 = CARTESIAN_POINT ( 'NONE',  ( -1.482939632545930975, -0.3690944881889765550, -0.3153832671262227771 ) ) ;
#25863 = CARTESIAN_POINT ( 'NONE',  ( -1.482939632545930975, 0.05413385826771666132, 0.4176697321401328100 ) ) ;
#25864 = CARTESIAN_POINT ( 'NONE',  ( -0.08530183727034056085, -0.05778040916215560624, -0.4822834645669293319 ) ) ;
#25865 = CARTESIAN_POINT ( 'NONE',  ( 1.587926509186352142, 0.05413385826771666132, 0.4176697321401328100 ) ) ;
#25866 = ORIENTED_EDGE ( 'NONE', *, *, #80420, .T. ) ;
#25867 = CARTESIAN_POINT ( 'NONE',  ( -0.4724409448818895907, -0.1265901696524993070, -2.093175853018372834 ) ) ;
#25868 = CARTESIAN_POINT ( 'NONE',  ( 0.4153789062890288486, 1.308162955913704462, -1.721441067367122990 ) ) ;
#25869 = CARTESIAN_POINT ( 'NONE',  ( -0.3025410870193214197, 0.000000000000000000, 0.3464511005275205946 ) ) ;
#25870 = CARTESIAN_POINT ( 'NONE',  ( -1.082677165354329896, -0.4536011799217368745, -0.2665933059059886201 ) ) ;
#25871 = CARTESIAN_POINT ( 'NONE',  ( -1.318897637795274802, 0.1660481256975885056, 0.3530559997133364547 ) ) ;
#25872 = CARTESIAN_POINT ( 'NONE',  ( 0.5971128608923891301, 0.2952755905511810774, -0.1292274648535930714 ) ) ;
#25873 = ORIENTED_EDGE ( 'NONE', *, *, #15671, .F. ) ;
#25875 = CARTESIAN_POINT ( 'NONE',  ( 0.000000000000000000, 2.145669291338582418, 0.000000000000000000 ) ) ;
#25874 = CARTESIAN_POINT ( 'NONE',  ( 1.033875059083676717, 1.724409448818897905, 0.4359958488159722534 ) ) ;
#25876 = CARTESIAN_POINT ( 'NONE',  ( 1.397637795275591177, 0.1660481256975883668, -0.3530559997133364547 ) ) ;
#25877 = CARTESIAN_POINT ( 'NONE',  ( -1.666666666666665853, 0.05413385826771626580, -0.4176697321401330321 ) ) ;
#25878 = CARTESIAN_POINT ( 'NONE',  ( -0.1049643490035301746, -0.3917322834645670659, -0.7821329151892896236 ) ) ;
#25879 = CIRCLE ( 'NONE', #48784, 1.178877988035069047 ) ;
#25880 = CARTESIAN_POINT ( 'NONE',  ( -0.5839895013123351797, 0.1771653543307087075, -0.09757992244046823083 ) ) ;
#25881 = CARTESIAN_POINT ( 'NONE',  ( -1.213910761154854745, -0.5511811023622046335, 0.09757992244046803654 ) ) ;
#25882 = CARTESIAN_POINT ( 'NONE',  ( 0.2867679344610366554, -0.2867679344610365444, -0.9704724409448819422 ) ) ;
#25883 = CARTESIAN_POINT ( 'NONE',  ( -0.6889763779527552368, 0.07958543189024085140, 0.2665933059059887866 ) ) ;
#25884 = CARTESIAN_POINT ( 'NONE',  ( -0.09186351706036689768, -0.004921259842519870586, -0.3153832671262229437 ) ) ;
#25885 = EDGE_CURVE ( 'NONE', #47374, #19415, #35107, .T. ) ;
#25886 = CARTESIAN_POINT ( 'NONE',  ( 0.1968503937007881344, 0.2952755905511811885, 0.000000000000000000 ) ) ;
#25887 = CARTESIAN_POINT ( 'NONE',  ( -1.089238845144356427, -0.3690944881889765550, -0.3153832671262227771 ) ) ;
#25888 = CARTESIAN_POINT ( 'NONE',  ( 0.1958661417322836440, -0.3392501089628017219, -2.603674540682414218 ) ) ;
#25889 = CARTESIAN_POINT ( 'NONE',  ( 1.089238845144357537, -0.4281496062992124485, 0.4176697321401328655 ) ) ;
#25890 = ADVANCED_FACE ( 'NONE', ( #4875 ), #17934, .F. ) ;
#25891 = CARTESIAN_POINT ( 'NONE',  ( -1.502624671916009680, -0.3162353388693405765, 0.4822834645669290543 ) ) ;
#25892 = CARTESIAN_POINT ( 'NONE',  ( -0.3458507752293906723, -0.3458507752293910609, -1.080708661417322691 ) ) ;
#25893 = CARTESIAN_POINT ( 'NONE',  ( -0.3083989501312330295, -0.05778040916215522460, 0.4822834645669289988 ) ) ;
#25894 = CARTESIAN_POINT ( 'NONE',  ( -0.9055118110236215490, -0.6692913385826771977, 8.415575281601705876E-17 ) ) ;
#25895 = CARTESIAN_POINT ( 'NONE',  ( 0.9317585301837276734, -0.004921259842519870586, -0.3153832671262229437 ) ) ;
#25896 = CARTESIAN_POINT ( 'NONE',  ( -0.5052493438320203589, -0.5511811023622046335, 0.09757992244046803654 ) ) ;
#25897 = CARTESIAN_POINT ( 'NONE',  ( -0.4921259842519677963, -0.5400638737290844871, 0.3530559997133364547 ) ) ;
#25898 = CARTESIAN_POINT ( 'NONE',  ( -1.358267716535432434, -0.5400638737290844871, 0.3530559997133364547 ) ) ;
#25899 = CARTESIAN_POINT ( 'NONE',  ( -0.5120078740157480990, -0.3045572308828553565, -0.01849200668098333403 ) ) ;
#25900 = CARTESIAN_POINT ( 'NONE',  ( 1.181102362204725198, -0.1870078740157479769, 0.3641732283464567677 ) ) ;
#25901 = CARTESIAN_POINT ( 'NONE',  ( -0.4527559055118102749, -0.5400638737290845981, -0.3530559997133363437 ) ) ;
#25902 = CARTESIAN_POINT ( 'NONE',  ( -1.410761154855642463, -0.05778040916215522460, 0.4822834645669289988 ) ) ;
#25903 = ORIENTED_EDGE ( 'NONE', *, *, #6471, .T. ) ;
#25904 = CARTESIAN_POINT ( 'NONE',  ( 0.3996062992125986035, -0.1070741851644052972, -2.550524934383202158 ) ) ;
#25905 = EDGE_CURVE ( 'NONE', #66126, #45287, #62720, .T. ) ;
#25906 = CARTESIAN_POINT ( 'NONE',  ( -0.9186351706036736120, -0.5023911411419708095, -0.1820866141732282451 ) ) ;
#25907 = CARTESIAN_POINT ( 'NONE',  ( 0.7086614173228352742, -0.1870078740157480879, -0.4822834645669291653 ) ) ;
#25908 = CARTESIAN_POINT ( 'NONE',  ( -0.8595800524934373854, -0.2845877964562161244, -0.3641732283464567121 ) ) ;
#25909 = CARTESIAN_POINT ( 'NONE',  ( -0.2925321140481932369, 0.2925321140481931259, -1.356299212598425452 ) ) ;
#25910 = CARTESIAN_POINT ( 'NONE',  ( -1.030183727034119867, -0.05778040916215560624, -0.4822834645669293319 ) ) ;
#25911 = CARTESIAN_POINT ( 'NONE',  ( 0.9055118110236227702, 0.2952755905511811885, 0.000000000000000000 ) ) ;
#25912 = CARTESIAN_POINT ( 'NONE',  ( 0.5643044619422579178, 0.05413385826771666132, 0.4176697321401328100 ) ) ;
#25913 = EDGE_CURVE ( 'NONE', #47146, #31420, #81913, .T. ) ;
#25914 = CARTESIAN_POINT ( 'NONE',  ( 1.423884514435696191, -0.05778040916215522460, 0.4822834645669289988 ) ) ;
#25915 = CARTESIAN_POINT ( 'NONE',  ( -1.404199475065615932, -0.004921259842519576551, 0.3153832671262227771 ) ) ;
#25916 = CARTESIAN_POINT ( 'NONE',  ( -0.1070741851644051862, -0.3996062992125986035, -0.7788713910761155823 ) ) ;
#25917 = CARTESIAN_POINT ( 'NONE',  ( 0.3460692066303959202, 0.1998031496062993295, -0.9186351706036745002 ) ) ;
#25918 = CARTESIAN_POINT ( 'NONE',  ( 0.1974969037888706369, -0.3420746716998659953, -0.2493438320209974690 ) ) ;
#25919 = PRODUCT_DEFINITION ( 'UNKNOWN', '', #49063, #7487 ) ;
#25920 = AXIS2_PLACEMENT_3D ( 'NONE', #38536, #6132, #64217 ) ;
#25921 = CARTESIAN_POINT ( 'NONE',  ( 0.3256317079376986889, 1.192144240734427818, -1.710856511100560029 ) ) ;
#25922 = CARTESIAN_POINT ( 'NONE',  ( 1.010498687664042716, -0.3690944881889763329, 0.3153832671262228327 ) ) ;
#25923 = CARTESIAN_POINT ( 'NONE',  ( 0.2887139107611556010, -0.5023911411419708095, 0.1820866141732285504 ) ) ;
#25924 = CARTESIAN_POINT ( 'NONE',  ( 0.1902887139107617975, 0.2952755905511811885, 0.1292274648535926551 ) ) ;
#25925 = CARTESIAN_POINT ( 'NONE',  ( 1.496062992125984703, -0.1870078740157480879, -0.4822834645669291653 ) ) ;
#25926 = CARTESIAN_POINT ( 'NONE',  ( 0.3420746716998660508, 0.1974969037888705814, -1.467847769028871374 ) ) ;
#25927 = CARTESIAN_POINT ( 'NONE',  ( 0.4986876640419954376, -0.5023911411419708095, -0.1820866141732282451 ) ) ;
#25928 = CARTESIAN_POINT ( 'NONE',  ( -0.7939632545931750718, -0.05778040916215560624, -0.4822834645669293319 ) ) ;
#25929 = CARTESIAN_POINT ( 'NONE',  ( -1.443569553805773564, 0.2306618581243847221, -0.2411417322834647770 ) ) ;
#25930 = CARTESIAN_POINT ( 'NONE',  ( 0.6496062992125991586, -0.5400638737290845981, -0.3530559997133363437 ) ) ;
#25931 = CARTESIAN_POINT ( 'NONE',  ( 0.4724409448818898682, 2.892866454678787531E-17, -1.535433070866141669 ) ) ;
#25932 = CARTESIAN_POINT ( 'NONE',  ( 0.3996062992125985480, 0.1070741851644054637, -2.644356955380577467 ) ) ;
#25933 = ORIENTED_EDGE ( 'NONE', *, *, #3931, .F. ) ;
#25934 = ORIENTED_EDGE ( 'NONE', *, *, #13593, .F. ) ;
#25935 = CARTESIAN_POINT ( 'NONE',  ( -1.102362204724408601, -0.1870078740157479769, 0.4822834645669291653 ) ) ;
#25936 = CARTESIAN_POINT ( 'NONE',  ( -0.5905511811023613777, -0.6692913385826771977, 8.415575281601705876E-17 ) ) ;
#25938 = CARTESIAN_POINT ( 'NONE',  ( -0.8005249343832011588, 0.05413385826771626580, -0.4176697321401330321 ) ) ;
#25937 = CARTESIAN_POINT ( 'NONE',  ( -0.9645669291338575535, 0.07958543189024071263, -0.2665933059059888421 ) ) ;
#25939 = CARTESIAN_POINT ( 'NONE',  ( -0.3917322834645670659, 0.1049643490035301607, -2.002605356134171455 ) ) ;
#25941 = EDGE_CURVE ( 'NONE', #35211, #33346, #43570, .T. ) ;
#25940 = CARTESIAN_POINT ( 'NONE',  ( 0.1936066689571366572, -0.2229926280064456756, 0.1399704324547694778 ) ) ;
#25942 = CARTESIAN_POINT ( 'NONE',  ( -1.620734908136482577, 0.1771653543307087630, 0.09757992244046791164 ) ) ;
#25943 = CARTESIAN_POINT ( 'NONE',  ( -1.049868766404198794, 0.2306618581243847221, -0.2411417322834647770 ) ) ;
#25944 = CARTESIAN_POINT ( 'NONE',  ( 0.2427821522309716595, -0.3162353388693409650, -0.4822834645669289433 ) ) ;
#25945 = CARTESIAN_POINT ( 'NONE',  ( -0.8136482939632537770, 0.2306618581243847221, -0.2411417322834647770 ) ) ;
#25946 = CARTESIAN_POINT ( 'NONE',  ( 0.2867679344610365999, 0.2867679344610365999, -1.547244094488189115 ) ) ;
#25947 = CARTESIAN_POINT ( 'NONE',  ( -0.9580052493438311334, -0.004921259842519870586, -0.3153832671262229437 ) ) ;
#25948 = ORIENTED_EDGE ( 'NONE', *, *, #4963, .F. ) ;
#25949 = CARTESIAN_POINT ( 'NONE',  ( 4.837279021331060870E-17, -0.3949938075777409963, -1.968503937007873850 ) ) ;
#25950 = EDGE_LOOP ( 'NONE', ( #48533, #38568, #69253, #17816 ) ) ;
#25951 = CARTESIAN_POINT ( 'NONE',  ( -1.620734908136482577, -0.5511811023622048555, -0.09757992244046775898 ) ) ;
#25952 = CARTESIAN_POINT ( 'NONE',  ( -1.246719160104986512, 0.05413385826771666132, 0.4176697321401328100 ) ) ;
#25953 = CARTESIAN_POINT ( 'NONE',  ( -0.8727034120734901146, -0.3162353388693405765, 0.4822834645669290543 ) ) ;
#25954 = CARTESIAN_POINT ( 'NONE',  ( -0.3460692066303960868, 0.1998031496062990242, -0.3412073490813647969 ) ) ;
#25955 = CARTESIAN_POINT ( 'NONE',  ( -0.9776902887139098386, -0.6692913385826771977, 0.1292274648535927661 ) ) ;
#25956 = CARTESIAN_POINT ( 'NONE',  ( -1.430446194225721390, -0.4281496062992124485, 0.4176697321401328655 ) ) ;
#25957 =( NAMED_UNIT ( * ) SI_UNIT ( $, .STERADIAN. ) SOLID_ANGLE_UNIT ( ) );
#25958 = DIRECTION ( 'NONE',  ( -0.000000000000000000, -1.000000000000000000, -0.000000000000000000 ) ) ;
#25959 = CARTESIAN_POINT ( 'NONE',  ( 0.6036745406824154392, 0.1283753931104746893, -0.1820866141732285504 ) ) ;
#25960 = CARTESIAN_POINT ( 'NONE',  ( 2.094141031014985721, 1.724409448818900570, -0.4359958488159719758 ) ) ;
#25961 = CARTESIAN_POINT ( 'NONE',  ( 0.3917322834645670104, -0.1049643490035303411, -0.1961942257217848817 ) ) ;
#25962 = CARTESIAN_POINT ( 'NONE',  ( -0.4199475065616791736, 0.1283753931104746893, -0.1820866141732285504 ) ) ;
#25963 = CARTESIAN_POINT ( 'NONE',  ( -0.7414698162729651543, -0.6692913385826771977, 0.1292274648535927661 ) ) ;
#25964 = CARTESIAN_POINT ( 'NONE',  ( 1.515748031496063186, -0.5400638737290845981, -0.3530559997133363437 ) ) ;
#25965 = CARTESIAN_POINT ( 'NONE',  ( -0.6364829396325453192, -0.05778040916215560624, -0.4822834645669293319 ) ) ;
#25966 = VERTEX_POINT ( 'NONE', #37278 ) ;
#25967 = ORIENTED_EDGE ( 'NONE', *, *, #80626, .T. ) ;
#25968 = CARTESIAN_POINT ( 'NONE',  ( 0.2925321140481932369, 0.2925321140481932369, -2.104330708661417138 ) ) ;
#25969 = CARTESIAN_POINT ( 'NONE',  ( -1.108923884514435132, -0.05778040916215560624, -0.4822834645669293319 ) ) ;
#25970 = CARTESIAN_POINT ( 'NONE',  ( 1.423884514435696191, -0.05778040916215522460, 0.4822834645669289988 ) ) ;
#25971 = CARTESIAN_POINT ( 'NONE',  ( -1.161417322834644716, -0.4536011799217368745, -0.2665933059059886201 ) ) ;
#25972 = CARTESIAN_POINT ( 'NONE',  ( -1.384514435695537005, 0.2952755905511811885, 0.1292274648535926551 ) ) ;
#25973 = CARTESIAN_POINT ( 'NONE',  ( 0.4091458600556404646, -0.2362204724409448231, -0.7349081364829396223 ) ) ;
#25974 = EDGE_CURVE ( 'NONE', #27710, #74865, #26353, .T. ) ;
#25975 = CARTESIAN_POINT ( 'NONE',  ( 2.114058874202384253, 1.379859446982308446, 0.4477348144951676656 ) ) ;
#25976 = CARTESIAN_POINT ( 'NONE',  ( 0.1958661417322834775, 0.3392501089628018884, -0.1364829396325459021 ) ) ;
#25977 = DIRECTION ( 'NONE',  ( 1.000000000000000000, 0.000000000000000000, 3.455050906509825972E-15 ) ) ;
#25978 = CARTESIAN_POINT ( 'NONE',  ( -0.02624671916010428221, 0.2306618581243847221, -0.2411417322834647770 ) ) ;
#25979 = CARTESIAN_POINT ( 'NONE',  ( -1.154855643044618851, 0.1283753931104748280, 0.1820866141732283561 ) ) ;
#25980 = CARTESIAN_POINT ( 'NONE',  ( -0.6955380577427815458, -0.4281496062992127816, -0.4176697321401328100 ) ) ;
#25981 = CARTESIAN_POINT ( 'NONE',  ( 0.4724409448818896462, 0.1265901696524990294, -2.721128608923884418 ) ) ;
#25982 = CARTESIAN_POINT ( 'NONE',  ( -1.423884514435694859, -0.3162353388693405765, 0.4822834645669290543 ) ) ;
#25983 = CARTESIAN_POINT ( 'NONE',  ( -1.167979002624671470, -0.4281496062992127816, -0.4176697321401328100 ) ) ;
#25984 = CARTESIAN_POINT ( 'NONE',  ( 0.1377952755905518800, -0.5400638737290844871, 0.3530559997133364547 ) ) ;
#25985 = CARTESIAN_POINT ( 'NONE',  ( 0.1974969037888704704, 0.3420746716998660508, -2.740813648293963567 ) ) ;
#25986 = CARTESIAN_POINT ( 'NONE',  ( 1.030183727034121421, -0.2845877964562161244, -0.3641732283464567121 ) ) ;
#25987 = CARTESIAN_POINT ( 'NONE',  ( -0.6364829396325453192, -0.2845877964562159024, 0.3641732283464567677 ) ) ;
#25988 = CARTESIAN_POINT ( 'NONE',  ( -0.03443470937343537375, 1.064243487142137568, -1.440673310089392478 ) ) ;
#25989 = AXIS2_PLACEMENT_3D ( 'NONE', #52506, #45774, #772 ) ;
#25990 = CARTESIAN_POINT ( 'NONE',  ( 0.6299212598425204535, -0.1870078740157480601, -0.3641732283464567677 ) ) ;
#25991 = CARTESIAN_POINT ( 'NONE',  ( 1.515748031496063186, -0.4536011799217368745, -0.2665933059059886201 ) ) ;
#25992 = CARTESIAN_POINT ( 'NONE',  ( 1.194225721784777594, -0.4281496062992127816, -0.4176697321401328100 ) ) ;
#25993 = UNCERTAINTY_MEASURE_WITH_UNIT (LENGTH_MEASURE( 1.000000000000000082E-05 ), #57438, 'distance_accuracy_value', 'NONE');
#25994 = CARTESIAN_POINT ( 'NONE',  ( -0.06561679790026180015, -0.004921259842519576551, 0.3153832671262227771 ) ) ;
#25995 = CARTESIAN_POINT ( 'NONE',  ( -0.1958661417322834220, -0.3392501089628018884, -1.317585301837270295 ) ) ;
#25996 = CARTESIAN_POINT ( 'NONE',  ( -1.030183727034119867, -0.3162353388693405765, 0.4822834645669290543 ) ) ;
#25997 = CARTESIAN_POINT ( 'NONE',  ( 1.437007874015748810, 0.1660481256975885056, 0.3530559997133364547 ) ) ;
#25998 = ADVANCED_FACE ( 'NONE', ( #52367 ), #63764, .F. ) ;
#25999 = CARTESIAN_POINT ( 'NONE',  ( 0.4091458600556404646, -0.2362204724409448231, 0.1332020997375328031 ) ) ;
#26000 = CARTESIAN_POINT ( 'NONE',  ( -0.5249343832020990641, 0.1283753931104748280, 0.1820866141732283561 ) ) ;
#26001 = CARTESIAN_POINT ( 'NONE',  ( 0.5249343832021005074, -0.6046776061558807314, 0.2411417322834647770 ) ) ;
#26002 = CARTESIAN_POINT ( 'NONE',  ( 0.000000000000000000, 0.000000000000000000, -1.512162153811850596 ) ) ;
#26003 = AXIS2_PLACEMENT_3D ( 'NONE', #21610, #59078, #46855 ) ;
#26004 = CARTESIAN_POINT ( 'NONE',  ( 1.003937007874016185, 0.07958543189024071263, -0.2665933059059888421 ) ) ;
#26005 = CARTESIAN_POINT ( 'NONE',  ( 0.01312335958005323398, -0.004921259842519576551, 0.3153832671262227771 ) ) ;
#26006 = CARTESIAN_POINT ( 'NONE',  ( 0.2952755905511819101, 0.1660481256975883668, -0.3530559997133364547 ) ) ;
#26007 = CARTESIAN_POINT ( 'NONE',  ( -1.318897637795274802, -0.5400638737290845981, -0.3530559997133363437 ) ) ;
#26008 = CARTESIAN_POINT ( 'NONE',  ( -0.8267716535433065062, 0.1771653543307087630, 0.000000000000000000 ) ) ;
#26009 = FACE_OUTER_BOUND ( 'NONE', #63041, .T. ) ;
#26010 = CARTESIAN_POINT ( 'NONE',  ( -0.9776902887139098386, 0.2952755905511810774, -0.1292274648535930714 ) ) ;
#26011 = CARTESIAN_POINT ( 'NONE',  ( 0.1998031496062994128, -0.3460692066303957537, -1.113517060367454015 ) ) ;
#26012 = CARTESIAN_POINT ( 'NONE',  ( 0.3917322834645670104, 2.398668435337828261E-17, -2.564960629921259727 ) ) ;
#26013 = CARTESIAN_POINT ( 'NONE',  ( 0.2099737532808405305, 0.1283753931104746893, -0.1820866141732285504 ) ) ;
#26014 = CARTESIAN_POINT ( 'NONE',  ( -0.6299212598425188991, -0.1870078740157480879, -0.4822834645669291653 ) ) ;
#26015 = CARTESIAN_POINT ( 'NONE',  ( -1.089238845144356427, -0.4281496062992127816, -0.4176697321401328100 ) ) ;
#26016 = CARTESIAN_POINT ( 'NONE',  ( -1.062992125984250968, -0.5511811023622047445, 6.969142054262312111E-17 ) ) ;
#26017 = CARTESIAN_POINT ( 'NONE',  ( 1.541994750656168645, 0.2952755905511810774, -0.1292274648535930714 ) ) ;
#26018 = CARTESIAN_POINT ( 'NONE',  ( -0.8792650918635160906, -0.3690944881889763329, 0.3153832671262228327 ) ) ;
#26019 = CARTESIAN_POINT ( 'NONE',  ( -1.692913385826770645, 0.1771653543307087630, 0.000000000000000000 ) ) ;
#26020 = CARTESIAN_POINT ( 'NONE',  ( 1.489501312335958172, -0.05778040916215560624, -0.4822834645669293319 ) ) ;
#26021 = CARTESIAN_POINT ( 'NONE',  ( -0.3996062992125986035, -7.340648628747425578E-17, 0.1181102362204724254 ) ) ;
#26022 = CARTESIAN_POINT ( 'NONE',  ( 0.3917322834645670104, 0.1049643490035304660, -2.011174171424884083 ) ) ;
#26023 = ORIENTED_EDGE ( 'NONE', *, *, #28811, .T. ) ;
#26024 = CARTESIAN_POINT ( 'NONE',  ( 0.2362204724409449064, 0.000000000000000000, 0.1279527559055117503 ) ) ;
#26025 = CARTESIAN_POINT ( 'NONE',  ( 1.404199475065617264, -0.3690944881889763329, 0.3153832671262228327 ) ) ;
#26026 = CARTESIAN_POINT ( 'NONE',  ( -1.122047244094487306, -0.5400638737290844871, 0.3530559997133364547 ) ) ;
#26027 = CARTESIAN_POINT ( 'NONE',  ( 1.161417322834646271, 0.1660481256975883668, -0.3530559997133364547 ) ) ;
#26028 = CARTESIAN_POINT ( 'NONE',  ( -0.2867679344610364334, -0.2867679344610367109, -2.190944881889763440 ) ) ;
#26029 = DIRECTION ( 'NONE',  ( -0.000000000000000000, 1.000000000000000000, -0.000000000000000000 ) ) ;
#26030 = CARTESIAN_POINT ( 'NONE',  ( 0.5708661417322842269, 0.1660481256975885056, 0.3530559997133364547 ) ) ;
#26031 = CARTESIAN_POINT ( 'NONE',  ( -0.05249343832020911260, 0.2306618581243848609, 0.2411417322834645549 ) ) ;
#26032 = CARTESIAN_POINT ( 'NONE',  ( -0.6967283859536032020, -3.965272662620685221E-15, 0.3627989612356152249 ) ) ;
#26033 = LINE ( 'NONE', #58013, #14355 ) ;
#26034 = CARTESIAN_POINT ( 'NONE',  ( 0.6692913385826777528, 0.1771653543307087630, 0.000000000000000000 ) ) ;
#26035 = EDGE_CURVE ( 'NONE', #36796, #25632, #22143, .T. ) ;
#26036 = CARTESIAN_POINT ( 'NONE',  ( -9.787531504996567848E-17, 0.3996062992125986035, -1.417322834645669216 ) ) ;
#26037 = ORIENTED_EDGE ( 'NONE', *, *, #60455, .T. ) ;
#26038 = CARTESIAN_POINT ( 'NONE',  ( -0.2867679344610365444, -0.2867679344610367664, -0.05579359399706226158 ) ) ;
#26039 = ORIENTED_EDGE ( 'NONE', *, *, #61973, .T. ) ;
#26040 = CARTESIAN_POINT ( 'NONE',  ( 0.1443569553805781891, -0.4281496062992124485, 0.4176697321401328655 ) ) ;
#26041 = CARTESIAN_POINT ( 'NONE',  ( -1.404199475065615932, -0.4281496062992127816, -0.4176697321401328100 ) ) ;
#26042 = CARTESIAN_POINT ( 'NONE',  ( 0.5052493438320218022, -0.6692913385826773087, -0.1292274648535924053 ) ) ;
#26043 = VECTOR ( 'NONE', #36845, 39.37007874015748143 ) ;
#26044 = CARTESIAN_POINT ( 'NONE',  ( 1.207349081364829990, 0.2306618581243848609, 0.2411417322834645549 ) ) ;
#26046 = ADVANCED_FACE ( 'NONE', ( #44384 ), #82720, .T. ) ;
#26045 = CARTESIAN_POINT ( 'NONE',  ( 1.397637795275591177, -0.5400638737290844871, 0.3530559997133364547 ) ) ;
#26047 = CARTESIAN_POINT ( 'NONE',  ( -0.3871391076115476282, -0.05778040916215522460, 0.4822834645669289988 ) ) ;
#26048 = CARTESIAN_POINT ( 'NONE',  ( -0.1837270341207343505, -0.6046776061558807314, 0.2411417322834647770 ) ) ;
#26049 = CARTESIAN_POINT ( 'NONE',  ( 1.443569553805774897, 0.2306618581243848609, 0.2411417322834645549 ) ) ;
#26050 = CARTESIAN_POINT ( 'NONE',  ( 1.502624671916010790, -0.3162353388693409650, -0.4822834645669289433 ) ) ;
#26051 = CARTESIAN_POINT ( 'NONE',  ( 1.259842519685040019, -0.1870078740157480879, -0.4822834645669291653 ) ) ;
#26052 = CARTESIAN_POINT ( 'NONE',  ( -0.3149606299212590610, -0.1870078740157479769, 0.4822834645669291653 ) ) ;
#26053 = CARTESIAN_POINT ( 'NONE',  ( -0.3392501089628017219, -0.1958661417322836718, -0.04461942257217842850 ) ) ;
#26054 = CARTESIAN_POINT ( 'NONE',  ( 0.2624671916010504757, 0.1283753931104748280, 0.1820866141732283561 ) ) ;
#26055 = ORIENTED_EDGE ( 'NONE', *, *, #63009, .T. ) ;
#26056 = CARTESIAN_POINT ( 'NONE',  ( 0.3949938075777411073, -0.1058382717557499464, -0.5839895013123359568 ) ) ;
#26057 = ORIENTED_EDGE ( 'NONE', *, *, #36412, .T. ) ;
#26058 = CARTESIAN_POINT ( 'NONE',  ( -0.5839895013123351797, 0.1771653543307087075, -0.09757992244046823083 ) ) ;
#26059 = FACE_OUTER_BOUND ( 'NONE', #77693, .T. ) ;
#26060 = CARTESIAN_POINT ( 'NONE',  ( 0.3149606299212603933, -0.1870078740157479769, 0.4822834645669291653 ) ) ;
#26061 = CARTESIAN_POINT ( 'NONE',  ( 0.1902887139107617975, 0.2952755905511811885, 0.1292274648535926551 ) ) ;
#26062 = CARTESIAN_POINT ( 'NONE',  ( -0.8398950131233589023, -0.6046776061558809534, -0.2411417322834644161 ) ) ;
#26063 = VECTOR ( 'NONE', #8835, 39.37007874015748854 ) ;
#26064 = CARTESIAN_POINT ( 'NONE',  ( -9.594673741351313045E-17, 0.3917322834645670659, -1.729021940453755013 ) ) ;
#26065 = CARTESIAN_POINT ( 'NONE',  ( -1.345144356955379816, -0.3162353388693405765, 0.4822834645669290543 ) ) ;
#26066 = CARTESIAN_POINT ( 'NONE',  ( 0.3917322834645670104, 2.398668435337828261E-17, -2.879921259842519454 ) ) ;
#26067 = CARTESIAN_POINT ( 'NONE',  ( 1.043307086614173818, -0.4536011799217368745, -0.2665933059059886201 ) ) ;
#26068 = CARTESIAN_POINT ( 'NONE',  ( 0.3280839895013130669, -0.4281496062992127816, -0.4176697321401328100 ) ) ;
#26069 = CARTESIAN_POINT ( 'NONE',  ( 0.5905511811023629321, 0.2952755905511811885, 0.000000000000000000 ) ) ;
#26070 = CARTESIAN_POINT ( 'NONE',  ( 0.2925321140481932369, 0.2925321140481932369, -1.397637795275590067 ) ) ;
#26071 = CARTESIAN_POINT ( 'NONE',  ( -2.594411373832338441, 1.668416680336019198, 0.4562095852119718575 ) ) ;
#26072 = CARTESIAN_POINT ( 'NONE',  ( 0.2925321140481932369, -0.2925321140481931814, -0.6476377952755905110 ) ) ;
#26073 = CARTESIAN_POINT ( 'NONE',  ( -0.2925321140481930149, -0.2925321140481933480, -0.2933070866141732069 ) ) ;
#26074 = CARTESIAN_POINT ( 'NONE',  ( -0.3215223097112853146, -0.3162353388693405765, 0.4822834645669290543 ) ) ;
#26075 = CARTESIAN_POINT ( 'NONE',  ( -0.3996062992125986035, -0.1070741851644056997, -2.880577427821522374 ) ) ;
#26076 = CARTESIAN_POINT ( 'NONE',  ( 0.2867679344610365999, 0.2867679344610365999, -1.954724409448818978 ) ) ;
#26077 = CARTESIAN_POINT ( 'NONE',  ( -1.338582677165353729, -0.1870078740157479769, 0.3641732283464567677 ) ) ;
#26078 = CARTESIAN_POINT ( 'NONE',  ( 1.476377952755906220, 0.1660481256975883668, -0.3530559997133364547 ) ) ;
#26079 = CARTESIAN_POINT ( 'NONE',  ( 1.167979002624672580, -0.4281496062992124485, 0.4176697321401328655 ) ) ;
#26080 = CARTESIAN_POINT ( 'NONE',  ( 0.2755905511811031494, 0.1771653543307087630, 0.000000000000000000 ) ) ;
#26081 = CARTESIAN_POINT ( 'NONE',  ( 0.4790026246719167324, -0.05778040916215522460, 0.4822834645669289988 ) ) ;
#26082 = CARTESIAN_POINT ( 'NONE',  ( 0.2362204724409449064, 0.4091458600556404646, -1.638451443569553634 ) ) ;
#26083 = CARTESIAN_POINT ( 'NONE',  ( 0.4921259842519691285, -0.4536011799217368745, -0.2665933059059886201 ) ) ;
#26084 = CARTESIAN_POINT ( 'NONE',  ( 0.1377952755905518800, -0.5400638737290844871, 0.3530559997133364547 ) ) ;
#26085 = CARTESIAN_POINT ( 'NONE',  ( -0.2891555358219911054, 0.2891555358219909388, -1.356299212598425230 ) ) ;
#26086 = CARTESIAN_POINT ( 'NONE',  ( -1.213910761154854745, 0.2952755905511810774, -0.1292274648535930714 ) ) ;
#26087 = CARTESIAN_POINT ( 'NONE',  ( 0.5118110236220478892, 0.1771653543307087630, 0.000000000000000000 ) ) ;
#26088 = CARTESIAN_POINT ( 'NONE',  ( -1.220472440944882386, -0.1870078740157480046, 1.254653134982923898E-17 ) ) ;
#26089 = CARTESIAN_POINT ( 'NONE',  ( -0.5314960629921254842, -0.5400638737290845981, -0.3530559997133363437 ) ) ;
#26090 = CARTESIAN_POINT ( 'NONE',  ( -0.2559055118110227234, -0.4536011799217367080, 0.2665933059059888421 ) ) ;
#26091 = LINE ( 'NONE', #39562, #38585 ) ;
#26092 = CARTESIAN_POINT ( 'NONE',  ( -0.3215223097112853146, -0.3162353388693405765, 0.4822834645669290543 ) ) ;
#26093 = CARTESIAN_POINT ( 'NONE',  ( -0.4265091863517051496, -0.6692913385826771977, 0.1292274648535927661 ) ) ;
#26094 = CARTESIAN_POINT ( 'NONE',  ( 0.3608923884514443348, 0.1771653543307087075, -0.09757992244046823083 ) ) ;
#26095 = CARTESIAN_POINT ( 'NONE',  ( -0.1998031496062994405, 0.3460692066303957537, -2.294619422572178546 ) ) ;
#26096 = CARTESIAN_POINT ( 'NONE',  ( -0.1902887139107604098, 0.2952755905511810774, -0.1292274648535930714 ) ) ;
#26097 = CARTESIAN_POINT ( 'NONE',  ( 0.1958661417322836162, -0.3392501089628018329, -1.589219529362517758 ) ) ;
#26098 = CARTESIAN_POINT ( 'NONE',  ( 0.8333333333333340365, -0.5511811023622046335, 0.09757992244046803654 ) ) ;
#26099 = CARTESIAN_POINT ( 'NONE',  ( 1.253280839895013710, -0.3162353388693405765, 0.4822834645669290543 ) ) ;
#26100 = CARTESIAN_POINT ( 'NONE',  ( -0.7283464566929126471, 0.07958543189024071263, -0.2665933059059888421 ) ) ;
#26101 = CARTESIAN_POINT ( 'NONE',  ( -0.6561679790026240244, -0.5023911411419708095, 0.1820866141732285504 ) ) ;
#26102 = CARTESIAN_POINT ( 'NONE',  ( -0.6364829396325453192, -0.05778040916215560624, -0.4822834645669293319 ) ) ;
#26103 = CARTESIAN_POINT ( 'NONE',  ( -0.2230971128608915943, -0.4281496062992127816, -0.4176697321401328100 ) ) ;
#26104 = CARTESIAN_POINT ( 'NONE',  ( 0.7480314960629927956, 0.1771653543307087630, 0.000000000000000000 ) ) ;
#26105 = CARTESIAN_POINT ( 'NONE',  ( -1.157146581871515012E-16, 0.4724409448818898682, -2.362204724409448620 ) ) ;
#26106 = CARTESIAN_POINT ( 'NONE',  ( 1.154855643044620184, 0.1283753931104746893, -0.1820866141732285504 ) ) ;
#26107 = VECTOR ( 'NONE', #54146, 39.37007874015748143 ) ;
#26108 = CARTESIAN_POINT ( 'NONE',  ( 0.9317585301837276734, 0.05413385826771626580, -0.4176697321401330321 ) ) ;
#26109 = CARTESIAN_POINT ( 'NONE',  ( -0.1070741851644056997, 0.3996062992125984925, 0.07414698162729659037 ) ) ;
#26110 = CARTESIAN_POINT ( 'NONE',  ( -0.2952755905511804668, 0.1660481256975885056, 0.3530559997133364547 ) ) ;
#26111 = CARTESIAN_POINT ( 'NONE',  ( 0.1958661417322836440, -0.3392501089628017219, -1.278871391076115582 ) ) ;
#26112 = CARTESIAN_POINT ( 'NONE',  ( 1.502624671916010790, -0.2845877964562161244, -0.3641732283464567121 ) ) ;
#26113 = CARTESIAN_POINT ( 'NONE',  ( 0.4921259842519691285, -0.5400638737290845981, -0.3530559997133363437 ) ) ;
#26114 = CARTESIAN_POINT ( 'NONE',  ( 0.2230971128608932319, -0.4281496062992124485, 0.4176697321401328655 ) ) ;
#26115 = CARTESIAN_POINT ( 'NONE',  ( -0.4709442531824371558, -0.03757601356356778805, -1.220472440944882164 ) ) ;
#26116 = CARTESIAN_POINT ( 'NONE',  ( 0.4790026246719168435, -0.2845877964562161244, -0.3641732283464567121 ) ) ;
#26117 = CARTESIAN_POINT ( 'NONE',  ( 0.8398950131233602345, -0.6046776061558807314, 0.2411417322834647770 ) ) ;
#26118 = CARTESIAN_POINT ( 'NONE',  ( -0.2624671916010490880, 0.1283753931104746893, -0.1820866141732285504 ) ) ;
#26119 = TOROIDAL_SURFACE ( 'NONE', #7326, 3.858267716535433323, 0.07874015748031495954 ) ;
#26120 = CARTESIAN_POINT ( 'NONE',  ( -0.7939632545931750718, -0.05778040916215560624, -0.4822834645669293319 ) ) ;
#26121 = CYLINDRICAL_SURFACE ( 'NONE', #82439, 0.4724409448818898682 ) ;
#26122 = CARTESIAN_POINT ( 'NONE',  ( -0.2165354330708654795, -0.5400638737290845981, -0.3530559997133363437 ) ) ;
#26123 = CARTESIAN_POINT ( 'NONE',  ( -1.102362204724408601, -0.1870078740157480879, -0.4822834645669291653 ) ) ;
#26124 = CARTESIAN_POINT ( 'NONE',  ( -0.7808398950131225646, -0.08942795157527998196, 0.3641732283464567121 ) ) ;
#26125 = CARTESIAN_POINT ( 'NONE',  ( 0.5314960629921264834, 0.1660481256975883668, -0.3530559997133364547 ) ) ;
#26126 = CARTESIAN_POINT ( 'NONE',  ( -1.391076115485563758, 0.2306618581243848609, 0.2411417322834645549 ) ) ;
#26127 = CARTESIAN_POINT ( 'NONE',  ( -0.4921259842519677963, 0.1660481256975883668, -0.3530559997133364547 ) ) ;
#26128 = DIRECTION ( 'NONE',  ( -1.000000000000000000, 0.000000000000000000, 0.000000000000000000 ) ) ;
#26129 = CARTESIAN_POINT ( 'NONE',  ( 1.351706036745407458, -0.4281496062992127816, -0.4176697321401328100 ) ) ;
#26130 = CARTESIAN_POINT ( 'NONE',  ( 1.240157480314961314, 0.1660481256975883668, -0.3530559997133364547 ) ) ;
#26131 = CARTESIAN_POINT ( 'NONE',  ( 0.3917322834645669549, 0.1049643490035304660, -2.321522309711285814 ) ) ;
#26132 = CARTESIAN_POINT ( 'NONE',  ( 0.4606732211678724598, 1.763126522798933227, -0.5309055118110237448 ) ) ;
#26133 = CARTESIAN_POINT ( 'NONE',  ( -1.115485564304461219, -0.4281496062992124485, 0.4176697321401328655 ) ) ;
#26134 = CARTESIAN_POINT ( 'NONE',  ( 0.3458507752293908943, -0.3458507752293908943, -0.7283464566929134243 ) ) ;
#26135 = EDGE_CURVE ( 'NONE', #72153, #49485, #32193, .T. ) ;
#26136 = CARTESIAN_POINT ( 'NONE',  ( 0.3996062992125986590, -0.1070741851644053111, 0.04593175853018371252 ) ) ;
#26137 = ORIENTED_EDGE ( 'NONE', *, *, #52927, .T. ) ;
#26138 = CARTESIAN_POINT ( 'NONE',  ( 0.03280839895013198948, -0.5511811023622048555, -0.09757992244046775898 ) ) ;
#26139 = CARTESIAN_POINT ( 'NONE',  ( 0.3392501089628018329, 0.1958661417322835607, -1.855643044619422533 ) ) ;
#26140 = ORIENTED_EDGE ( 'NONE', *, *, #37551, .T. ) ;
#26141 = CARTESIAN_POINT ( 'NONE',  ( 0.3280839895013130669, 0.05413385826771666132, 0.4176697321401328100 ) ) ;
#26142 = CARTESIAN_POINT ( 'NONE',  ( 0.5314960629921264834, 0.1660481256975883668, -0.3530559997133364547 ) ) ;
#26143 = CARTESIAN_POINT ( 'NONE',  ( 0.1265901696524990294, -0.4724409448818896462, -2.919947506561679784 ) ) ;
#26144 = CARTESIAN_POINT ( 'NONE',  ( 2.795275590551181910, 1.805669738366189048, 0.000000000000000000 ) ) ;
#26145 = CARTESIAN_POINT ( 'NONE',  ( -0.2821522309711278487, -0.5511811023622048555, -0.09757992244046775898 ) ) ;
#26146 = CARTESIAN_POINT ( 'NONE',  ( -0.2199809220305531665, -0.1970133122064496867, 0.1374248322900812891 ) ) ;
#26147 = CARTESIAN_POINT ( 'NONE',  ( 0.9580052493438327987, -0.4281496062992127816, -0.4176697321401328100 ) ) ;
#26148 = CARTESIAN_POINT ( 'NONE',  ( 1.076115485564305141, -0.5023911411419708095, 0.1820866141732285504 ) ) ;
#26149 = CARTESIAN_POINT ( 'NONE',  ( -0.5183727034120726440, 0.2952755905511811885, 0.1292274648535926551 ) ) ;
#26150 = CARTESIAN_POINT ( 'NONE',  ( -0.3392501089628019439, 0.1958661417322832554, -1.051161786580365742 ) ) ;
#26151 = CARTESIAN_POINT ( 'NONE',  ( -0.9973753280839886548, 0.2306618581243848609, 0.2411417322834645549 ) ) ;
#26152 = CARTESIAN_POINT ( 'NONE',  ( -1.437007874015747477, -0.4536011799217367080, 0.2665933059059888421 ) ) ;
#26153 = CARTESIAN_POINT ( 'NONE',  ( -1.030183727034119867, -0.05778040916215560624, -0.4822834645669293319 ) ) ;
#26154 = CARTESIAN_POINT ( 'NONE',  ( 1.187664041994751285, -0.05778040916215522460, 0.4822834645669289988 ) ) ;
#26155 = DIRECTION ( 'NONE',  ( 0.000000000000000000, 0.000000000000000000, 1.000000000000000000 ) ) ;
#26156 = ORIENTED_EDGE ( 'NONE', *, *, #54694, .T. ) ;
#26157 = CARTESIAN_POINT ( 'NONE',  ( 4.797336870675656522E-17, -0.3917322834645670659, -2.595163672737219596 ) ) ;
#26158 = CARTESIAN_POINT ( 'NONE',  ( -0.03937007874015669567, 0.2952755905511811885, 0.000000000000000000 ) ) ;
#26159 = ORIENTED_EDGE ( 'NONE', *, *, #54850, .F. ) ;
#26160 = CARTESIAN_POINT ( 'NONE',  ( -0.8070866141732276899, -0.5400638737290844871, 0.3530559997133364547 ) ) ;
#26161 = CARTESIAN_POINT ( 'NONE',  ( 1.541994750656168645, -0.6692913385826771977, 0.1292274648535927661 ) ) ;
#26162 = CARTESIAN_POINT ( 'NONE',  ( 1.076115485564305141, -0.6046776061558807314, 0.2411417322834647770 ) ) ;
#26163 =( BOUNDED_SURFACE ( )  B_SPLINE_SURFACE ( 1, 2, ( 
 ( #79887, #73566, #9580, #16321, #29751, #35661, #48692, #80303, #22618, #79062, #61746, #47033, #53758, #22205, #68072, #15491, #9996, #48277, #41966, #80711, #28104, #41148, #23026, #67248, #74390, #16734, #66837, #9171, #34842, #10417, #36075, #8751, #60505, #34425, #2853, #47861, #15910, #28517, #36896, #50338, #10820, #81533, #25075, #56651, #57060, #49102, #4913, #30582, #82753, #76449, #4496, #55826, #63389, #56248, #37313, #76035, #50749, #18776, #36480, #18380, #44419, #44021, #70114, #69714, #12465, #63801, #49520, #17966, #81944, #81121, #11654, #74806, #17153, #42786, #5724, #23853, #24670, #82352, #24257, #75628, #62155, #62986, #31395, #6139, #68481, #30163, #43603, #68886, #12058, #55414, #5325, #62572, #37715, #49930, #75213, #38127, #23438, #17557, #69305, #43190, #11236, #30983, #64224, #33068, #32230, #71794, #57888, #6558, #1100, #65903, #38544, #39800, #25488, #71373, #20866, #26751, #65062, #78541, #7400, #72218, #40221, #38955, #6976, #26329, #45677, #52406, #31814, #14147, #1513, #13723, #58738, #57474, #14569, #83168, #255, #32645, #46516, #12884, #25907, #51567, #77270, #19599, #45262, #27167, #39377, #78115, #51154, #76849, #19182, #70958, #58310, #44831, #13303, #64639, #675, #51991, #77696, #20026, #20448, #46101, #65494, #7826, #33493, #59155, #52829, #70529, #54076, #54495, #35155, #14974, #34325, #53662, #80206, #47767, #79791, #59987, #67563, #73040, #60406, #9075, #60815, #15389, #3167, #46934, #2346, #61229, #9480, #9895, #1925, #41051, #66736, #35566, #29249, #40633, #8654, #16222, #34746, #73465, #28831, #3582, #54913, #72626, #22523, #80619, #48185, #22931, #73882, #48597, #16639, #28002, #22107, #2757, #33905, #15817, #27588, #53245, #78960, #41869, #79369, #74293, #42279, #28416, #41466, #66315, #67151, #8239, #59569, #21279, #21688, #47351, #81441, #37214, #76355, #24166, #49429, #24578, #75123, #42696, #24979, #67977, #11557, #30486, #29659, #61654, #62063, #17056, #69208, #68393, #50245, #10732, #36389, #62893, #18687, #74710, #75941, #3995, #49835, #56966, #5228, #17874, #31302, #43508, #50652, #10319, #17468, #43099, #62475, #81855, #30892, #35984, #18282, #56559, #36799, #82664, #55321, #81030, #23342, #63297, #49013, #82260, #4402, #68795, #30070, #55733, #23755, #43924, #56151, #11140, #4810, #69621, #75534, #11966, #37621, #5635, #57791, #59060, #38032, #12374, #63707, #32548, #12790, #52312, #27071, #51059, #51471, #52730, #64129, #25811, #71276, #77174, #33398, #64964, #76759, #83074, #6464, #6047, #45583, #31719, #158, #57379, #25395, #19089, #78019, #20347, #45999, #1415, #32134, #13625, #71695, #70433, #45159, #14049, #39703, #39277, #64541, #44330, #7300, #578, #44738, #38446, #19505, #78441, #19934, #70021, #70863, #13214, #38860, #6878, #77600, #65395, #32969, #58637, #7730, #58212, #26232, #1004, #51895, #26659, #78857, #59473, #40123, #55937, #53144, #80104, #33808, #66218, #3065, #40539, #27486, #15709, #16118, #60716, #53977, #2657, #9791, #9380, #66632, #73782, #48080, #28732, #21182, #54393, #79689, #60308, #28316, #46837, #2240, #1826, #72531, #14879, #20767, #22423, #34643, #27905, #8557, #41764, #22006, #53565, #72940, #34225, #73361, #47666, #79274, #40952, #59886, #41366, #67457, #46420, #65810, #8143, #8969, #21589, #67047, #30274, #35050, #47251, #35463, #15292, #61127, #3478, #72112, #14470, #44131, #43300, #75323, #75737, #30695, #82869, #82057, #38240, #24371, #56359, #50859, #32344, #5027, #6252, #17669, #37830, #70647, #76559, #31512, #44950, #57171, #38658, #6672, #5435, #56762, #76148, #12172, #18887, #81652, #63916, #51267, #63506, #25193, #23963, #64335, #49629, #50041, #82462, #13002, #62685, #18078, #43713, #69415, #11769, #37423, #63096, #12581, #5838, #44536, #70227, #31095, #24778, #31929, #69823, #57591, #83281, #50446, #18488, #25604, #76969, #19299, #68997, #11349, #37007, #39497, #26865, #58858, #1623, #65185, #52940, #13416, #792, #27700, #59266, #59679, #51685, #7521, #33190, #2035, #79074, #7093, #58430, #66015, #1216, #39921, #78654, #53364, #21390, #39073 ),
 ( #77387, #8351, #52105, #32763, #27280, #26451, #14678, #77813, #20144, #20975, #8762, #64754, #34019, #19719, #14263, #47046, #46634, #7941, #72738, #33603, #15085, #66427, #52526, #78232, #20566, #71913, #72330, #58005, #40334, #40743, #65611, #370, #26025, #45377, #71074, #45793, #46217, #71491, #13839, #9182, #60516, #2865, #66849, #41160, #34854, #48703, #16334, #35672, #23037, #28528, #54185, #16746, #80315, #80723, #61337, #79899, #22217, #47873, #74402, #73988, #22630, #73577, #10429, #15923, #3276, #35261, #3690, #41570, #29355, #73153, #67260, #4094, #55014, #36086, #28115, #9593, #60926, #61757, #55425, #28939, #54606, #42385, #48291, #41977, #68084, #29763, #81133, #15502, #23449, #49114, #74819, #17164, #42798, #68492, #34437, #67671, #10007, #60103, #2457, #53769, #79482, #21796, #47460, #44433, #36908, #63402, #37728, #69317, #30995, #75225, #50350, #70127, #44845, #55837, #30174, #82364, #24270, #5738, #19196, #76048, #75640, #50762, #17979, #68897, #51167, #10831, #31409, #56664, #81546, #4506, #57073, #6153, #76463, #44034, #18392, #83181, #82767, #24683, #63814, #38142, #18789, #11250, #12478, #69726, #12071, #25089, #62584, #43616, #17569, #4926, #30594, #36491, #31827, #57488, #11668, #56260, #25502, #76864, #37326, #62998, #62167, #5337, #23864, #49531, #43202, #81956, #49942, #33916, #33504, #45276, #77709, #6572, #32243, #32658, #46115, #58751, #13736, #52004, #27178, #38557, #59581, #1524, #7414, #687, #1938, #64237, #57902, #268, #1113, #38969, #78553, #53260, #77283, #20039, #78971, #6990, #45690, #14160, #71387, #27600, #7837, #19614, #25923, #58325, #51581, #71809, #70971, #26343, #13316, #64652, #39392, #20878, #46530, #72230, #21292, #65076, #39816, #14579, #33084, #26764, #40232, #65915, #65505, #52419, #70543, #59166, #78128, #20462, #52842, #8251, #12898, #22536, #29671, #40644, #60002, #9087, #34759, #80220, #54925, #48199, #67575, #22943, #28013, #79804, #73894, #67164, #46945, #21700, #2357, #66328, #81042, #79381, #48610, #53673, #60419, #29261, #66753, #47363, #73054, #80632, #9494, #9907, #16234, #15404, #41064, #2770, #35579, #3180, #35167, #28429, #74305, #54089, #15831, #47779, #41881, #22120, #61242, #73481, #41479, #16652, #3596, #42292, #8666, #60828, #28844, #67989, #10334, #54506, #35996, #61666, #4007, #55333, #72637, #14985, #34337, #4414, #18294, #18700, #11978, #38044, #69633, #63720, #31731, #17480, #69221, #81866, #49026, #62905, #42708, #68404, #10744, #56979, #49441, #75956, #50258, #24178, #43523, #30083, #5240, #82676, #57396, #36401, #62076, #11569, #36812, #43939, #23355, #30904, #4822, #63309, #30500, #81453, #6060, #74722, #37633, #37228, #55745, #17071, #43111, #23770, #24590, #75135, #5647, #68807, #11154, #31314, #62488, #56163, #24993, #49847, #56571, #12386, #50667, #82272, #70033, #76367, #75546, #17886, #44342, #58223, #77612, #13636, #20360, #8153, #39714, #52743, #39289, #1016, #83086, #65820, #51071, #57804, #590, #72123, #64144, #170, #25823, #51483, #32147, #6478, #77186, #14060, #64975, #26669, #71706, #19518, #45171, #70877, #7743, #26246, #7312, #46010, #1425, #20777, #13226, #78030, #78451, #65405, #14481, #33408, #40135, #33818, #38875, #45595, #51905, #25408, #32981, #19101, #44750, #70446, #59070, #64553, #52324, #27081, #19945, #71289, #6891, #58649, #46431, #76770, #12803, #38458, #32560, #72952, #28745, #67891, #15724, #40966, #16131, #66648, #34237, #16551, #59484, #3081, #22019, #21192, #53154, #53575, #8567, #60729, #59898, #41777, #2250, #27916, #54407, #10228, #66229, #67471, #78866, #41379, #48503, #80118, #9393, #22844, #35064, #42195, #1838, #8984, #34657, #53991, #73374, #22436, #27498, #9805, #29158, #67060, #48096, #46846, #72541, #14888, #79284, #60321, #74204, #40548, #21601, #47262, #15303, #2670, #28329, #79703, #73795, #35477, #61141, #3493, #47679, #54828, #80533, #81766, #82172, #62806, #42606, #61974, #81351, #24489, #75445, #24076, #4312, #11881, #17381, #4717, #36705, #5140, #43011, #30805, #74623, #29976, #5548, #37122, #37533, #29569, #68705 ) ),
 .UNSPECIFIED., .F., .F., .F. ) 
 B_SPLINE_SURFACE_WITH_KNOTS ( ( 2, 2 ),
 ( 3, 2, 2, 2, 2, 2, 2, 2, 2, 2, 2, 2, 2, 2, 2, 2, 2, 2, 2, 2, 2, 2, 2, 2, 2, 2, 2, 2, 2, 2, 2, 2, 2, 2, 2, 2, 2, 2, 2, 2, 2, 2, 2, 2, 2, 2, 2, 2, 2, 2, 2, 2, 2, 2, 2, 2, 2, 2, 2, 2, 2, 2, 2, 2, 2, 2, 2, 2, 2, 2, 2, 2, 2, 2, 2, 2, 2, 2, 2, 2, 2, 2, 2, 2, 2, 2, 2, 2, 2, 2, 2, 2, 2, 2, 2, 2, 2, 2, 2, 2, 2, 2, 2, 2, 2, 2, 2, 2, 2, 2, 2, 2, 2, 2, 2, 2, 2, 2, 2, 2, 2, 2, 2, 2, 2, 2, 2, 2, 2, 2, 2, 2, 2, 2, 2, 2, 2, 2, 2, 2, 2, 2, 2, 2, 2, 2, 2, 2, 2, 2, 2, 2, 2, 2, 2, 2, 2, 2, 2, 2, 2, 2, 2, 2, 2, 2, 2, 2, 2, 2, 2, 2, 2, 2, 2, 2, 2, 2, 2, 2, 2, 2, 2, 2, 2, 2, 2, 2, 2, 2, 2, 2, 2, 2, 2, 2, 2, 2, 2, 2, 2, 2, 2, 2, 2, 2, 2, 2, 2, 2, 2, 2, 2, 2, 2, 2, 2, 2, 2, 2, 2, 2, 2, 2, 2, 2, 2, 2, 2, 2, 2, 2, 2, 2, 2, 2, 2, 2, 2, 2, 2, 2, 2, 2, 2, 2, 2, 2, 2, 2, 2, 2, 2, 2, 2, 3 ),
 ( 0.000000000000000000, 1.000000000000000000 ),
 ( 0.000000000000000000, 0.003787878787878787984, 0.007575757575757575968, 0.01136363636363636395, 0.01515151515151515194, 0.01893939393939393992, 0.02272727272727272790, 0.02651515151515151589, 0.03030303030303030387, 0.03409090909090908839, 0.03787878787878787984, 0.04166666666666666435, 0.04545454545454545581, 0.04924242424242424032, 0.05303030303030303177, 0.05681818181818181629, 0.06060606060606060774, 0.06439393939393939226, 0.06818181818181817677, 0.07196969696969697516, 0.07575757575757575968, 0.07954545454545454419, 0.08333333333333332871, 0.08712121212121212710, 0.09090909090909091161, 0.09469696969696969613, 0.09848484848484848064, 0.1022727272727272790, 0.1060606060606060635, 0.1098484848484848481, 0.1136363636363636326, 0.1174242424242424310, 0.1212121212121212155, 0.1250000000000000000, 0.1287878787878787845, 0.1325757575757575690, 0.1363636363636363535, 0.1401515151515151381, 0.1439393939393939503, 0.1477272727272727348, 0.1515151515151515194, 0.1553030303030303039, 0.1590909090909090884, 0.1628787878787878729, 0.1666666666666666574, 0.1704545454545454419, 0.1742424242424242542, 0.1780303030303030387, 0.1818181818181818232, 0.1856060606060606077, 0.1893939393939393923, 0.1931818181818181768, 0.1969696969696969613, 0.2007575757575757458, 0.2045454545454545581, 0.2083333333333333426, 0.2121212121212121271, 0.2159090909090909116, 0.2196969696969696961, 0.2234848484848484806, 0.2272727272727272652, 0.2310606060606060497, 0.2348484848484848619, 0.2386363636363636465, 0.2424242424242424310, 0.2462121212121212155, 0.2500000000000000000, 0.2537878787878787845, 0.2575757575757575690, 0.2613636363636363535, 0.2651515151515151381, 0.2689393939393939226, 0.2727272727272727071, 0.2765151515151514916, 0.2803030303030302761, 0.2840909090909091161, 0.2878787878787879007, 0.2916666666666666852, 0.2954545454545454697, 0.2992424242424242542, 0.3030303030303030387, 0.3068181818181818232, 0.3106060606060606077, 0.3143939393939393923, 0.3181818181818181768, 0.3219696969696969613, 0.3257575757575757458, 0.3295454545454545303, 0.3333333333333333148, 0.3371212121212120993, 0.3409090909090908839, 0.3446969696969697239, 0.3484848484848485084, 0.3522727272727272929, 0.3560606060606060774, 0.3598484848484848619, 0.3636363636363636465, 0.3674242424242424310, 0.3712121212121212155, 0.3750000000000000000, 0.3787878787878787845, 0.3825757575757575690, 0.3863636363636363535, 0.3901515151515151381, 0.3939393939393939226, 0.3977272727272727071, 0.4015151515151514916, 0.4053030303030302761, 0.4090909090909091161, 0.4128787878787879007, 0.4166666666666666852, 0.4204545454545454697, 0.4242424242424242542, 0.4280303030303030387, 0.4318181818181818232, 0.4356060606060606077, 0.4393939393939393923, 0.4431818181818181768, 0.4469696969696969613, 0.4507575757575757458, 0.4545454545454545303, 0.4583333333333333148, 0.4621212121212120993, 0.4659090909090908839, 0.4696969696969697239, 0.4734848484848485084, 0.4772727272727272929, 0.4810606060606060774, 0.4848484848484848619, 0.4886363636363636465, 0.4924242424242424310, 0.4962121212121212155, 0.5000000000000000000, 0.5037878787878787845, 0.5075757575757575690, 0.5113636363636363535, 0.5151515151515151381, 0.5189393939393939226, 0.5227272727272727071, 0.5265151515151514916, 0.5303030303030302761, 0.5340909090909090606, 0.5378787878787878451, 0.5416666666666666297, 0.5454545454545454142, 0.5492424242424241987, 0.5530303030303029832, 0.5568181818181817677, 0.5606060606060605522, 0.5643939393939394478, 0.5681818181818182323, 0.5719696969696970168, 0.5757575757575758013, 0.5795454545454545858, 0.5833333333333333703, 0.5871212121212121549, 0.5909090909090909394, 0.5946969696969697239, 0.5984848484848485084, 0.6022727272727272929, 0.6060606060606060774, 0.6098484848484848619, 0.6136363636363636465, 0.6174242424242424310, 0.6212121212121212155, 0.6250000000000000000, 0.6287878787878787845, 0.6325757575757575690, 0.6363636363636363535, 0.6401515151515151381, 0.6439393939393939226, 0.6477272727272727071, 0.6515151515151514916, 0.6553030303030302761, 0.6590909090909090606, 0.6628787878787878451, 0.6666666666666666297, 0.6704545454545454142, 0.6742424242424241987, 0.6780303030303029832, 0.6818181818181817677, 0.6856060606060605522, 0.6893939393939394478, 0.6931818181818182323, 0.6969696969696970168, 0.7007575757575758013, 0.7045454545454545858, 0.7083333333333333703, 0.7121212121212121549, 0.7159090909090909394, 0.7196969696969697239, 0.7234848484848485084, 0.7272727272727272929, 0.7310606060606060774, 0.7348484848484848619, 0.7386363636363636465, 0.7424242424242424310, 0.7462121212121212155, 0.7500000000000000000, 0.7537878787878787845, 0.7575757575757575690, 0.7613636363636363535, 0.7651515151515151381, 0.7689393939393939226, 0.7727272727272727071, 0.7765151515151514916, 0.7803030303030302761, 0.7840909090909090606, 0.7878787878787878451, 0.7916666666666666297, 0.7954545454545454142, 0.7992424242424241987, 0.8030303030303029832, 0.8068181818181817677, 0.8106060606060605522, 0.8143939393939394478, 0.8181818181818182323, 0.8219696969696970168, 0.8257575757575758013, 0.8295454545454545858, 0.8333333333333333703, 0.8371212121212121549, 0.8409090909090909394, 0.8446969696969697239, 0.8484848484848485084, 0.8522727272727272929, 0.8560606060606060774, 0.8598484848484848619, 0.8636363636363636465, 0.8674242424242424310, 0.8712121212121212155, 0.8750000000000000000, 0.8787878787878787845, 0.8825757575757575690, 0.8863636363636363535, 0.8901515151515151381, 0.8939393939393939226, 0.8977272727272727071, 0.9015151515151514916, 0.9053030303030302761, 0.9090909090909090606, 0.9128787878787878451, 0.9166666666666666297, 0.9204545454545454142, 0.9242424242424241987, 0.9280303030303029832, 0.9318181818181817677, 0.9356060606060605522, 0.9393939393939394478, 0.9431818181818182323, 0.9469696969696970168, 0.9507575757575758013, 0.9545454545454545858, 0.9583333333333333703, 0.9621212121212121549, 0.9659090909090909394 ),
 .UNSPECIFIED. ) 
 GEOMETRIC_REPRESENTATION_ITEM ( )  RATIONAL_B_SPLINE_SURFACE ( (
 ( 1.000000000000000000, 0.9659258262890683122, 1.000000000000000000, 0.9659258262890683122, 1.000000000000000000, 0.9659258262890683122, 1.000000000000000000, 0.9659258262890683122, 1.000000000000000000, 0.9659258262890683122, 1.000000000000000000, 0.9659258262890683122, 1.000000000000000000, 0.9659258262890683122, 1.000000000000000000, 0.9659258262890683122, 1.000000000000000000, 0.9659258262890683122, 1.000000000000000000, 0.9659258262890683122, 1.000000000000000000, 0.9659258262890683122, 1.000000000000000000, 0.9659258262890683122, 1.000000000000000000, 0.9659258262890683122, 1.000000000000000000, 0.9659258262890683122, 1.000000000000000000, 0.9659258262890683122, 1.000000000000000000, 0.9659258262890683122, 1.000000000000000000, 0.9659258262890683122, 1.000000000000000000, 0.9659258262890683122, 1.000000000000000000, 0.9659258262890683122, 1.000000000000000000, 0.9659258262890683122, 1.000000000000000000, 0.9659258262890683122, 1.000000000000000000, 0.9659258262890683122, 1.000000000000000000, 0.9659258262890683122, 1.000000000000000000, 0.9659258262890683122, 1.000000000000000000, 0.9659258262890683122, 1.000000000000000000, 0.9659258262890683122, 1.000000000000000000, 0.9659258262890683122, 1.000000000000000000, 0.9659258262890683122, 1.000000000000000000, 0.9659258262890683122, 1.000000000000000000, 0.9659258262890683122, 1.000000000000000000, 0.9659258262890683122, 1.000000000000000000, 0.9659258262890683122, 1.000000000000000000, 0.9659258262890683122, 1.000000000000000000, 0.9659258262890683122, 1.000000000000000000, 0.9659258262890683122, 1.000000000000000000, 0.9659258262890683122, 1.000000000000000000, 0.9659258262890683122, 1.000000000000000000, 0.9659258262890683122, 1.000000000000000000, 0.9659258262890683122, 1.000000000000000000, 0.9659258262890683122, 1.000000000000000000, 0.9659258262890683122, 1.000000000000000000, 0.9659258262890683122, 1.000000000000000000, 0.9659258262890683122, 1.000000000000000000, 0.9659258262890683122, 1.000000000000000000, 0.9659258262890683122, 1.000000000000000000, 0.9659258262890683122, 1.000000000000000000, 0.9659258262890683122, 1.000000000000000000, 0.9659258262890683122, 1.000000000000000000, 0.9659258262890683122, 1.000000000000000000, 0.9659258262890683122, 1.000000000000000000, 0.9659258262890683122, 1.000000000000000000, 0.9659258262890683122, 1.000000000000000000, 0.9659258262890683122, 1.000000000000000000, 0.9659258262890683122, 1.000000000000000000, 0.9659258262890683122, 1.000000000000000000, 0.9659258262890683122, 1.000000000000000000, 0.9659258262890683122, 1.000000000000000000, 0.9659258262890683122, 1.000000000000000000, 0.9659258262890683122, 1.000000000000000000, 0.9659258262890683122, 1.000000000000000000, 0.9659258262890683122, 1.000000000000000000, 0.9659258262890683122, 1.000000000000000000, 0.9659258262890683122, 1.000000000000000000, 0.9659258262890683122, 1.000000000000000000, 0.9659258262890683122, 1.000000000000000000, 0.9659258262890683122, 1.000000000000000000, 0.9659258262890683122, 1.000000000000000000, 0.9659258262890683122, 1.000000000000000000, 0.9659258262890683122, 1.000000000000000000, 0.9659258262890683122, 1.000000000000000000, 0.9659258262890683122, 1.000000000000000000, 0.9659258262890683122, 1.000000000000000000, 0.9659258262890683122, 1.000000000000000000, 0.9659258262890683122, 1.000000000000000000, 0.9659258262890683122, 1.000000000000000000, 0.9659258262890683122, 1.000000000000000000, 0.9659258262890683122, 1.000000000000000000, 0.9659258262890683122, 1.000000000000000000, 0.9659258262890683122, 1.000000000000000000, 0.9659258262890683122, 1.000000000000000000, 0.9659258262890683122, 1.000000000000000000, 0.9659258262890683122, 1.000000000000000000, 0.9659258262890683122, 1.000000000000000000, 0.9659258262890683122, 1.000000000000000000, 0.9659258262890683122, 1.000000000000000000, 0.9659258262890683122, 1.000000000000000000, 0.9659258262890683122, 1.000000000000000000, 0.9659258262890683122, 1.000000000000000000, 0.9659258262890683122, 1.000000000000000000, 0.9659258262890683122, 1.000000000000000000, 0.9659258262890683122, 1.000000000000000000, 0.9659258262890683122, 1.000000000000000000, 0.9659258262890683122, 1.000000000000000000, 0.9659258262890683122, 1.000000000000000000, 0.9659258262890683122, 1.000000000000000000, 0.9659258262890683122, 1.000000000000000000, 0.9659258262890683122, 1.000000000000000000, 0.9659258262890683122, 1.000000000000000000, 0.9659258262890683122, 1.000000000000000000, 0.9659258262890683122, 1.000000000000000000, 0.9659258262890683122, 1.000000000000000000, 0.9659258262890683122, 1.000000000000000000, 0.9659258262890683122, 1.000000000000000000, 0.9659258262890683122, 1.000000000000000000, 0.9659258262890683122, 1.000000000000000000, 0.9659258262890683122, 1.000000000000000000, 0.9659258262890683122, 1.000000000000000000, 0.9659258262890683122, 1.000000000000000000, 0.9659258262890683122, 1.000000000000000000, 0.9659258262890683122, 1.000000000000000000, 0.9659258262890683122, 1.000000000000000000, 0.9659258262890683122, 1.000000000000000000, 0.9659258262890683122, 1.000000000000000000, 0.9659258262890683122, 1.000000000000000000, 0.9659258262890683122, 1.000000000000000000, 0.9659258262890683122, 1.000000000000000000, 0.9659258262890683122, 1.000000000000000000, 0.9659258262890683122, 1.000000000000000000, 0.9659258262890683122, 1.000000000000000000, 0.9659258262890683122, 1.000000000000000000, 0.9659258262890683122, 1.000000000000000000, 0.9659258262890683122, 1.000000000000000000, 0.9659258262890683122, 1.000000000000000000, 0.9659258262890683122, 1.000000000000000000, 0.9659258262890683122, 1.000000000000000000, 0.9659258262890683122, 1.000000000000000000, 0.9659258262890683122, 1.000000000000000000, 0.9659258262890683122, 1.000000000000000000, 0.9659258262890683122, 1.000000000000000000, 0.9659258262890683122, 1.000000000000000000, 0.9659258262890683122, 1.000000000000000000, 0.9659258262890683122, 1.000000000000000000, 0.9659258262890683122, 1.000000000000000000, 0.9659258262890683122, 1.000000000000000000, 0.9659258262890683122, 1.000000000000000000, 0.9659258262890683122, 1.000000000000000000, 0.9659258262890683122, 1.000000000000000000, 0.9659258262890683122, 1.000000000000000000, 0.9659258262890683122, 1.000000000000000000, 0.9659258262890683122, 1.000000000000000000, 0.9659258262890683122, 1.000000000000000000, 0.9659258262890683122, 1.000000000000000000, 0.9659258262890683122, 1.000000000000000000, 0.9659258262890683122, 1.000000000000000000, 0.9659258262890683122, 1.000000000000000000, 0.9659258262890683122, 1.000000000000000000, 0.9659258262890683122, 1.000000000000000000, 0.9659258262890683122, 1.000000000000000000, 0.9659258262890683122, 1.000000000000000000, 0.9659258262890683122, 1.000000000000000000, 0.9659258262890683122, 1.000000000000000000, 0.9659258262890683122, 1.000000000000000000, 0.9659258262890683122, 1.000000000000000000, 0.9659258262890683122, 1.000000000000000000, 0.9659258262890683122, 1.000000000000000000, 0.9659258262890683122, 1.000000000000000000, 0.9659258262890683122, 1.000000000000000000, 0.9659258262890683122, 1.000000000000000000, 0.9659258262890683122, 1.000000000000000000, 0.9659258262890683122, 1.000000000000000000, 0.9659258262890683122, 1.000000000000000000, 0.9659258262890683122, 1.000000000000000000, 0.9659258262890683122, 1.000000000000000000, 0.9659258262890683122, 1.000000000000000000, 0.9659258262890683122, 1.000000000000000000, 0.9659258262890683122, 1.000000000000000000, 0.9659258262890683122, 1.000000000000000000, 0.9659258262890683122, 1.000000000000000000, 0.9659258262890683122, 1.000000000000000000, 0.9659258262890683122, 1.000000000000000000, 0.9659258262890683122, 1.000000000000000000, 0.9659258262890683122, 1.000000000000000000, 0.9659258262890683122, 1.000000000000000000, 0.9659258262890683122, 1.000000000000000000, 0.9659258262890683122, 1.000000000000000000, 0.9659258262890683122, 1.000000000000000000, 0.9659258262890683122, 1.000000000000000000, 0.9659258262890683122, 1.000000000000000000, 0.9659258262890683122, 1.000000000000000000, 0.9659258262890683122, 1.000000000000000000, 0.9659258262890683122, 1.000000000000000000, 0.9659258262890683122, 1.000000000000000000, 0.9659258262890683122, 1.000000000000000000, 0.9659258262890683122, 1.000000000000000000, 0.9659258262890683122, 1.000000000000000000, 0.9659258262890683122, 1.000000000000000000, 0.9659258262890683122, 1.000000000000000000, 0.9659258262890683122, 1.000000000000000000, 0.9659258262890683122, 1.000000000000000000, 0.9659258262890683122, 1.000000000000000000, 0.9659258262890683122, 1.000000000000000000, 0.9659258262890683122, 1.000000000000000000, 0.9659258262890683122, 1.000000000000000000, 0.9659258262890683122, 1.000000000000000000, 0.9659258262890683122, 1.000000000000000000, 0.9659258262890683122, 1.000000000000000000, 0.9659258262890683122, 1.000000000000000000, 0.9659258262890683122, 1.000000000000000000, 0.9659258262890683122, 1.000000000000000000, 0.9659258262890683122, 1.000000000000000000, 0.9659258262890683122, 1.000000000000000000, 0.9659258262890683122, 1.000000000000000000, 0.9659258262890683122, 1.000000000000000000, 0.9659258262890683122, 1.000000000000000000, 0.9659258262890683122, 1.000000000000000000, 0.9659258262890683122, 1.000000000000000000, 0.9659258262890683122, 1.000000000000000000, 0.9659258262890683122, 1.000000000000000000, 0.9659258262890683122, 1.000000000000000000, 0.9659258262890683122, 1.000000000000000000, 0.9659258262890683122, 1.000000000000000000, 0.9659258262890683122, 1.000000000000000000, 0.9659258262890683122, 1.000000000000000000, 0.9659258262890683122, 1.000000000000000000, 0.9659258262890683122, 1.000000000000000000, 0.9659258262890683122, 1.000000000000000000, 0.9659258262890683122, 1.000000000000000000, 0.9659258262890683122, 1.000000000000000000, 0.9659258262890683122, 1.000000000000000000, 0.9659258262890683122, 1.000000000000000000, 0.9659258262890683122, 1.000000000000000000, 0.9659258262890683122, 1.000000000000000000, 0.9659258262890683122, 1.000000000000000000, 0.9659258262890683122, 1.000000000000000000, 0.9659258262890683122, 1.000000000000000000, 0.9659258262890683122, 1.000000000000000000, 0.9659258262890683122, 1.000000000000000000, 0.9659258262890683122, 1.000000000000000000, 0.9659258262890683122, 1.000000000000000000, 0.9659258262890683122, 1.000000000000000000, 0.9659258262890683122, 1.000000000000000000, 0.9659258262890683122, 1.000000000000000000, 0.9659258262890683122, 1.000000000000000000, 0.9659258262890683122, 1.000000000000000000, 0.9659258262890683122, 1.000000000000000000, 0.9659258262890683122, 1.000000000000000000, 0.9659258262890683122, 1.000000000000000000, 0.9659258262890683122, 1.000000000000000000, 0.9659258262890683122, 1.000000000000000000, 0.9659258262890683122, 1.000000000000000000, 0.9659258262890683122, 1.000000000000000000, 0.9659258262890683122, 1.000000000000000000, 0.9659258262890683122, 1.000000000000000000, 0.9659258262890683122, 1.000000000000000000, 0.9659258262890683122, 1.000000000000000000, 0.9659258262890683122, 1.000000000000000000, 0.9659258262890683122, 1.000000000000000000, 0.9659258262890683122, 1.000000000000000000, 0.9659258262890683122, 1.000000000000000000, 0.9659258262890683122, 1.000000000000000000, 0.9659258262890683122, 1.000000000000000000, 0.9659258262890683122, 1.000000000000000000, 0.9659258262890683122, 1.000000000000000000, 0.9659258262890683122, 1.000000000000000000, 0.9659258262890683122, 1.000000000000000000),
 ( 1.000000000000000000, 0.9659258262890683122, 1.000000000000000000, 0.9659258262890683122, 1.000000000000000000, 0.9659258262890683122, 1.000000000000000000, 0.9659258262890683122, 1.000000000000000000, 0.9659258262890683122, 1.000000000000000000, 0.9659258262890683122, 1.000000000000000000, 0.9659258262890683122, 1.000000000000000000, 0.9659258262890683122, 1.000000000000000000, 0.9659258262890683122, 1.000000000000000000, 0.9659258262890683122, 1.000000000000000000, 0.9659258262890683122, 1.000000000000000000, 0.9659258262890683122, 1.000000000000000000, 0.9659258262890683122, 1.000000000000000000, 0.9659258262890683122, 1.000000000000000000, 0.9659258262890683122, 1.000000000000000000, 0.9659258262890683122, 1.000000000000000000, 0.9659258262890683122, 1.000000000000000000, 0.9659258262890683122, 1.000000000000000000, 0.9659258262890683122, 1.000000000000000000, 0.9659258262890683122, 1.000000000000000000, 0.9659258262890683122, 1.000000000000000000, 0.9659258262890683122, 1.000000000000000000, 0.9659258262890683122, 1.000000000000000000, 0.9659258262890683122, 1.000000000000000000, 0.9659258262890683122, 1.000000000000000000, 0.9659258262890683122, 1.000000000000000000, 0.9659258262890683122, 1.000000000000000000, 0.9659258262890683122, 1.000000000000000000, 0.9659258262890683122, 1.000000000000000000, 0.9659258262890683122, 1.000000000000000000, 0.9659258262890683122, 1.000000000000000000, 0.9659258262890683122, 1.000000000000000000, 0.9659258262890683122, 1.000000000000000000, 0.9659258262890683122, 1.000000000000000000, 0.9659258262890683122, 1.000000000000000000, 0.9659258262890683122, 1.000000000000000000, 0.9659258262890683122, 1.000000000000000000, 0.9659258262890683122, 1.000000000000000000, 0.9659258262890683122, 1.000000000000000000, 0.9659258262890683122, 1.000000000000000000, 0.9659258262890683122, 1.000000000000000000, 0.9659258262890683122, 1.000000000000000000, 0.9659258262890683122, 1.000000000000000000, 0.9659258262890683122, 1.000000000000000000, 0.9659258262890683122, 1.000000000000000000, 0.9659258262890683122, 1.000000000000000000, 0.9659258262890683122, 1.000000000000000000, 0.9659258262890683122, 1.000000000000000000, 0.9659258262890683122, 1.000000000000000000, 0.9659258262890683122, 1.000000000000000000, 0.9659258262890683122, 1.000000000000000000, 0.9659258262890683122, 1.000000000000000000, 0.9659258262890683122, 1.000000000000000000, 0.9659258262890683122, 1.000000000000000000, 0.9659258262890683122, 1.000000000000000000, 0.9659258262890683122, 1.000000000000000000, 0.9659258262890683122, 1.000000000000000000, 0.9659258262890683122, 1.000000000000000000, 0.9659258262890683122, 1.000000000000000000, 0.9659258262890683122, 1.000000000000000000, 0.9659258262890683122, 1.000000000000000000, 0.9659258262890683122, 1.000000000000000000, 0.9659258262890683122, 1.000000000000000000, 0.9659258262890683122, 1.000000000000000000, 0.9659258262890683122, 1.000000000000000000, 0.9659258262890683122, 1.000000000000000000, 0.9659258262890683122, 1.000000000000000000, 0.9659258262890683122, 1.000000000000000000, 0.9659258262890683122, 1.000000000000000000, 0.9659258262890683122, 1.000000000000000000, 0.9659258262890683122, 1.000000000000000000, 0.9659258262890683122, 1.000000000000000000, 0.9659258262890683122, 1.000000000000000000, 0.9659258262890683122, 1.000000000000000000, 0.9659258262890683122, 1.000000000000000000, 0.9659258262890683122, 1.000000000000000000, 0.9659258262890683122, 1.000000000000000000, 0.9659258262890683122, 1.000000000000000000, 0.9659258262890683122, 1.000000000000000000, 0.9659258262890683122, 1.000000000000000000, 0.9659258262890683122, 1.000000000000000000, 0.9659258262890683122, 1.000000000000000000, 0.9659258262890683122, 1.000000000000000000, 0.9659258262890683122, 1.000000000000000000, 0.9659258262890683122, 1.000000000000000000, 0.9659258262890683122, 1.000000000000000000, 0.9659258262890683122, 1.000000000000000000, 0.9659258262890683122, 1.000000000000000000, 0.9659258262890683122, 1.000000000000000000, 0.9659258262890683122, 1.000000000000000000, 0.9659258262890683122, 1.000000000000000000, 0.9659258262890683122, 1.000000000000000000, 0.9659258262890683122, 1.000000000000000000, 0.9659258262890683122, 1.000000000000000000, 0.9659258262890683122, 1.000000000000000000, 0.9659258262890683122, 1.000000000000000000, 0.9659258262890683122, 1.000000000000000000, 0.9659258262890683122, 1.000000000000000000, 0.9659258262890683122, 1.000000000000000000, 0.9659258262890683122, 1.000000000000000000, 0.9659258262890683122, 1.000000000000000000, 0.9659258262890683122, 1.000000000000000000, 0.9659258262890683122, 1.000000000000000000, 0.9659258262890683122, 1.000000000000000000, 0.9659258262890683122, 1.000000000000000000, 0.9659258262890683122, 1.000000000000000000, 0.9659258262890683122, 1.000000000000000000, 0.9659258262890683122, 1.000000000000000000, 0.9659258262890683122, 1.000000000000000000, 0.9659258262890683122, 1.000000000000000000, 0.9659258262890683122, 1.000000000000000000, 0.9659258262890683122, 1.000000000000000000, 0.9659258262890683122, 1.000000000000000000, 0.9659258262890683122, 1.000000000000000000, 0.9659258262890683122, 1.000000000000000000, 0.9659258262890683122, 1.000000000000000000, 0.9659258262890683122, 1.000000000000000000, 0.9659258262890683122, 1.000000000000000000, 0.9659258262890683122, 1.000000000000000000, 0.9659258262890683122, 1.000000000000000000, 0.9659258262890683122, 1.000000000000000000, 0.9659258262890683122, 1.000000000000000000, 0.9659258262890683122, 1.000000000000000000, 0.9659258262890683122, 1.000000000000000000, 0.9659258262890683122, 1.000000000000000000, 0.9659258262890683122, 1.000000000000000000, 0.9659258262890683122, 1.000000000000000000, 0.9659258262890683122, 1.000000000000000000, 0.9659258262890683122, 1.000000000000000000, 0.9659258262890683122, 1.000000000000000000, 0.9659258262890683122, 1.000000000000000000, 0.9659258262890683122, 1.000000000000000000, 0.9659258262890683122, 1.000000000000000000, 0.9659258262890683122, 1.000000000000000000, 0.9659258262890683122, 1.000000000000000000, 0.9659258262890683122, 1.000000000000000000, 0.9659258262890683122, 1.000000000000000000, 0.9659258262890683122, 1.000000000000000000, 0.9659258262890683122, 1.000000000000000000, 0.9659258262890683122, 1.000000000000000000, 0.9659258262890683122, 1.000000000000000000, 0.9659258262890683122, 1.000000000000000000, 0.9659258262890683122, 1.000000000000000000, 0.9659258262890683122, 1.000000000000000000, 0.9659258262890683122, 1.000000000000000000, 0.9659258262890683122, 1.000000000000000000, 0.9659258262890683122, 1.000000000000000000, 0.9659258262890683122, 1.000000000000000000, 0.9659258262890683122, 1.000000000000000000, 0.9659258262890683122, 1.000000000000000000, 0.9659258262890683122, 1.000000000000000000, 0.9659258262890683122, 1.000000000000000000, 0.9659258262890683122, 1.000000000000000000, 0.9659258262890683122, 1.000000000000000000, 0.9659258262890683122, 1.000000000000000000, 0.9659258262890683122, 1.000000000000000000, 0.9659258262890683122, 1.000000000000000000, 0.9659258262890683122, 1.000000000000000000, 0.9659258262890683122, 1.000000000000000000, 0.9659258262890683122, 1.000000000000000000, 0.9659258262890683122, 1.000000000000000000, 0.9659258262890683122, 1.000000000000000000, 0.9659258262890683122, 1.000000000000000000, 0.9659258262890683122, 1.000000000000000000, 0.9659258262890683122, 1.000000000000000000, 0.9659258262890683122, 1.000000000000000000, 0.9659258262890683122, 1.000000000000000000, 0.9659258262890683122, 1.000000000000000000, 0.9659258262890683122, 1.000000000000000000, 0.9659258262890683122, 1.000000000000000000, 0.9659258262890683122, 1.000000000000000000, 0.9659258262890683122, 1.000000000000000000, 0.9659258262890683122, 1.000000000000000000, 0.9659258262890683122, 1.000000000000000000, 0.9659258262890683122, 1.000000000000000000, 0.9659258262890683122, 1.000000000000000000, 0.9659258262890683122, 1.000000000000000000, 0.9659258262890683122, 1.000000000000000000, 0.9659258262890683122, 1.000000000000000000, 0.9659258262890683122, 1.000000000000000000, 0.9659258262890683122, 1.000000000000000000, 0.9659258262890683122, 1.000000000000000000, 0.9659258262890683122, 1.000000000000000000, 0.9659258262890683122, 1.000000000000000000, 0.9659258262890683122, 1.000000000000000000, 0.9659258262890683122, 1.000000000000000000, 0.9659258262890683122, 1.000000000000000000, 0.9659258262890683122, 1.000000000000000000, 0.9659258262890683122, 1.000000000000000000, 0.9659258262890683122, 1.000000000000000000, 0.9659258262890683122, 1.000000000000000000, 0.9659258262890683122, 1.000000000000000000, 0.9659258262890683122, 1.000000000000000000, 0.9659258262890683122, 1.000000000000000000, 0.9659258262890683122, 1.000000000000000000, 0.9659258262890683122, 1.000000000000000000, 0.9659258262890683122, 1.000000000000000000, 0.9659258262890683122, 1.000000000000000000, 0.9659258262890683122, 1.000000000000000000, 0.9659258262890683122, 1.000000000000000000, 0.9659258262890683122, 1.000000000000000000, 0.9659258262890683122, 1.000000000000000000, 0.9659258262890683122, 1.000000000000000000, 0.9659258262890683122, 1.000000000000000000, 0.9659258262890683122, 1.000000000000000000, 0.9659258262890683122, 1.000000000000000000, 0.9659258262890683122, 1.000000000000000000, 0.9659258262890683122, 1.000000000000000000, 0.9659258262890683122, 1.000000000000000000, 0.9659258262890683122, 1.000000000000000000, 0.9659258262890683122, 1.000000000000000000, 0.9659258262890683122, 1.000000000000000000, 0.9659258262890683122, 1.000000000000000000, 0.9659258262890683122, 1.000000000000000000, 0.9659258262890683122, 1.000000000000000000, 0.9659258262890683122, 1.000000000000000000, 0.9659258262890683122, 1.000000000000000000, 0.9659258262890683122, 1.000000000000000000, 0.9659258262890683122, 1.000000000000000000, 0.9659258262890683122, 1.000000000000000000, 0.9659258262890683122, 1.000000000000000000, 0.9659258262890683122, 1.000000000000000000, 0.9659258262890683122, 1.000000000000000000, 0.9659258262890683122, 1.000000000000000000, 0.9659258262890683122, 1.000000000000000000, 0.9659258262890683122, 1.000000000000000000, 0.9659258262890683122, 1.000000000000000000, 0.9659258262890683122, 1.000000000000000000, 0.9659258262890683122, 1.000000000000000000, 0.9659258262890683122, 1.000000000000000000, 0.9659258262890683122, 1.000000000000000000, 0.9659258262890683122, 1.000000000000000000, 0.9659258262890683122, 1.000000000000000000, 0.9659258262890683122, 1.000000000000000000, 0.9659258262890683122, 1.000000000000000000, 0.9659258262890683122, 1.000000000000000000, 0.9659258262890683122, 1.000000000000000000, 0.9659258262890683122, 1.000000000000000000, 0.9659258262890683122, 1.000000000000000000, 0.9659258262890683122, 1.000000000000000000, 0.9659258262890683122, 1.000000000000000000, 0.9659258262890683122, 1.000000000000000000, 0.9659258262890683122, 1.000000000000000000, 0.9659258262890683122, 1.000000000000000000, 0.9659258262890683122, 1.000000000000000000, 0.9659258262890683122, 1.000000000000000000, 0.9659258262890683122, 1.000000000000000000, 0.9659258262890683122, 1.000000000000000000, 0.9659258262890683122, 1.000000000000000000, 0.9659258262890683122, 1.000000000000000000, 0.9659258262890683122, 1.000000000000000000, 0.9659258262890683122, 1.000000000000000000, 0.9659258262890683122, 1.000000000000000000, 0.9659258262890683122, 1.000000000000000000, 0.9659258262890683122, 1.000000000000000000) ) ) 
 REPRESENTATION_ITEM ( '' )  SURFACE ( )  );
#26164 = CARTESIAN_POINT ( 'NONE',  ( 0.05249343832021075018, 0.2306618581243847221, -0.2411417322834647770 ) ) ;
#26165 = CARTESIAN_POINT ( 'NONE',  ( 0.04593175853018440641, -0.6692913385826771977, 0.1292274648535927661 ) ) ;
#26166 = CARTESIAN_POINT ( 'NONE',  ( 0.3392501089628018884, -0.1958661417322834220, -1.606955380577427928 ) ) ;
#26167 = CARTESIAN_POINT ( 'NONE',  ( -1.076115485564303809, 0.2306618581243848609, 0.2411417322834645549 ) ) ;
#26168 = CARTESIAN_POINT ( 'NONE',  ( -0.3674540682414689785, 0.2306618581243848609, 0.2411417322834645549 ) ) ;
#26169 = CARTESIAN_POINT ( 'NONE',  ( 0.02624671916010564918, -0.5023911411419708095, -0.1820866141732282451 ) ) ;
#26170 = CARTESIAN_POINT ( 'NONE',  ( 1.587926509186352586, -0.4281496062992127816, -0.4176697321401328100 ) ) ;
#26171 = CARTESIAN_POINT ( 'NONE',  ( 1.437007874015748810, -0.5400638737290845981, -0.3530559997133363437 ) ) ;
#26172 = CARTESIAN_POINT ( 'NONE',  ( -0.6430446194225716283, -0.4281496062992124485, 0.4176697321401328655 ) ) ;
#26173 = DIRECTION ( 'NONE',  ( 1.000000000000000000, 0.000000000000000000, 0.000000000000000000 ) ) ;
#26174 = CARTESIAN_POINT ( 'NONE',  ( 1.246719160104987623, -0.4281496062992124485, 0.4176697321401328655 ) ) ;
#26175 = CARTESIAN_POINT ( 'NONE',  ( 0.5249343832021003964, 0.1539470093639521697, -0.1968503937007875793 ) ) ;
#26176 = VERTEX_POINT ( 'NONE', #77656 ) ;
#26177 = ORIENTED_EDGE ( 'NONE', *, *, #46912, .T. ) ;
#26178 = CARTESIAN_POINT ( 'NONE',  ( 0.3280839895013130669, -0.4281496062992127816, -0.4176697321401328100 ) ) ;
#26179 = CARTESIAN_POINT ( 'NONE',  ( -0.4790026246719154557, -0.2845877964562159024, 0.3641732283464567677 ) ) ;
#26181 = DIRECTION ( 'NONE',  ( 1.000000000000000000, 8.881784197001252323E-16, 0.000000000000000000 ) ) ;
#26180 = CARTESIAN_POINT ( 'NONE',  ( 1.528871391076116026, 0.1771653543307087630, 0.09757992244046791164 ) ) ;
#26182 = CARTESIAN_POINT ( 'NONE',  ( -0.2362204724409447953, -0.4091458600556404646, -0.2998687664041995160 ) ) ;
#26183 = DIRECTION ( 'NONE',  ( 0.000000000000000000, 0.000000000000000000, 1.000000000000000000 ) ) ;
#26184 = CARTESIAN_POINT ( 'NONE',  ( 1.509186351706037543, -0.4281496062992127816, -0.4176697321401328100 ) ) ;
#26185 = CIRCLE ( 'NONE', #663, 0.1181102362204723977 ) ;
#26186 = CARTESIAN_POINT ( 'NONE',  ( 0.1058382717557500852, -0.3949938075777408852, -0.3195538057742782212 ) ) ;
#26187 = CARTESIAN_POINT ( 'NONE',  ( -0.1640419947506555343, -0.3162353388693405765, 0.4822834645669290543 ) ) ;
#26188 = LINE ( 'NONE', #45537, #9591 ) ;
#26189 = CARTESIAN_POINT ( 'NONE',  ( -1.555118110236219930, 0.1660481256975885056, 0.3530559997133364547 ) ) ;
#26190 = CARTESIAN_POINT ( 'NONE',  ( 0.1246719160104994284, -0.6692913385826771977, 0.1292274648535927661 ) ) ;
#26191 = CARTESIAN_POINT ( 'NONE',  ( 0.3949938075777409963, 2.418639510665530743E-17, -0.03740157480314962313 ) ) ;
#26192 = CARTESIAN_POINT ( 'NONE',  ( 1.614173228346457378, -0.6692913385826771977, 8.415575281601705876E-17 ) ) ;
#26193 = CARTESIAN_POINT ( 'NONE',  ( 0.4790026246719167324, -0.05778040916215522460, 0.4822834645669289988 ) ) ;
#26194 = CARTESIAN_POINT ( 'NONE',  ( 1.089238845144357759, -0.004921259842519870586, -0.3153832671262229437 ) ) ;
#26195 = LINE ( 'NONE', #53110, #80207 ) ;
#26196 = CARTESIAN_POINT ( 'NONE',  ( 0.6692913385826778638, -0.5511811023622047445, 6.969142054262312111E-17 ) ) ;
#26197 = CARTESIAN_POINT ( 'NONE',  ( -1.108923884514435132, -0.05778040916215560624, -0.4822834645669293319 ) ) ;
#26198 = CARTESIAN_POINT ( 'NONE',  ( 0.3460692066303958092, 0.1998031496062993018, -0.8379265091863516979 ) ) ;
#26199 = CARTESIAN_POINT ( 'NONE',  ( 1.128608923884515169, -0.6046776061558809534, -0.2411417322834644161 ) ) ;
#26200 = CARTESIAN_POINT ( 'NONE',  ( 0.3917322834645670104, -0.1049643490035303411, -0.5761154855643042527 ) ) ;
#26202 = CARTESIAN_POINT ( 'NONE',  ( -0.1345703391920888281, 1.081211091791626222, 1.867241868865190391 ) ) ;
#26201 = CARTESIAN_POINT ( 'NONE',  ( 0.7086614173228353852, -0.1870078740157479769, 0.4822834645669291653 ) ) ;
#26203 = DIRECTION ( 'NONE',  ( -0.7071067811865472397, 0.000000000000000000, -0.7071067811865476838 ) ) ;
#26204 = CARTESIAN_POINT ( 'NONE',  ( 0.3477690288713918276, 0.1771653543307087630, 0.09757992244046791164 ) ) ;
#26205 = B_SPLINE_CURVE_WITH_KNOTS ( 'NONE', 3,
 ( #82811, #74867, #69362, #62213, #75685, #56306, #69772 ),
 .UNSPECIFIED., .F., .F.,
 ( 4, 3, 4 ),
 ( 3.643951726750583631E-17, 0.001246232571205249445, 0.002492492258783241162 ),
 .UNSPECIFIED. ) ;
#26206 = CARTESIAN_POINT ( 'NONE',  ( 0.4855643044619430415, -0.4281496062992127816, -0.4176697321401328100 ) ) ;
#26207 = CARTESIAN_POINT ( 'NONE',  ( 1.673228346456693494, 0.07958543189024085140, 0.2665933059059887866 ) ) ;
#26208 = CARTESIAN_POINT ( 'NONE',  ( -1.076115485564303809, 0.1283753931104748280, 0.1820866141732283561 ) ) ;
#26209 = CARTESIAN_POINT ( 'NONE',  ( -1.076115485564303809, 0.2306618581243848609, 0.2411417322834645549 ) ) ;
#26210 = CARTESIAN_POINT ( 'NONE',  ( 1.076115485564305141, 0.2306618581243847221, -0.2411417322834647770 ) ) ;
#26211 = CARTESIAN_POINT ( 'NONE',  ( -1.095800524934382292, -0.05778040916215522460, 0.4822834645669289988 ) ) ;
#26212 = CARTESIAN_POINT ( 'NONE',  ( 1.095800524934383846, -0.05778040916215560624, -0.4822834645669293319 ) ) ;
#26213 = CARTESIAN_POINT ( 'NONE',  ( -1.463254593175852492, 0.1771653543307087630, 0.09757992244046791164 ) ) ;
#26214 = PLANE ( 'NONE',  #10166 ) ;
#26215 = CARTESIAN_POINT ( 'NONE',  ( 0.9055118110236227702, -0.6692913385826771977, 8.415575281601705876E-17 ) ) ;
#26216 = CARTESIAN_POINT ( 'NONE',  ( 0.1265901696524989462, 0.4724409448818897572, -2.589895013123359568 ) ) ;
#26217 = CARTESIAN_POINT ( 'NONE',  ( -0.08943933388982759636, 1.809133623825372073E-16, -0.4118484887281974038 ) ) ;
#26218 = CARTESIAN_POINT ( 'NONE',  ( 1.482939632545932307, -0.4281496062992124485, 0.4176697321401328655 ) ) ;
#26219 = CARTESIAN_POINT ( 'NONE',  ( -1.095800524934382292, -0.08942795157527998196, 0.3641732283464567121 ) ) ;
#26220 = DIRECTION ( 'NONE',  ( 0.000000000000000000, 0.000000000000000000, -1.000000000000000000 ) ) ;
#26221 = CARTESIAN_POINT ( 'NONE',  ( -1.397637795275589623, -0.4536011799217368745, -0.2665933059059886201 ) ) ;
#26222 = CARTESIAN_POINT ( 'NONE',  ( -0.5183727034120726440, 0.1771653543307087630, 0.09757992244046791164 ) ) ;
#26223 = CARTESIAN_POINT ( 'NONE',  ( -1.568241469816272105, -0.08942795157527998196, 0.3641732283464567121 ) ) ;
#26224 = CARTESIAN_POINT ( 'NONE',  ( 0.9317585301837276734, -0.3690944881889763329, 0.3153832671262228327 ) ) ;
#26225 = CARTESIAN_POINT ( 'NONE',  ( 0.6758530183727039509, -0.6692913385826771977, 0.1292274648535927661 ) ) ;
#26226 = CARTESIAN_POINT ( 'NONE',  ( 1.266404199475066328, -0.05778040916215522460, 0.4822834645669289988 ) ) ;
#26227 = CARTESIAN_POINT ( 'NONE',  ( 0.02624671916010564918, -0.6046776061558809534, -0.2411417322834644161 ) ) ;
#26228 = CARTESIAN_POINT ( 'NONE',  ( 0.7414698162729663755, -0.5511811023622048555, -0.09757992244046775898 ) ) ;
#26229 = CARTESIAN_POINT ( 'NONE',  ( 1.581364829396326277, -0.05778040916215522460, 0.4822834645669289988 ) ) ;
#26230 = EDGE_CURVE ( 'NONE', #56386, #17817, #51951, .T. ) ;
#26231 = CARTESIAN_POINT ( 'NONE',  ( -1.476377952755905110, 0.1660481256975885056, 0.3530559997133364547 ) ) ;
#26232 = CARTESIAN_POINT ( 'NONE',  ( -0.7086614173228339419, -0.1870078740157480879, -0.4822834645669291653 ) ) ;
#26233 = CARTESIAN_POINT ( 'NONE',  ( -0.1998031496062991907, -0.3460692066303959757, -0.3805774278215223183 ) ) ;
#26234 = FACE_OUTER_BOUND ( 'NONE', #73824, .T. ) ;
#26235 = CARTESIAN_POINT ( 'NONE',  ( -0.09186351706036689768, 0.05413385826771626580, -0.4176697321401330321 ) ) ;
#26237 = CIRCLE ( 'NONE', #30324, 0.3051181102362204856 ) ;
#26236 = CARTESIAN_POINT ( 'NONE',  ( -0.4265091863517051496, -0.6692913385826771977, 0.1292274648535927661 ) ) ;
#26238 = CARTESIAN_POINT ( 'NONE',  ( 0.5314960629921264834, 0.1660481256975883668, -0.3530559997133364547 ) ) ;
#26239 = CARTESIAN_POINT ( 'NONE',  ( 0.3996062992125986035, 2.446882876249141962E-17, -2.795275590551181022 ) ) ;
#26240 = AXIS2_PLACEMENT_3D ( 'NONE', #7854, #46132, #71826 ) ;
#26241 = CARTESIAN_POINT ( 'NONE',  ( -0.1058382717557497937, -0.3949938075777411628, -1.804461942257217899 ) ) ;
#26242 = CARTESIAN_POINT ( 'NONE',  ( -0.1049643490035302024, -0.3917322834645671215, -0.3792650918635169233 ) ) ;
#26244 = EDGE_CURVE ( 'NONE', #53395, #80562, #71751, .T. ) ;
#26243 = CARTESIAN_POINT ( 'NONE',  ( 0.2746814661183891726, -0.1088119808354341550, 5.842252906343563090 ) ) ;
#26245 = CARTESIAN_POINT ( 'NONE',  ( -0.1049643490035301885, -0.3917322834645671215, -1.166666666666666519 ) ) ;
#26246 = CARTESIAN_POINT ( 'NONE',  ( -0.9383202099737524282, -0.08942795157527998196, 0.3641732283464567121 ) ) ;
#26247 = CARTESIAN_POINT ( 'NONE',  ( 0.1958661417322834775, 0.3392501089628018884, -0.9238845144356954142 ) ) ;
#26248 = CARTESIAN_POINT ( 'NONE',  ( -1.325459317585300889, -0.4281496062992127816, -0.4176697321401328100 ) ) ;
#26249 = CARTESIAN_POINT ( 'NONE',  ( -0.3420746716998660508, -0.1974969037888706924, -2.806430446194226214 ) ) ;
#26250 = CARTESIAN_POINT ( 'NONE',  ( 0.4265091863517067594, 0.2952755905511811885, 0.1292274648535926551 ) ) ;
#26251 = CARTESIAN_POINT ( 'NONE',  ( 5.463695987328526437E-16, -0.1870078740157479769, 0.3641732283464567677 ) ) ;
#26252 = CARTESIAN_POINT ( 'NONE',  ( 1.115485564304462551, 0.05413385826771666132, 0.4176697321401328100 ) ) ;
#26253 = CARTESIAN_POINT ( 'NONE',  ( 0.5118110236220478892, 0.2952755905511811885, 0.000000000000000000 ) ) ;
#26254 = CARTESIAN_POINT ( 'NONE',  ( -0.4724409448818899238, 0.1265901696524986686, -2.867454068241469756 ) ) ;
#26255 = CARTESIAN_POINT ( 'NONE',  ( 0.3460692066303959202, 0.1998031496062993295, -2.650918635170603554 ) ) ;
#26256 = CARTESIAN_POINT ( 'NONE',  ( -0.3917322834645670104, -0.1049643490035307020, -1.145032439141419500 ) ) ;
#26257 = CARTESIAN_POINT ( 'NONE',  ( 1.272965879265092637, -0.4281496062992127816, -0.4176697321401328100 ) ) ;
#26258 = CARTESIAN_POINT ( 'NONE',  ( 0.6036745406824153282, -0.6046776061558807314, 0.2411417322834647770 ) ) ;
#26259 = CARTESIAN_POINT ( 'NONE',  ( 0.2821522309711292364, -0.6692913385826771977, 0.1292274648535927661 ) ) ;
#26260 = CARTESIAN_POINT ( 'NONE',  ( 0.8989501312335963501, -0.5511811023622048555, -0.09757992244046775898 ) ) ;
#26261 = CARTESIAN_POINT ( 'NONE',  ( 1.272965879265092637, -0.4281496062992127816, -0.4176697321401328100 ) ) ;
#26262 = CARTESIAN_POINT ( 'NONE',  ( -0.3917322834645671215, 0.1049643490035301469, -0.5898950131233595684 ) ) ;
#26263 = CARTESIAN_POINT ( 'NONE',  ( 0.1640419947506569498, -0.05778040916215522460, 0.4822834645669289988 ) ) ;
#26264 = CARTESIAN_POINT ( 'NONE',  ( 1.010498687664042716, -0.4281496062992124485, 0.4176697321401328655 ) ) ;
#26265 = CARTESIAN_POINT ( 'NONE',  ( 0.5511811023622055217, -0.1870078740157479769, 0.4822834645669291653 ) ) ;
#26266 = CARTESIAN_POINT ( 'NONE',  ( 1.286089238845145033, -0.5023911411419708095, -0.1820866141732282451 ) ) ;
#26267 = CARTESIAN_POINT ( 'NONE',  ( -1.062992125984250968, 0.2952755905511811885, 0.000000000000000000 ) ) ;
#26268 = CARTESIAN_POINT ( 'NONE',  ( -1.509186351706035767, 0.05413385826771626580, -0.4176697321401330321 ) ) ;
#26269 = CARTESIAN_POINT ( 'NONE',  ( 1.062992125984252745, -0.6692913385826771977, 8.415575281601705876E-17 ) ) ;
#26270 = CARTESIAN_POINT ( 'NONE',  ( 0.05722014594059725984, -0.3876764156947919981, -1.929133858267717549 ) ) ;
#26271 = CARTESIAN_POINT ( 'NONE',  ( 0.1049643490035303689, 0.3917322834645670104, -1.875328083989501460 ) ) ;
#26272 = CARTESIAN_POINT ( 'NONE',  ( 4.797336870675656522E-17, -0.3917322834645670104, -2.748031496062991685 ) ) ;
#26273 = VERTEX_POINT ( 'NONE', #19988 ) ;
#26274 = CARTESIAN_POINT ( 'NONE',  ( -9.787531504996567848E-17, 0.3996062992125986035, 0.1574803149606298913 ) ) ;
#26275 = ORIENTED_EDGE ( 'NONE', *, *, #63069, .T. ) ;
#26276 = CARTESIAN_POINT ( 'NONE',  ( 1.496062992125985147, -0.1870078740157479769, 0.4822834645669291653 ) ) ;
#26277 = CARTESIAN_POINT ( 'NONE',  ( 0.8202099737532813073, 0.1771653543307087630, 0.09757992244046791164 ) ) ;
#26278 = CARTESIAN_POINT ( 'NONE',  ( 1.076935383196057749, 2.559055118110236560, -0.3149606299212596716 ) ) ;
#26279 = CARTESIAN_POINT ( 'NONE',  ( -0.04294987210466714306, 1.064862614867412516, 2.872282311130982979 ) ) ;
#26280 = CARTESIAN_POINT ( 'NONE',  ( 0.4177787735907000366, 0.2755905511811023723, -1.559171609364239375 ) ) ;
#26281 = CARTESIAN_POINT ( 'NONE',  ( 0.1958661417322836440, -0.3392501089628017219, -0.8064304461942258806 ) ) ;
#26282 = CARTESIAN_POINT ( 'NONE',  ( -1.259842519685038686, -0.1870078740157480601, -0.3641732283464567677 ) ) ;
#26283 = CARTESIAN_POINT ( 'NONE',  ( -1.633858267716534529, -0.4536011799217368745, -0.2665933059059886201 ) ) ;
#26284 = CARTESIAN_POINT ( 'NONE',  ( -0.3960428127060340864, -0.01218835185216879564, -1.929133858267718660 ) ) ;
#26285 = CARTESIAN_POINT ( 'NONE',  ( -0.1706036745406816491, -0.4281496062992124485, 0.4176697321401328655 ) ) ;
#26286 = CARTESIAN_POINT ( 'NONE',  ( 1.522309711286089939, -0.6046776061558809534, -0.2411417322834644161 ) ) ;
#26287 = ORIENTED_EDGE ( 'NONE', *, *, #61531, .F. ) ;
#26288 = LINE ( 'NONE', #65019, #29917 ) ;
#26289 = DIRECTION ( 'NONE',  ( -6.123233995736774664E-17, 1.000000000000000000, 9.948661822760610116E-18 ) ) ;
#26290 = CARTESIAN_POINT ( 'NONE',  ( 0.5314960629921396951, 2.755905511811024056, -3.937007874015760578 ) ) ;
#26291 = CARTESIAN_POINT ( 'NONE',  ( -0.5314960629921193780, 2.755905511811024056, -1.895394334970793793 ) ) ;
#26292 = CARTESIAN_POINT ( 'NONE',  ( -1.102362204724408601, -0.1870078740157480601, -0.3641732283464567677 ) ) ;
#26293 =( BOUNDED_CURVE ( )  B_SPLINE_CURVE ( 1, ( #53936, #80884 ),
 .UNSPECIFIED., .F., .F. ) 
 B_SPLINE_CURVE_WITH_KNOTS ( ( 2, 2 ),
 ( 5.421010862427522170E-20, 0.002000000000000006113 ),
 .UNSPECIFIED. ) 
 CURVE ( )  GEOMETRIC_REPRESENTATION_ITEM ( )  RATIONAL_B_SPLINE_CURVE ( ( 0.9875488213027530104, 0.9875488213027530104 ) ) 
 REPRESENTATION_ITEM ( '' )  );
#26294 = CARTESIAN_POINT ( 'NONE',  ( -1.633858267716534529, 0.1660481256975885056, 0.3530559997133364547 ) ) ;
#26295 = CARTESIAN_POINT ( 'NONE',  ( 0.4593175853018380828, 0.05413385826771626580, -0.4176697321401330321 ) ) ;
#26296 = AXIS2_PLACEMENT_3D ( 'NONE', #18633, #82610, #71229 ) ;
#26297 = ORIENTED_EDGE ( 'NONE', *, *, #27035, .F. ) ;
#26299 = CARTESIAN_POINT ( 'NONE',  ( 2.583694225513480713, 2.755905511811024056, -0.5314960629921260393 ) ) ;
#26298 = CARTESIAN_POINT ( 'NONE',  ( -1.895394334970792016, 2.755905511811024056, -0.5314960629921260393 ) ) ;
#26300 = CARTESIAN_POINT ( 'NONE',  ( 1.227034120734908917, 0.2952755905511810774, -0.1292274648535930714 ) ) ;
#26301 = CARTESIAN_POINT ( 'NONE',  ( 1.601049868766404982, 0.1283753931104748280, 0.1820866141732283561 ) ) ;
#26302 = CARTESIAN_POINT ( 'NONE',  ( 0.1958661417322836162, -0.3392501089628018329, -0.6443376395987383543 ) ) ;
#26303 = CARTESIAN_POINT ( 'NONE',  ( -0.5643044619422565855, -0.004921259842519870586, -0.3153832671262229437 ) ) ;
#26304 = EDGE_CURVE ( 'NONE', #52886, #49832, #37600, .T. ) ;
#26305 = CARTESIAN_POINT ( 'NONE',  ( -1.371391076115484609, -0.5511811023622046335, 0.09757992244046803654 ) ) ;
#26306 = DIRECTION ( 'NONE',  ( 1.000000000000000000, -0.000000000000000000, -0.000000000000000000 ) ) ;
#26307 = CARTESIAN_POINT ( 'NONE',  ( -0.4133858267716528645, -0.4536011799217367080, 0.2665933059059888421 ) ) ;
#26308 = CARTESIAN_POINT ( 'NONE',  ( 0.09842519685039434474, -0.4536011799217368745, -0.2665933059059886201 ) ) ;
#26309 = CARTESIAN_POINT ( 'NONE',  ( -0.06561679790026180015, -0.4281496062992127816, -0.4176697321401328100 ) ) ;
#26310 = CARTESIAN_POINT ( 'NONE',  ( -1.227034120734907141, -0.5511811023622048555, -0.09757992244046775898 ) ) ;
#26311 = CARTESIAN_POINT ( 'NONE',  ( 0.3392501089628018884, -0.1958661417322833942, -0.1017253525272460019 ) ) ;
#26312 = CARTESIAN_POINT ( 'NONE',  ( 0.9383202099737536495, -0.3162353388693405765, 0.4822834645669290543 ) ) ;
#26313 = CARTESIAN_POINT ( 'NONE',  ( -1.371391076115484609, -0.6692913385826771977, 0.1292274648535927661 ) ) ;
#26314 = CARTESIAN_POINT ( 'NONE',  ( -0.4724409448818899238, 0.1265901696524986686, -1.054461942257217899 ) ) ;
#26315 = CARTESIAN_POINT ( 'NONE',  ( -0.4199475065616791736, 0.2306618581243847221, -0.2411417322834647770 ) ) ;
#26316 = CARTESIAN_POINT ( 'NONE',  ( 0.09186351706036799403, -0.3690944881889765550, -0.3153832671262227771 ) ) ;
#26317 = CARTESIAN_POINT ( 'NONE',  ( -1.010498687664041384, 0.05413385826771666132, 0.4176697321401328100 ) ) ;
#26318 = CARTESIAN_POINT ( 'NONE',  ( 0.7939632545931766261, -0.2845877964562161244, -0.3641732283464567121 ) ) ;
#26319 = CARTESIAN_POINT ( 'NONE',  ( -0.2034120734908131112, -0.5511811023622048555, -0.09757992244046775898 ) ) ;
#26320 = CARTESIAN_POINT ( 'NONE',  ( -0.4461942257217840213, 0.2306618581243848609, 0.2411417322834645549 ) ) ;
#26321 = FACE_OUTER_BOUND ( 'NONE', #34770, .T. ) ;
#26322 = DIRECTION ( 'NONE',  ( 0.000000000000000000, 1.000000000000000000, 0.000000000000000000 ) ) ;
#26323 = CARTESIAN_POINT ( 'NONE',  ( 1.496062992125985147, -0.1870078740157479769, 0.3641732283464567677 ) ) ;
#26324 = CARTESIAN_POINT ( 'NONE',  ( -1.397637795275589623, -0.5400638737290845981, -0.3530559997133363437 ) ) ;
#26325 = CARTESIAN_POINT ( 'NONE',  ( -1.443569553805773564, -0.6046776061558807314, 0.2411417322834647770 ) ) ;
#26326 = ORIENTED_EDGE ( 'NONE', *, *, #21327, .T. ) ;
#26327 = CARTESIAN_POINT ( 'NONE',  ( 0.1998031496062992463, 0.3460692066303959202, -2.425853018372703396 ) ) ;
#26328 = CARTESIAN_POINT ( 'NONE',  ( -1.023622047244093558, -0.1870078740157479769, 0.3641732283464567677 ) ) ;
#26329 = CARTESIAN_POINT ( 'NONE',  ( 0.8070866141732288002, 0.1660481256975885056, 0.3530559997133364547 ) ) ;
#26330 = CARTESIAN_POINT ( 'NONE',  ( -1.128608923884513837, -0.5023911411419708095, 0.1820866141732285504 ) ) ;
#26331 = CARTESIAN_POINT ( 'NONE',  ( -0.3996062992125984925, -0.1070741851644056858, -1.854986876640420057 ) ) ;
#26332 = CARTESIAN_POINT ( 'NONE',  ( -1.181102362204723644, -0.1870078740157480879, -0.4822834645669291653 ) ) ;
#26333 = VECTOR ( 'NONE', #35612, 39.37007874015748143 ) ;
#26334 = CARTESIAN_POINT ( 'NONE',  ( 0.8398950131233602345, -0.6046776061558807314, 0.2411417322834647770 ) ) ;
#26335 = CARTESIAN_POINT ( 'NONE',  ( 0.3674540682414705883, -0.6046776061558807314, 0.2411417322834647770 ) ) ;
#26336 = CARTESIAN_POINT ( 'NONE',  ( 1.561679790026247350, -0.4281496062992124485, 0.4176697321401328655 ) ) ;
#26337 = CARTESIAN_POINT ( 'NONE',  ( -1.627296587926508442, -0.5023911411419708095, -0.1820866141732282451 ) ) ;
#26338 = CARTESIAN_POINT ( 'NONE',  ( -0.3996062992125986035, 0.1070741851644051584, -0.8969816272965878134 ) ) ;
#26339 = CARTESIAN_POINT ( 'NONE',  ( 0.3996062992125986035, 2.446882876249141962E-17, -1.377952755905511806 ) ) ;
#26340 = CARTESIAN_POINT ( 'NONE',  ( 0.3949938075777411073, -0.1058382717557499464, -0.5839895013123359568 ) ) ;
#26341 = CARTESIAN_POINT ( 'NONE',  ( 1.019880138406203063, 1.617842475621884768, 0.4678109194727893549 ) ) ;
#26342 = CARTESIAN_POINT ( 'NONE',  ( 0.8267716535433078384, -0.5511811023622047445, 6.969142054262312111E-17 ) ) ;
#26343 = CARTESIAN_POINT ( 'NONE',  ( 0.2559055118110243332, -0.4536011799217368745, -0.2665933059059886201 ) ) ;
#26344 = CARTESIAN_POINT ( 'NONE',  ( -0.05905511811023545637, -0.5400638737290845981, -0.3530559997133363437 ) ) ;
#26345 = CARTESIAN_POINT ( 'NONE',  ( 1.364829396325459854, -0.6046776061558809534, -0.2411417322834644161 ) ) ;
#26346 = CARTESIAN_POINT ( 'NONE',  ( 0.3420746716998660508, -0.1974969037888704149, -1.914041994750656395 ) ) ;
#26347 = CARTESIAN_POINT ( 'NONE',  ( 0.5577427821522316087, -0.08942795157527998196, 0.3641732283464567121 ) ) ;
#26348 = CARTESIAN_POINT ( 'NONE',  ( -0.8989501312335946848, -0.6692913385826771977, 0.1292274648535927661 ) ) ;
#26349 = CARTESIAN_POINT ( 'NONE',  ( -1.141732283464566011, 0.2952755905511811885, 0.000000000000000000 ) ) ;
#26350 = CARTESIAN_POINT ( 'NONE',  ( 0.6692913385826778638, -0.6692913385826771977, 8.415575281601705876E-17 ) ) ;
#26351 = CARTESIAN_POINT ( 'NONE',  ( 0.4724409448818896462, 0.1265901696524990294, -1.699475065616798064 ) ) ;
#26352 = CARTESIAN_POINT ( 'NONE',  ( 0.000000000000000000, 1.724409448818897905, 0.000000000000000000 ) ) ;
#26353 = CIRCLE ( 'NONE', #35814, 1.244489337948954555 ) ;
#26354 = ORIENTED_EDGE ( 'NONE', *, *, #63984, .F. ) ;
#26355 = ORIENTED_EDGE ( 'NONE', *, *, #23260, .F. ) ;
#26356 = CARTESIAN_POINT ( 'NONE',  ( -1.377952755905511140, 0.2952755905511811885, 0.000000000000000000 ) ) ;
#26357 = CARTESIAN_POINT ( 'NONE',  ( -0.5249343832020990641, 0.2306618581243848609, 0.2411417322834645549 ) ) ;
#26359 = CARTESIAN_POINT ( 'NONE',  ( -0.6955380577427815458, 0.05413385826771666132, 0.4176697321401328100 ) ) ;
#26358 = CARTESIAN_POINT ( 'NONE',  ( -0.9383202099737524282, -0.2845877964562161244, -0.3641732283464567121 ) ) ;
#26360 = CARTESIAN_POINT ( 'NONE',  ( 0.3917322834645668994, -0.1049643490035303134, -1.923865198653856634 ) ) ;
#26361 = LINE ( 'NONE', #39410, #78666 ) ;
#26362 = CARTESIAN_POINT ( 'NONE',  ( 1.646981627296588035, -0.3162353388693405765, 0.4822834645669290543 ) ) ;
#26363 = CARTESIAN_POINT ( 'NONE',  ( -1.253280839895012377, -0.05778040916215522460, 0.4822834645669289988 ) ) ;
#26364 = CARTESIAN_POINT ( 'NONE',  ( 0.1640419947506569498, -0.05778040916215522460, 0.4822834645669289988 ) ) ;
#26365 = EDGE_CURVE ( 'NONE', #10035, #36478, #14105, .T. ) ;
#26366 = CARTESIAN_POINT ( 'NONE',  ( -0.8267716535433065062, 0.2952755905511811885, 0.000000000000000000 ) ) ;
#26367 = EDGE_CURVE ( 'NONE', #55060, #80751, #6026, .T. ) ;
#26368 = CARTESIAN_POINT ( 'NONE',  ( 0.7283464566929140904, -0.5400638737290845981, -0.3530559997133363437 ) ) ;
#26369 = CARTESIAN_POINT ( 'NONE',  ( -0.3392501089628019995, 0.1958661417322832277, -1.278215223097112885 ) ) ;
#26370 = CARTESIAN_POINT ( 'NONE',  ( -0.7808398950131222316, -0.2845877964562161244, -0.3641732283464567121 ) ) ;
#26371 = ORIENTED_EDGE ( 'NONE', *, *, #23961, .F. ) ;
#26372 = CARTESIAN_POINT ( 'NONE',  ( -0.3949938075777411628, 0.1058382717557497937, -1.765091863517060267 ) ) ;
#26373 = ORIENTED_EDGE ( 'NONE', *, *, #34764, .F. ) ;
#26374 = CARTESIAN_POINT ( 'NONE',  ( -1.627296587926508442, -0.5023911411419708095, -0.1820866141732282451 ) ) ;
#26375 = CARTESIAN_POINT ( 'NONE',  ( -1.213910761154854745, 0.2952755905511810774, -0.1292274648535930714 ) ) ;
#26376 = CARTESIAN_POINT ( 'NONE',  ( -1.181102362204723644, -0.1870078740157479769, 0.4822834645669291653 ) ) ;
#26377 = CARTESIAN_POINT ( 'NONE',  ( -0.3460692066303958092, -0.1998031496062994683, -0.3674540682414698112 ) ) ;
#26378 = CARTESIAN_POINT ( 'NONE',  ( -0.9448818897637790704, -0.1870078740157479769, 0.4822834645669291653 ) ) ;
#26379 = CARTESIAN_POINT ( 'NONE',  ( -1.312335958005248715, -0.6046776061558809534, -0.2411417322834644161 ) ) ;
#26380 = CARTESIAN_POINT ( 'NONE',  ( -1.601049868766403650, 0.2306618581243847221, -0.2411417322834647770 ) ) ;
#26382 = LENGTH_MEASURE_WITH_UNIT ( LENGTH_MEASURE( 0.02539999999999999897 ), #32277 );
#26381 = B_SPLINE_CURVE_WITH_KNOTS ( 'NONE', 3,
 ( #68716, #43429, #69126, #82583, #11476, #18609, #37132, #30814, #56479, #82182, #44252, #24499, #50165, #75861, #18203, #6800, #7223, #21107, #13135, #32471, #58133, #32056, #502, #70784, #51393, #66144, #64463, #8072, #45080, #77521 ),
 .UNSPECIFIED., .F., .F.,
 ( 4, 2, 2, 2, 2, 2, 2, 2, 2, 2, 2, 2, 2, 2, 4 ),
 ( 0.02630788966047508878, 0.02761938857346193238, 0.02893088748644877597, 0.03024238639943561957, 0.03155388531242245970, 0.03417688313839615383, 0.03548838205138300089, 0.03679988096436985490, 0.03942287879034354903, 0.04073437770333040303, 0.04204587661631725704, 0.04335737552930411798, 0.04466887444229096504, 0.04598037335527782599, 0.04729187226826467999 ),
 .UNSPECIFIED. ) ;
#26383 = FACE_OUTER_BOUND ( 'NONE', #33205, .T. ) ;
#26384 = CARTESIAN_POINT ( 'NONE',  ( 0.2624671916010504757, 0.1283753931104748280, 0.1820866141732283561 ) ) ;
#26385 = CARTESIAN_POINT ( 'NONE',  ( 0.4695140184743307188, 1.605872332714558537, 2.158445410120229724 ) ) ;
#26386 = CARTESIAN_POINT ( 'NONE',  ( 0.3917322834645670104, 2.398668435337828261E-17, -0.5177165354330709457 ) ) ;
#26387 = CARTESIAN_POINT ( 'NONE',  ( -0.2427821522309703550, -0.08942795157528024563, -0.3641732283464568787 ) ) ;
#26388 = CARTESIAN_POINT ( 'NONE',  ( -0.9514435695538050464, -0.05778040916215560624, -0.4822834645669293319 ) ) ;
#26389 = CARTESIAN_POINT ( 'NONE',  ( 1.253280839895013710, -0.3162353388693405765, 0.4822834645669290543 ) ) ;
#26390 = CARTESIAN_POINT ( 'NONE',  ( -0.3280839895013117347, 0.05413385826771626580, -0.4176697321401330321 ) ) ;
#26391 = ORIENTED_EDGE ( 'NONE', *, *, #44509, .F. ) ;
#26392 = ORIENTED_EDGE ( 'NONE', *, *, #12851, .F. ) ;
#26393 = CARTESIAN_POINT ( 'NONE',  ( -0.1998031496062994405, 0.3460692066303957537, -1.979658792650918597 ) ) ;
#26394 = CARTESIAN_POINT ( 'NONE',  ( -0.9842519685039360366, 0.2952755905511811885, 0.000000000000000000 ) ) ;
#26395 = CARTESIAN_POINT ( 'NONE',  ( 1.286089238845145033, 0.2306618581243848609, 0.2411417322834645549 ) ) ;
#26396 = CARTESIAN_POINT ( 'NONE',  ( -1.502624671916009680, -0.08942795157528024563, -0.3641732283464568787 ) ) ;
#26397 = CARTESIAN_POINT ( 'NONE',  ( 0.4724409448818897572, -0.1265901696524988906, -0.7414698162729659314 ) ) ;
#26398 = DIRECTION ( 'NONE',  ( 0.000000000000000000, -1.000000000000000000, 0.000000000000000000 ) ) ;
#26399 = ADVANCED_FACE ( 'NONE', ( #12849 ), #46540, .F. ) ;
#26400 = CARTESIAN_POINT ( 'NONE',  ( -0.1049643490035307020, 0.3917322834645669549, -0.3136482939632545541 ) ) ;
#26401 = AXIS2_PLACEMENT_3D ( 'NONE', #40701, #8310, #15463 ) ;
#26402 = DIRECTION ( 'NONE',  ( 1.000000000000000000, 0.000000000000000000, 0.000000000000000000 ) ) ;
#26403 = CARTESIAN_POINT ( 'NONE',  ( -0.2165354330708654795, 0.1660481256975885056, 0.3530559997133364547 ) ) ;
#26404 = CARTESIAN_POINT ( 'NONE',  ( -1.410761154855641575, -0.2845877964562161244, -0.3641732283464567121 ) ) ;
#26405 = CONICAL_SURFACE ( 'NONE', #4897, 3.307086614173228689, 0.7853981633974500554 ) ;
#26406 = VECTOR ( 'NONE', #6937, 39.37007874015748143 ) ;
#26407 = CARTESIAN_POINT ( 'NONE',  ( -0.8989501312335946848, 0.2952755905511810774, -0.1292274648535930714 ) ) ;
#26408 = CARTESIAN_POINT ( 'NONE',  ( -0.2925321140481932369, 0.2925321140481931259, 0.2185039370078740162 ) ) ;
#26410 = LINE ( 'NONE', #50098, #79480 ) ;
#26409 = CARTESIAN_POINT ( 'NONE',  ( -1.338582677165353729, -0.1870078740157480879, -0.4822834645669291653 ) ) ;
#26411 = CARTESIAN_POINT ( 'NONE',  ( -1.062992125984250968, 0.2952755905511811885, 0.000000000000000000 ) ) ;
#26412 = CARTESIAN_POINT ( 'NONE',  ( -0.4790026246719154557, -0.3162353388693405765, 0.4822834645669290543 ) ) ;
#26413 = CARTESIAN_POINT ( 'NONE',  ( 0.3949938075777408852, 0.1058382717557500435, -2.563648293963254776 ) ) ;
#26414 = CARTESIAN_POINT ( 'NONE',  ( 0.8661417322834652488, -0.1870078740157480601, -0.3641732283464567677 ) ) ;
#26415 = CARTESIAN_POINT ( 'NONE',  ( 0.1958661417322836440, -0.3392501089628017219, -0.1765091863517061210 ) ) ;
#26416 = CARTESIAN_POINT ( 'NONE',  ( 0.5839895013123367340, 0.1771653543307087630, 0.09757992244046791164 ) ) ;
#26417 = CARTESIAN_POINT ( 'NONE',  ( 1.312335958005249825, 0.1283753931104746893, -0.1820866141732285504 ) ) ;
#26418 = CARTESIAN_POINT ( 'NONE',  ( 1.410761154855643795, -0.3162353388693405765, 0.4822834645669290543 ) ) ;
#26419 = CARTESIAN_POINT ( 'NONE',  ( 0.08530183727034192087, -0.08942795157527998196, 0.3641732283464567121 ) ) ;
#26420 = CARTESIAN_POINT ( 'NONE',  ( -0.3392501089628019995, 0.1958661417322832277, -1.593175853018372612 ) ) ;
#26421 = CARTESIAN_POINT ( 'NONE',  ( -0.9711286089238838626, 0.2306618581243847221, -0.2411417322834647770 ) ) ;
#26422 = CARTESIAN_POINT ( 'NONE',  ( 1.115485564304462551, 0.05413385826771666132, 0.4176697321401328100 ) ) ;
#26423 = VECTOR ( 'NONE', #76100, 39.37007874015748143 ) ;
#26424 = CARTESIAN_POINT ( 'NONE',  ( 0.4724409448818897572, -0.1265901696524988906, 0.1266404199475065218 ) ) ;
#26425 = CARTESIAN_POINT ( 'NONE',  ( -0.3149606299212590610, -0.1870078740157480601, -0.3641732283464567677 ) ) ;
#26426 = CARTESIAN_POINT ( 'NONE',  ( 0.000000000000000000, 0.000000000000000000, 0.000000000000000000 ) ) ;
#26427 = CARTESIAN_POINT ( 'NONE',  ( 0.4133858267716541968, 0.1660481256975885056, 0.3530559997133364547 ) ) ;
#26428 = DIRECTION ( 'NONE',  ( 1.000000000000000000, 0.000000000000000000, 0.000000000000000000 ) ) ;
#26429 = CARTESIAN_POINT ( 'NONE',  ( 1.135170603674541256, 0.1771653543307087630, 0.09757992244046791164 ) ) ;
#26430 = CARTESIAN_POINT ( 'NONE',  ( 0.3280839895013130669, -0.004921259842519576551, 0.3153832671262227771 ) ) ;
#26431 = CARTESIAN_POINT ( 'NONE',  ( -0.4790026246719152336, -0.05778040916215560624, -0.4822834645669293319 ) ) ;
#26432 = CARTESIAN_POINT ( 'NONE',  ( -1.430446194225721390, -0.4281496062992124485, 0.4176697321401328655 ) ) ;
#26433 = CARTESIAN_POINT ( 'NONE',  ( -0.5249343832020990641, 0.1283753931104748280, 0.1820866141732283561 ) ) ;
#26434 = DIRECTION ( 'NONE',  ( -0.7071067811865524577, 0.000000000000000000, 0.7071067811865425767 ) ) ;
#26435 = CARTESIAN_POINT ( 'NONE',  ( 0.6627296587926517768, -0.6692913385826773087, -0.1292274648535924053 ) ) ;
#26436 = CARTESIAN_POINT ( 'NONE',  ( -0.8398950131233585692, 0.2306618581243848609, 0.2411417322834645549 ) ) ;
#26437 = CARTESIAN_POINT ( 'NONE',  ( -0.3460692066303957537, -0.1998031496062994405, -1.074146981627296604 ) ) ;
#26438 = CARTESIAN_POINT ( 'NONE',  ( 0.3917322834645669549, 0.1049643490035304660, -2.729002624671915900 ) ) ;
#26439 = CARTESIAN_POINT ( 'NONE',  ( 0.2362204724409456558, -0.1870078740157480601, -0.3641732283464567677 ) ) ;
#26440 = CARTESIAN_POINT ( 'NONE',  ( -0.8464566929133852113, 0.1660481256975885056, 0.3530559997133364547 ) ) ;
#26441 = CARTESIAN_POINT ( 'NONE',  ( -1.305774278215222184, 0.2952755905511811885, 0.1292274648535926551 ) ) ;
#26442 = CARTESIAN_POINT ( 'NONE',  ( -1.161417322834644716, 0.07958543189024085140, 0.2665933059059887866 ) ) ;
#26443 = CARTESIAN_POINT ( 'NONE',  ( 1.640419947506562393, -0.4281496062992124485, 0.4176697321401328655 ) ) ;
#26444 = CARTESIAN_POINT ( 'NONE',  ( -1.062992125984250968, -0.5511811023622047445, 6.969142054262312111E-17 ) ) ;
#26445 = CARTESIAN_POINT ( 'NONE',  ( -1.653543307086613234, -0.1870078740157480601, -0.3641732283464567677 ) ) ;
#26446 = CARTESIAN_POINT ( 'NONE',  ( 1.181102362204724976, -0.1870078740157480879, -0.4822834645669291653 ) ) ;
#26447 = CARTESIAN_POINT ( 'NONE',  ( 1.141392835773559211, 0.3937007874015747699, 1.339227481442854195 ) ) ;
#26448 = CARTESIAN_POINT ( 'NONE',  ( 0.3917322834645670659, 2.398668435337828261E-17, -2.477053436516747364 ) ) ;
#26449 = EDGE_LOOP ( 'NONE', ( #64221, #28144, #59396, #59510 ) ) ;
#26450 = CARTESIAN_POINT ( 'NONE',  ( -0.7426113562971994320, 1.972848275015058439, 0.5309055118110236338 ) ) ;
#26451 = CARTESIAN_POINT ( 'NONE',  ( 1.581364829396326277, -0.08942795157527998196, 0.3641732283464567121 ) ) ;
#26452 = CARTESIAN_POINT ( 'NONE',  ( -1.233595800524933894, 0.2306618581243848609, 0.2411417322834645549 ) ) ;
#26453 = VECTOR ( 'NONE', #34849, 39.37007874015748143 ) ;
#26454 = EDGE_CURVE ( 'NONE', #81796, #11874, #64189, .T. ) ;
#26455 = CARTESIAN_POINT ( 'NONE',  ( 1.371391076115485719, -0.6692913385826773087, -0.1292274648535924053 ) ) ;
#26456 = CARTESIAN_POINT ( 'NONE',  ( 0.3917322834645670104, 2.398668435337828261E-17, -2.092519685039370358 ) ) ;
#26457 = CARTESIAN_POINT ( 'NONE',  ( -0.7480314960629916854, 2.165354330708661124, 0.000000000000000000 ) ) ;
#26458 = CARTESIAN_POINT ( 'NONE',  ( 0.6496062992125991586, -0.5400638737290845981, -0.3530559997133363437 ) ) ;
#26459 = CARTESIAN_POINT ( 'NONE',  ( -0.03937007874015669567, 0.2952755905511811885, 0.000000000000000000 ) ) ;
#26460 = CARTESIAN_POINT ( 'NONE',  ( 0.2098426342062970074, 1.111641651325031566, -3.931435521548293455 ) ) ;
#26461 = AXIS2_PLACEMENT_3D ( 'NONE', #40171, #65855, #743 ) ;
#26463 = CARTESIAN_POINT ( 'NONE',  ( -0.3996062992125984925, -0.1070741851644056719, -2.642388451443570041 ) ) ;
#26462 = CIRCLE ( 'NONE', #74852, 0.09842519685039344268 ) ;
#26464 = CARTESIAN_POINT ( 'NONE',  ( 0.7349081364829402885, -0.5023911411419708095, -0.1820866141732282451 ) ) ;
#26465 = CARTESIAN_POINT ( 'NONE',  ( -0.1998031496062994683, 0.3460692066303958092, -1.430446194225721834 ) ) ;
#26466 = EDGE_LOOP ( 'NONE', ( #68302, #69147, #32254, #76845 ) ) ;
#26467 = CARTESIAN_POINT ( 'NONE',  ( 0.1958661417322834775, 0.3392501089628018884, -0.1410954312674034816 ) ) ;
#26468 = ORIENTED_EDGE ( 'NONE', *, *, #48374, .F. ) ;
#26469 = CARTESIAN_POINT ( 'NONE',  ( 0.1312335958005255154, -0.6046776061558807314, 0.2411417322834647770 ) ) ;
#26470 = CARTESIAN_POINT ( 'NONE',  ( 1.417322834645670104, -0.1870078740157479769, 0.4822834645669291653 ) ) ;
#26471 = CARTESIAN_POINT ( 'NONE',  ( 0.6955380577427828781, -0.4281496062992124485, 0.4176697321401328655 ) ) ;
#26472 = CARTESIAN_POINT ( 'NONE',  ( 1.056430446194226658, 0.2952755905511811885, 0.1292274648535926551 ) ) ;
#26473 = CARTESIAN_POINT ( 'NONE',  ( 1.522309711286089939, -0.6046776061558809534, -0.2411417322834644161 ) ) ;
#26474 = CARTESIAN_POINT ( 'NONE',  ( -0.6824146981627288167, 0.2306618581243848609, 0.2411417322834645549 ) ) ;
#26475 = CARTESIAN_POINT ( 'NONE',  ( 0.04593175853018440641, 0.2952755905511810774, -0.1292274648535930714 ) ) ;
#26476 = CARTESIAN_POINT ( 'NONE',  ( 1.397637795275591177, -0.5400638737290844871, 0.3530559997133364547 ) ) ;
#26477 = CARTESIAN_POINT ( 'NONE',  ( 1.220472440944882386, -0.6692913385826771977, 8.415575281601705876E-17 ) ) ;
#26478 = CARTESIAN_POINT ( 'NONE',  ( 1.108923884514436686, -0.3162353388693409650, -0.4822834645669289433 ) ) ;
#26479 = CARTESIAN_POINT ( 'NONE',  ( -0.05905511811023545637, -0.5400638737290845981, -0.3530559997133363437 ) ) ;
#26480 = CARTESIAN_POINT ( 'NONE',  ( 4.797336870675656522E-17, -0.3917322834645670104, -0.3858267716535432879 ) ) ;
#26481 = CARTESIAN_POINT ( 'NONE',  ( 0.6299212598425204535, -0.1870078740157480601, -0.3641732283464567677 ) ) ;
#26482 = ORIENTED_EDGE ( 'NONE', *, *, #41448, .T. ) ;
#26483 = CARTESIAN_POINT ( 'NONE',  ( 0.1058382717557500713, -0.3949938075777409408, -0.5577427821522310536 ) ) ;
#26484 = VERTEX_POINT ( 'NONE', #39334 ) ;
#26485 = CARTESIAN_POINT ( 'NONE',  ( -0.4658792650918627265, -0.08942795157527998196, 0.3641732283464567121 ) ) ;
#26486 = CARTESIAN_POINT ( 'NONE',  ( 0.006561679790026889343, -0.3162353388693409650, -0.4822834645669289433 ) ) ;
#26487 = LINE ( 'NONE', #5869, #65011 ) ;
#26488 = CARTESIAN_POINT ( 'NONE',  ( 0.1968503937007881344, 0.2952755905511811885, 0.000000000000000000 ) ) ;
#26489 = CARTESIAN_POINT ( 'NONE',  ( -0.1837270341207343505, -0.6046776061558807314, 0.2411417322834647770 ) ) ;
#26490 = CARTESIAN_POINT ( 'NONE',  ( -0.9448818897637790704, -0.1870078740157479769, 0.4822834645669291653 ) ) ;
#26491 = CARTESIAN_POINT ( 'NONE',  ( 1.476377952755906442, -0.4536011799217367080, 0.2665933059059888421 ) ) ;
#26492 = CYLINDRICAL_SURFACE ( 'NONE', #73490, 0.1937007874015747588 ) ;
#26493 = CARTESIAN_POINT ( 'NONE',  ( 0.1249024489578631214, 1.054114278624317835, 0.2754824702603712039 ) ) ;
#26494 = CARTESIAN_POINT ( 'NONE',  ( 0.8333333333333340365, 0.1771653543307087075, -0.09757992244046823083 ) ) ;
#26495 = CARTESIAN_POINT ( 'NONE',  ( 0.3871391076115493490, -0.3162353388693405765, 0.4822834645669290543 ) ) ;
#26496 = CARTESIAN_POINT ( 'NONE',  ( 0.7480314960629927956, 0.2952755905511811885, 0.000000000000000000 ) ) ;
#26497 = CARTESIAN_POINT ( 'NONE',  ( 0.1998031496062992740, 0.3460692066303959757, -1.404199475065616820 ) ) ;
#26498 = CARTESIAN_POINT ( 'NONE',  ( 0.2726377952755905665, 0.000000000000000000, 0.07874015748031495954 ) ) ;
#26499 = CARTESIAN_POINT ( 'NONE',  ( -9.787531504996566615E-17, 0.3996062992125985480, -0.7066929133858268486 ) ) ;
#26500 = CARTESIAN_POINT ( 'NONE',  ( 0.3996062992125986035, -0.1070741851644052972, -0.03083989501312338344 ) ) ;
#26501 = CARTESIAN_POINT ( 'NONE',  ( -0.05249343832020938322, -0.6046776061558809534, -0.2411417322834644161 ) ) ;
#26502 = CARTESIAN_POINT ( 'NONE',  ( -0.3460692066303958092, -0.1998031496062994683, -2.572178477690288734 ) ) ;
#26503 = CARTESIAN_POINT ( 'NONE',  ( -0.3392501089628017219, -0.1958661417322836718, -2.026902887139107712 ) ) ;
#26504 = CARTESIAN_POINT ( 'NONE',  ( -1.023622047244093558, -0.1870078740157479769, 0.3641732283464567677 ) ) ;
#26505 = CARTESIAN_POINT ( 'NONE',  ( 1.299212598425197429, 0.2952755905511811885, 0.000000000000000000 ) ) ;
#26506 = CARTESIAN_POINT ( 'NONE',  ( 1.391076115485564868, 0.2306618581243847221, -0.2411417322834647770 ) ) ;
#26507 = CARTESIAN_POINT ( 'NONE',  ( -0.2952755905511803003, -0.4536011799217368745, -0.2665933059059886201 ) ) ;
#26508 = CARTESIAN_POINT ( 'NONE',  ( 0.6430446194225728496, 0.05413385826771666132, 0.4176697321401328100 ) ) ;
#26509 = CARTESIAN_POINT ( 'NONE',  ( 0.1265901696524989462, 0.4724409448818897572, -1.645013123359579943 ) ) ;
#26510 = CARTESIAN_POINT ( 'NONE',  ( 0.2821522309711292364, 0.1771653543307087075, -0.09757992244046823083 ) ) ;
#26511 = CARTESIAN_POINT ( 'NONE',  ( -0.01968503937007793844, -0.5400638737290844871, 0.3530559997133364547 ) ) ;
#26512 = CARTESIAN_POINT ( 'NONE',  ( -9.674558042662122972E-17, 0.3949938075777409963, -1.336614173228346081 ) ) ;
#26513 = CARTESIAN_POINT ( 'NONE',  ( -1.049868766404198794, 0.2306618581243847221, -0.2411417322834647770 ) ) ;
#26514 = CARTESIAN_POINT ( 'NONE',  ( 0.3346456692913390985, 0.07958543189024085140, 0.2665933059059887866 ) ) ;
#26515 = CARTESIAN_POINT ( 'NONE',  ( -2.571961977011561817, 1.622068519643037554, -0.4668652553835666574 ) ) ;
#26516 = CARTESIAN_POINT ( 'NONE',  ( -0.8202099737532801971, -0.6692913385826771977, 0.1292274648535927661 ) ) ;
#26517 = CARTESIAN_POINT ( 'NONE',  ( -0.4396325459317577122, -0.5511811023622048555, -0.09757992244046775898 ) ) ;
#26518 = CARTESIAN_POINT ( 'NONE',  ( 0.000000000000000000, 0.000000000000000000, -1.929133858267716661 ) ) ;
#26519 = CARTESIAN_POINT ( 'NONE',  ( -0.6102362204724400829, 0.1660481256975885056, 0.3530559997133364547 ) ) ;
#26520 = CARTESIAN_POINT ( 'NONE',  ( -0.1509186351706028884, -0.3162353388693409650, -0.4822834645669289433 ) ) ;
#26521 = CARTESIAN_POINT ( 'NONE',  ( 0.2887139107611556010, -0.5023911411419708095, 0.1820866141732285504 ) ) ;
#26522 = CARTESIAN_POINT ( 'NONE',  ( -0.3996062992125985480, -7.340648628747423112E-17, -2.163385826771653697 ) ) ;
#26523 = CARTESIAN_POINT ( 'NONE',  ( 0.01968503937007957949, -0.5400638737290845981, -0.3530559997133363437 ) ) ;
#26524 = CIRCLE ( 'NONE', #76220, 0.1190944881889763746 ) ;
#26525 = CARTESIAN_POINT ( 'NONE',  ( 0.3917322834645668994, 0.1049643490035304522, -1.936988558233908808 ) ) ;
#26526 = CARTESIAN_POINT ( 'NONE',  ( -1.640419947506561060, -0.3690944881889765550, -0.3153832671262227771 ) ) ;
#26527 = CARTESIAN_POINT ( 'NONE',  ( 0.7480314960629927956, 0.1771653543307087630, 0.000000000000000000 ) ) ;
#26528 = CARTESIAN_POINT ( 'NONE',  ( 1.561679790026247350, -0.4281496062992124485, 0.4176697321401328655 ) ) ;
#26529 = CARTESIAN_POINT ( 'NONE',  ( -0.8858267716535425107, 0.07958543189024071263, -0.2665933059059888421 ) ) ;
#26530 = ADVANCED_FACE ( 'NONE', ( #51530 ), #77233, .F. ) ;
#26531 = CARTESIAN_POINT ( 'NONE',  ( -1.358267716535432434, 0.07958543189024071263, -0.2665933059059888421 ) ) ;
#26532 = CARTESIAN_POINT ( 'NONE',  ( -0.5708661417322825615, -0.5400638737290844871, 0.3530559997133364547 ) ) ;
#26533 = CARTESIAN_POINT ( 'NONE',  ( -0.2821522309711278487, 0.2952755905511811885, 0.1292274648535926551 ) ) ;
#26534 = CARTESIAN_POINT ( 'NONE',  ( 0.6955380577427828781, -0.3690944881889763329, 0.3153832671262228327 ) ) ;
#26535 = CYLINDRICAL_SURFACE ( 'NONE', #1803, 3.937007874015748143 ) ;
#26536 = CARTESIAN_POINT ( 'NONE',  ( 1.069553805774278610, -0.5511811023622046335, 0.09757992244046803654 ) ) ;
#26537 = ADVANCED_FACE ( 'NONE', ( #58270 ), #34492, .T. ) ;
#26538 = CARTESIAN_POINT ( 'NONE',  ( 0.4986876640419954376, -0.6046776061558809534, -0.2411417322834644161 ) ) ;
#26539 = DIRECTION ( 'NONE',  ( 1.000000000000000000, -0.000000000000000000, -0.000000000000000000 ) ) ;
#26540 = CARTESIAN_POINT ( 'NONE',  ( -0.7414698162729651543, 0.2952755905511810774, -0.1292274648535930714 ) ) ;
#26541 = CARTESIAN_POINT ( 'NONE',  ( 0.1049643490035303689, 0.3917322834645670104, -1.337926509186352142 ) ) ;
#26542 = CARTESIAN_POINT ( 'NONE',  ( 1.305774278215223960, 0.1771653543307087075, -0.09757992244046823083 ) ) ;
#26543 = CARTESIAN_POINT ( 'NONE',  ( 0.4527559055118117182, 0.1660481256975883668, -0.3530559997133364547 ) ) ;
#26544 = CARTESIAN_POINT ( 'NONE',  ( 0.09186351706036827158, 0.05413385826771666132, 0.4176697321401328100 ) ) ;
#26545 = DIRECTION ( 'NONE',  ( 0.000000000000000000, 0.000000000000000000, -1.000000000000000000 ) ) ;
#26546 = CARTESIAN_POINT ( 'NONE',  ( 0.07874015748031558404, -0.1870078740157479769, 0.3641732283464567677 ) ) ;
#26547 = CARTESIAN_POINT ( 'NONE',  ( 0.9317585301837276734, 0.05413385826771626580, -0.4176697321401330321 ) ) ;
#26548 = CARTESIAN_POINT ( 'NONE',  ( -0.5314960629921254842, -0.4536011799217368745, -0.2665933059059886201 ) ) ;
#26549 = CARTESIAN_POINT ( 'NONE',  ( -0.7874015748031489847, -0.1870078740157480879, -0.4822834645669291653 ) ) ;
#26550 = CARTESIAN_POINT ( 'NONE',  ( -0.1265901696524986964, -0.4724409448818899238, -2.591863517060367439 ) ) ;
#26551 = CARTESIAN_POINT ( 'NONE',  ( -0.3346456692913377662, -0.5400638737290844871, 0.3530559997133364547 ) ) ;
#26552 = VERTEX_POINT ( 'NONE', #73840 ) ;
#26553 = CARTESIAN_POINT ( 'NONE',  ( -1.030183727034119867, -0.3162353388693405765, 0.4822834645669290543 ) ) ;
#26554 = CARTESIAN_POINT ( 'NONE',  ( -0.7939632545931754048, -0.2845877964562159024, 0.3641732283464567677 ) ) ;
#26555 = CARTESIAN_POINT ( 'NONE',  ( 5.463695987328526437E-16, -0.1870078740157479769, 0.4822834645669291653 ) ) ;
#26556 = CARTESIAN_POINT ( 'NONE',  ( -1.167979002624671470, -0.4281496062992127816, -0.4176697321401328100 ) ) ;
#26557 = CARTESIAN_POINT ( 'NONE',  ( -0.8333333333333323711, 0.2952755905511811885, 0.1292274648535926551 ) ) ;
#26558 = LINE ( 'NONE', #40438, #49830 ) ;
#26560 = CARTESIAN_POINT ( 'NONE',  ( 0.8267716535433077274, 0.2952755905511811885, 0.000000000000000000 ) ) ;
#26559 = CARTESIAN_POINT ( 'NONE',  ( 1.056430446194226658, 0.2952755905511811885, 0.1292274648535926551 ) ) ;
#26561 = CARTESIAN_POINT ( 'NONE',  ( 1.108923884514436686, -0.3162353388693409650, -0.4822834645669289433 ) ) ;
#26562 = CARTESIAN_POINT ( 'NONE',  ( -9.594673741351313045E-17, 0.3917322834645670104, -2.669291338582676865 ) ) ;
#26563 = CARTESIAN_POINT ( 'NONE',  ( -1.535433070866141225, -0.6692913385826771977, 8.415575281601705876E-17 ) ) ;
#26564 = CARTESIAN_POINT ( 'NONE',  ( -1.246719160104986512, 0.05413385826771666132, 0.4176697321401328100 ) ) ;
#26565 = CARTESIAN_POINT ( 'NONE',  ( 0.4091458600556404646, -0.2362204724409448231, -0.7349081364829396223 ) ) ;
#26566 = CARTESIAN_POINT ( 'NONE',  ( -0.3460692066303960868, 0.1998031496062990242, -0.02624671916010500733 ) ) ;
#26568 = EDGE_CURVE ( 'NONE', #41893, #15840, #17092, .T. ) ;
#26567 = ORIENTED_EDGE ( 'NONE', *, *, #47141, .T. ) ;
#26569 = CARTESIAN_POINT ( 'NONE',  ( -0.05905511811023545637, 0.07958543189024085140, 0.2665933059059887866 ) ) ;
#26570 = CARTESIAN_POINT ( 'NONE',  ( -0.1958661417322834220, -0.3392501089628018884, -1.632545931758530244 ) ) ;
#26571 = ORIENTED_EDGE ( 'NONE', *, *, #5433, .F. ) ;
#26572 = CARTESIAN_POINT ( 'NONE',  ( 0.1312335958005255154, -0.6046776061558807314, 0.2411417322834647770 ) ) ;
#26573 = CARTESIAN_POINT ( 'NONE',  ( -0.01968503937007793844, -0.5400638737290844871, 0.3530559997133364547 ) ) ;
#26574 = CARTESIAN_POINT ( 'NONE',  ( -0.02578378529929148399, 0.3963884504522700580, -2.755905511811024056 ) ) ;
#26575 = DIRECTION ( 'NONE',  ( 0.000000000000000000, 0.000000000000000000, -1.000000000000000000 ) ) ;
#26576 = CARTESIAN_POINT ( 'NONE',  ( -0.7677165354330699465, -0.4536011799217368745, -0.2665933059059886201 ) ) ;
#26577 = PLANE ( 'NONE',  #34647 ) ;
#26578 = CARTESIAN_POINT ( 'NONE',  ( 0.6102362204724416372, 0.1660481256975883668, -0.3530559997133364547 ) ) ;
#26579 = CARTESIAN_POINT ( 'NONE',  ( 0.8398950131233602345, 0.1283753931104746893, -0.1820866141732285504 ) ) ;
#26580 = CARTESIAN_POINT ( 'NONE',  ( -0.3608923884514428360, 0.2952755905511811885, 0.1292274648535926551 ) ) ;
#26581 = CARTESIAN_POINT ( 'NONE',  ( -0.1049643490035306742, 0.3917322834645668994, -1.346437377131546764 ) ) ;
#26582 = CARTESIAN_POINT ( 'NONE',  ( -0.8333333333333323711, 0.2952755905511811885, 0.1292274648535926551 ) ) ;
#26583 = CARTESIAN_POINT ( 'NONE',  ( 1.595398199321655275, 0.7375059713363276703, 0.1559797534342493575 ) ) ;
#26584 = CARTESIAN_POINT ( 'NONE',  ( 1.312335958005250269, -0.6046776061558807314, 0.2411417322834647770 ) ) ;
#26585 = CARTESIAN_POINT ( 'NONE',  ( 1.587926509186352586, -0.3690944881889765550, -0.3153832671262227771 ) ) ;
#26586 = VERTEX_POINT ( 'NONE', #2299 ) ;
#26587 = CARTESIAN_POINT ( 'NONE',  ( 0.3917322834645670104, 0.1049643490035304660, -2.483615116306773452 ) ) ;
#26588 = CARTESIAN_POINT ( 'NONE',  ( -0.2034120734908128059, 0.2952755905511811885, 0.1292274648535926551 ) ) ;
#26589 = ORIENTED_EDGE ( 'NONE', *, *, #5285, .T. ) ;
#26590 = CONICAL_SURFACE ( 'NONE', #21239, 2.559055118110236560, 0.7853981633974500554 ) ;
#26591 = CARTESIAN_POINT ( 'NONE',  ( -0.5708661417322828946, 0.1660481256975883668, -0.3530559997133364547 ) ) ;
#26592 = CARTESIAN_POINT ( 'NONE',  ( 1.397637795275591177, -0.5400638737290844871, 0.3530559997133364547 ) ) ;
#26593 = CARTESIAN_POINT ( 'NONE',  ( 1.279527559055118724, 0.1660481256975885056, 0.3530559997133364547 ) ) ;
#26594 = CARTESIAN_POINT ( 'NONE',  ( 0.3215223097112867578, -0.05778040916215522460, 0.4822834645669289988 ) ) ;
#26595 = CARTESIAN_POINT ( 'NONE',  ( -0.2887139107611542133, -0.6046776061558809534, -0.2411417322834644161 ) ) ;
#26596 = CARTESIAN_POINT ( 'NONE',  ( -0.1958661417322836718, 0.3392501089628017219, -1.987532808398950079 ) ) ;
#26597 = CARTESIAN_POINT ( 'NONE',  ( -1.003937007874015297, -0.5400638737290845981, -0.3530559997133363437 ) ) ;
#26598 = CARTESIAN_POINT ( 'NONE',  ( 0.006561679790026889343, -0.3162353388693409650, -0.4822834645669289433 ) ) ;
#26599 = CARTESIAN_POINT ( 'NONE',  ( -0.07874015748031421014, -0.1870078740157479769, 0.3641732283464567677 ) ) ;
#26600 = CARTESIAN_POINT ( 'NONE',  ( 1.594488188976378673, -0.5400638737290845981, -0.3530559997133363437 ) ) ;
#26601 = CARTESIAN_POINT ( 'NONE',  ( 1.338582677165355062, -0.1870078740157479769, 0.4822834645669291653 ) ) ;
#26602 = CARTESIAN_POINT ( 'NONE',  ( -0.5314960629921254842, -0.5400638737290845981, -0.3530559997133363437 ) ) ;
#26603 = CARTESIAN_POINT ( 'NONE',  ( -0.5314960629921394730, 2.745602313593968891, 3.861135848600277143 ) ) ;
#26604 = CARTESIAN_POINT ( 'NONE',  ( 1.279527559055118724, 0.1660481256975885056, 0.3530559997133364547 ) ) ;
#26605 = CARTESIAN_POINT ( 'NONE',  ( 2.795275590551181466, 2.793565526369266916, 0.000000000000000000 ) ) ;
#26606 = ORIENTED_EDGE ( 'NONE', *, *, #34823, .F. ) ;
#26607 = CARTESIAN_POINT ( 'NONE',  ( 0.4330708661417329575, 0.2952755905511811885, 0.000000000000000000 ) ) ;
#26608 = CARTESIAN_POINT ( 'NONE',  ( -0.1312335958005241554, 0.1283753931104748280, 0.1820866141732283561 ) ) ;
#26610 = CARTESIAN_POINT ( 'NONE',  ( -0.9321091654255228010, 0.004960608223778174841, 0.3437734562760193513 ) ) ;
#26609 = CARTESIAN_POINT ( 'NONE',  ( 1.292650918635171564, -0.5511811023622048555, -0.09757992244046775898 ) ) ;
#26611 = CARTESIAN_POINT ( 'NONE',  ( -0.3458507752293906723, -0.3458507752293910609, -0.1358267716535432879 ) ) ;
#26612 = CARTESIAN_POINT ( 'NONE',  ( -1.614173228346457378, 1.330640075373402897, -0.1372047244094477536 ) ) ;
#26613 = CARTESIAN_POINT ( 'NONE',  ( 1.279527559055118724, 0.1660481256975885056, 0.3530559997133364547 ) ) ;
#26614 = CARTESIAN_POINT ( 'NONE',  ( -0.3949938075777408852, -0.1058382717557502933, 0.03477690288713909672 ) ) ;
#26615 = CARTESIAN_POINT ( 'NONE',  ( 0.2099737532808405305, 0.2306618581243847221, -0.2411417322834647770 ) ) ;
#26616 = CARTESIAN_POINT ( 'NONE',  ( -1.548556430446193399, -0.6046776061558809534, -0.2411417322834644161 ) ) ;
#26617 = CARTESIAN_POINT ( 'NONE',  ( -1.574803149606298636, -0.1870078740157479769, 0.4822834645669291653 ) ) ;
#26618 = CARTESIAN_POINT ( 'NONE',  ( -0.1115485564304456306, 0.2952755905511810774, -0.1292274648535930714 ) ) ;
#26619 = CARTESIAN_POINT ( 'NONE',  ( -0.1058382717557497660, -0.3949938075777411073, -0.1489501312335957950 ) ) ;
#26620 = CARTESIAN_POINT ( 'NONE',  ( 1.548556430446194954, 0.2306618581243847221, -0.2411417322834647770 ) ) ;
#26621 = CARTESIAN_POINT ( 'NONE',  ( 0.6889763779527563470, 0.1660481256975883668, -0.3530559997133364547 ) ) ;
#26622 = CARTESIAN_POINT ( 'NONE',  ( 1.122047244094488860, -0.4536011799217368745, -0.2665933059059886201 ) ) ;
#26623 = CARTESIAN_POINT ( 'NONE',  ( 0.1876687465225647666, 1.067092265285233266, 0.2507773264951494996 ) ) ;
#26624 = CARTESIAN_POINT ( 'NONE',  ( 0.8661417322834653598, -0.1870078740157479769, 0.3641732283464567677 ) ) ;
#26625 = CARTESIAN_POINT ( 'NONE',  ( -1.181102362204723644, -0.1870078740157479769, 0.4822834645669291653 ) ) ;
#26626 = CARTESIAN_POINT ( 'NONE',  ( -0.1070741851644051862, -0.3996062992125986590, -1.093832020997375087 ) ) ;
#26627 = CARTESIAN_POINT ( 'NONE',  ( 1.332020997375329197, -0.3162353388693405765, 0.4822834645669290543 ) ) ;
#26628 = CARTESIAN_POINT ( 'NONE',  ( 0.3392501089628018329, 0.1958661417322835607, -0.7532808398950130435 ) ) ;
#26630 = FACE_OUTER_BOUND ( 'NONE', #19296, .T. ) ;
#26629 = CARTESIAN_POINT ( 'NONE',  ( 0.5839895013123367340, 0.2952755905511811885, 0.1292274648535926551 ) ) ;
#26631 = FACE_OUTER_BOUND ( 'NONE', #7245, .T. ) ;
#26632 = CARTESIAN_POINT ( 'NONE',  ( 0.5052493438320215802, 0.1771653543307087630, 0.09757992244046791164 ) ) ;
#26633 = EDGE_CURVE ( 'NONE', #79730, #68390, #66694, .T. ) ;
#26634 = CARTESIAN_POINT ( 'NONE',  ( 0.4068241469816281097, 0.05413385826771666132, 0.4176697321401328100 ) ) ;
#26635 = CARTESIAN_POINT ( 'NONE',  ( 1.679790026246720025, 0.1283753931104748280, 0.1820866141732283561 ) ) ;
#26636 = CARTESIAN_POINT ( 'NONE',  ( -0.8464566929133852113, -0.4536011799217368745, -0.2665933059059886201 ) ) ;
#26637 = CARTESIAN_POINT ( 'NONE',  ( -1.102362204724408601, -0.1870078740157479769, 0.4822834645669291653 ) ) ;
#26638 = CARTESIAN_POINT ( 'NONE',  ( -1.719160104986876103, 0.05413385826771666132, 0.4176697321401328100 ) ) ;
#26639 = CARTESIAN_POINT ( 'NONE',  ( 0.9842519685039378130, -0.6692913385826771977, 8.415575281601705876E-17 ) ) ;
#26640 = CARTESIAN_POINT ( 'NONE',  ( 1.607611548556431069, -0.6692913385826773087, -0.1292274648535924053 ) ) ;
#26641 = CARTESIAN_POINT ( 'NONE',  ( -0.3957358693849766240, -0.01930322177395251207, -1.220472440945443493 ) ) ;
#26642 = CARTESIAN_POINT ( 'NONE',  ( 0.8595800524934390507, -0.05778040916215560624, -0.4822834645669293319 ) ) ;
#26643 = CARTESIAN_POINT ( 'NONE',  ( 0.1265901696524990294, -0.4724409448818896462, -2.681758530183727895 ) ) ;
#26644 = FACE_OUTER_BOUND ( 'NONE', #53183, .T. ) ;
#26645 = CARTESIAN_POINT ( 'NONE',  ( 1.279527559055118724, -0.5400638737290845981, -0.3530559997133363437 ) ) ;
#26646 = CARTESIAN_POINT ( 'NONE',  ( -1.279527559055116948, -0.4536011799217367080, 0.2665933059059888421 ) ) ;
#26647 = CARTESIAN_POINT ( 'NONE',  ( 1.089238845144357759, -0.004921259842519870586, -0.3153832671262229437 ) ) ;
#26648 = CARTESIAN_POINT ( 'NONE',  ( -1.502624671916009680, -0.2845877964562159024, 0.3641732283464567677 ) ) ;
#26649 = CARTESIAN_POINT ( 'NONE',  ( -0.5971128608923877978, -0.5511811023622048555, -0.09757992244046775898 ) ) ;
#26650 = DIRECTION ( 'NONE',  ( 1.000000000000000000, 1.408710688920637755E-15, 0.000000000000000000 ) ) ;
#26651 = CARTESIAN_POINT ( 'NONE',  ( 0.7480314960629927956, -0.5511811023622047445, 6.969142054262312111E-17 ) ) ;
#26652 = CARTESIAN_POINT ( 'NONE',  ( 0.5380577427821529035, -0.4281496062992124485, 0.4176697321401328655 ) ) ;
#26653 = CARTESIAN_POINT ( 'NONE',  ( 0.9842519685039375910, 0.2952755905511811885, 0.000000000000000000 ) ) ;
#26654 = CARTESIAN_POINT ( 'NONE',  ( -0.07874015748031421014, -0.1870078740157479769, 0.4822834645669291653 ) ) ;
#26655 = CARTESIAN_POINT ( 'NONE',  ( 0.7283464566929140904, -0.4536011799217368745, -0.2665933059059886201 ) ) ;
#26657 = CARTESIAN_POINT ( 'NONE',  ( 1.286089238845145033, 0.2306618581243848609, 0.2411417322834645549 ) ) ;
#26656 = B_SPLINE_CURVE_WITH_KNOTS ( 'NONE', 3,
 ( #2029, #9178, #66421, #40329, #73149, #21792, #2453 ),
 .UNSPECIFIED., .F., .F.,
 ( 4, 3, 4 ),
 ( 1.561251128379126385E-17, 0.001246230184515585400, 0.002492489877932648965 ),
 .UNSPECIFIED. ) ;
#26658 = DIRECTION ( 'NONE',  ( 0.000000000000000000, 0.000000000000000000, -1.000000000000000000 ) ) ;
#26659 = CARTESIAN_POINT ( 'NONE',  ( -0.7283464566929126471, 0.1660481256975883668, -0.3530559997133364547 ) ) ;
#26660 = CARTESIAN_POINT ( 'NONE',  ( -0.2925321140481932369, 0.2925321140481931814, -0.1771653543307086798 ) ) ;
#26661 = CARTESIAN_POINT ( 'NONE',  ( 0.2296587926509192634, -0.05778040916215560624, -0.4822834645669293319 ) ) ;
#26662 = CARTESIAN_POINT ( 'NONE',  ( -0.2427821522309703550, -0.3162353388693405765, 0.4822834645669290543 ) ) ;
#26663 = CARTESIAN_POINT ( 'NONE',  ( -0.1246719160104980823, 0.2952755905511811885, 0.1292274648535926551 ) ) ;
#26664 = CARTESIAN_POINT ( 'NONE',  ( 0.3996062992125986590, -0.1070741851644053111, -2.473753280839894764 ) ) ;
#26665 = CARTESIAN_POINT ( 'NONE',  ( -0.2891555358219908833, -0.2891555358219912164, -2.106299212598425452 ) ) ;
#26666 = CARTESIAN_POINT ( 'NONE',  ( -0.3392501089628019995, 0.1958661417322832277, -0.4908136482939632339 ) ) ;
#26667 = CARTESIAN_POINT ( 'NONE',  ( 0.2814827926786539480, -0.08976297916237284402, 5.855142794233184844 ) ) ;
#26668 = CARTESIAN_POINT ( 'NONE',  ( 0.1049643490035304799, -0.3917322834645669549, -1.022309711286089051 ) ) ;
#26669 = CARTESIAN_POINT ( 'NONE',  ( -0.8989501312335946848, 0.1771653543307087075, -0.09757992244046823083 ) ) ;
#26670 = CARTESIAN_POINT ( 'NONE',  ( 0.3392501089628018884, -0.1958661417322834220, -0.8845144356955378928 ) ) ;
#26671 = CARTESIAN_POINT ( 'NONE',  ( -0.9776902887139098386, -0.6692913385826771977, 0.1292274648535927661 ) ) ;
#26672 = CARTESIAN_POINT ( 'NONE',  ( 0.2867679344610365999, -0.2867679344610365999, -0.02097805954624490030 ) ) ;
#26673 = CARTESIAN_POINT ( 'NONE',  ( 0.2362204724409456558, -0.1870078740157479769, 0.4822834645669291653 ) ) ;
#26674 = CARTESIAN_POINT ( 'NONE',  ( -0.4986876640419942164, -0.5023911411419708095, 0.1820866141732285504 ) ) ;
#26675 = CARTESIAN_POINT ( 'NONE',  ( 1.148293963254593653, 0.2952755905511810774, -0.1292274648535930714 ) ) ;
#26676 = CARTESIAN_POINT ( 'NONE',  ( 0.2099737532808405305, 0.2306618581243847221, -0.2411417322834647770 ) ) ;
#26677 = CARTESIAN_POINT ( 'NONE',  ( 0.1687987930166117423, 1.093765707632013306, 1.109372847106409932 ) ) ;
#26678 = CARTESIAN_POINT ( 'NONE',  ( -0.3996062992125986035, -0.1070741851644056997, -2.565616797900262647 ) ) ;
#26679 = CARTESIAN_POINT ( 'NONE',  ( 0.3917322834645670104, 0.1049643490035304660, -1.066292281661104457 ) ) ;
#26680 = CARTESIAN_POINT ( 'NONE',  ( 1.351706036745407680, 0.05413385826771666132, 0.4176697321401328100 ) ) ;
#26681 = CARTESIAN_POINT ( 'NONE',  ( 0.4790026246719167324, -0.05778040916215522460, 0.4822834645669289988 ) ) ;
#26682 = CARTESIAN_POINT ( 'NONE',  ( 0.2624671916010504757, -0.6046776061558809534, -0.2411417322834644161 ) ) ;
#26683 = CARTESIAN_POINT ( 'NONE',  ( 1.338582677165355062, -0.1870078740157479769, 0.4822834645669291653 ) ) ;
#26684 =( REPRESENTATION_RELATIONSHIP ('NONE','NONE', #79348, #48103 ) REPRESENTATION_RELATIONSHIP_WITH_TRANSFORMATION ( #62020 )SHAPE_REPRESENTATION_RELATIONSHIP( ) );
#26685 = CARTESIAN_POINT ( 'NONE',  ( 0.1958661417322834775, 0.3392501089628018884, -0.5439632545931759600 ) ) ;
#26686 = CARTESIAN_POINT ( 'NONE',  ( -0.05905511811023545637, -0.5400638737290845981, -0.3530559997133363437 ) ) ;
#26687 = CARTESIAN_POINT ( 'NONE',  ( 0.9251968503937015864, 0.1660481256975883668, -0.3530559997133364547 ) ) ;
#26688 = CARTESIAN_POINT ( 'NONE',  ( 0.3608923884514443348, -0.6692913385826771977, 0.1292274648535927661 ) ) ;
#26689 = CARTESIAN_POINT ( 'NONE',  ( 0.9645669291338591078, -0.4536011799217368745, -0.2665933059059886201 ) ) ;
#26690 = CARTESIAN_POINT ( 'NONE',  ( -1.108923884514435132, -0.3162353388693405765, 0.4822834645669290543 ) ) ;
#26691 = CARTESIAN_POINT ( 'NONE',  ( -1.417322834645668772, -0.1870078740157479769, 0.4822834645669291653 ) ) ;
#26692 = CARTESIAN_POINT ( 'NONE',  ( 0.6824146981627303710, 0.2306618581243847221, -0.2411417322834647770 ) ) ;
#26693 = CYLINDRICAL_SURFACE ( 'NONE', #77547, 0.1574803149606299746 ) ;
#26694 = CARTESIAN_POINT ( 'NONE',  ( -0.3917322834645671215, 0.1049643490035301469, -2.072178477690288734 ) ) ;
#26695 = ORIENTED_EDGE ( 'NONE', *, *, #33639, .F. ) ;
#26696 = CARTESIAN_POINT ( 'NONE',  ( -0.1070741851644056997, 0.3996062992125986035, -0.1640419947506562004 ) ) ;
#26697 = ORIENTED_EDGE ( 'NONE', *, *, #29666, .F. ) ;
#26698 = CARTESIAN_POINT ( 'NONE',  ( 1.430446194225722500, -0.4281496062992127816, -0.4176697321401328100 ) ) ;
#26699 = CARTESIAN_POINT ( 'NONE',  ( 1.115485564304462551, -0.004921259842519576551, 0.3153832671262227771 ) ) ;
#26700 = CARTESIAN_POINT ( 'NONE',  ( -0.2726377952755906220, 0.1133856558944467546, 0.1574803149606299191 ) ) ;
#26701 = CARTESIAN_POINT ( 'NONE',  ( -0.7080320533160963103, 2.401574803149606474, 0.4915354330708645025 ) ) ;
#26702 = PLANE ( 'NONE',  #41705 ) ;
#26703 = CARTESIAN_POINT ( 'NONE',  ( 0.1049643490035303689, 0.3917322834645670104, -0.7080052493438320216 ) ) ;
#26704 = CARTESIAN_POINT ( 'NONE',  ( -1.318897637795274802, 0.07958543189024085140, 0.2665933059059887866 ) ) ;
#26705 = CARTESIAN_POINT ( 'NONE',  ( 1.548556430446194954, -0.6046776061558807314, 0.2411417322834647770 ) ) ;
#26706 = CARTESIAN_POINT ( 'NONE',  ( 0.4359958488159859091, 1.724409448818897905, -3.912791665790197992 ) ) ;
#26707 = CARTESIAN_POINT ( 'NONE',  ( -0.4658792650918627265, -0.05778040916215522460, 0.4822834645669289988 ) ) ;
#26708 = CARTESIAN_POINT ( 'NONE',  ( 1.023622047244095112, -0.1870078740157480879, -0.4822834645669291653 ) ) ;
#26709 = ORIENTED_EDGE ( 'NONE', *, *, #79843, .T. ) ;
#26710 = CARTESIAN_POINT ( 'NONE',  ( -1.528871391076114250, 0.2952755905511810774, -0.1292274648535930714 ) ) ;
#26711 = CARTESIAN_POINT ( 'NONE',  ( -0.7197590744588117095, -5.642773921931522838E-15, -0.3954985857520079695 ) ) ;
#26712 = CARTESIAN_POINT ( 'NONE',  ( 1.964447536376671133, 3.481290980825508807, 6.391091853172183868 ) ) ;
#26713 = DIRECTION ( 'NONE',  ( 0.000000000000000000, 1.000000000000000000, -0.000000000000000000 ) ) ;
#26714 = CARTESIAN_POINT ( 'NONE',  ( -0.8464566929133852113, 0.07958543189024085140, 0.2665933059059887866 ) ) ;
#26715 = EDGE_CURVE ( 'NONE', #51415, #32057, #79746, .T. ) ;
#26716 = DIRECTION ( 'NONE',  ( 0.000000000000000000, 0.000000000000000000, 1.000000000000000000 ) ) ;
#26717 = CARTESIAN_POINT ( 'NONE',  ( 0.4002624671916016896, -0.05778040916215522460, 0.4822834645669289988 ) ) ;
#26718 = VERTEX_POINT ( 'NONE', #46474 ) ;
#26720 = DIRECTION ( 'NONE',  ( 0.000000000000000000, 0.000000000000000000, -1.000000000000000000 ) ) ;
#26719 = DIRECTION ( 'NONE',  ( -0.000000000000000000, -1.000000000000000000, -0.000000000000000000 ) ) ;
#26721 = CARTESIAN_POINT ( 'NONE',  ( 1.377952755905512472, 0.2952755905511811885, 0.000000000000000000 ) ) ;
#26722 = CARTESIAN_POINT ( 'NONE',  ( 1.607611548556431069, 0.1771653543307087630, 0.09757992244046791164 ) ) ;
#26723 = CARTESIAN_POINT ( 'NONE',  ( -0.1958661417322834497, -0.3392501089628018884, -0.7755712353992633146 ) ) ;
#26724 = CARTESIAN_POINT ( 'NONE',  ( -0.9973753280839886548, -0.5023911411419708095, -0.1820866141732282451 ) ) ;
#26725 = CARTESIAN_POINT ( 'NONE',  ( -1.469816272965878357, 0.1283753931104748280, 0.1820866141732283561 ) ) ;
#26726 = CARTESIAN_POINT ( 'NONE',  ( 0.3458507752293908943, 0.3458507752293908943, -0.7677165354330708347 ) ) ;
#26727 = CARTESIAN_POINT ( 'NONE',  ( 0.4068241469816279987, -0.4281496062992127816, -0.4176697321401328100 ) ) ;
#26728 = CARTESIAN_POINT ( 'NONE',  ( -0.8464566929133852113, 0.07958543189024085140, 0.2665933059059887866 ) ) ;
#26729 = CARTESIAN_POINT ( 'NONE',  ( 5.463695987328526437E-16, -0.1870078740157479769, 0.3641732283464567677 ) ) ;
#26730 = CARTESIAN_POINT ( 'NONE',  ( 0.2887139107611556010, -0.6046776061558807314, 0.2411417322834647770 ) ) ;
#26731 = CARTESIAN_POINT ( 'NONE',  ( -1.181102362204723644, -0.1870078740157479769, 0.3641732283464567677 ) ) ;
#26732 = CARTESIAN_POINT ( 'NONE',  ( -0.1958661417322836995, 0.3392501089628017219, -0.1673421504275084681 ) ) ;
#26733 = CARTESIAN_POINT ( 'NONE',  ( 0.8267716535433077274, 0.2952755905511811885, 0.000000000000000000 ) ) ;
#26734 = CARTESIAN_POINT ( 'NONE',  ( -1.587926509186350810, 0.05413385826771626580, -0.4176697321401330321 ) ) ;
#26735 = CARTESIAN_POINT ( 'NONE',  ( -1.157146581871515012E-16, 0.4724409448818898682, -1.336614173228346303 ) ) ;
#26736 = CARTESIAN_POINT ( 'NONE',  ( -0.6102362204724400829, 0.1660481256975885056, 0.3530559997133364547 ) ) ;
#26737 = CARTESIAN_POINT ( 'NONE',  ( 0.006561679790026889343, -0.08942795157527998196, 0.3641732283464567121 ) ) ;
#26738 = CARTESIAN_POINT ( 'NONE',  ( -0.8267716535433065062, 0.2952755905511811885, 0.000000000000000000 ) ) ;
#26739 = CARTESIAN_POINT ( 'NONE',  ( 0.7086614173228353852, -0.1870078740157479769, 0.3641732283464567677 ) ) ;
#26740 = CARTESIAN_POINT ( 'NONE',  ( -0.2165354330708654795, -0.4536011799217368745, -0.2665933059059886201 ) ) ;
#26741 = CARTESIAN_POINT ( 'NONE',  ( -0.6561679790026240244, -0.6046776061558807314, 0.2411417322834647770 ) ) ;
#26742 = CARTESIAN_POINT ( 'NONE',  ( -1.069553805774277722, 0.2952755905511811885, 0.1292274648535926551 ) ) ;
#26743 = CARTESIAN_POINT ( 'NONE',  ( 2.787279214012418738, 0.000000000000000000, 0.000000000000000000 ) ) ;
#26744 = CARTESIAN_POINT ( 'NONE',  ( 1.423884514435696413, -0.2845877964562161244, -0.3641732283464567121 ) ) ;
#26745 = CARTESIAN_POINT ( 'NONE',  ( 0.4593175853018380828, 0.05413385826771626580, -0.4176697321401330321 ) ) ;
#26746 = DIRECTION ( 'NONE',  ( -0.000000000000000000, -1.000000000000000000, -0.000000000000000000 ) ) ;
#26747 = CARTESIAN_POINT ( 'NONE',  ( -1.679790026246718693, 0.2306618581243847221, -0.2411417322834647770 ) ) ;
#26748 = ORIENTED_EDGE ( 'NONE', *, *, #48534, .F. ) ;
#26749 = CARTESIAN_POINT ( 'NONE',  ( -0.3460692066303957537, -0.1998031496062994405, -2.491469816272966042 ) ) ;
#26750 = CARTESIAN_POINT ( 'NONE',  ( -0.8398950131233585692, 0.1283753931104748280, 0.1820866141732283561 ) ) ;
#26751 = CARTESIAN_POINT ( 'NONE',  ( 0.8595800524934390507, -0.05778040916215560624, -0.4822834645669293319 ) ) ;
#26752 = CARTESIAN_POINT ( 'NONE',  ( -1.207349081364828880, 0.1283753931104746893, -0.1820866141732285504 ) ) ;
#26753 = CARTESIAN_POINT ( 'NONE',  ( 0.3996062992125984925, 0.1070741851644054637, -1.618766404199474929 ) ) ;
#26754 = CARTESIAN_POINT ( 'NONE',  ( -0.8858267716535425107, 0.1660481256975883668, -0.3530559997133364547 ) ) ;
#26755 = CARTESIAN_POINT ( 'NONE',  ( 0.9711286089238851948, -0.6046776061558809534, -0.2411417322834644161 ) ) ;
#26756 = CARTESIAN_POINT ( 'NONE',  ( 0.5118110236220480003, -0.6692913385826771977, 8.415575281601705876E-17 ) ) ;
#26757 = CARTESIAN_POINT ( 'NONE',  ( 1.194225721784777594, -0.4281496062992127816, -0.4176697321401328100 ) ) ;
#26758 = CARTESIAN_POINT ( 'NONE',  ( -1.535433070866141225, 0.1771653543307087630, 0.000000000000000000 ) ) ;
#26759 = CARTESIAN_POINT ( 'NONE',  ( -0.1998031496062994405, 0.3460692066303957537, -1.034776902887139194 ) ) ;
#26760 = CARTESIAN_POINT ( 'NONE',  ( 4.893765752498283924E-17, -0.3996062992125986035, -1.338582677165354173 ) ) ;
#26761 = CARTESIAN_POINT ( 'NONE',  ( 0.3949938075777409963, 2.418639510665530435E-17, -0.5905511811023622659 ) ) ;
#26762 = CARTESIAN_POINT ( 'NONE',  ( 1.191111281560510715, -4.927456884911482678E-16, 0.4445507791589062840 ) ) ;
#26763 = CARTESIAN_POINT ( 'NONE',  ( 0.7808398950131241190, -0.08942795157528024563, -0.3641732283464568787 ) ) ;
#26764 = CARTESIAN_POINT ( 'NONE',  ( 0.1771653543307093182, 0.07958543189024085140, 0.2665933059059887866 ) ) ;
#26765 = CARTESIAN_POINT ( 'NONE',  ( -0.08530183727034056085, -0.05778040916215560624, -0.4822834645669293319 ) ) ;
#26766 = CARTESIAN_POINT ( 'NONE',  ( 1.102362204724410155, -0.1870078740157479769, 0.4822834645669291653 ) ) ;
#26767 = CARTESIAN_POINT ( 'NONE',  ( 0.2891555358219910499, -0.2891555358219909944, -1.907480314960629419 ) ) ;
#26768 = CARTESIAN_POINT ( 'NONE',  ( 0.3215223097112867578, -0.2845877964562161244, -0.3641732283464567121 ) ) ;
#26769 = CARTESIAN_POINT ( 'NONE',  ( -0.7808398950131222316, -0.3162353388693409650, -0.4822834645669289433 ) ) ;
#26770 = CARTESIAN_POINT ( 'NONE',  ( 1.410761154855643795, -0.3162353388693405765, 0.4822834645669290543 ) ) ;
#26771 = CARTESIAN_POINT ( 'NONE',  ( 0.9186351706036752773, 0.2306618581243847221, -0.2411417322834647770 ) ) ;
#26772 = CARTESIAN_POINT ( 'NONE',  ( 0.4724409448818896462, 0.1265901696524990294, -1.856955380577427928 ) ) ;
#26773 = CARTESIAN_POINT ( 'NONE',  ( 0.3272402980636514580, -0.2155943732411718938, -2.755905511811024944 ) ) ;
#26774 = ORIENTED_EDGE ( 'NONE', *, *, #38804, .T. ) ;
#26775 = EDGE_LOOP ( 'NONE', ( #26037, #10638, #15451, #32705 ) ) ;
#26776 = CARTESIAN_POINT ( 'NONE',  ( -1.463254593175852492, -0.6692913385826773087, -0.1292274648535924053 ) ) ;
#26778 = CARTESIAN_POINT ( 'NONE',  ( -0.6299212598425188991, -0.1870078740157480879, -0.4822834645669291653 ) ) ;
#26777 = CARTESIAN_POINT ( 'NONE',  ( -0.7742782152230962556, -0.3690944881889765550, -0.3153832671262227771 ) ) ;
#26779 = CARTESIAN_POINT ( 'NONE',  ( -0.3392501089628019439, 0.1958661417322832554, -2.468484621226035181 ) ) ;
#26780 = FACE_OUTER_BOUND ( 'NONE', #82780, .T. ) ;
#26781 = CARTESIAN_POINT ( 'NONE',  ( 1.489501312335958172, -0.3162353388693405765, 0.4822834645669290543 ) ) ;
#26782 = CARTESIAN_POINT ( 'NONE',  ( -1.187664041994750175, -0.05778040916215560624, -0.4822834645669293319 ) ) ;
#26783 = CARTESIAN_POINT ( 'NONE',  ( 0.3543307086614179147, 0.2952755905511811885, 0.000000000000000000 ) ) ;
#26784 = CARTESIAN_POINT ( 'NONE',  ( -1.128608923884513837, 0.2306618581243847221, -0.2411417322834647770 ) ) ;
#26785 = CARTESIAN_POINT ( 'NONE',  ( -0.3917322834645668994, -0.1049643490035306742, -2.645649975556744415 ) ) ;
#26786 = CARTESIAN_POINT ( 'NONE',  ( 0.5118110236220478892, 0.2952755905511811885, 0.000000000000000000 ) ) ;
#26787 = CARTESIAN_POINT ( 'NONE',  ( -0.3917322834645671215, 0.1049643490035301469, -2.072178477690288734 ) ) ;
#26788 = CARTESIAN_POINT ( 'NONE',  ( -0.8858267716535425107, -0.4536011799217367080, 0.2665933059059888421 ) ) ;
#26789 = ORIENTED_EDGE ( 'NONE', *, *, #27779, .T. ) ;
#26790 = CARTESIAN_POINT ( 'NONE',  ( -0.3949938075777409408, -0.1058382717557502933, -1.935695538057742748 ) ) ;
#26791 = EDGE_LOOP ( 'NONE', ( #58372, #8776, #52661, #63335 ) ) ;
#26792 = CARTESIAN_POINT ( 'NONE',  ( -0.6423408027444563739, -2.609869883881465018E-15, -0.3464511005275220379 ) ) ;
#26793 = CARTESIAN_POINT ( 'NONE',  ( -1.259842519685038686, -0.1870078740157479769, 0.4822834645669291653 ) ) ;
#26794 = CARTESIAN_POINT ( 'NONE',  ( -1.115485564304461219, 0.05413385826771626580, -0.4176697321401330321 ) ) ;
#26795 = CARTESIAN_POINT ( 'NONE',  ( 0.3996062992125986035, 2.446882876249141962E-17, -0.4330708661417322913 ) ) ;
#26796 = CARTESIAN_POINT ( 'NONE',  ( -1.423884514435694859, -0.3162353388693405765, 0.4822834645669290543 ) ) ;
#26797 = CARTESIAN_POINT ( 'NONE',  ( -1.213910761154854745, 0.2952755905511810774, -0.1292274648535930714 ) ) ;
#26798 = VECTOR ( 'NONE', #32943, 39.37007874015748143 ) ;
#26799 = CARTESIAN_POINT ( 'NONE',  ( -1.325459317585300889, 0.05413385826771666132, 0.4176697321401328100 ) ) ;
#26800 = CARTESIAN_POINT ( 'NONE',  ( -0.3812812444996365180, -2.294479370626195693E-15, 0.3464511005275217603 ) ) ;
#26801 = CARTESIAN_POINT ( 'NONE',  ( -0.6962418744208963561, -2.294479370626195693E-15, 0.3464511005275217603 ) ) ;
#26802 = CARTESIAN_POINT ( 'NONE',  ( 0.06561679790026316017, -0.3690944881889763329, 0.3153832671262228327 ) ) ;
#26803 = FACE_OUTER_BOUND ( 'NONE', #28891, .T. ) ;
#26804 = CARTESIAN_POINT ( 'NONE',  ( -0.3392501089628019995, 0.1958661417322832277, -0.4258530183727035068 ) ) ;
#26805 = CARTESIAN_POINT ( 'NONE',  ( -0.1706036745406816491, -0.3690944881889763329, 0.3153832671262228327 ) ) ;
#26806 = CARTESIAN_POINT ( 'NONE',  ( -0.9251968503937002541, -0.5400638737290845981, -0.3530559997133363437 ) ) ;
#26807 = CARTESIAN_POINT ( 'NONE',  ( 0.8595800524934390507, -0.05778040916215560624, -0.4822834645669293319 ) ) ;
#26808 = CARTESIAN_POINT ( 'NONE',  ( -0.5643044619422565855, -0.4281496062992124485, 0.4176697321401328655 ) ) ;
#26809 = EDGE_LOOP ( 'NONE', ( #22245, #33131, #76679, #65319, #63125, #61784 ) ) ;
#26810 = ORIENTED_EDGE ( 'NONE', *, *, #56687, .T. ) ;
#26811 = CARTESIAN_POINT ( 'NONE',  ( 0.1998031496062994128, -0.3460692066303957537, -1.900918635170603554 ) ) ;
#26812 = CARTESIAN_POINT ( 'NONE',  ( -0.7677165354330699465, -0.5400638737290845981, -0.3530559997133363437 ) ) ;
#26813 = CARTESIAN_POINT ( 'NONE',  ( 1.062992125984252745, -0.6692913385826771977, 8.415575281601705876E-17 ) ) ;
#26814 = FACE_OUTER_BOUND ( 'NONE', #82794, .T. ) ;
#26815 = CARTESIAN_POINT ( 'NONE',  ( -0.08317555404016972742, 1.066210426301412717, 0.2524679153701900325 ) ) ;
#26816 = CARTESIAN_POINT ( 'NONE',  ( 0.1265901696524989462, 0.4724409448818897572, -1.410761154855643129 ) ) ;
#26817 = CARTESIAN_POINT ( 'NONE',  ( -0.4744094488189106174, 1.537401574803149984, 3.908320185825790105 ) ) ;
#26818 = CARTESIAN_POINT ( 'NONE',  ( -9.594673741351313045E-17, 0.3917322834645670104, -0.1496062992125983815 ) ) ;
#26819 = CARTESIAN_POINT ( 'NONE',  ( -0.3392501089628019995, 0.1958661417322832277, -2.630577427821522374 ) ) ;
#26820 = CARTESIAN_POINT ( 'NONE',  ( -0.4593175853018364174, -0.4281496062992127816, -0.4176697321401328100 ) ) ;
#26821 = CARTESIAN_POINT ( 'NONE',  ( -1.561679790026246017, -0.3690944881889765550, -0.3153832671262227771 ) ) ;
#26822 = CARTESIAN_POINT ( 'NONE',  ( -0.8267716535433065062, -0.6692913385826771977, 8.415575281601705876E-17 ) ) ;
#26823 = CARTESIAN_POINT ( 'NONE',  ( 4.893765752498283308E-17, -0.3996062992125985480, -0.1555118110236220763 ) ) ;
#26825 = DIRECTION ( 'NONE',  ( -3.096699300667737957E-16, 1.000000000000000000, -0.000000000000000000 ) ) ;
#26824 = CARTESIAN_POINT ( 'NONE',  ( -1.318897637795274802, -0.5400638737290845981, -0.3530559997133363437 ) ) ;
#26826 = CARTESIAN_POINT ( 'NONE',  ( -0.7939632545931754048, -0.3162353388693405765, 0.4822834645669290543 ) ) ;
#26827 = CARTESIAN_POINT ( 'NONE',  ( -0.2099737532808391705, -0.6046776061558809534, -0.2411417322834644161 ) ) ;
#26828 = CARTESIAN_POINT ( 'NONE',  ( -0.1058382717557497660, -0.3949938075777411073, -2.826115485564304475 ) ) ;
#26829 = CARTESIAN_POINT ( 'NONE',  ( 0.8070866141732288002, 0.07958543189024085140, 0.2665933059059887866 ) ) ;
#26830 = CARTESIAN_POINT ( 'NONE',  ( 0.3917322834645669549, 0.1049643490035304660, -0.2093175853018373889 ) ) ;
#26831 = CARTESIAN_POINT ( 'NONE',  ( 0.2099737532808405305, -0.5023911411419708095, 0.1820866141732285504 ) ) ;
#26832 = CARTESIAN_POINT ( 'NONE',  ( 1.522309711286089939, -0.5023911411419708095, -0.1820866141732282451 ) ) ;
#26833 = CARTESIAN_POINT ( 'NONE',  ( 1.561679790026247350, -0.4281496062992124485, 0.4176697321401328655 ) ) ;
#26834 = CARTESIAN_POINT ( 'NONE',  ( -0.01312335958005186876, -0.004921259842519870586, -0.3153832671262229437 ) ) ;
#26835 = CARTESIAN_POINT ( 'NONE',  ( -0.3917322834645669549, -0.1049643490035306603, -1.927821522309711044 ) ) ;
#26836 = CARTESIAN_POINT ( 'NONE',  ( -1.194225721784776262, -0.4281496062992124485, 0.4176697321401328655 ) ) ;
#26837 = CARTESIAN_POINT ( 'NONE',  ( 1.161417322834646271, 0.1660481256975883668, -0.3530559997133364547 ) ) ;
#26838 = CARTESIAN_POINT ( 'NONE',  ( -0.1265901696524993347, 0.4724409448818895907, 0.07414698162729659037 ) ) ;
#26839 = CARTESIAN_POINT ( 'NONE',  ( -0.3674540682414689785, 0.1283753931104748280, 0.1820866141732283561 ) ) ;
#26840 = CARTESIAN_POINT ( 'NONE',  ( 0.3871391076115493490, -0.3162353388693405765, 0.4822834645669290543 ) ) ;
#26841 = CARTESIAN_POINT ( 'NONE',  ( -1.016821367227983552, 1.537401574803149984, -0.4744094488188975722 ) ) ;
#26842 = CARTESIAN_POINT ( 'NONE',  ( 1.062992125984252745, -0.5511811023622047445, 6.969142054262312111E-17 ) ) ;
#26843 = CARTESIAN_POINT ( 'NONE',  ( 0.2493438320209980519, -0.3690944881889765550, -0.3153832671262227771 ) ) ;
#26844 = CARTESIAN_POINT ( 'NONE',  ( -0.3412073490813641308, 0.2306618581243847221, -0.2411417322834647770 ) ) ;
#26845 = CARTESIAN_POINT ( 'NONE',  ( 0.3149606299212737159, 2.165354330708661568, -3.937007874015761022 ) ) ;
#26846 = CARTESIAN_POINT ( 'NONE',  ( -0.8989501312335946848, -0.5511811023622046335, 0.09757992244046803654 ) ) ;
#26847 = FACE_OUTER_BOUND ( 'NONE', #9577, .T. ) ;
#26848 = ADVANCED_FACE ( 'NONE', ( #27543 ), #9029, .F. ) ;
#26849 = CARTESIAN_POINT ( 'NONE',  ( 0.5905511811023629321, 0.2952755905511811885, 0.000000000000000000 ) ) ;
#26850 = CARTESIAN_POINT ( 'NONE',  ( -1.069553805774277722, -0.6692913385826773087, -0.1292274648535924053 ) ) ;
#26851 = CARTESIAN_POINT ( 'NONE',  ( 0.1070741851644054776, -0.3996062992125984925, -1.264435695538057569 ) ) ;
#26852 = CARTESIAN_POINT ( 'NONE',  ( 0.1049643490035304938, -0.3917322834645669549, -2.847112860892388131 ) ) ;
#26853 = CARTESIAN_POINT ( 'NONE',  ( 0.1509186351706042484, -0.2845877964562159024, 0.3641732283464567677 ) ) ;
#26854 = CARTESIAN_POINT ( 'NONE',  ( -0.8333333333333323711, 0.2952755905511811885, 0.1292274648535926551 ) ) ;
#26855 = CARTESIAN_POINT ( 'NONE',  ( -1.023622047244093558, -0.1870078740157479769, 0.4822834645669291653 ) ) ;
#26856 = CARTESIAN_POINT ( 'NONE',  ( -1.332020997375327642, -0.08942795157527998196, 0.3641732283464567121 ) ) ;
#26857 = CARTESIAN_POINT ( 'NONE',  ( 1.679790026246720025, 0.2306618581243848609, 0.2411417322834645549 ) ) ;
#26858 = CARTESIAN_POINT ( 'NONE',  ( -0.7939632545931750718, -0.08942795157528024563, -0.3641732283464568787 ) ) ;
#26859 = CARTESIAN_POINT ( 'NONE',  ( -1.586052503253846169, 1.850393700787402729, 0.1653254495020583248 ) ) ;
#26860 = CARTESIAN_POINT ( 'NONE',  ( 1.122047244094488860, 0.1660481256975885056, 0.3530559997133364547 ) ) ;
#26861 = CARTESIAN_POINT ( 'NONE',  ( -0.3460692066303960868, 0.1998031496062990242, -0.1837270341207349056 ) ) ;
#26862 = CARTESIAN_POINT ( 'NONE',  ( 0.1958661417322834775, 0.3392501089628018884, -2.503300155676852157 ) ) ;
#26863 = ORIENTED_EDGE ( 'NONE', *, *, #53218, .T. ) ;
#26864 = CARTESIAN_POINT ( 'NONE',  ( 0.000000000000000000, 0.000000000000000000, 0.000000000000000000 ) ) ;
#26865 = CARTESIAN_POINT ( 'NONE',  ( -1.581364829396324945, -0.3162353388693405765, 0.4822834645669290543 ) ) ;
#26866 = CARTESIAN_POINT ( 'NONE',  ( -1.397637795275589623, 0.1660481256975885056, 0.3530559997133364547 ) ) ;
#26867 = CARTESIAN_POINT ( 'NONE',  ( 1.358267716535433323, -0.5400638737290845981, -0.3530559997133363437 ) ) ;
#26868 = CARTESIAN_POINT ( 'NONE',  ( 4.797336870675656522E-17, -0.3917322834645670104, -2.368110236220472675 ) ) ;
#26869 = DIRECTION ( 'NONE',  ( 0.000000000000000000, 1.000000000000000000, 0.000000000000000000 ) ) ;
#26870 = ADVANCED_FACE ( 'NONE', ( #34702 ), #80165, .T. ) ;
#26871 = CARTESIAN_POINT ( 'NONE',  ( 0.5577427821522316087, -0.05778040916215522460, 0.4822834645669289988 ) ) ;
#26872 = CARTESIAN_POINT ( 'NONE',  ( -0.4265091863517051496, -0.6692913385826771977, 0.1292274648535927661 ) ) ;
#26873 = CARTESIAN_POINT ( 'NONE',  ( 0.4713254705329260053, 1.475163719089159997, -3.908698025846080171 ) ) ;
#26874 = CARTESIAN_POINT ( 'NONE',  ( 0.7974104941589355011, -4.927456884911482678E-16, 0.4445507791589062840 ) ) ;
#26875 = CARTESIAN_POINT ( 'NONE',  ( 0.9645669291338588858, 0.07958543189024085140, 0.2665933059059887866 ) ) ;
#26876 = CARTESIAN_POINT ( 'NONE',  ( -0.2925321140481930704, -0.2925321140481933480, -1.476377952755905554 ) ) ;
#26877 = ORIENTED_EDGE ( 'NONE', *, *, #22300, .T. ) ;
#26878 = CARTESIAN_POINT ( 'NONE',  ( -9.594673741351313045E-17, 0.3917322834645670659, -0.1542187908474559610 ) ) ;
#26879 = ORIENTED_EDGE ( 'NONE', *, *, #57231, .T. ) ;
#26880 = CARTESIAN_POINT ( 'NONE',  ( 0.03280839895013198948, 0.2952755905511811885, 0.1292274648535926551 ) ) ;
#26881 = CARTESIAN_POINT ( 'NONE',  ( 1.450131233595801428, 0.2952755905511811885, 0.1292274648535926551 ) ) ;
#26882 = CARTESIAN_POINT ( 'NONE',  ( 0.3871391076115493490, -0.3162353388693405765, 0.4822834645669290543 ) ) ;
#26883 = CARTESIAN_POINT ( 'NONE',  ( 1.240157480314961314, 0.1660481256975883668, -0.3530559997133364547 ) ) ;
#26884 = CARTESIAN_POINT ( 'NONE',  ( -0.4724409448818890911, -0.1870078740157480879, -0.4822834645669291653 ) ) ;
#26885 = CARTESIAN_POINT ( 'NONE',  ( -0.1115485564304456306, 0.2952755905511810774, -0.1292274648535930714 ) ) ;
#26886 = CARTESIAN_POINT ( 'NONE',  ( -1.568241469816272105, -0.3162353388693409650, -0.4822834645669289433 ) ) ;
#26888 = ADVANCED_FACE ( 'NONE', ( #65862 ), #14529, .F. ) ;
#26887 = CARTESIAN_POINT ( 'NONE',  ( 1.187664041994751285, -0.3162353388693409650, -0.4822834645669289433 ) ) ;
#26889 = CARTESIAN_POINT ( 'NONE',  ( 1.358267716535433323, 0.1660481256975885056, 0.3530559997133364547 ) ) ;
#26890 = CARTESIAN_POINT ( 'NONE',  ( 0.1049643490035303689, 0.3917322834645670104, -0.6154855643044617741 ) ) ;
#26891 = CARTESIAN_POINT ( 'NONE',  ( 0.5249343832021005074, -0.5023911411419708095, 0.1820866141732285504 ) ) ;
#26892 = ORIENTED_EDGE ( 'NONE', *, *, #56817, .T. ) ;
#26893 = CARTESIAN_POINT ( 'NONE',  ( 0.1058382717557499880, 0.3949938075777411073, -0.7808398950131234528 ) ) ;
#26894 = ORIENTED_EDGE ( 'NONE', *, *, #38729, .F. ) ;
#26895 = CARTESIAN_POINT ( 'NONE',  ( -0.5511811023622041894, -0.1870078740157480601, -0.3641732283464567677 ) ) ;
#26896 = CARTESIAN_POINT ( 'NONE',  ( 0.05249343832021075018, -0.6046776061558807314, 0.2411417322834647770 ) ) ;
#26897 = CARTESIAN_POINT ( 'NONE',  ( 2.723802780027873016, 1.230840736494986709, 0.3632157284009329135 ) ) ;
#26898 = CARTESIAN_POINT ( 'NONE',  ( 0.1115485564304467270, -0.6692913385826773087, -0.1292274648535924053 ) ) ;
#26899 = CARTESIAN_POINT ( 'NONE',  ( 0.1837270341207354329, 0.2306618581243848609, 0.2411417322834645549 ) ) ;
#26900 = CARTESIAN_POINT ( 'NONE',  ( -0.8202099737532799750, 0.2952755905511810774, -0.1292274648535930714 ) ) ;
#26901 = CARTESIAN_POINT ( 'NONE',  ( -0.8923884514435688198, 0.2306618581243847221, -0.2411417322834647770 ) ) ;
#26902 = CARTESIAN_POINT ( 'NONE',  ( 1.430446194225722500, -0.3690944881889765550, -0.3153832671262227771 ) ) ;
#26903 = CARTESIAN_POINT ( 'NONE',  ( -1.489501312335957062, -0.05778040916215522460, 0.4822834645669289988 ) ) ;
#26904 = CARTESIAN_POINT ( 'NONE',  ( 1.348312163386739426, 0.2755905511811023723, 0.7386866130305692613 ) ) ;
#26905 = CARTESIAN_POINT ( 'NONE',  ( 0.9383202099737536495, -0.2845877964562159024, 0.3641732283464567677 ) ) ;
#26906 = CARTESIAN_POINT ( 'NONE',  ( 0.3543307086614181922, -0.6692913385826771977, 8.415575281601705876E-17 ) ) ;
#26907 = CARTESIAN_POINT ( 'NONE',  ( 0.6299212598425204535, -0.1870078740157480879, -0.4822834645669291653 ) ) ;
#26908 = CARTESIAN_POINT ( 'NONE',  ( -0.2925321140481932924, 0.2925321140481931814, -1.279527559055118058 ) ) ;
#26909 = CARTESIAN_POINT ( 'NONE',  ( -0.3149606299212558413, 2.165354330708661568, -1.076935383196058860 ) ) ;
#26910 = CARTESIAN_POINT ( 'NONE',  ( 0.2925321140481932369, -0.2925321140481931814, -0.8051181102362205966 ) ) ;
#26911 = CARTESIAN_POINT ( 'NONE',  ( -0.3460692066303957537, -0.1998031496062994405, -0.1292650918635170898 ) ) ;
#26912 = CARTESIAN_POINT ( 'NONE',  ( -0.5511811023622041894, -0.1870078740157480879, -0.4822834645669291653 ) ) ;
#26913 = CARTESIAN_POINT ( 'NONE',  ( -9.787531504996567848E-17, 0.3996062992125986035, -2.834645669291338432 ) ) ;
#26914 = CARTESIAN_POINT ( 'NONE',  ( 0.2867679344610365999, -0.2867679344610365444, -2.072834645669291209 ) ) ;
#26915 = CARTESIAN_POINT ( 'NONE',  ( -1.253280839895012377, -0.2845877964562161244, -0.3641732283464567121 ) ) ;
#26916 = CARTESIAN_POINT ( 'NONE',  ( 1.207349081364829990, -0.6046776061558809534, -0.2411417322834644161 ) ) ;
#26917 = CARTESIAN_POINT ( 'NONE',  ( 1.089238845144357759, 0.05413385826771626580, -0.4176697321401330321 ) ) ;
#26918 = CARTESIAN_POINT ( 'NONE',  ( -0.05905511811023545637, 0.07958543189024085140, 0.2665933059059887866 ) ) ;
#26919 = CARTESIAN_POINT ( 'NONE',  ( 0.6889763779527563470, 0.1660481256975883668, -0.3530559997133364547 ) ) ;
#26920 = CARTESIAN_POINT ( 'NONE',  ( -0.1265901696524986964, -0.4724409448818899238, -2.038713910761154491 ) ) ;
#26921 = CARTESIAN_POINT ( 'NONE',  ( -0.1509186351706028884, -0.2845877964562161244, -0.3641732283464567121 ) ) ;
#26922 = CARTESIAN_POINT ( 'NONE',  ( -0.2165354330708654795, -0.5400638737290845981, -0.3530559997133363437 ) ) ;
#26924 = CIRCLE ( 'NONE', #22898, 1.220472440944881942 ) ;
#26923 = CARTESIAN_POINT ( 'NONE',  ( -0.3949938075777411073, 0.1058382717557497660, -1.369422572178477848 ) ) ;
#26925 = CARTESIAN_POINT ( 'NONE',  ( -1.220472440944881054, 0.2952755905511811885, 0.000000000000000000 ) ) ;
#26926 = CARTESIAN_POINT ( 'NONE',  ( 0.6824146981627303710, 0.1283753931104746893, -0.1820866141732285504 ) ) ;
#26927 = CARTESIAN_POINT ( 'NONE',  ( 0.5027385518334777093, 1.496062992125983815, -0.5309055118110237448 ) ) ;
#26928 = CARTESIAN_POINT ( 'NONE',  ( -0.8398950131233589023, -0.6046776061558809534, -0.2411417322834644161 ) ) ;
#26929 = CARTESIAN_POINT ( 'NONE',  ( -0.2165354330708654795, 0.07958543189024085140, 0.2665933059059887866 ) ) ;
#26930 = PLANE ( 'NONE',  #56068 ) ;
#26931 = CARTESIAN_POINT ( 'NONE',  ( -0.7086614173228339419, -0.1870078740157480879, -0.4822834645669291653 ) ) ;
#26932 = CARTESIAN_POINT ( 'NONE',  ( -0.5052493438320203589, 0.2952755905511810774, -0.1292274648535930714 ) ) ;
#26933 = CARTESIAN_POINT ( 'NONE',  ( 0.1902887139107617975, -0.6692913385826773087, -0.1292274648535924053 ) ) ;
#26934 = CARTESIAN_POINT ( 'NONE',  ( 4.893765752498283308E-17, -0.3996062992125985480, -2.360236220472441193 ) ) ;
#26935 = CARTESIAN_POINT ( 'NONE',  ( -0.1958661417322834497, -0.3392501089628018884, -2.192894070044932420 ) ) ;
#26936 = CARTESIAN_POINT ( 'NONE',  ( -1.548556430446193399, 0.1283753931104748280, 0.1820866141732283561 ) ) ;
#26937 = CARTESIAN_POINT ( 'NONE',  ( 0.6561679790026253567, -0.5023911411419708095, -0.1820866141732282451 ) ) ;
#26938 = CARTESIAN_POINT ( 'NONE',  ( 1.391076115485564868, -0.6046776061558807314, 0.2411417322834647770 ) ) ;
#26939 = CARTESIAN_POINT ( 'NONE',  ( -0.7086614173228339419, -0.1870078740157480601, -0.3641732283464567677 ) ) ;
#26940 = CARTESIAN_POINT ( 'NONE',  ( -1.030183727034119867, -0.08942795157528024563, -0.3641732283464568787 ) ) ;
#26941 = B_SPLINE_CURVE_WITH_KNOTS ( 'NONE', 3,
 ( #83022, #7683, #19039, #78390 ),
 .UNSPECIFIED., .F., .F.,
 ( 4, 4 ),
 ( 2.857347768990396770E-07, 0.001436604392377179105 ),
 .UNSPECIFIED. ) ;
#26942 = CARTESIAN_POINT ( 'NONE',  ( -0.7611548556430438595, -0.6046776061558809534, -0.2411417322834644161 ) ) ;
#26943 = CARTESIAN_POINT ( 'NONE',  ( -0.1181102362204717315, 0.2952755905511811885, 0.000000000000000000 ) ) ;
#26944 = CARTESIAN_POINT ( 'NONE',  ( 0.7414698162729663755, 0.1771653543307087630, 0.09757992244046791164 ) ) ;
#26945 = CARTESIAN_POINT ( 'NONE',  ( -0.2950900605411925781, 0.01202116872835609987, 5.525111687089956369 ) ) ;
#26946 = CARTESIAN_POINT ( 'NONE',  ( 1.089238845144357537, -0.3690944881889763329, 0.3153832671262228327 ) ) ;
#26947 = CARTESIAN_POINT ( 'NONE',  ( 0.2952755905511819101, 0.1660481256975883668, -0.3530559997133364547 ) ) ;
#26948 = CARTESIAN_POINT ( 'NONE',  ( 0.1998031496062992463, 0.3460692066303959202, -0.06364829396325459576 ) ) ;
#26949 = CARTESIAN_POINT ( 'NONE',  ( -0.8464566929133852113, -0.5400638737290845981, -0.3530559997133363437 ) ) ;
#26950 = CARTESIAN_POINT ( 'NONE',  ( -0.1958661417322834220, -0.3392501089628018884, -1.252624671916010568 ) ) ;
#26951 = CARTESIAN_POINT ( 'NONE',  ( 1.332020997375328974, -0.08942795157528024563, -0.3641732283464568787 ) ) ;
#26952 = CARTESIAN_POINT ( 'NONE',  ( 0.5511811023622055217, -0.1870078740157479769, 0.4822834645669291653 ) ) ;
#26953 = CARTESIAN_POINT ( 'NONE',  ( 0.3149606299212606708, -0.1870078740157480879, -0.4822834645669291653 ) ) ;
#26954 = CARTESIAN_POINT ( 'NONE',  ( 0.04593175853018440641, -0.5511811023622046335, 0.09757992244046803654 ) ) ;
#26955 = LINE ( 'NONE', #52618, #70980 ) ;
#26956 = CARTESIAN_POINT ( 'NONE',  ( -0.1246719160104980823, -0.5511811023622048555, -0.09757992244046775898 ) ) ;
#26957 = CARTESIAN_POINT ( 'NONE',  ( 0.8005249343832028242, -0.4281496062992127816, -0.4176697321401328100 ) ) ;
#26958 = CARTESIAN_POINT ( 'NONE',  ( -0.7808398950131225646, -0.08942795157527998196, 0.3641732283464567121 ) ) ;
#26959 = CARTESIAN_POINT ( 'NONE',  ( -0.6430446194225712953, 0.05413385826771626580, -0.4176697321401330321 ) ) ;
#26960 = CARTESIAN_POINT ( 'NONE',  ( 0.2362204724409449064, 0.000000000000000000, 0.000000000000000000 ) ) ;
#26961 = EDGE_LOOP ( 'NONE', ( #16360, #81777, #39740, #46559 ) ) ;
#26962 = CARTESIAN_POINT ( 'NONE',  ( -1.043307086614172041, -0.5400638737290844871, 0.3530559997133364547 ) ) ;
#26963 = CARTESIAN_POINT ( 'NONE',  ( -1.305774278215222184, -0.5511811023622048555, -0.09757992244046775898 ) ) ;
#26964 = CARTESIAN_POINT ( 'NONE',  ( -0.1049868766404193215, 0.2306618581243847221, -0.2411417322834647770 ) ) ;
#26965 = CARTESIAN_POINT ( 'NONE',  ( -1.535433070866141225, 0.2952755905511811885, 0.000000000000000000 ) ) ;
#26966 = CARTESIAN_POINT ( 'NONE',  ( -0.8070866141732276899, 0.1660481256975883668, -0.3530559997133364547 ) ) ;
#26967 = CARTESIAN_POINT ( 'NONE',  ( 0.4603218807116906675, 1.653261878685373665, -2.138334326189375023 ) ) ;
#26969 = CARTESIAN_POINT ( 'NONE',  ( 1.115485564304462551, 0.05413385826771666132, 0.4176697321401328100 ) ) ;
#26968 = CARTESIAN_POINT ( 'NONE',  ( 1.036745406824147731, 0.05413385826771666132, 0.4176697321401328100 ) ) ;
#26970 = CARTESIAN_POINT ( 'NONE',  ( 1.286089238845145033, -0.6046776061558809534, -0.2411417322834644161 ) ) ;
#26971 = CARTESIAN_POINT ( 'NONE',  ( -0.2867679344610366554, 0.2867679344610365444, -2.531496062992125484 ) ) ;
#26972 = CARTESIAN_POINT ( 'NONE',  ( 3.937007874015748143, 2.165354330708661568, 0.3149606299212600047 ) ) ;
#26973 = CARTESIAN_POINT ( 'NONE',  ( -1.292650918635170010, -0.6692913385826771977, 0.1292274648535927661 ) ) ;
#26974 = CARTESIAN_POINT ( 'NONE',  ( 0.4091458600556403535, 0.2362204724409449896, -0.7611548556430446366 ) ) ;
#26975 = CARTESIAN_POINT ( 'NONE',  ( -0.1998031496062991907, -0.3460692066303959757, -0.2230971128608923992 ) ) ;
#26976 = ORIENTED_EDGE ( 'NONE', *, *, #22300, .F. ) ;
#26977 = CARTESIAN_POINT ( 'NONE',  ( -0.2755905511811015396, -0.5511811023622047445, 6.969142054262312111E-17 ) ) ;
#26978 = CARTESIAN_POINT ( 'NONE',  ( -0.3392501089628019995, 0.1958661417322832277, -1.750656167979002698 ) ) ;
#26979 = VERTEX_POINT ( 'NONE', #15126 ) ;
#26980 = CARTESIAN_POINT ( 'NONE',  ( 0.3215223097112867578, -0.05778040916215522460, 0.4822834645669289988 ) ) ;
#26981 = CARTESIAN_POINT ( 'NONE',  ( 0.1509186351706042484, -0.3162353388693405765, 0.4822834645669290543 ) ) ;
#26982 = CARTESIAN_POINT ( 'NONE',  ( -0.6692913385826764205, 0.2952755905511811885, 0.000000000000000000 ) ) ;
#26983 = CARTESIAN_POINT ( 'NONE',  ( 1.348312163386739426, 0.2755905511811023723, 0.7386866130305692613 ) ) ;
#26984 = CARTESIAN_POINT ( 'NONE',  ( -0.9711286089238838626, 0.1283753931104746893, -0.1820866141732285504 ) ) ;
#26985 = CARTESIAN_POINT ( 'NONE',  ( 0.3477690288713918276, 0.2952755905511811885, 0.1292274648535926551 ) ) ;
#26986 = CARTESIAN_POINT ( 'NONE',  ( 0.7086614173228353852, -0.1870078740157479769, 0.4822834645669291653 ) ) ;
#26987 = CARTESIAN_POINT ( 'NONE',  ( 0.4461942257217855201, -0.5023911411419708095, 0.1820866141732285504 ) ) ;
#26988 = CIRCLE ( 'NONE', #67326, 2.362204724409449064 ) ;
#26989 = CARTESIAN_POINT ( 'NONE',  ( -0.2493438320209966919, -0.4281496062992124485, 0.4176697321401328655 ) ) ;
#26990 = CARTESIAN_POINT ( 'NONE',  ( -0.1049643490035301746, -0.3917322834645670659, -1.254573860071179103 ) ) ;
#26991 = CARTESIAN_POINT ( 'NONE',  ( -0.7677165354330699465, -0.5400638737290845981, -0.3530559997133363437 ) ) ;
#26992 = CARTESIAN_POINT ( 'NONE',  ( 0.000000000000000000, 2.755905511811024056, 0.000000000000000000 ) ) ;
#26993 = CARTESIAN_POINT ( 'NONE',  ( 1.240157480314961314, 0.1660481256975883668, -0.3530559997133364547 ) ) ;
#26994 = CARTESIAN_POINT ( 'NONE',  ( 1.686351706036745890, 0.1771653543307087630, 0.09757992244046791164 ) ) ;
#26995 = ORIENTED_EDGE ( 'NONE', *, *, #65114, .T. ) ;
#26996 = CARTESIAN_POINT ( 'NONE',  ( 0.1958661417322834775, 0.3392501089628018884, -2.660780470637482242 ) ) ;
#26997 = CARTESIAN_POINT ( 'NONE',  ( -0.02624671916010428221, 0.2306618581243847221, -0.2411417322834647770 ) ) ;
#26998 = ORIENTED_EDGE ( 'NONE', *, *, #62552, .T. ) ;
#26999 = CARTESIAN_POINT ( 'NONE',  ( -1.325459317585300889, -0.4281496062992127816, -0.4176697321401328100 ) ) ;
#27000 = CARTESIAN_POINT ( 'NONE',  ( 1.292650918635171564, 0.2952755905511811885, 0.1292274648535926551 ) ) ;
#27001 = CARTESIAN_POINT ( 'NONE',  ( 1.318897637795276356, 0.1660481256975883668, -0.3530559997133364547 ) ) ;
#27002 = ADVANCED_FACE ( 'NONE', ( #66053 ), #26492, .T. ) ;
#27003 = CARTESIAN_POINT ( 'NONE',  ( 0.3871391076115492380, -0.05778040916215560624, -0.4822834645669293319 ) ) ;
#27004 = CARTESIAN_POINT ( 'NONE',  ( -0.2362204724409440182, -0.1870078740157479769, 0.4822834645669291653 ) ) ;
#27005 = CARTESIAN_POINT ( 'NONE',  ( -9.594673741351313045E-17, 0.3917322834645670104, -1.816929133858267820 ) ) ;
#27006 = CARTESIAN_POINT ( 'NONE',  ( -1.246719160104986512, 0.05413385826771666132, 0.4176697321401328100 ) ) ;
#27007 = CARTESIAN_POINT ( 'NONE',  ( -0.7217847769028863381, -0.4281496062992124485, 0.4176697321401328655 ) ) ;
#27008 = ADVANCED_FACE ( 'NONE', ( #1662 ), #27319, .T. ) ;
#27009 = CARTESIAN_POINT ( 'NONE',  ( 0.05905511811023709395, -0.4536011799217367080, 0.2665933059059888421 ) ) ;
#27010 = STYLED_ITEM ( 'NONE', ( #37517 ), #6682 ) ;
#27011 = CARTESIAN_POINT ( 'NONE',  ( -0.6299212598425188991, -0.1870078740157479769, 0.4822834645669291653 ) ) ;
#27012 = CARTESIAN_POINT ( 'NONE',  ( -1.220472440944881054, 0.2952755905511811885, 0.000000000000000000 ) ) ;
#27013 = CARTESIAN_POINT ( 'NONE',  ( 0.7086614173228352742, -0.1870078740157480879, -0.4822834645669291653 ) ) ;
#27014 = CARTESIAN_POINT ( 'NONE',  ( 3.916325068365210438, 1.286797242935906471, -0.4031187015191872725 ) ) ;
#27015 = ORIENTED_EDGE ( 'NONE', *, *, #13664, .F. ) ;
#27016 = CARTESIAN_POINT ( 'NONE',  ( -0.1312335958005241554, -0.6046776061558809534, -0.2411417322834644161 ) ) ;
#27017 = CARTESIAN_POINT ( 'NONE',  ( -0.3149606299212590610, -0.1870078740157479769, 0.3641732283464567677 ) ) ;
#27019 = DIRECTION ( 'NONE',  ( -1.000000000000000000, 0.000000000000000000, 0.000000000000000000 ) ) ;
#27018 = CARTESIAN_POINT ( 'NONE',  ( 1.187664041994751285, -0.08942795157527998196, 0.3641732283464567121 ) ) ;
#27020 = CARTESIAN_POINT ( 'NONE',  ( -0.4724409448818899238, 0.1265901696524986686, -0.2670603674540683037 ) ) ;
#27021 = CARTESIAN_POINT ( 'NONE',  ( 1.581364829396326277, -0.2845877964562161244, -0.3641732283464567121 ) ) ;
#27022 = CARTESIAN_POINT ( 'NONE',  ( 1.272965879265092637, 0.05413385826771666132, 0.4176697321401328100 ) ) ;
#27023 = CARTESIAN_POINT ( 'NONE',  ( 0.3949938075777409963, 2.418639510665530743E-17, -0.1948818897637795700 ) ) ;
#27024 = CARTESIAN_POINT ( 'NONE',  ( 0.1574803149606306130, -0.1870078740157479769, 0.4822834645669291653 ) ) ;
#27025 = CARTESIAN_POINT ( 'NONE',  ( -1.496062992125983815, -0.1870078740157479769, 0.4822834645669291653 ) ) ;
#27026 = CARTESIAN_POINT ( 'NONE',  ( -1.476377952755905110, -0.5400638737290845981, -0.3530559997133363437 ) ) ;
#27027 = CARTESIAN_POINT ( 'NONE',  ( -0.02624671916010428221, -0.6046776061558807314, 0.2411417322834647770 ) ) ;
#27028 = CARTESIAN_POINT ( 'NONE',  ( 0.1058382717557499880, 0.3949938075777409408, -0.2276902887139107823 ) ) ;
#27029 = CARTESIAN_POINT ( 'NONE',  ( 1.594488188976378673, -0.5400638737290845981, -0.3530559997133363437 ) ) ;
#27030 = CARTESIAN_POINT ( 'NONE',  ( 0.5118110236220478892, 0.2952755905511811885, 0.000000000000000000 ) ) ;
#27031 = CARTESIAN_POINT ( 'NONE',  ( 1.115485564304462551, -0.3690944881889765550, -0.3153832671262227771 ) ) ;
#27032 = CARTESIAN_POINT ( 'NONE',  ( 0.3129921259842522452, 1.470238543415450350, 1.333910153156375395E-19 ) ) ;
#27033 = CARTESIAN_POINT ( 'NONE',  ( 0.2034120734908144990, -0.5511811023622046335, 0.09757992244046803654 ) ) ;
#27034 = CARTESIAN_POINT ( 'NONE',  ( -1.154855643044618851, 0.2306618581243848609, 0.2411417322834645549 ) ) ;
#27035 = EDGE_CURVE ( 'NONE', #11962, #11380, #50135, .T. ) ;
#27036 = CARTESIAN_POINT ( 'NONE',  ( -9.787531504996566615E-17, 0.3996062992125985480, -1.021653543307086576 ) ) ;
#27037 = CARTESIAN_POINT ( 'NONE',  ( 1.318897637795276356, -0.5400638737290844871, 0.3530559997133364547 ) ) ;
#27038 = CARTESIAN_POINT ( 'NONE',  ( 0.3917322834645669549, 0.1049643490035304660, -0.5892388451443569819 ) ) ;
#27040 = CARTESIAN_POINT ( 'NONE',  ( 0.8777275986338668456, 0.02791078216816225699, 0.4328096321851905293 ) ) ;
#27039 = CARTESIAN_POINT ( 'NONE',  ( 0.9383202099737538715, -0.05778040916215560624, -0.4822834645669293319 ) ) ;
#27041 = DIRECTION ( 'NONE',  ( -0.000000000000000000, -1.000000000000000000, -0.000000000000000000 ) ) ;
#27042 = CARTESIAN_POINT ( 'NONE',  ( 0.4724409448818904789, -0.1870078740157479769, 0.3641732283464567677 ) ) ;
#27043 = EDGE_CURVE ( 'NONE', #43326, #29291, #78692, .T. ) ;
#27044 = CARTESIAN_POINT ( 'NONE',  ( 0.5183727034120741983, -0.6692913385826771977, 0.1292274648535927661 ) ) ;
#27045 = CARTESIAN_POINT ( 'NONE',  ( 0.7545931758530189937, 0.2066929133858267098, -0.1054918080437494132 ) ) ;
#27046 = CARTESIAN_POINT ( 'NONE',  ( -0.8070866141732276899, -0.4536011799217367080, 0.2665933059059888421 ) ) ;
#27047 = CARTESIAN_POINT ( 'NONE',  ( -1.128608923884513837, -0.6046776061558807314, 0.2411417322834647770 ) ) ;
#27048 = CARTESIAN_POINT ( 'NONE',  ( -1.555118110236219930, 0.1660481256975885056, 0.3530559997133364547 ) ) ;
#27049 =( GEOMETRIC_REPRESENTATION_CONTEXT ( 3 ) GLOBAL_UNCERTAINTY_ASSIGNED_CONTEXT ( ( #22601 ) ) GLOBAL_UNIT_ASSIGNED_CONTEXT ( ( #12933, #45728, #25957 ) ) REPRESENTATION_CONTEXT ( 'NONE', 'WORKASPACE' ) );
#27050 = CARTESIAN_POINT ( 'NONE',  ( 0.8136482939632553313, -0.6046776061558809534, -0.2411417322834644161 ) ) ;
#27051 = CARTESIAN_POINT ( 'NONE',  ( -1.587926509186350810, -0.004921259842519870586, -0.3153832671262229437 ) ) ;
#27052 = EDGE_CURVE ( 'NONE', #37547, #23879, #46255, .T. ) ;
#27053 = CARTESIAN_POINT ( 'NONE',  ( 1.074005671585215538, 1.191469999471042041, -0.3250085130549520973 ) ) ;
#27054 = CARTESIAN_POINT ( 'NONE',  ( 0.5839895013123367340, -0.6692913385826773087, -0.1292274648535924053 ) ) ;
#27055 = CARTESIAN_POINT ( 'NONE',  ( 5.785732909357575061E-17, -0.4724409448818898682, -2.675196850393700920 ) ) ;
#27056 = DIRECTION ( 'NONE',  ( 0.000000000000000000, 0.000000000000000000, -1.000000000000000000 ) ) ;
#27057 = CARTESIAN_POINT ( 'NONE',  ( 1.587926509186352586, -0.4281496062992127816, -0.4176697321401328100 ) ) ;
#27058 = CARTESIAN_POINT ( 'NONE',  ( -1.496062992125983815, -0.1870078740157480601, -0.3641732283464567677 ) ) ;
#27059 = CARTESIAN_POINT ( 'NONE',  ( 1.141732283464567788, -0.5511811023622047445, 6.969142054262312111E-17 ) ) ;
#27060 = CARTESIAN_POINT ( 'NONE',  ( -1.253280839895012377, -0.2845877964562161244, -0.3641732283464567121 ) ) ;
#27061 = CARTESIAN_POINT ( 'NONE',  ( -0.6299212598425188991, -0.1870078740157480601, -0.3641732283464567677 ) ) ;
#27062 = DIRECTION ( 'NONE',  ( -1.000000000000000000, -0.000000000000000000, -0.000000000000000000 ) ) ;
#27063 = CARTESIAN_POINT ( 'NONE',  ( 0.9776902887139113929, 0.1771653543307087630, 0.09757992244046791164 ) ) ;
#27064 = CARTESIAN_POINT ( 'NONE',  ( 0.7480314960629927956, 0.2952755905511811885, 0.000000000000000000 ) ) ;
#27065 = CARTESIAN_POINT ( 'NONE',  ( 1.108923884514436242, -0.05778040916215522460, 0.4822834645669289988 ) ) ;
#27066 = CARTESIAN_POINT ( 'NONE',  ( 0.09186351706036827158, 0.05413385826771666132, 0.4176697321401328100 ) ) ;
#27067 = CIRCLE ( 'NONE', #17652, 1.122047244094488194 ) ;
#27068 = CARTESIAN_POINT ( 'NONE',  ( 0.6233595800524939223, -0.2845877964562159024, 0.3641732283464567677 ) ) ;
#27069 = CARTESIAN_POINT ( 'NONE',  ( 1.174540682414699111, -0.05778040916215560624, -0.4822834645669293319 ) ) ;
#27070 = CARTESIAN_POINT ( 'NONE',  ( 0.1181102362204724532, -0.04921259842519685318, -0.08523872084492505052 ) ) ;
#27071 = CARTESIAN_POINT ( 'NONE',  ( -0.3674540682414692561, -0.6046776061558809534, -0.2411417322834644161 ) ) ;
#27072 = CARTESIAN_POINT ( 'NONE',  ( -0.1998031496062994683, 0.3460692066303958092, -0.9580052493438320216 ) ) ;
#27073 = CARTESIAN_POINT ( 'NONE',  ( -0.3458507752293909498, 0.3458507752293908388, -1.198818897637795367 ) ) ;
#27074 = CARTESIAN_POINT ( 'NONE',  ( 0.09186351706036799403, -0.4281496062992127816, -0.4176697321401328100 ) ) ;
#27075 = CARTESIAN_POINT ( 'NONE',  ( -0.6430446194225712953, 0.05413385826771626580, -0.4176697321401330321 ) ) ;
#27076 = CARTESIAN_POINT ( 'NONE',  ( -0.2362204724409442680, -0.1870078740157480879, -0.4822834645669291653 ) ) ;
#27077 = CARTESIAN_POINT ( 'NONE',  ( -0.2925321140481930704, -0.2925321140481933480, -2.736220472440944018 ) ) ;
#27078 = CARTESIAN_POINT ( 'NONE',  ( 0.1974969037888704704, 0.3420746716998660508, -1.876640419947506633 ) ) ;
#27079 = CARTESIAN_POINT ( 'NONE',  ( 0.2867679344610365999, -0.2867679344610365444, -0.4055118110236220486 ) ) ;
#27080 = CARTESIAN_POINT ( 'NONE',  ( 0.3726288332213487653, 0.1208384647389236927, -1.220472440944882164 ) ) ;
#27081 = CARTESIAN_POINT ( 'NONE',  ( -1.095800524934382292, -0.08942795157527998196, 0.3641732283464567121 ) ) ;
#27082 = CARTESIAN_POINT ( 'NONE',  ( 0.3917322834645670104, 2.398668435337828261E-17, -1.212598425196850238 ) ) ;
#27083 = CARTESIAN_POINT ( 'NONE',  ( -1.640419947506561060, -0.4281496062992127816, -0.4176697321401328100 ) ) ;
#27084 = CARTESIAN_POINT ( 'NONE',  ( 0.1958661417322836162, -0.3392501089628018329, 0.1430639352044112689 ) ) ;
#27085 = CARTESIAN_POINT ( 'NONE',  ( 0.3740157480314966754, -0.5400638737290844871, 0.3530559997133364547 ) ) ;
#27086 = CARTESIAN_POINT ( 'NONE',  ( -0.6496062992125976043, -0.4536011799217367080, 0.2665933059059888421 ) ) ;
#27087 = CARTESIAN_POINT ( 'NONE',  ( 1.279527559055118724, 0.1660481256975885056, 0.3530559997133364547 ) ) ;
#27088 = CARTESIAN_POINT ( 'NONE',  ( 0.3346456692913390985, 0.1660481256975885056, 0.3530559997133364547 ) ) ;
#27089 = CARTESIAN_POINT ( 'NONE',  ( 0.2118050467152636229, 1.111762164670342390, 1.102258206560161158 ) ) ;
#27090 = CARTESIAN_POINT ( 'NONE',  ( -0.3996062992125986035, -7.340648628747425578E-17, -2.401574803149606474 ) ) ;
#27091 = CARTESIAN_POINT ( 'NONE',  ( 0.3917322834645670104, 0.1049643490035304660, -1.223772596621734321 ) ) ;
#27092 = CARTESIAN_POINT ( 'NONE',  ( 1.181102362204725198, -0.1870078740157479769, 0.4822834645669291653 ) ) ;
#27093 = CARTESIAN_POINT ( 'NONE',  ( 0.4986876640419954376, 0.2306618581243848609, 0.2411417322834645549 ) ) ;
#27094 = ADVANCED_FACE ( 'NONE', ( #72369 ), #14303, .F. ) ;
#27095 = CARTESIAN_POINT ( 'NONE',  ( 0.2690288713910767848, -0.6692913385826773087, -0.1292274648535924053 ) ) ;
#27096 = CARTESIAN_POINT ( 'NONE',  ( 1.404199475065617264, -0.4281496062992124485, 0.4176697321401328655 ) ) ;
#27097 = CARTESIAN_POINT ( 'NONE',  ( 0.8792650918635177559, 0.05413385826771666132, 0.4176697321401328100 ) ) ;
#27098 = CARTESIAN_POINT ( 'NONE',  ( 0.3917322834645670104, 2.398668435337828261E-17, -0.6751968503937009203 ) ) ;
#27099 = CARTESIAN_POINT ( 'NONE',  ( -0.01312335958005186876, -0.4281496062992124485, 0.4176697321401328655 ) ) ;
#27100 = CARTESIAN_POINT ( 'NONE',  ( 1.069553805774278832, 0.2952755905511810774, -0.1292274648535930714 ) ) ;
#27101 = CARTESIAN_POINT ( 'NONE',  ( 0.3149606299212606708, -0.1870078740157480879, -0.4822834645669291653 ) ) ;
#27102 = CARTESIAN_POINT ( 'NONE',  ( 0.9908136482939640111, -0.5511811023622046335, 0.09757992244046803654 ) ) ;
#27103 = CARTESIAN_POINT ( 'NONE',  ( -1.345144356955379816, -0.05778040916215560624, -0.4822834645669293319 ) ) ;
#27104 = CARTESIAN_POINT ( 'NONE',  ( -1.286089238845143479, -0.6046776061558807314, 0.2411417322834647770 ) ) ;
#27105 = CARTESIAN_POINT ( 'NONE',  ( 0.5708661417322841158, -0.5400638737290845981, -0.3530559997133363437 ) ) ;
#27106 = CARTESIAN_POINT ( 'NONE',  ( 0.3458507752293908943, 0.3458507752293908943, -0.5295275590551181688 ) ) ;
#27107 = CARTESIAN_POINT ( 'NONE',  ( 4.797336870675656522E-17, -0.3917322834645670104, -1.803149606299212726 ) ) ;
#27108 = ORIENTED_EDGE ( 'NONE', *, *, #39374, .T. ) ;
#27109 = CARTESIAN_POINT ( 'NONE',  ( 0.3460692066303959757, -0.1998031496062991907, -0.2624671916010499206 ) ) ;
#27110 = ORIENTED_EDGE ( 'NONE', *, *, #60977, .F. ) ;
#27111 = CARTESIAN_POINT ( 'NONE',  ( 1.135170603674541256, -0.6692913385826773087, -0.1292274648535924053 ) ) ;
#27112 = CARTESIAN_POINT ( 'NONE',  ( 0.7742782152230978099, -0.3690944881889763329, 0.3153832671262228327 ) ) ;
#27113 = DIRECTION ( 'NONE',  ( 0.000000000000000000, 0.000000000000000000, 1.000000000000000000 ) ) ;
#27114 = CARTESIAN_POINT ( 'NONE',  ( -0.2240801135442098413, 1.118954560528812037, 2.822610029984497171 ) ) ;
#27115 = CARTESIAN_POINT ( 'NONE',  ( -0.4724409448818898682, -8.678599364036362592E-17, -1.141732283464566899 ) ) ;
#27116 = CARTESIAN_POINT ( 'NONE',  ( 0.2867679344610365999, -0.2867679344610365444, -0.9704724409448820532 ) ) ;
#27117 = CARTESIAN_POINT ( 'NONE',  ( 1.443569553805774897, 0.2306618581243848609, 0.2411417322834645549 ) ) ;
#27118 = CARTESIAN_POINT ( 'NONE',  ( -0.3841287887292183512, -0.08106202739158083204, -1.929133858267717105 ) ) ;
#27119 = CARTESIAN_POINT ( 'NONE',  ( -0.1115485564304456306, 0.2952755905511810774, -0.1292274648535930714 ) ) ;
#27120 = CARTESIAN_POINT ( 'NONE',  ( 0.9711286089238851948, 0.2306618581243848609, 0.2411417322834645549 ) ) ;
#27121 = ORIENTED_EDGE ( 'NONE', *, *, #48672, .T. ) ;
#27122 = CARTESIAN_POINT ( 'NONE',  ( -1.660104986876639543, -0.05778040916215560624, -0.4822834645669293319 ) ) ;
#27123 = CARTESIAN_POINT ( 'NONE',  ( -0.7193605937323468424, -5.642773921931522838E-15, -0.4118484887281985696 ) ) ;
#27124 = APPLICATION_PROTOCOL_DEFINITION ( 'draft international standard', 'automotive_design', 1998, #2497 ) ;
#27125 = CARTESIAN_POINT ( 'NONE',  ( 1.528871391076116026, 0.1771653543307087630, 0.09757992244046791164 ) ) ;
#27126 = CARTESIAN_POINT ( 'NONE',  ( -0.3042614371611541690, -2.551093532135090261E-15, 0.4118477457933002461 ) ) ;
#27127 = CARTESIAN_POINT ( 'NONE',  ( -0.9448818897637790704, -0.1870078740157480601, -0.3641732283464567677 ) ) ;
#27128 = CARTESIAN_POINT ( 'NONE',  ( 0.8792650918635177559, 0.009842519685039467087, 0.3409548833797002021 ) ) ;
#27129 = CARTESIAN_POINT ( 'NONE',  ( 0.7939632545931766261, -0.3162353388693409650, -0.4822834645669289433 ) ) ;
#27130 = ORIENTED_EDGE ( 'NONE', *, *, #71612, .F. ) ;
#27132 = CARTESIAN_POINT ( 'NONE',  ( -3.937007874015748143, 1.537401574803149984, -2.901595197523589142E-16 ) ) ;
#27131 = CARTESIAN_POINT ( 'NONE',  ( 0.4724409448818915891, -0.1265901696524958653, -2.550524934383202158 ) ) ;
#27133 = CARTESIAN_POINT ( 'NONE',  ( 0.9908136482939640111, -0.6692913385826771977, 0.1292274648535927661 ) ) ;
#27134 = CARTESIAN_POINT ( 'NONE',  ( -1.476377952755905110, -0.5400638737290845981, -0.3530559997133363437 ) ) ;
#27135 = CARTESIAN_POINT ( 'NONE',  ( 0.1049643490035303689, 0.3917322834645668994, -0.7033927577089746919 ) ) ;
#27136 = CARTESIAN_POINT ( 'NONE',  ( -0.6299212598425188991, -0.1870078740157479769, 0.3641732283464567677 ) ) ;
#27137 = CARTESIAN_POINT ( 'NONE',  ( -1.607611548556429737, 0.1771653543307087075, -0.09757992244046823083 ) ) ;
#27138 = DIRECTION ( 'NONE',  ( 0.000000000000000000, 1.000000000000000000, 0.000000000000000000 ) ) ;
#27139 = CARTESIAN_POINT ( 'NONE',  ( 0.4855643044619428750, 0.05413385826771666132, 0.4176697321401328100 ) ) ;
#27140 = CARTESIAN_POINT ( 'NONE',  ( -1.108923884514435132, -0.08942795157528024563, -0.3641732283464568787 ) ) ;
#27141 = CARTESIAN_POINT ( 'NONE',  ( 0.07217847769028949700, -0.08942795157528024563, -0.3641732283464568787 ) ) ;
#27142 = CARTESIAN_POINT ( 'NONE',  ( -0.1246719160104980823, 0.2952755905511811885, 0.1292274648535926551 ) ) ;
#27143 = CARTESIAN_POINT ( 'NONE',  ( -0.9580052493438311334, -0.004921259842519870586, -0.3153832671262229437 ) ) ;
#27144 = CARTESIAN_POINT ( 'NONE',  ( 0.3917322834645670659, -0.1049643490035303273, -0.1082870323172722415 ) ) ;
#27145 = CARTESIAN_POINT ( 'NONE',  ( 0.8727034120734912248, -0.3162353388693409650, -0.4822834645669289433 ) ) ;
#27146 = CARTESIAN_POINT ( 'NONE',  ( -0.4724409448818896462, -0.1265901696524993070, -0.2034120734908136108 ) ) ;
#27147 = CARTESIAN_POINT ( 'NONE',  ( -0.4724409448818898682, -8.678599364036362592E-17, -1.533464566929133799 ) ) ;
#27148 = CARTESIAN_POINT ( 'NONE',  ( -0.9186351706036736120, 0.2306618581243848609, 0.2411417322834645549 ) ) ;
#27149 = CARTESIAN_POINT ( 'NONE',  ( -0.2821522309711278487, 0.1771653543307087630, 0.09757992244046791164 ) ) ;
#27150 = CARTESIAN_POINT ( 'NONE',  ( -1.338582677165353729, -0.1870078740157479769, 0.4822834645669291653 ) ) ;
#27151 = CARTESIAN_POINT ( 'NONE',  ( 0.8333333333333340365, -0.5511811023622046335, 0.09757992244046803654 ) ) ;
#27152 = CARTESIAN_POINT ( 'NONE',  ( -0.9186351706036736120, 0.1283753931104748280, 0.1820866141732283561 ) ) ;
#27153 = CARTESIAN_POINT ( 'NONE',  ( -1.194225721784776262, 0.05413385826771626580, -0.4176697321401330321 ) ) ;
#27154 = CARTESIAN_POINT ( 'NONE',  ( -1.030183727034119867, -0.05778040916215560624, -0.4822834645669293319 ) ) ;
#27155 = CARTESIAN_POINT ( 'NONE',  ( 1.660104986876641320, -0.05778040916215522460, 0.4822834645669289988 ) ) ;
#27156 = CARTESIAN_POINT ( 'NONE',  ( 0.5314960629920859603, 2.755905511811024056, 3.821484228344198986 ) ) ;
#27157 = CARTESIAN_POINT ( 'NONE',  ( 0.8267716535433078384, -0.5511811023622047445, 6.969142054262312111E-17 ) ) ;
#27158 = PRODUCT_DEFINITION_SHAPE ( 'NONE', 'NONE',  #83315 ) ;
#27159 = CARTESIAN_POINT ( 'NONE',  ( 0.4527559055118117182, 0.1660481256975883668, -0.3530559997133364547 ) ) ;
#27160 = CARTESIAN_POINT ( 'NONE',  ( -1.522309711286088607, -0.6046776061558807314, 0.2411417322834647770 ) ) ;
#27161 = CARTESIAN_POINT ( 'NONE',  ( -1.620734908136482577, -0.6692913385826773087, -0.1292274648535924053 ) ) ;
#27162 = VECTOR ( 'NONE', #82159, 39.37007874015748143 ) ;
#27163 = ORIENTED_EDGE ( 'NONE', *, *, #14047, .F. ) ;
#27164 = CARTESIAN_POINT ( 'NONE',  ( 4.893765752498283308E-17, -0.3996062992125985480, -2.675196850393700920 ) ) ;
#27165 = CARTESIAN_POINT ( 'NONE',  ( -1.430446194225720724, -0.004921259842519870586, -0.3153832671262229437 ) ) ;
#27166 = CARTESIAN_POINT ( 'NONE',  ( -0.4593175853018364174, -0.4281496062992127816, -0.4176697321401328100 ) ) ;
#27167 = CARTESIAN_POINT ( 'NONE',  ( 0.6758530183727039509, 0.2952755905511810774, -0.1292274648535930714 ) ) ;
#27168 = CARTESIAN_POINT ( 'NONE',  ( -1.476377952755905110, -0.4536011799217368745, -0.2665933059059886201 ) ) ;
#27169 = CARTESIAN_POINT ( 'NONE',  ( -0.3996062992125985480, -7.340648628747423112E-17, -1.690944881889763884 ) ) ;
#27170 = CARTESIAN_POINT ( 'NONE',  ( -1.384514435695537005, 0.2952755905511811885, 0.1292274648535926551 ) ) ;
#27171 = CARTESIAN_POINT ( 'NONE',  ( 0.9317585301837276734, 0.05413385826771626580, -0.4176697321401330321 ) ) ;
#27172 = CARTESIAN_POINT ( 'NONE',  ( 0.4396325459317593221, 0.2952755905511810774, -0.1292274648535930714 ) ) ;
#27173 = CARTESIAN_POINT ( 'NONE',  ( 1.377952755905512472, -0.6692913385826771977, 8.415575281601705876E-17 ) ) ;
#27174 = FACE_OUTER_BOUND ( 'NONE', #48335, .T. ) ;
#27175 = CARTESIAN_POINT ( 'NONE',  ( -0.2925321140481930704, -0.2925321140481933480, -1.476377952755905554 ) ) ;
#27176 = CARTESIAN_POINT ( 'NONE',  ( 0.1058382717557500713, -0.3949938075777409408, -0.7152230971128611392 ) ) ;
#27177 = CYLINDRICAL_SURFACE ( 'NONE', #58716, 3.543307086614173151 ) ;
#27178 = CARTESIAN_POINT ( 'NONE',  ( 0.4461942257217855201, -0.5023911411419708095, 0.1820866141732285504 ) ) ;
#27179 = CARTESIAN_POINT ( 'NONE',  ( 0.07217847769028949700, -0.05778040916215560624, -0.4822834645669293319 ) ) ;
#27180 = CARTESIAN_POINT ( 'NONE',  ( 1.200787401574803681, -0.5400638737290845981, -0.3530559997133363437 ) ) ;
#27181 = CARTESIAN_POINT ( 'NONE',  ( -0.1974969037888704149, -0.3420746716998661063, -1.717191601049868677 ) ) ;
#27182 = CARTESIAN_POINT ( 'NONE',  ( 0.5052493438320218022, -0.5511811023622048555, -0.09757992244046775898 ) ) ;
#27183 = CARTESIAN_POINT ( 'NONE',  ( -0.6758530183727028406, 0.2952755905511811885, 0.1292274648535926551 ) ) ;
#27184 = CARTESIAN_POINT ( 'NONE',  ( 1.535433070866142335, -0.6692913385826771977, 8.415575281601705876E-17 ) ) ;
#27185 = CARTESIAN_POINT ( 'NONE',  ( 0.5446194225721792126, -0.3162353388693405765, 0.4822834645669290543 ) ) ;
#27186 = CARTESIAN_POINT ( 'NONE',  ( 0.4091458600556403535, 0.2362204724409449896, -2.178477690288713742 ) ) ;
#27187 = CARTESIAN_POINT ( 'NONE',  ( -2.503252890251015828, 2.755905511811024056, 0.5314960629921260393 ) ) ;
#27188 = ORIENTED_EDGE ( 'NONE', *, *, #2315, .T. ) ;
#27189 = EDGE_CURVE ( 'NONE', #66338, #79813, #34477, .T. ) ;
#27190 = VERTEX_POINT ( 'NONE', #28569 ) ;
#27191 = CARTESIAN_POINT ( 'NONE',  ( -1.528871391076114250, 0.2952755905511810774, -0.1292274648535930714 ) ) ;
#27193 = CARTESIAN_POINT ( 'NONE',  ( -1.036745406824146176, -0.4281496062992124485, 0.4176697321401328655 ) ) ;
#27192 = CARTESIAN_POINT ( 'NONE',  ( -1.345144356955379816, -0.2845877964562159024, 0.3641732283464567677 ) ) ;
#27194 = CARTESIAN_POINT ( 'NONE',  ( 0.3917322834645668994, -0.1049643490035303134, -2.238825828575116805 ) ) ;
#27195 = CARTESIAN_POINT ( 'NONE',  ( -0.1070741851644056997, 0.3996062992125984925, -2.760498687664041384 ) ) ;
#27196 = CARTESIAN_POINT ( 'NONE',  ( -1.633858267716534529, 0.07958543189024085140, 0.2665933059059887866 ) ) ;
#27197 = CARTESIAN_POINT ( 'NONE',  ( -1.259842519685038686, -0.1870078740157479769, 0.4822834645669291653 ) ) ;
#27198 = CARTESIAN_POINT ( 'NONE',  ( 0.2493438320209980519, -0.4281496062992127816, -0.4176697321401328100 ) ) ;
#27199 = CARTESIAN_POINT ( 'NONE',  ( -1.174540682414697335, -0.05778040916215522460, 0.4822834645669289988 ) ) ;
#27200 = CARTESIAN_POINT ( 'NONE',  ( -0.3917322834645668994, -0.1049643490035306742, -2.803130290517373613 ) ) ;
#27201 = SHAPE_REPRESENTATION ( 'Chuck Body Assembly Bolts', ( #22098 ), #46360 ) ;
#27202 = CARTESIAN_POINT ( 'NONE',  ( 0.7874015748031503170, -0.1870078740157479769, 0.4822834645669291653 ) ) ;
#27203 = CARTESIAN_POINT ( 'NONE',  ( 0.2867679344610365999, 0.2867679344610365999, -2.019685039370078261 ) ) ;
#27204 = CARTESIAN_POINT ( 'NONE',  ( -1.141732283464566011, 0.1771653543307087630, 0.000000000000000000 ) ) ;
#27205 = ORIENTED_EDGE ( 'NONE', *, *, #31652, .F. ) ;
#27206 = CARTESIAN_POINT ( 'NONE',  ( -0.2891555358219911054, 0.2891555358219909388, -2.224409448818897683 ) ) ;
#27207 = VERTEX_POINT ( 'NONE', #41202 ) ;
#27208 = DIRECTION ( 'NONE',  ( -3.096699300667737957E-16, 1.000000000000000000, -0.000000000000000000 ) ) ;
#27209 = CARTESIAN_POINT ( 'NONE',  ( -1.135170603674539924, -0.6692913385826771977, 0.1292274648535927661 ) ) ;
#27210 = CARTESIAN_POINT ( 'NONE',  ( -1.135170603674539924, 0.2952755905511810774, -0.1292274648535930714 ) ) ;
#27211 = CARTESIAN_POINT ( 'NONE',  ( -0.2925321140481930704, -0.2925321140481933480, -0.5314960629921260393 ) ) ;
#27212 = CARTESIAN_POINT ( 'NONE',  ( -1.351706036745406347, 0.05413385826771626580, -0.4176697321401330321 ) ) ;
#27213 = CARTESIAN_POINT ( 'NONE',  ( -1.469816272965878357, -0.6046776061558809534, -0.2411417322834644161 ) ) ;
#27214 = CARTESIAN_POINT ( 'NONE',  ( -1.279527559055116948, 0.1660481256975883668, -0.3530559997133364547 ) ) ;
#27215 = SURFACE_STYLE_FILL_AREA ( #32694 ) ;
#27216 = CARTESIAN_POINT ( 'NONE',  ( -0.8202099737532798640, 0.2952755905511810219, -0.1292274648535930437 ) ) ;
#27217 = AXIS2_PLACEMENT_3D ( 'NONE', #70075, #57437, #62534 ) ;
#27218 = CARTESIAN_POINT ( 'NONE',  ( -0.05249343832020911260, 0.1283753931104748280, 0.1820866141732283561 ) ) ;
#27219 = CARTESIAN_POINT ( 'NONE',  ( 0.4359958488159500489, 1.724409448818897905, 2.094141031014936871 ) ) ;
#27220 = CARTESIAN_POINT ( 'NONE',  ( 0.1958661417322834775, 0.3392501089628018884, -0.3864829396325459854 ) ) ;
#27221 = CARTESIAN_POINT ( 'NONE',  ( -0.6102362204724400829, 0.07958543189024085140, 0.2665933059059887866 ) ) ;
#27222 = CARTESIAN_POINT ( 'NONE',  ( -0.7808398950131222316, -0.3162353388693409650, -0.4822834645669289433 ) ) ;
#27223 = CARTESIAN_POINT ( 'NONE',  ( 0.8070866141732288002, 0.1660481256975885056, 0.3530559997133364547 ) ) ;
#27224 = CARTESIAN_POINT ( 'NONE',  ( -1.036745406824146176, -0.4281496062992124485, 0.4176697321401328655 ) ) ;
#27225 = ORIENTED_EDGE ( 'NONE', *, *, #24920, .T. ) ;
#27226 = VERTEX_POINT ( 'NONE', #10469 ) ;
#27228 = AXIS2_PLACEMENT_3D ( 'NONE', #64858, #58107, #72015 ) ;
#27227 = CARTESIAN_POINT ( 'NONE',  ( -1.076115485564303809, -0.6046776061558809534, -0.2411417322834644161 ) ) ;
#27229 = CARTESIAN_POINT ( 'NONE',  ( 0.8858267716535438430, -0.5400638737290845981, -0.3530559997133363437 ) ) ;
#27230 = CARTESIAN_POINT ( 'NONE',  ( -1.548556430446193399, 0.1283753931104748280, 0.1820866141732283561 ) ) ;
#27231 =( LENGTH_UNIT ( ) NAMED_UNIT ( * ) SI_UNIT ( $, .METRE. ) );
#27232 = CARTESIAN_POINT ( 'NONE',  ( 0.4724409448818898682, 2.892866454678787531E-17, -1.220472440944881942 ) ) ;
#27233 = CARTESIAN_POINT ( 'NONE',  ( 2.139011644334231743, 1.422882880004778139, 0.4606469518571244537 ) ) ;
#27234 = CARTESIAN_POINT ( 'NONE',  ( -0.1958661417322836718, 0.3392501089628017219, -0.3202099737532808077 ) ) ;
#27235 = CARTESIAN_POINT ( 'NONE',  ( 0.1049643490035304799, -0.3917322834645669549, -2.374671916010498762 ) ) ;
#27236 = CARTESIAN_POINT ( 'NONE',  ( -0.3937007874015740483, -0.1870078740157479769, 0.4822834645669291653 ) ) ;
#27237 = CARTESIAN_POINT ( 'NONE',  ( -1.371391076115484609, -0.5511811023622046335, 0.09757992244046803654 ) ) ;
#27238 = CARTESIAN_POINT ( 'NONE',  ( 0.3996062992125984925, 0.1070741851644054637, -0.04396325459317587669 ) ) ;
#27240 = FACE_OUTER_BOUND ( 'NONE', #12711, .T. ) ;
#27239 = CARTESIAN_POINT ( 'NONE',  ( -1.496062992125983815, -0.1870078740157480879, -0.4822834645669291653 ) ) ;
#27241 = CARTESIAN_POINT ( 'NONE',  ( -1.574803149606298636, -0.1870078740157479769, 0.4822834645669291653 ) ) ;
#27242 = CARTESIAN_POINT ( 'NONE',  ( -0.2559055118110230564, 0.1660481256975883668, -0.3530559997133364547 ) ) ;
#27243 = CARTESIAN_POINT ( 'NONE',  ( 0.1974969037888706092, -0.3420746716998660508, -2.845800524934383624 ) ) ;
#27244 = CARTESIAN_POINT ( 'NONE',  ( 0.3346456692913390985, 0.07958543189024085140, 0.2665933059059887866 ) ) ;
#27245 = CARTESIAN_POINT ( 'NONE',  ( 0.3917322834645670104, -0.1049643490035303273, -0.03871391076115493490 ) ) ;
#27246 = CARTESIAN_POINT ( 'NONE',  ( 0.4790026246719168435, -0.2845877964562161244, -0.3641732283464567121 ) ) ;
#27247 = CARTESIAN_POINT ( 'NONE',  ( 1.555118110236221041, -0.4536011799217367080, 0.2665933059059888421 ) ) ;
#27248 = CARTESIAN_POINT ( 'NONE',  ( 1.017060367454068581, -0.05778040916215560624, -0.4822834645669293319 ) ) ;
#27249 = CARTESIAN_POINT ( 'NONE',  ( 0.09186351706036827158, -0.004921259842519576551, 0.3153832671262227771 ) ) ;
#27250 = CARTESIAN_POINT ( 'NONE',  ( -0.3917322834645670104, -7.196005306013484475E-17, -1.763779527559055094 ) ) ;
#27251 = CARTESIAN_POINT ( 'NONE',  ( -1.154855643044618851, 0.2306618581243848609, 0.2411417322834645549 ) ) ;
#27252 = CARTESIAN_POINT ( 'NONE',  ( 0.01312335958005323398, -0.004921259842519576551, 0.3153832671262227771 ) ) ;
#27253 = CARTESIAN_POINT ( 'NONE',  ( -0.3458507752293909498, 0.3458507752293907833, -0.2539370078740156855 ) ) ;
#27254 = CARTESIAN_POINT ( 'NONE',  ( -0.3018372703412066094, -0.3690944881889765550, -0.3153832671262227771 ) ) ;
#27255 = CARTESIAN_POINT ( 'NONE',  ( 2.795275590551181910, 1.488513638086842006, 0.000000000000000000 ) ) ;
#27256 = CARTESIAN_POINT ( 'NONE',  ( -0.01968503937007793844, 0.1660481256975883668, -0.3530559997133364547 ) ) ;
#27257 = CARTESIAN_POINT ( 'NONE',  ( -0.4724409448818898682, -8.678599364036362592E-17, -0.7460629921259841479 ) ) ;
#27258 = CARTESIAN_POINT ( 'NONE',  ( 1.076115485564305141, -0.5023911411419708095, 0.1820866141732285504 ) ) ;
#27259 = CARTESIAN_POINT ( 'NONE',  ( -0.3149606299212590610, -0.1870078740157479769, 0.3641732283464567677 ) ) ;
#27260 = CARTESIAN_POINT ( 'NONE',  ( -0.1049868766404193215, -0.6046776061558807314, 0.2411417322834647770 ) ) ;
#27261 = CARTESIAN_POINT ( 'NONE',  ( 0.000000000000000000, 0.000000000000000000, -2.755905511811024056 ) ) ;
#27262 = CARTESIAN_POINT ( 'NONE',  ( -0.9383202099737524282, -0.2845877964562161244, -0.3641732283464567121 ) ) ;
#27263 = CARTESIAN_POINT ( 'NONE',  ( 0.4744094488188886904, 1.537401574803149984, 2.554262525012303886 ) ) ;
#27264 = CARTESIAN_POINT ( 'NONE',  ( 0.6233595800524942554, -0.05778040916215560624, -0.4822834645669293319 ) ) ;
#27265 = CARTESIAN_POINT ( 'NONE',  ( -0.8267716535433065062, 0.2952755905511811885, 0.000000000000000000 ) ) ;
#27266 = CARTESIAN_POINT ( 'NONE',  ( -0.3996062992125985480, -7.340648628747423112E-17, -1.218503937007874072 ) ) ;
#27267 = CARTESIAN_POINT ( 'NONE',  ( -0.2867679344610365999, 0.2867679344610364889, -2.624015748031495399 ) ) ;
#27268 = CARTESIAN_POINT ( 'NONE',  ( 0.1902887139107617975, 0.1771653543307087630, 0.09757992244046791164 ) ) ;
#27269 = CARTESIAN_POINT ( 'NONE',  ( -0.7152230971128602510, -0.3162353388693405765, 0.4822834645669290543 ) ) ;
#27270 = CARTESIAN_POINT ( 'NONE',  ( -1.082677165354329896, -0.5400638737290845981, -0.3530559997133363437 ) ) ;
#27271 = CARTESIAN_POINT ( 'NONE',  ( -1.207349081364828436, -0.5023911411419708095, 0.1820866141732285504 ) ) ;
#27272 = CARTESIAN_POINT ( 'NONE',  ( -3.916339746322849980, 1.286570825603250201, -0.4029754474414414256 ) ) ;
#27273 = CARTESIAN_POINT ( 'NONE',  ( -1.003937007874014853, 0.07958543189024085140, 0.2665933059059887866 ) ) ;
#27274 = CARTESIAN_POINT ( 'NONE',  ( -0.7214341416610897673, 0.004960608223778500969, -0.3437734562760191848 ) ) ;
#27275 = CARTESIAN_POINT ( 'NONE',  ( 0.9711286089238851948, 0.2306618581243848609, 0.2411417322834645549 ) ) ;
#27276 = CARTESIAN_POINT ( 'NONE',  ( 0.3996062992125986590, -0.1070741851644053111, -0.2690288713910760632 ) ) ;
#27277 = AXIS2_PLACEMENT_3D ( 'NONE', #59361, #2964, #65708 ) ;
#27278 = CARTESIAN_POINT ( 'NONE',  ( -0.3392501089628019995, 0.1958661417322831999, -2.385189919456379926 ) ) ;
#27279 = CARTESIAN_POINT ( 'NONE',  ( -0.8561328129276786214, -2.191421614605370878E-15, 0.4445507791589071167 ) ) ;
#27280 = CARTESIAN_POINT ( 'NONE',  ( 1.587926509186352142, -0.004921259842519576551, 0.3153832671262227771 ) ) ;
#27281 = CARTESIAN_POINT ( 'NONE',  ( -1.443569553805773564, -0.6046776061558807314, 0.2411417322834647770 ) ) ;
#27282 = CARTESIAN_POINT ( 'NONE',  ( 1.423884514435696191, -0.05778040916215522460, 0.4822834645669289988 ) ) ;
#27283 = CARTESIAN_POINT ( 'NONE',  ( -9.594673741351313045E-17, 0.3917322834645670104, -2.446850393700787496 ) ) ;
#27284 = CARTESIAN_POINT ( 'NONE',  ( 1.686351706036745890, 0.1771653543307087630, 0.09757992244046791164 ) ) ;
#27285 = EDGE_CURVE ( 'NONE', #56091, #8593, #75370, .T. ) ;
#27286 =( BOUNDED_SURFACE ( )  B_SPLINE_SURFACE ( 1, 2, ( 
 ( #50927, #6330, #58507, #71564, #7597, #2110, #20638, #870, #26528, #64828, #59755, #79147, #51760, #53439, #52182, #32416, #38732, #39144, #27775, #32838, #8424, #34092, #77885, #20217, #58930, #1289, #6744, #21464, #21052, #47122, #7167, #13914, #33678, #46712, #26938, #65687, #8014, #14753, #45866, #40407, #13079, #65261, #1697, #64409, #52600, #39999, #77462, #58078, #46290, #27355, #45449, #19800, #39571, #444, #13488, #26099, #33271, #78306, #71986, #78728, #14339, #71146, #59340, #53014, #72404, #66089, #80393, #79560, #41645, #34930, #16408, #79979, #73229, #9669, #53847, #60178, #74062, #22292, #74478, #40818, #47953, #2531, #66502, #73656, #42054, #15580, #28189, #54681, #3765, #67750, #35338, #67336, #8837, #61002, #54263, #9258, #15998, #10084, #3350, #29016, #22705, #15161, #29429, #21873, #34513, #48363, #60592, #55087, #47539, #2942, #35748, #80796, #41238, #28606, #61415, #23113, #48779, #16825, #66926, #72811, #33526, #73078, #58348, #1548, #77732, #709, #27202, #46968, #1136, #71412, #59604, #60026, #21315, #14601, #46554, #26368, #20901, #65529, #20484, #59189, #72662, #52865, #72252, #78575, #7013, #2381, #20063, #32681, #40255, #46138, #28038, #52026, #71833, #7862, #53696, #45715, #14182, #78995, #65938, #47387, #66352, #65100, #79405, #13759, #21724, #15428, #8274, #39416, #26786, #15010, #40667, #64674, #7437, #52443, #39840, #33940, #33108, #1959, #78153, #27621, #58776, #53284, #8690, #34360, #81475, #28868, #60442, #66777, #67188, #30106, #60852, #36425, #62098, #54530, #3205, #3619, #29286, #34783, #23792, #49047, #4440, #9519, #16260, #61690, #74744, #54949, #10358, #36018, #42729, #35191, #68425, #55768, #9931, #29695, #9110, #80655, #68014, #79828, #49464, #48634, #55357, #73506, #22145, #67600, #2794, #41503, #54113, #80246, #22968, #22561, #23379, #48223, #28453, #74329, #42315, #73919, #4030, #81063, #15854, #16676, #41906, #17094, #35603, #61265, #10765, #47803, #75158, #41088, #30975, #17550, #62978, #5317, #81113, #4076, #30156, #55818, #61318, #50330, #75620, #56642, #10410, #42778, #4904, #17958, #81526, #36889, #62565, #69297, #61739, #11646, #82343, #36472, #56241, #9989, #23846, #11228, #23019, #24661, #75206, #81938, #16726, #48686, #10812, #35655, #68066, #80705, #29743, #49513, #36067, #49922, #55407, #3673, #43182, #68879, #23431, #30575, #24249, #42367, #43595, #49095, #37304, #62147, #74799, #76027, #74383, #17146, #18372, #4488, #67652, #29336, #54997, #68474, #37707, #64215, #26320, #63792, #50740, #38946, #39365, #665, #77261, #25897, #63380, #245, #44821, #83159, #12875, #51981, #6549, #51557, #38534, #69706, #65050, #82745, #12049, #19590, #25478, #7388, #5716, #51145, #70519, #33055, #31386, #76839, #58299, #32220, #26741, #45667, #44410, #58726, #57052, #1089, #52395, #45252, #76438, #6130, #77686, #20016, #78104, #25066, #31805, #19173, #57878, #44012, #70949, #57465, #13294, #12456, #18767, #70104, #38117, #64629, #6965, #32636, #71363, #13711, #15802, #14557, #46089, #15377, #34733, #33891, #7815, #20852, #52817, #41453, #79777, #2333, #67137, #66724, #9466, #33481, #27575, #47337, #59557, #47754, #20435, #41039, #22093, #40619, #54484, #46504, #65892, #21676, #59143, #8227, #27989, #1501, #71781, #35140, #73027, #9061, #60393, #46921, #72204, #3156, #1912, #14136, #28819, #8641, #2744, #53232, #60802, #40209, #78948, #34313, #39788, #65483, #27153, #28404, #66302, #54062, #73452, #78528, #21266, #72614, #14962, #59974, #53649, #79357, #36379, #80608, #62053, #80195, #35973, #56139, #22918, #38328, #18969, #41857, #55720, #24155, #29238, #36787, #4391, #81844, #70313, #30059, #81430, #43088, #23745, #48585, #81018, #50941, #10722, #67965, #67549, #74282, #9884, #44618, #12668, #64001, #10307, #35553, #49418, #61216, #62463, #16626, #42268, #76638, #75112, #3984, #23331, #29648, #61643, #55310, #6343, #32015, #49001, #3571, #22513, #54902, #17458, #48174, #4798, #73870, #16210, #74700, #30475, #17045, #68785, #11129, #42685, #68383, #57675, #13500, #33691, #58091, #14764, #78740, #19387 ),
 ( #51351, #72415, #21063, #13927, #64421, #19813, #40011, #65698, #46723, #45039, #45462, #32850, #52195, #40420, #65273, #71160, #39156, #26112, #66101, #8437, #13092, #37, #64841, #77054, #8028, #7179, #25690, #7610, #53027, #70739, #58519, #77477, #20230, #45878, #38745, #6756, #59352, #32428, #456, #883, #78320, #1711, #71576, #26951, #52614, #27366, #51773, #26542, #77899, #39584, #46304, #33283, #58944, #1302, #20651, #71998, #14352, #48377, #66517, #15175, #60605, #2123, #34527, #47134, #53860, #73669, #60192, #16422, #28201, #27789, #67348, #35352, #2543, #80406, #54698, #8849, #47968, #73244, #74076, #2954, #79572, #41657, #40832, #72825, #42068, #28619, #42473, #53451, #54277, #21888, #79159, #79993, #67763, #47552, #15593, #29029, #29443, #10099, #9681, #16011, #21476, #61014, #34942, #41252, #22307, #35763, #3365, #66939, #9271, #22718, #61431, #80811, #23126, #74492, #3780, #55102, #48794, #16839, #68176, #34107, #59768, #37816, #11757, #17658, #11335, #43289, #36575, #4590, #31499, #25179, #68986, #17254, #76547, #74906, #24359, #50847, #50434, #61844, #57158, #81640, #44119, #42882, #18066, #43700, #69811, #81219, #5826, #30261, #36171, #5422, #24766, #23949, #23535, #10918, #68577, #82858, #12160, #75726, #18875, #56751, #44524, #49204, #36994, #37412, #49617, #63492, #10517, #31084, #4185, #30684, #29848, #62254, #55925, #63084, #75311, #62674, #69404, #5015, #55511, #56345, #82451, #76136, #18477, #82046, #50029, #52929, #32330, #63903, #78642, #58418, #71479, #356, #59255, #12989, #38644, #777, #20965, #1612, #83268, #52512, #32751, #33177, #13826, #76956, #64322, #57992, #58845, #6658, #39485, #20132, #26439, #70632, #52091, #70212, #26013, #46205, #51671, #27268, #7929, #31915, #45780, #14250, #19284, #26853, #77800, #71899, #12568, #65172, #7508, #1203, #78220, #77374, #71060, #39909, #38226, #6239, #25591, #20553, #65596, #33590, #57577, #44935, #19706, #45364, #51254, #13404, #39059, #64742, #7080, #47034, #28518, #46624, #2446, #22619, #72728, #3680, #67660, #8341, #22206, #73976, #79063, #3265, #54174, #48278, #35662, #2854, #79888, #9581, #47862, #15074, #47448, #16322, #60506, #34426, #34007, #40732, #59669, #9997, #61325, #29344, #60092, #2024, #73567, #27689, #28926, #66416, #8752, #41967, #15911, #53759, #73143, #79470, #28105, #21786, #55004, #80712, #15492, #53353, #72320, #21380, #41560, #14666, #54594, #40324, #66002, #41149, #80304, #66838, #67249, #35250, #9172, #34843, #60914, #17154, #48693, #17967, #37314, #36481, #10418, #23439, #55415, #44022, #82353, #4914, #69715, #69306, #12059, #36076, #30164, #49931, #62156, #50339, #23027, #43604, #24671, #43191, #57061, #49103, #68482, #24258, #61747, #10821, #30583, #4084, #74391, #37716, #75629, #11655, #62987, #49521, #74808, #5725, #4497, #16735, #31396, #11237, #5326, #55827, #63390, #42787, #81534, #36897, #76036, #23854, #18381, #42375, #75214, #30984, #68073, #62573, #56652, #29752, #81122, #56249, #17559, #68887, #81945, #25908, #50750, #83169, #12466, #19183, #38956, #25489, #65063, #76850, #76450, #32646, #676, #51155, #45678, #20027, #57475, #13304, #38545, #39378, #51568, #44832, #6977, #6140, #38128, #7401, #77271, #7827, #18777, #19600, #63802, #44420, #45263, #33070, #70530, #31815, #77697, #78116, #58739, #58311, #64640, #70115, #26330, #256, #64225, #70959, #1101, #51992, #71374, #13724, #25076, #20449, #12885, #6559, #26752, #32231, #46102, #57889, #52407, #71795, #14148, #39802, #65495, #33494, #82754, #41870, #60816, #59570, #73883, #52830, #16223, #22524, #15390, #65904, #21280, #41467, #67152, #48186, #20867, #46935, #34326, #53663, #67564, #66738, #72627, #14975, #27589, #9896, #59156, #14570, #1514, #40634, #78542, #9481, #66316, #27168, #9076, #54496, #80208, #8655, #78961, #21689, #47352, #46518, #72219, #35156, #40222, #1926, #59989, #79792, #3168, #73041, #28417, #54077, #79370, #28832, #2347, #8240, #22108, #33906, #15818, #34747, #41052, #53247, #60407, #28003, #2758, #47768, #73467, #55734, #17469, #30071, #61230, #30893, #74294 ) ),
 .UNSPECIFIED., .F., .F., .F. ) 
 B_SPLINE_SURFACE_WITH_KNOTS ( ( 2, 2 ),
 ( 3, 2, 2, 2, 2, 2, 2, 2, 2, 2, 2, 2, 2, 2, 2, 2, 2, 2, 2, 2, 2, 2, 2, 2, 2, 2, 2, 2, 2, 2, 2, 2, 2, 2, 2, 2, 2, 2, 2, 2, 2, 2, 2, 2, 2, 2, 2, 2, 2, 2, 2, 2, 2, 2, 2, 2, 2, 2, 2, 2, 2, 2, 2, 2, 2, 2, 2, 2, 2, 2, 2, 2, 2, 2, 2, 2, 2, 2, 2, 2, 2, 2, 2, 2, 2, 2, 2, 2, 2, 2, 2, 2, 2, 2, 2, 2, 2, 2, 2, 2, 2, 2, 2, 2, 2, 2, 2, 2, 2, 2, 2, 2, 2, 2, 2, 2, 2, 2, 2, 2, 2, 2, 2, 2, 2, 2, 2, 2, 2, 2, 2, 2, 2, 2, 2, 2, 2, 2, 2, 2, 2, 2, 2, 2, 2, 2, 2, 2, 2, 2, 2, 2, 2, 2, 2, 2, 2, 2, 2, 2, 2, 2, 2, 2, 2, 2, 2, 2, 2, 2, 2, 2, 2, 2, 2, 2, 2, 2, 2, 2, 2, 2, 2, 2, 2, 2, 2, 2, 2, 2, 2, 2, 2, 2, 2, 2, 2, 2, 2, 2, 2, 2, 2, 2, 2, 2, 2, 2, 2, 2, 2, 2, 2, 2, 2, 2, 2, 2, 2, 2, 2, 2, 2, 2, 2, 2, 2, 2, 2, 2, 2, 2, 2, 2, 2, 2, 2, 2, 2, 2, 2, 2, 2, 2, 2, 2, 2, 2, 2, 2, 2, 2, 2, 2, 2, 3 ),
 ( 0.000000000000000000, 1.000000000000000000 ),
 ( 0.000000000000000000, 0.003787878787878787984, 0.007575757575757575968, 0.01136363636363636395, 0.01515151515151515194, 0.01893939393939393992, 0.02272727272727272790, 0.02651515151515151589, 0.03030303030303030387, 0.03409090909090908839, 0.03787878787878787984, 0.04166666666666666435, 0.04545454545454545581, 0.04924242424242424032, 0.05303030303030303177, 0.05681818181818181629, 0.06060606060606060774, 0.06439393939393939226, 0.06818181818181817677, 0.07196969696969697516, 0.07575757575757575968, 0.07954545454545454419, 0.08333333333333332871, 0.08712121212121212710, 0.09090909090909091161, 0.09469696969696969613, 0.09848484848484848064, 0.1022727272727272790, 0.1060606060606060635, 0.1098484848484848481, 0.1136363636363636326, 0.1174242424242424310, 0.1212121212121212155, 0.1250000000000000000, 0.1287878787878787845, 0.1325757575757575690, 0.1363636363636363535, 0.1401515151515151381, 0.1439393939393939503, 0.1477272727272727348, 0.1515151515151515194, 0.1553030303030303039, 0.1590909090909090884, 0.1628787878787878729, 0.1666666666666666574, 0.1704545454545454419, 0.1742424242424242542, 0.1780303030303030387, 0.1818181818181818232, 0.1856060606060606077, 0.1893939393939393923, 0.1931818181818181768, 0.1969696969696969613, 0.2007575757575757458, 0.2045454545454545581, 0.2083333333333333426, 0.2121212121212121271, 0.2159090909090909116, 0.2196969696969696961, 0.2234848484848484806, 0.2272727272727272652, 0.2310606060606060497, 0.2348484848484848619, 0.2386363636363636465, 0.2424242424242424310, 0.2462121212121212155, 0.2500000000000000000, 0.2537878787878787845, 0.2575757575757575690, 0.2613636363636363535, 0.2651515151515151381, 0.2689393939393939226, 0.2727272727272727071, 0.2765151515151514916, 0.2803030303030302761, 0.2840909090909091161, 0.2878787878787879007, 0.2916666666666666852, 0.2954545454545454697, 0.2992424242424242542, 0.3030303030303030387, 0.3068181818181818232, 0.3106060606060606077, 0.3143939393939393923, 0.3181818181818181768, 0.3219696969696969613, 0.3257575757575757458, 0.3295454545454545303, 0.3333333333333333148, 0.3371212121212120993, 0.3409090909090908839, 0.3446969696969697239, 0.3484848484848485084, 0.3522727272727272929, 0.3560606060606060774, 0.3598484848484848619, 0.3636363636363636465, 0.3674242424242424310, 0.3712121212121212155, 0.3750000000000000000, 0.3787878787878787845, 0.3825757575757575690, 0.3863636363636363535, 0.3901515151515151381, 0.3939393939393939226, 0.3977272727272727071, 0.4015151515151514916, 0.4053030303030302761, 0.4090909090909091161, 0.4128787878787879007, 0.4166666666666666852, 0.4204545454545454697, 0.4242424242424242542, 0.4280303030303030387, 0.4318181818181818232, 0.4356060606060606077, 0.4393939393939393923, 0.4431818181818181768, 0.4469696969696969613, 0.4507575757575757458, 0.4545454545454545303, 0.4583333333333333148, 0.4621212121212120993, 0.4659090909090908839, 0.4696969696969697239, 0.4734848484848485084, 0.4772727272727272929, 0.4810606060606060774, 0.4848484848484848619, 0.4886363636363636465, 0.4924242424242424310, 0.4962121212121212155, 0.5000000000000000000, 0.5037878787878787845, 0.5075757575757575690, 0.5113636363636363535, 0.5151515151515151381, 0.5189393939393939226, 0.5227272727272727071, 0.5265151515151514916, 0.5303030303030302761, 0.5340909090909090606, 0.5378787878787878451, 0.5416666666666666297, 0.5454545454545454142, 0.5492424242424241987, 0.5530303030303029832, 0.5568181818181817677, 0.5606060606060605522, 0.5643939393939394478, 0.5681818181818182323, 0.5719696969696970168, 0.5757575757575758013, 0.5795454545454545858, 0.5833333333333333703, 0.5871212121212121549, 0.5909090909090909394, 0.5946969696969697239, 0.5984848484848485084, 0.6022727272727272929, 0.6060606060606060774, 0.6098484848484848619, 0.6136363636363636465, 0.6174242424242424310, 0.6212121212121212155, 0.6250000000000000000, 0.6287878787878787845, 0.6325757575757575690, 0.6363636363636363535, 0.6401515151515151381, 0.6439393939393939226, 0.6477272727272727071, 0.6515151515151514916, 0.6553030303030302761, 0.6590909090909090606, 0.6628787878787878451, 0.6666666666666666297, 0.6704545454545454142, 0.6742424242424241987, 0.6780303030303029832, 0.6818181818181817677, 0.6856060606060605522, 0.6893939393939394478, 0.6931818181818182323, 0.6969696969696970168, 0.7007575757575758013, 0.7045454545454545858, 0.7083333333333333703, 0.7121212121212121549, 0.7159090909090909394, 0.7196969696969697239, 0.7234848484848485084, 0.7272727272727272929, 0.7310606060606060774, 0.7348484848484848619, 0.7386363636363636465, 0.7424242424242424310, 0.7462121212121212155, 0.7500000000000000000, 0.7537878787878787845, 0.7575757575757575690, 0.7613636363636363535, 0.7651515151515151381, 0.7689393939393939226, 0.7727272727272727071, 0.7765151515151514916, 0.7803030303030302761, 0.7840909090909090606, 0.7878787878787878451, 0.7916666666666666297, 0.7954545454545454142, 0.7992424242424241987, 0.8030303030303029832, 0.8068181818181817677, 0.8106060606060605522, 0.8143939393939394478, 0.8181818181818182323, 0.8219696969696970168, 0.8257575757575758013, 0.8295454545454545858, 0.8333333333333333703, 0.8371212121212121549, 0.8409090909090909394, 0.8446969696969697239, 0.8484848484848485084, 0.8522727272727272929, 0.8560606060606060774, 0.8598484848484848619, 0.8636363636363636465, 0.8674242424242424310, 0.8712121212121212155, 0.8750000000000000000, 0.8787878787878787845, 0.8825757575757575690, 0.8863636363636363535, 0.8901515151515151381, 0.8939393939393939226, 0.8977272727272727071, 0.9015151515151514916, 0.9053030303030302761, 0.9090909090909090606, 0.9128787878787878451, 0.9166666666666666297, 0.9204545454545454142, 0.9242424242424241987, 0.9280303030303029832, 0.9318181818181817677, 0.9356060606060605522, 0.9393939393939394478, 0.9431818181818182323, 0.9469696969696970168, 0.9507575757575758013, 0.9545454545454545858, 0.9583333333333333703, 0.9621212121212121549, 0.9659090909090909394 ),
 .UNSPECIFIED. ) 
 GEOMETRIC_REPRESENTATION_ITEM ( )  RATIONAL_B_SPLINE_SURFACE ( (
 ( 1.000000000000000000, 0.9659258262890683122, 1.000000000000000000, 0.9659258262890683122, 1.000000000000000000, 0.9659258262890683122, 1.000000000000000000, 0.9659258262890683122, 1.000000000000000000, 0.9659258262890683122, 1.000000000000000000, 0.9659258262890683122, 1.000000000000000000, 0.9659258262890683122, 1.000000000000000000, 0.9659258262890683122, 1.000000000000000000, 0.9659258262890683122, 1.000000000000000000, 0.9659258262890683122, 1.000000000000000000, 0.9659258262890683122, 1.000000000000000000, 0.9659258262890683122, 1.000000000000000000, 0.9659258262890683122, 1.000000000000000000, 0.9659258262890683122, 1.000000000000000000, 0.9659258262890683122, 1.000000000000000000, 0.9659258262890683122, 1.000000000000000000, 0.9659258262890683122, 1.000000000000000000, 0.9659258262890683122, 1.000000000000000000, 0.9659258262890683122, 1.000000000000000000, 0.9659258262890683122, 1.000000000000000000, 0.9659258262890683122, 1.000000000000000000, 0.9659258262890683122, 1.000000000000000000, 0.9659258262890683122, 1.000000000000000000, 0.9659258262890683122, 1.000000000000000000, 0.9659258262890683122, 1.000000000000000000, 0.9659258262890683122, 1.000000000000000000, 0.9659258262890683122, 1.000000000000000000, 0.9659258262890683122, 1.000000000000000000, 0.9659258262890683122, 1.000000000000000000, 0.9659258262890683122, 1.000000000000000000, 0.9659258262890683122, 1.000000000000000000, 0.9659258262890683122, 1.000000000000000000, 0.9659258262890683122, 1.000000000000000000, 0.9659258262890683122, 1.000000000000000000, 0.9659258262890683122, 1.000000000000000000, 0.9659258262890683122, 1.000000000000000000, 0.9659258262890683122, 1.000000000000000000, 0.9659258262890683122, 1.000000000000000000, 0.9659258262890683122, 1.000000000000000000, 0.9659258262890683122, 1.000000000000000000, 0.9659258262890683122, 1.000000000000000000, 0.9659258262890683122, 1.000000000000000000, 0.9659258262890683122, 1.000000000000000000, 0.9659258262890683122, 1.000000000000000000, 0.9659258262890683122, 1.000000000000000000, 0.9659258262890683122, 1.000000000000000000, 0.9659258262890683122, 1.000000000000000000, 0.9659258262890683122, 1.000000000000000000, 0.9659258262890683122, 1.000000000000000000, 0.9659258262890683122, 1.000000000000000000, 0.9659258262890683122, 1.000000000000000000, 0.9659258262890683122, 1.000000000000000000, 0.9659258262890683122, 1.000000000000000000, 0.9659258262890683122, 1.000000000000000000, 0.9659258262890683122, 1.000000000000000000, 0.9659258262890683122, 1.000000000000000000, 0.9659258262890683122, 1.000000000000000000, 0.9659258262890683122, 1.000000000000000000, 0.9659258262890683122, 1.000000000000000000, 0.9659258262890683122, 1.000000000000000000, 0.9659258262890683122, 1.000000000000000000, 0.9659258262890683122, 1.000000000000000000, 0.9659258262890683122, 1.000000000000000000, 0.9659258262890683122, 1.000000000000000000, 0.9659258262890683122, 1.000000000000000000, 0.9659258262890683122, 1.000000000000000000, 0.9659258262890683122, 1.000000000000000000, 0.9659258262890683122, 1.000000000000000000, 0.9659258262890683122, 1.000000000000000000, 0.9659258262890683122, 1.000000000000000000, 0.9659258262890683122, 1.000000000000000000, 0.9659258262890683122, 1.000000000000000000, 0.9659258262890683122, 1.000000000000000000, 0.9659258262890683122, 1.000000000000000000, 0.9659258262890683122, 1.000000000000000000, 0.9659258262890683122, 1.000000000000000000, 0.9659258262890683122, 1.000000000000000000, 0.9659258262890683122, 1.000000000000000000, 0.9659258262890683122, 1.000000000000000000, 0.9659258262890683122, 1.000000000000000000, 0.9659258262890683122, 1.000000000000000000, 0.9659258262890683122, 1.000000000000000000, 0.9659258262890683122, 1.000000000000000000, 0.9659258262890683122, 1.000000000000000000, 0.9659258262890683122, 1.000000000000000000, 0.9659258262890683122, 1.000000000000000000, 0.9659258262890683122, 1.000000000000000000, 0.9659258262890683122, 1.000000000000000000, 0.9659258262890683122, 1.000000000000000000, 0.9659258262890683122, 1.000000000000000000, 0.9659258262890683122, 1.000000000000000000, 0.9659258262890683122, 1.000000000000000000, 0.9659258262890683122, 1.000000000000000000, 0.9659258262890683122, 1.000000000000000000, 0.9659258262890683122, 1.000000000000000000, 0.9659258262890683122, 1.000000000000000000, 0.9659258262890683122, 1.000000000000000000, 0.9659258262890683122, 1.000000000000000000, 0.9659258262890683122, 1.000000000000000000, 0.9659258262890683122, 1.000000000000000000, 0.9659258262890683122, 1.000000000000000000, 0.9659258262890683122, 1.000000000000000000, 0.9659258262890683122, 1.000000000000000000, 0.9659258262890683122, 1.000000000000000000, 0.9659258262890683122, 1.000000000000000000, 0.9659258262890683122, 1.000000000000000000, 0.9659258262890683122, 1.000000000000000000, 0.9659258262890683122, 1.000000000000000000, 0.9659258262890683122, 1.000000000000000000, 0.9659258262890683122, 1.000000000000000000, 0.9659258262890683122, 1.000000000000000000, 0.9659258262890683122, 1.000000000000000000, 0.9659258262890683122, 1.000000000000000000, 0.9659258262890683122, 1.000000000000000000, 0.9659258262890683122, 1.000000000000000000, 0.9659258262890683122, 1.000000000000000000, 0.9659258262890683122, 1.000000000000000000, 0.9659258262890683122, 1.000000000000000000, 0.9659258262890683122, 1.000000000000000000, 0.9659258262890683122, 1.000000000000000000, 0.9659258262890683122, 1.000000000000000000, 0.9659258262890683122, 1.000000000000000000, 0.9659258262890683122, 1.000000000000000000, 0.9659258262890683122, 1.000000000000000000, 0.9659258262890683122, 1.000000000000000000, 0.9659258262890683122, 1.000000000000000000, 0.9659258262890683122, 1.000000000000000000, 0.9659258262890683122, 1.000000000000000000, 0.9659258262890683122, 1.000000000000000000, 0.9659258262890683122, 1.000000000000000000, 0.9659258262890683122, 1.000000000000000000, 0.9659258262890683122, 1.000000000000000000, 0.9659258262890683122, 1.000000000000000000, 0.9659258262890683122, 1.000000000000000000, 0.9659258262890683122, 1.000000000000000000, 0.9659258262890683122, 1.000000000000000000, 0.9659258262890683122, 1.000000000000000000, 0.9659258262890683122, 1.000000000000000000, 0.9659258262890683122, 1.000000000000000000, 0.9659258262890683122, 1.000000000000000000, 0.9659258262890683122, 1.000000000000000000, 0.9659258262890683122, 1.000000000000000000, 0.9659258262890683122, 1.000000000000000000, 0.9659258262890683122, 1.000000000000000000, 0.9659258262890683122, 1.000000000000000000, 0.9659258262890683122, 1.000000000000000000, 0.9659258262890683122, 1.000000000000000000, 0.9659258262890683122, 1.000000000000000000, 0.9659258262890683122, 1.000000000000000000, 0.9659258262890683122, 1.000000000000000000, 0.9659258262890683122, 1.000000000000000000, 0.9659258262890683122, 1.000000000000000000, 0.9659258262890683122, 1.000000000000000000, 0.9659258262890683122, 1.000000000000000000, 0.9659258262890683122, 1.000000000000000000, 0.9659258262890683122, 1.000000000000000000, 0.9659258262890683122, 1.000000000000000000, 0.9659258262890683122, 1.000000000000000000, 0.9659258262890683122, 1.000000000000000000, 0.9659258262890683122, 1.000000000000000000, 0.9659258262890683122, 1.000000000000000000, 0.9659258262890683122, 1.000000000000000000, 0.9659258262890683122, 1.000000000000000000, 0.9659258262890683122, 1.000000000000000000, 0.9659258262890683122, 1.000000000000000000, 0.9659258262890683122, 1.000000000000000000, 0.9659258262890683122, 1.000000000000000000, 0.9659258262890683122, 1.000000000000000000, 0.9659258262890683122, 1.000000000000000000, 0.9659258262890683122, 1.000000000000000000, 0.9659258262890683122, 1.000000000000000000, 0.9659258262890683122, 1.000000000000000000, 0.9659258262890683122, 1.000000000000000000, 0.9659258262890683122, 1.000000000000000000, 0.9659258262890683122, 1.000000000000000000, 0.9659258262890683122, 1.000000000000000000, 0.9659258262890683122, 1.000000000000000000, 0.9659258262890683122, 1.000000000000000000, 0.9659258262890683122, 1.000000000000000000, 0.9659258262890683122, 1.000000000000000000, 0.9659258262890683122, 1.000000000000000000, 0.9659258262890683122, 1.000000000000000000, 0.9659258262890683122, 1.000000000000000000, 0.9659258262890683122, 1.000000000000000000, 0.9659258262890683122, 1.000000000000000000, 0.9659258262890683122, 1.000000000000000000, 0.9659258262890683122, 1.000000000000000000, 0.9659258262890683122, 1.000000000000000000, 0.9659258262890683122, 1.000000000000000000, 0.9659258262890683122, 1.000000000000000000, 0.9659258262890683122, 1.000000000000000000, 0.9659258262890683122, 1.000000000000000000, 0.9659258262890683122, 1.000000000000000000, 0.9659258262890683122, 1.000000000000000000, 0.9659258262890683122, 1.000000000000000000, 0.9659258262890683122, 1.000000000000000000, 0.9659258262890683122, 1.000000000000000000, 0.9659258262890683122, 1.000000000000000000, 0.9659258262890683122, 1.000000000000000000, 0.9659258262890683122, 1.000000000000000000, 0.9659258262890683122, 1.000000000000000000, 0.9659258262890683122, 1.000000000000000000, 0.9659258262890683122, 1.000000000000000000, 0.9659258262890683122, 1.000000000000000000, 0.9659258262890683122, 1.000000000000000000, 0.9659258262890683122, 1.000000000000000000, 0.9659258262890683122, 1.000000000000000000, 0.9659258262890683122, 1.000000000000000000, 0.9659258262890683122, 1.000000000000000000, 0.9659258262890683122, 1.000000000000000000, 0.9659258262890683122, 1.000000000000000000, 0.9659258262890683122, 1.000000000000000000, 0.9659258262890683122, 1.000000000000000000, 0.9659258262890683122, 1.000000000000000000, 0.9659258262890683122, 1.000000000000000000, 0.9659258262890683122, 1.000000000000000000, 0.9659258262890683122, 1.000000000000000000, 0.9659258262890683122, 1.000000000000000000, 0.9659258262890683122, 1.000000000000000000, 0.9659258262890683122, 1.000000000000000000, 0.9659258262890683122, 1.000000000000000000, 0.9659258262890683122, 1.000000000000000000, 0.9659258262890683122, 1.000000000000000000, 0.9659258262890683122, 1.000000000000000000, 0.9659258262890683122, 1.000000000000000000, 0.9659258262890683122, 1.000000000000000000, 0.9659258262890683122, 1.000000000000000000, 0.9659258262890683122, 1.000000000000000000, 0.9659258262890683122, 1.000000000000000000, 0.9659258262890683122, 1.000000000000000000, 0.9659258262890683122, 1.000000000000000000, 0.9659258262890683122, 1.000000000000000000, 0.9659258262890683122, 1.000000000000000000, 0.9659258262890683122, 1.000000000000000000, 0.9659258262890683122, 1.000000000000000000, 0.9659258262890683122, 1.000000000000000000, 0.9659258262890683122, 1.000000000000000000, 0.9659258262890683122, 1.000000000000000000, 0.9659258262890683122, 1.000000000000000000, 0.9659258262890683122, 1.000000000000000000, 0.9659258262890683122, 1.000000000000000000, 0.9659258262890683122, 1.000000000000000000, 0.9659258262890683122, 1.000000000000000000, 0.9659258262890683122, 1.000000000000000000, 0.9659258262890683122, 1.000000000000000000, 0.9659258262890683122, 1.000000000000000000, 0.9659258262890683122, 1.000000000000000000, 0.9659258262890683122, 1.000000000000000000, 0.9659258262890683122, 1.000000000000000000, 0.9659258262890683122, 1.000000000000000000, 0.9659258262890683122, 1.000000000000000000, 0.9659258262890683122, 1.000000000000000000, 0.9659258262890683122, 1.000000000000000000, 0.9659258262890683122, 1.000000000000000000, 0.9659258262890683122, 1.000000000000000000),
 ( 1.000000000000000000, 0.9659258262890683122, 1.000000000000000000, 0.9659258262890683122, 1.000000000000000000, 0.9659258262890683122, 1.000000000000000000, 0.9659258262890683122, 1.000000000000000000, 0.9659258262890683122, 1.000000000000000000, 0.9659258262890683122, 1.000000000000000000, 0.9659258262890683122, 1.000000000000000000, 0.9659258262890683122, 1.000000000000000000, 0.9659258262890683122, 1.000000000000000000, 0.9659258262890683122, 1.000000000000000000, 0.9659258262890683122, 1.000000000000000000, 0.9659258262890683122, 1.000000000000000000, 0.9659258262890683122, 1.000000000000000000, 0.9659258262890683122, 1.000000000000000000, 0.9659258262890683122, 1.000000000000000000, 0.9659258262890683122, 1.000000000000000000, 0.9659258262890683122, 1.000000000000000000, 0.9659258262890683122, 1.000000000000000000, 0.9659258262890683122, 1.000000000000000000, 0.9659258262890683122, 1.000000000000000000, 0.9659258262890683122, 1.000000000000000000, 0.9659258262890683122, 1.000000000000000000, 0.9659258262890683122, 1.000000000000000000, 0.9659258262890683122, 1.000000000000000000, 0.9659258262890683122, 1.000000000000000000, 0.9659258262890683122, 1.000000000000000000, 0.9659258262890683122, 1.000000000000000000, 0.9659258262890683122, 1.000000000000000000, 0.9659258262890683122, 1.000000000000000000, 0.9659258262890683122, 1.000000000000000000, 0.9659258262890683122, 1.000000000000000000, 0.9659258262890683122, 1.000000000000000000, 0.9659258262890683122, 1.000000000000000000, 0.9659258262890683122, 1.000000000000000000, 0.9659258262890683122, 1.000000000000000000, 0.9659258262890683122, 1.000000000000000000, 0.9659258262890683122, 1.000000000000000000, 0.9659258262890683122, 1.000000000000000000, 0.9659258262890683122, 1.000000000000000000, 0.9659258262890683122, 1.000000000000000000, 0.9659258262890683122, 1.000000000000000000, 0.9659258262890683122, 1.000000000000000000, 0.9659258262890683122, 1.000000000000000000, 0.9659258262890683122, 1.000000000000000000, 0.9659258262890683122, 1.000000000000000000, 0.9659258262890683122, 1.000000000000000000, 0.9659258262890683122, 1.000000000000000000, 0.9659258262890683122, 1.000000000000000000, 0.9659258262890683122, 1.000000000000000000, 0.9659258262890683122, 1.000000000000000000, 0.9659258262890683122, 1.000000000000000000, 0.9659258262890683122, 1.000000000000000000, 0.9659258262890683122, 1.000000000000000000, 0.9659258262890683122, 1.000000000000000000, 0.9659258262890683122, 1.000000000000000000, 0.9659258262890683122, 1.000000000000000000, 0.9659258262890683122, 1.000000000000000000, 0.9659258262890683122, 1.000000000000000000, 0.9659258262890683122, 1.000000000000000000, 0.9659258262890683122, 1.000000000000000000, 0.9659258262890683122, 1.000000000000000000, 0.9659258262890683122, 1.000000000000000000, 0.9659258262890683122, 1.000000000000000000, 0.9659258262890683122, 1.000000000000000000, 0.9659258262890683122, 1.000000000000000000, 0.9659258262890683122, 1.000000000000000000, 0.9659258262890683122, 1.000000000000000000, 0.9659258262890683122, 1.000000000000000000, 0.9659258262890683122, 1.000000000000000000, 0.9659258262890683122, 1.000000000000000000, 0.9659258262890683122, 1.000000000000000000, 0.9659258262890683122, 1.000000000000000000, 0.9659258262890683122, 1.000000000000000000, 0.9659258262890683122, 1.000000000000000000, 0.9659258262890683122, 1.000000000000000000, 0.9659258262890683122, 1.000000000000000000, 0.9659258262890683122, 1.000000000000000000, 0.9659258262890683122, 1.000000000000000000, 0.9659258262890683122, 1.000000000000000000, 0.9659258262890683122, 1.000000000000000000, 0.9659258262890683122, 1.000000000000000000, 0.9659258262890683122, 1.000000000000000000, 0.9659258262890683122, 1.000000000000000000, 0.9659258262890683122, 1.000000000000000000, 0.9659258262890683122, 1.000000000000000000, 0.9659258262890683122, 1.000000000000000000, 0.9659258262890683122, 1.000000000000000000, 0.9659258262890683122, 1.000000000000000000, 0.9659258262890683122, 1.000000000000000000, 0.9659258262890683122, 1.000000000000000000, 0.9659258262890683122, 1.000000000000000000, 0.9659258262890683122, 1.000000000000000000, 0.9659258262890683122, 1.000000000000000000, 0.9659258262890683122, 1.000000000000000000, 0.9659258262890683122, 1.000000000000000000, 0.9659258262890683122, 1.000000000000000000, 0.9659258262890683122, 1.000000000000000000, 0.9659258262890683122, 1.000000000000000000, 0.9659258262890683122, 1.000000000000000000, 0.9659258262890683122, 1.000000000000000000, 0.9659258262890683122, 1.000000000000000000, 0.9659258262890683122, 1.000000000000000000, 0.9659258262890683122, 1.000000000000000000, 0.9659258262890683122, 1.000000000000000000, 0.9659258262890683122, 1.000000000000000000, 0.9659258262890683122, 1.000000000000000000, 0.9659258262890683122, 1.000000000000000000, 0.9659258262890683122, 1.000000000000000000, 0.9659258262890683122, 1.000000000000000000, 0.9659258262890683122, 1.000000000000000000, 0.9659258262890683122, 1.000000000000000000, 0.9659258262890683122, 1.000000000000000000, 0.9659258262890683122, 1.000000000000000000, 0.9659258262890683122, 1.000000000000000000, 0.9659258262890683122, 1.000000000000000000, 0.9659258262890683122, 1.000000000000000000, 0.9659258262890683122, 1.000000000000000000, 0.9659258262890683122, 1.000000000000000000, 0.9659258262890683122, 1.000000000000000000, 0.9659258262890683122, 1.000000000000000000, 0.9659258262890683122, 1.000000000000000000, 0.9659258262890683122, 1.000000000000000000, 0.9659258262890683122, 1.000000000000000000, 0.9659258262890683122, 1.000000000000000000, 0.9659258262890683122, 1.000000000000000000, 0.9659258262890683122, 1.000000000000000000, 0.9659258262890683122, 1.000000000000000000, 0.9659258262890683122, 1.000000000000000000, 0.9659258262890683122, 1.000000000000000000, 0.9659258262890683122, 1.000000000000000000, 0.9659258262890683122, 1.000000000000000000, 0.9659258262890683122, 1.000000000000000000, 0.9659258262890683122, 1.000000000000000000, 0.9659258262890683122, 1.000000000000000000, 0.9659258262890683122, 1.000000000000000000, 0.9659258262890683122, 1.000000000000000000, 0.9659258262890683122, 1.000000000000000000, 0.9659258262890683122, 1.000000000000000000, 0.9659258262890683122, 1.000000000000000000, 0.9659258262890683122, 1.000000000000000000, 0.9659258262890683122, 1.000000000000000000, 0.9659258262890683122, 1.000000000000000000, 0.9659258262890683122, 1.000000000000000000, 0.9659258262890683122, 1.000000000000000000, 0.9659258262890683122, 1.000000000000000000, 0.9659258262890683122, 1.000000000000000000, 0.9659258262890683122, 1.000000000000000000, 0.9659258262890683122, 1.000000000000000000, 0.9659258262890683122, 1.000000000000000000, 0.9659258262890683122, 1.000000000000000000, 0.9659258262890683122, 1.000000000000000000, 0.9659258262890683122, 1.000000000000000000, 0.9659258262890683122, 1.000000000000000000, 0.9659258262890683122, 1.000000000000000000, 0.9659258262890683122, 1.000000000000000000, 0.9659258262890683122, 1.000000000000000000, 0.9659258262890683122, 1.000000000000000000, 0.9659258262890683122, 1.000000000000000000, 0.9659258262890683122, 1.000000000000000000, 0.9659258262890683122, 1.000000000000000000, 0.9659258262890683122, 1.000000000000000000, 0.9659258262890683122, 1.000000000000000000, 0.9659258262890683122, 1.000000000000000000, 0.9659258262890683122, 1.000000000000000000, 0.9659258262890683122, 1.000000000000000000, 0.9659258262890683122, 1.000000000000000000, 0.9659258262890683122, 1.000000000000000000, 0.9659258262890683122, 1.000000000000000000, 0.9659258262890683122, 1.000000000000000000, 0.9659258262890683122, 1.000000000000000000, 0.9659258262890683122, 1.000000000000000000, 0.9659258262890683122, 1.000000000000000000, 0.9659258262890683122, 1.000000000000000000, 0.9659258262890683122, 1.000000000000000000, 0.9659258262890683122, 1.000000000000000000, 0.9659258262890683122, 1.000000000000000000, 0.9659258262890683122, 1.000000000000000000, 0.9659258262890683122, 1.000000000000000000, 0.9659258262890683122, 1.000000000000000000, 0.9659258262890683122, 1.000000000000000000, 0.9659258262890683122, 1.000000000000000000, 0.9659258262890683122, 1.000000000000000000, 0.9659258262890683122, 1.000000000000000000, 0.9659258262890683122, 1.000000000000000000, 0.9659258262890683122, 1.000000000000000000, 0.9659258262890683122, 1.000000000000000000, 0.9659258262890683122, 1.000000000000000000, 0.9659258262890683122, 1.000000000000000000, 0.9659258262890683122, 1.000000000000000000, 0.9659258262890683122, 1.000000000000000000, 0.9659258262890683122, 1.000000000000000000, 0.9659258262890683122, 1.000000000000000000, 0.9659258262890683122, 1.000000000000000000, 0.9659258262890683122, 1.000000000000000000, 0.9659258262890683122, 1.000000000000000000, 0.9659258262890683122, 1.000000000000000000, 0.9659258262890683122, 1.000000000000000000, 0.9659258262890683122, 1.000000000000000000, 0.9659258262890683122, 1.000000000000000000, 0.9659258262890683122, 1.000000000000000000, 0.9659258262890683122, 1.000000000000000000, 0.9659258262890683122, 1.000000000000000000, 0.9659258262890683122, 1.000000000000000000, 0.9659258262890683122, 1.000000000000000000, 0.9659258262890683122, 1.000000000000000000, 0.9659258262890683122, 1.000000000000000000, 0.9659258262890683122, 1.000000000000000000, 0.9659258262890683122, 1.000000000000000000, 0.9659258262890683122, 1.000000000000000000, 0.9659258262890683122, 1.000000000000000000, 0.9659258262890683122, 1.000000000000000000, 0.9659258262890683122, 1.000000000000000000, 0.9659258262890683122, 1.000000000000000000, 0.9659258262890683122, 1.000000000000000000, 0.9659258262890683122, 1.000000000000000000, 0.9659258262890683122, 1.000000000000000000, 0.9659258262890683122, 1.000000000000000000, 0.9659258262890683122, 1.000000000000000000, 0.9659258262890683122, 1.000000000000000000, 0.9659258262890683122, 1.000000000000000000, 0.9659258262890683122, 1.000000000000000000, 0.9659258262890683122, 1.000000000000000000, 0.9659258262890683122, 1.000000000000000000, 0.9659258262890683122, 1.000000000000000000, 0.9659258262890683122, 1.000000000000000000, 0.9659258262890683122, 1.000000000000000000, 0.9659258262890683122, 1.000000000000000000, 0.9659258262890683122, 1.000000000000000000, 0.9659258262890683122, 1.000000000000000000, 0.9659258262890683122, 1.000000000000000000, 0.9659258262890683122, 1.000000000000000000, 0.9659258262890683122, 1.000000000000000000, 0.9659258262890683122, 1.000000000000000000, 0.9659258262890683122, 1.000000000000000000, 0.9659258262890683122, 1.000000000000000000, 0.9659258262890683122, 1.000000000000000000, 0.9659258262890683122, 1.000000000000000000, 0.9659258262890683122, 1.000000000000000000, 0.9659258262890683122, 1.000000000000000000, 0.9659258262890683122, 1.000000000000000000, 0.9659258262890683122, 1.000000000000000000, 0.9659258262890683122, 1.000000000000000000, 0.9659258262890683122, 1.000000000000000000, 0.9659258262890683122, 1.000000000000000000, 0.9659258262890683122, 1.000000000000000000, 0.9659258262890683122, 1.000000000000000000, 0.9659258262890683122, 1.000000000000000000, 0.9659258262890683122, 1.000000000000000000, 0.9659258262890683122, 1.000000000000000000, 0.9659258262890683122, 1.000000000000000000, 0.9659258262890683122, 1.000000000000000000, 0.9659258262890683122, 1.000000000000000000, 0.9659258262890683122, 1.000000000000000000, 0.9659258262890683122, 1.000000000000000000, 0.9659258262890683122, 1.000000000000000000) ) ) 
 REPRESENTATION_ITEM ( '' )  SURFACE ( )  );
#27287 = CARTESIAN_POINT ( 'NONE',  ( 0.3937007874015754361, -0.1870078740157479769, 0.4822834645669291653 ) ) ;
#27288 = CARTESIAN_POINT ( 'NONE',  ( -0.4002624671916004129, -0.3162353388693405765, 0.4822834645669290543 ) ) ;
#27289 = CARTESIAN_POINT ( 'NONE',  ( 0.3462931014723631407, 1.212771528347503347, -3.921763973690792326 ) ) ;
#27290 = CARTESIAN_POINT ( 'NONE',  ( 0.3996062992125986035, -0.1070741851644053111, -2.001312335958005395 ) ) ;
#27291 = CARTESIAN_POINT ( 'NONE',  ( 0.5971128608923890191, -0.5511811023622046335, 0.09757992244046803654 ) ) ;
#27292 = CARTESIAN_POINT ( 'NONE',  ( -0.2925321140481930704, -0.2925321140481933480, -1.791338582677165059 ) ) ;
#27293 = VERTEX_POINT ( 'NONE', #42835 ) ;
#27294 = CARTESIAN_POINT ( 'NONE',  ( -0.2867679344610367109, 0.2867679344610365444, -0.1739038302175346939 ) ) ;
#27295 = ORIENTED_EDGE ( 'NONE', *, *, #5901, .T. ) ;
#27296 = CARTESIAN_POINT ( 'NONE',  ( 0.1049868766404206816, -0.6046776061558809534, -0.2411417322834644161 ) ) ;
#27297 = CARTESIAN_POINT ( 'NONE',  ( 1.240157480314961314, -0.5400638737290844871, 0.3530559997133364547 ) ) ;
#27298 = CARTESIAN_POINT ( 'NONE',  ( 0.1115485564304470323, 0.2952755905511811885, 0.1292274648535926551 ) ) ;
#27299 = CARTESIAN_POINT ( 'NONE',  ( -0.2493438320209966919, -0.3690944881889763329, 0.3153832671262228327 ) ) ;
#27300 = CARTESIAN_POINT ( 'NONE',  ( 1.115485564304462551, -0.4281496062992127816, -0.4176697321401328100 ) ) ;
#27301 = CARTESIAN_POINT ( 'NONE',  ( -0.5314960629921250401, 0.1660481256975885056, 0.3530559997133364547 ) ) ;
#27302 = CARTESIAN_POINT ( 'NONE',  ( -0.1706036745406816491, -0.4281496062992124485, 0.4176697321401328655 ) ) ;
#27303 = CARTESIAN_POINT ( 'NONE',  ( -1.489501312335957062, -0.05778040916215522460, 0.4822834645669289988 ) ) ;
#27304 = CARTESIAN_POINT ( 'NONE',  ( 0.9580052493438326877, 0.05413385826771666132, 0.4176697321401328100 ) ) ;
#27305 = CARTESIAN_POINT ( 'NONE',  ( 1.213910761154856299, 0.2952755905511811885, 0.1292274648535926551 ) ) ;
#27306 = CARTESIAN_POINT ( 'NONE',  ( 0.2867679344610365999, 0.2867679344610365999, -0.7598425196850391306 ) ) ;
#27307 = CARTESIAN_POINT ( 'NONE',  ( 0.4002624671916016896, -0.08942795157527998196, 0.3641732283464567121 ) ) ;
#27308 = ORIENTED_EDGE ( 'NONE', *, *, #4102, .T. ) ;
#27309 = CARTESIAN_POINT ( 'NONE',  ( 0.2891555358219910499, 0.2891555358219910499, -0.4527559055118110520 ) ) ;
#27310 = VERTEX_POINT ( 'NONE', #35710 ) ;
#27311 = CARTESIAN_POINT ( 'NONE',  ( -0.6364829396325453192, -0.2845877964562159024, 0.3641732283464567677 ) ) ;
#27312 = CARTESIAN_POINT ( 'NONE',  ( 0.1443569553805781891, 0.05413385826771626580, -0.4176697321401330321 ) ) ;
#27313 = CARTESIAN_POINT ( 'NONE',  ( -1.504247987312398616, 1.133706091002348426, 0.2492029244898440743 ) ) ;
#27314 = CARTESIAN_POINT ( 'NONE',  ( -0.1968503937007867743, -0.6692913385826771977, 8.415575281601705876E-17 ) ) ;
#27315 = CARTESIAN_POINT ( 'NONE',  ( -0.08530183727034056085, -0.05778040916215560624, -0.4822834645669293319 ) ) ;
#27316 = CARTESIAN_POINT ( 'NONE',  ( -0.7086614173228339419, -0.1870078740157479769, 0.4822834645669291653 ) ) ;
#27317 = CARTESIAN_POINT ( 'NONE',  ( -1.122047244094487306, -0.5400638737290844871, 0.3530559997133364547 ) ) ;
#27318 = CARTESIAN_POINT ( 'NONE',  ( 1.502624671916010790, -0.08942795157527998196, 0.3641732283464567121 ) ) ;
#27319 = CYLINDRICAL_SURFACE ( 'NONE', #37176, 0.4724409448818898682 ) ;
#27320 = CARTESIAN_POINT ( 'NONE',  ( 0.9842519685039375910, 0.1771653543307087630, 0.000000000000000000 ) ) ;
#27321 = AXIS2_PLACEMENT_3D ( 'NONE', #80399, #29022, #28613 ) ;
#27322 = CARTESIAN_POINT ( 'NONE',  ( 0.6430446194225729606, -0.4281496062992127816, -0.4176697321401328100 ) ) ;
#27323 = CARTESIAN_POINT ( 'NONE',  ( 0.4265091863517067594, 0.2952755905511811885, 0.1292274648535926551 ) ) ;
#27324 = CARTESIAN_POINT ( 'NONE',  ( 0.1998031496062992740, 0.3460692066303959757, -1.089238845144356871 ) ) ;
#27325 = CARTESIAN_POINT ( 'NONE',  ( -2.630268417803885317, 1.724409448818897905, 0.4359958488159718093 ) ) ;
#27326 = CARTESIAN_POINT ( 'NONE',  ( -0.2925321140481932369, 0.2925321140481931259, -0.5688976377952755792 ) ) ;
#27327 = CARTESIAN_POINT ( 'NONE',  ( -0.2925321140481932369, 0.2925321140481931259, -0.5688976377952755792 ) ) ;
#27328 = CARTESIAN_POINT ( 'NONE',  ( -0.3543307086614165824, -0.6692913385826771977, 8.415575281601705876E-17 ) ) ;
#27329 = CARTESIAN_POINT ( 'NONE',  ( -0.4724409448818895907, -0.1265901696524993070, -0.2034120734908136108 ) ) ;
#27330 = CARTESIAN_POINT ( 'NONE',  ( 0.3917322834645670104, -0.1049643490035303411, -2.085958005249344271 ) ) ;
#27331 = CARTESIAN_POINT ( 'NONE',  ( -1.332020997375327642, -0.08942795157527998196, 0.3641732283464567121 ) ) ;
#27332 = CARTESIAN_POINT ( 'NONE',  ( 1.030183727034121421, -0.3162353388693409650, -0.4822834645669289433 ) ) ;
#27333 = CARTESIAN_POINT ( 'NONE',  ( 0.9186351706036752773, 0.2306618581243847221, -0.2411417322834647770 ) ) ;
#27334 = CARTESIAN_POINT ( 'NONE',  ( -0.2296587926509179312, -0.08942795157527998196, 0.3641732283464567121 ) ) ;
#27335 = CARTESIAN_POINT ( 'NONE',  ( 0.3149606299212603933, -0.1870078740157479769, 0.4822834645669291653 ) ) ;
#27336 = CARTESIAN_POINT ( 'NONE',  ( 0.3458507752293908943, 0.3458507752293908943, -1.789370078740157410 ) ) ;
#27337 = CARTESIAN_POINT ( 'NONE',  ( -0.2165354330708654795, 0.07958543189024085140, 0.2665933059059887866 ) ) ;
#27338 = B_SPLINE_CURVE_WITH_KNOTS ( 'NONE', 3,
 ( #52702, #33370, #40095, #27459, #40511, #66192, #8528 ),
 .UNSPECIFIED., .F., .F.,
 ( 4, 3, 4 ),
 ( 1.734723475976807094E-17, 0.001246230184515588870, 0.002492489877932651133 ),
 .UNSPECIFIED. ) ;
#27339 = CARTESIAN_POINT ( 'NONE',  ( -0.09186351706036689768, 0.05413385826771626580, -0.4176697321401330321 ) ) ;
#27340 = CIRCLE ( 'NONE', #19273, 0.1978346456692914035 ) ;
#27341 = CARTESIAN_POINT ( 'NONE',  ( 0.1974969037888704704, 0.3420746716998660508, -1.323490813648294129 ) ) ;
#27342 = CARTESIAN_POINT ( 'NONE',  ( -1.463254593175852492, -0.6692913385826773087, -0.1292274648535924053 ) ) ;
#27343 = CARTESIAN_POINT ( 'NONE',  ( 0.3937007874015754361, -0.1870078740157480601, -0.3641732283464567677 ) ) ;
#27344 = CARTESIAN_POINT ( 'NONE',  ( 1.423884514435696413, -0.2845877964562161244, -0.3641732283464567121 ) ) ;
#27345 = CARTESIAN_POINT ( 'NONE',  ( -0.9120734908136475250, 0.2952755905511811885, 0.1292274648535926551 ) ) ;
#27346 = CARTESIAN_POINT ( 'NONE',  ( -0.3674540682414689785, 0.1283753931104748280, 0.1820866141732283561 ) ) ;
#27347 = DIRECTION ( 'NONE',  ( 0.000000000000000000, -0.6427876096865352551, -0.7660444431189814551 ) ) ;
#27348 = CARTESIAN_POINT ( 'NONE',  ( -0.5708661417322828946, 0.1660481256975883668, -0.3530559997133364547 ) ) ;
#27349 = CARTESIAN_POINT ( 'NONE',  ( -0.5643044619422565855, -0.4281496062992124485, 0.4176697321401328655 ) ) ;
#27350 = CARTESIAN_POINT ( 'NONE',  ( -0.09842519685039295696, -0.5400638737290844871, 0.3530559997133364547 ) ) ;
#27351 = CARTESIAN_POINT ( 'NONE',  ( 0.3996062992125985480, 2.446882876249141654E-17, -2.714566929133858331 ) ) ;
#27352 = CARTESIAN_POINT ( 'NONE',  ( 0.3392501089628018329, -0.1958661417322834497, -1.917303518863830103 ) ) ;
#27353 = CARTESIAN_POINT ( 'NONE',  ( -1.686351706036744558, 0.1771653543307087075, -0.09757992244046823083 ) ) ;
#27354 = CARTESIAN_POINT ( 'NONE',  ( 0.6889763779527566800, -0.4536011799217367080, 0.2665933059059888421 ) ) ;
#27355 = CARTESIAN_POINT ( 'NONE',  ( 1.292650918635171564, 0.2952755905511811885, 0.1292274648535926551 ) ) ;
#27356 = CARTESIAN_POINT ( 'NONE',  ( -1.082677165354329896, 0.07958543189024085140, 0.2665933059059887866 ) ) ;
#27357 = CARTESIAN_POINT ( 'NONE',  ( -0.9580052493438311334, -0.3690944881889763329, 0.3153832671262228327 ) ) ;
#27358 = CARTESIAN_POINT ( 'NONE',  ( -0.4265091863517051496, 0.2952755905511810774, -0.1292274648535930714 ) ) ;
#27359 = CARTESIAN_POINT ( 'NONE',  ( 0.5380577427821529035, -0.3690944881889763329, 0.3153832671262228327 ) ) ;
#27360 = DIRECTION ( 'NONE',  ( 8.881784197001252323E-16, 0.000000000000000000, 1.000000000000000000 ) ) ;
#27361 = CARTESIAN_POINT ( 'NONE',  ( 0.9711286089238851948, 0.1283753931104748280, 0.1820866141732283561 ) ) ;
#27362 = CARTESIAN_POINT ( 'NONE',  ( 0.5052493438320218022, -0.6692913385826773087, -0.1292274648535924053 ) ) ;
#27363 = CARTESIAN_POINT ( 'NONE',  ( 0.2925321140481932369, 0.2925321140481932369, 0.1003937007874015769 ) ) ;
#27364 = CARTESIAN_POINT ( 'NONE',  ( -0.5905511811023615998, 0.2952755905511811885, 0.000000000000000000 ) ) ;
#27365 = CARTESIAN_POINT ( 'NONE',  ( -0.3392501089628019995, 0.1958661417322832277, -1.370734908136483021 ) ) ;
#27366 = CARTESIAN_POINT ( 'NONE',  ( 1.318897637795276356, 0.07958543189024071263, -0.2665933059059888421 ) ) ;
#27367 = CARTESIAN_POINT ( 'NONE',  ( 0.6036745406824154392, 0.2306618581243847221, -0.2411417322834647770 ) ) ;
#27368 = CARTESIAN_POINT ( 'NONE',  ( 0.1312335958005257930, 0.2306618581243847221, -0.2411417322834647770 ) ) ;
#27369 = CARTESIAN_POINT ( 'NONE',  ( 0.2099737532808405305, -0.5023911411419708095, 0.1820866141732285504 ) ) ;
#27370 = CARTESIAN_POINT ( 'NONE',  ( -1.646051170424378096, 0.000000000000000000, -0.3464511005275205946 ) ) ;
#27371 = CARTESIAN_POINT ( 'NONE',  ( -0.2034120734908128059, 0.1771653543307087630, 0.09757992244046791164 ) ) ;
#27372 = CARTESIAN_POINT ( 'NONE',  ( 0.6233595800524942554, -0.05778040916215560624, -0.4822834645669293319 ) ) ;
#27373 = CARTESIAN_POINT ( 'NONE',  ( -0.8005249343832013809, -0.3690944881889763329, 0.3153832671262228327 ) ) ;
#27374 = CARTESIAN_POINT ( 'NONE',  ( -0.3996062992125986590, 0.1070741851644051723, -0.8969816272965877024 ) ) ;
#27375 = CARTESIAN_POINT ( 'NONE',  ( -0.9776902887139098386, 0.2952755905511810774, -0.1292274648535930714 ) ) ;
#27376 = CARTESIAN_POINT ( 'NONE',  ( 0.1771653543307093459, 0.1012011053420777407, 0.2882089793578257453 ) ) ;
#27377 = VERTEX_POINT ( 'NONE', #28978 ) ;
#27378 = CARTESIAN_POINT ( 'NONE',  ( -1.351706036745406347, -0.4281496062992124485, 0.4176697321401328655 ) ) ;
#27379 = AXIS2_PLACEMENT_3D ( 'NONE', #34839, #54169, #9575 ) ;
#27380 = CARTESIAN_POINT ( 'NONE',  ( -0.9448818897637790704, -0.1870078740157479769, 0.3641732283464567677 ) ) ;
#27381 = CARTESIAN_POINT ( 'NONE',  ( 0.1443569553805781891, -0.4281496062992124485, 0.4176697321401328655 ) ) ;
#27382 = CARTESIAN_POINT ( 'NONE',  ( -1.653543307086613234, -0.1870078740157480879, -0.4822834645669291653 ) ) ;
#27383 = CARTESIAN_POINT ( 'NONE',  ( -0.6102362204724400829, -0.5400638737290845981, -0.3530559997133363437 ) ) ;
#27384 = CARTESIAN_POINT ( 'NONE',  ( 0.4470293165555208059, 1.696956328257586577, -2.112781292380983444 ) ) ;
#27386 = CARTESIAN_POINT ( 'NONE',  ( 0.8005249343832027131, 0.05413385826771666132, 0.4176697321401328100 ) ) ;
#27385 = CARTESIAN_POINT ( 'NONE',  ( 1.607611548556431069, -0.6692913385826773087, -0.1292274648535924053 ) ) ;
#27387 = CARTESIAN_POINT ( 'NONE',  ( 0.9908136482939640111, -0.6692913385826771977, 0.1292274648535927661 ) ) ;
#27388 = CARTESIAN_POINT ( 'NONE',  ( 0.2867679344610366554, 0.2867679344610366554, -2.492125984251968518 ) ) ;
#27389 = CARTESIAN_POINT ( 'NONE',  ( 1.535433070866142335, -0.6692913385826771977, 8.415575281601705876E-17 ) ) ;
#27390 = CARTESIAN_POINT ( 'NONE',  ( -1.377952755905511140, 0.2952755905511811885, 0.000000000000000000 ) ) ;
#27391 = CARTESIAN_POINT ( 'NONE',  ( 0.1998031496062994405, -0.3460692066303958092, -0.2493438320209974135 ) ) ;
#27392 = ORIENTED_EDGE ( 'NONE', *, *, #52169, .T. ) ;
#27393 = CARTESIAN_POINT ( 'NONE',  ( -0.6364829396325453192, -0.08942795157528024563, -0.3641732283464568787 ) ) ;
#27395 = CARTESIAN_POINT ( 'NONE',  ( -9.594673741351313045E-17, 0.3917322834645670104, -1.881889763779527769 ) ) ;
#27394 = AXIS2_PLACEMENT_3D ( 'NONE', #68971, #59238, #57977 ) ;
#27396 = ORIENTED_EDGE ( 'NONE', *, *, #64058, .F. ) ;
#27397 = CARTESIAN_POINT ( 'NONE',  ( 0.4593175853018379162, -0.4281496062992124485, 0.4176697321401328655 ) ) ;
#27398 = CARTESIAN_POINT ( 'NONE',  ( -0.08530183727034056085, -0.05778040916215560624, -0.4822834645669293319 ) ) ;
#27399 = CARTESIAN_POINT ( 'NONE',  ( -0.7808398950131222316, -0.3162353388693409650, -0.4822834645669289433 ) ) ;
#27400 = CARTESIAN_POINT ( 'NONE',  ( 1.391076115485564868, 0.2306618581243847221, -0.2411417322834647770 ) ) ;
#27401 = CARTESIAN_POINT ( 'NONE',  ( -0.9842519685039360366, 0.1771653543307087630, 0.000000000000000000 ) ) ;
#27402 = CARTESIAN_POINT ( 'NONE',  ( 0.4724409448818898682, 2.892866454678787531E-17, -2.084645669291338432 ) ) ;
#27403 = CARTESIAN_POINT ( 'NONE',  ( 0.6692913385826778638, -0.6692913385826771977, 8.415575281601705876E-17 ) ) ;
#27404 = CARTESIAN_POINT ( 'NONE',  ( 0.5183727034120741983, 0.1771653543307087075, -0.09757992244046823083 ) ) ;
#27405 = CARTESIAN_POINT ( 'NONE',  ( -0.2821522309711278487, -0.6692913385826773087, -0.1292274648535924053 ) ) ;
#27406 = CARTESIAN_POINT ( 'NONE',  ( -9.594673741351310580E-17, 0.3917322834645669549, -1.339875697341520455 ) ) ;
#27407 = CARTESIAN_POINT ( 'NONE',  ( -0.9580052493438311334, 0.05413385826771626580, -0.4176697321401330321 ) ) ;
#27408 = CARTESIAN_POINT ( 'NONE',  ( -1.666666666666665853, -0.004921259842519870586, -0.3153832671262229437 ) ) ;
#27409 = CARTESIAN_POINT ( 'NONE',  ( 1.437007874015748810, -0.5400638737290845981, -0.3530559997133363437 ) ) ;
#27410 = CARTESIAN_POINT ( 'NONE',  ( 1.548556430446194954, 0.1283753931104746893, -0.1820866141732285504 ) ) ;
#27411 = ORIENTED_EDGE ( 'NONE', *, *, #8016, .T. ) ;
#27412 = CARTESIAN_POINT ( 'NONE',  ( 0.3917322834645670659, 2.398668435337828261E-17, -2.634533751477377450 ) ) ;
#27413 = CARTESIAN_POINT ( 'NONE',  ( 8.195543980992789655E-16, -0.1870078740157480879, -0.4822834645669291653 ) ) ;
#27414 = ORIENTED_EDGE ( 'NONE', *, *, #49189, .F. ) ;
#27415 = CARTESIAN_POINT ( 'NONE',  ( -1.076115485564303809, 0.2306618581243848609, 0.2411417322834645549 ) ) ;
#27416 = CARTESIAN_POINT ( 'NONE',  ( 1.187664041994751285, -0.3162353388693409650, -0.4822834645669289433 ) ) ;
#27417 = CARTESIAN_POINT ( 'NONE',  ( 1.286089238845145033, 0.2306618581243848609, 0.2411417322834645549 ) ) ;
#27418 = CARTESIAN_POINT ( 'NONE',  ( 0.2034120734908142214, 0.2952755905511810774, -0.1292274648535930714 ) ) ;
#27419 = CARTESIAN_POINT ( 'NONE',  ( -0.4199475065616791736, -0.6046776061558807314, 0.2411417322834647770 ) ) ;
#27420 = CARTESIAN_POINT ( 'NONE',  ( -0.3392501089628019995, 0.1958661417322832277, -2.000656167979002920 ) ) ;
#27421 = CARTESIAN_POINT ( 'NONE',  ( -1.318897637795274802, -0.5400638737290845981, -0.3530559997133363437 ) ) ;
#27422 = CARTESIAN_POINT ( 'NONE',  ( -0.5971128608923877978, -0.6692913385826773087, -0.1292274648535924053 ) ) ;
#27423 = CARTESIAN_POINT ( 'NONE',  ( -0.4265091863517051496, -0.5511811023622046335, 0.09757992244046803654 ) ) ;
#27424 = CARTESIAN_POINT ( 'NONE',  ( 2.543486866223389153, 2.716535433070866645, -0.5314960629921260393 ) ) ;
#27425 = EDGE_CURVE ( 'NONE', #59512, #2851, #46203, .T. ) ;
#27426 = CARTESIAN_POINT ( 'NONE',  ( -0.4593175853018366950, 0.05413385826771666132, 0.4176697321401328100 ) ) ;
#27427 = CARTESIAN_POINT ( 'NONE',  ( -1.200787401574802349, 0.1660481256975883391, -0.3530559997133364547 ) ) ;
#27428 = CARTESIAN_POINT ( 'NONE',  ( 0.9186351706036751663, -0.6046776061558807314, 0.2411417322834647770 ) ) ;
#27429 = CARTESIAN_POINT ( 'NONE',  ( 0.3460692066303959757, -0.1998031496062991907, -1.994750656167979086 ) ) ;
#27430 = CARTESIAN_POINT ( 'NONE',  ( 3.908688349857626587, 1.475633291777086020, -0.4714062836140362478 ) ) ;
#27431 = EDGE_CURVE ( 'NONE', #60812, #21419, #24271, .T. ) ;
#27432 = CARTESIAN_POINT ( 'NONE',  ( -0.2821522309711278487, -0.6692913385826773087, -0.1292274648535924053 ) ) ;
#27434 = CARTESIAN_POINT ( 'NONE',  ( 0.6986524979670498681, 8.471767977567108961E-16, -0.4445507791589058955 ) ) ;
#27433 = CARTESIAN_POINT ( 'NONE',  ( 1.154855643044620184, -0.5023911411419708095, 0.1820866141732285504 ) ) ;
#27435 = CARTESIAN_POINT ( 'NONE',  ( -0.3458507752293906723, -0.3458507752293910609, -0.7657480314960628531 ) ) ;
#27436 = CARTESIAN_POINT ( 'NONE',  ( 1.167979002624672580, -0.3690944881889763329, 0.3153832671262228327 ) ) ;
#27437 = B_SPLINE_CURVE_WITH_KNOTS ( 'NONE', 3,
 ( #50980, #17391, #70355, #24902, #43022, #31637, #57297 ),
 .UNSPECIFIED., .F., .F.,
 ( 4, 3, 4 ),
 ( 5.204170427930421283E-18, 0.001246230184515576727, 0.002492489877932660240 ),
 .UNSPECIFIED. ) ;
#27438 = CARTESIAN_POINT ( 'NONE',  ( 1.207349081364829990, -0.6046776061558809534, -0.2411417322834644161 ) ) ;
#27439 = CARTESIAN_POINT ( 'NONE',  ( 0.2891555358219910499, 0.2891555358219910499, -0.05708661417322836301 ) ) ;
#27440 = CARTESIAN_POINT ( 'NONE',  ( -0.01312335958005186876, -0.4281496062992124485, 0.4176697321401328655 ) ) ;
#27441 = CARTESIAN_POINT ( 'NONE',  ( -0.7080320533160963103, 2.362204724409448620, -0.5309055118110235227 ) ) ;
#27442 = AXIS2_PLACEMENT_3D ( 'NONE', #13111, #12690, #82975 ) ;
#27443 = CARTESIAN_POINT ( 'NONE',  ( -1.430446194225721390, -0.4281496062992124485, 0.4176697321401328655 ) ) ;
#27444 = CARTESIAN_POINT ( 'NONE',  ( -0.08530183727034056085, -0.05778040916215560624, -0.4822834645669293319 ) ) ;
#27445 = CARTESIAN_POINT ( 'NONE',  ( -0.3420746716998662729, 0.1974969037888702206, -0.5754593175853018883 ) ) ;
#27446 = CARTESIAN_POINT ( 'NONE',  ( 1.181102362204725198, -0.1870078740157479769, 0.4822834645669291653 ) ) ;
#27447 = CARTESIAN_POINT ( 'NONE',  ( 0.5971128608923890191, -0.6692913385826771977, 0.1292274648535927661 ) ) ;
#27448 = CARTESIAN_POINT ( 'NONE',  ( 0.8661417322834653598, -0.1870078740157479769, 0.3641732283464567677 ) ) ;
#27449 = CARTESIAN_POINT ( 'NONE',  ( 0.3011055150036106021, 1.218137231435314272, 0.08579257120109930190 ) ) ;
#27450 = CARTESIAN_POINT ( 'NONE',  ( 0.5971128608923891301, 0.1771653543307087075, -0.09757992244046823083 ) ) ;
#27451 = CARTESIAN_POINT ( 'NONE',  ( -1.076115485564303809, -0.6046776061558809534, -0.2411417322834644161 ) ) ;
#27452 = CARTESIAN_POINT ( 'NONE',  ( -0.2925321140481930149, -0.2925321140481933480, -1.080708661417322691 ) ) ;
#27453 = CARTESIAN_POINT ( 'NONE',  ( 1.213910761154856299, 0.2952755905511811885, 0.1292274648535926551 ) ) ;
#27454 = EDGE_CURVE ( 'NONE', #53272, #8593, #3729, .T. ) ;
#27455 = CARTESIAN_POINT ( 'NONE',  ( -0.1958661417322836718, 0.3392501089628017219, -0.7926509186351704539 ) ) ;
#27456 = EDGE_CURVE ( 'NONE', #42276, #49776, #10047, .T. ) ;
#27458 = CARTESIAN_POINT ( 'NONE',  ( 0.9120734908136490793, 0.2952755905511810219, -0.1292274648535930437 ) ) ;
#27457 = CARTESIAN_POINT ( 'NONE',  ( 0.3543307086614181922, -0.6692913385826771977, 8.415575281601705876E-17 ) ) ;
#27459 = CARTESIAN_POINT ( 'NONE',  ( -0.7984992590978650107, -3.187520833735697382E-15, -0.3954974714151482384 ) ) ;
#27460 = CARTESIAN_POINT ( 'NONE',  ( 0.2690288713910767848, -0.5511811023622048555, -0.09757992244046775898 ) ) ;
#27461 = AXIS2_PLACEMENT_3D ( 'NONE', #23555, #29868, #5845 ) ;
#27462 = CARTESIAN_POINT ( 'NONE',  ( 0.3805774278215230400, -0.4281496062992124485, 0.4176697321401328655 ) ) ;
#27463 = CARTESIAN_POINT ( 'NONE',  ( -0.4602852883866647149, 1.653403552777526819, 2.138259192565361566 ) ) ;
#27464 = CARTESIAN_POINT ( 'NONE',  ( -0.8727034120734901146, -0.08942795157528024563, -0.3641732283464568787 ) ) ;
#27465 = CARTESIAN_POINT ( 'NONE',  ( -0.9711286089238838626, -0.6046776061558807314, 0.2411417322834647770 ) ) ;
#27466 = CARTESIAN_POINT ( 'NONE',  ( -1.640419947506561060, -0.4281496062992127816, -0.4176697321401328100 ) ) ;
#27467 = CARTESIAN_POINT ( 'NONE',  ( 0.4396325459317593221, 0.2952755905511810774, -0.1292274648535930714 ) ) ;
#27468 = CARTESIAN_POINT ( 'NONE',  ( -1.640419947506561060, -0.004921259842519576551, 0.3153832671262227771 ) ) ;
#27469 = DIRECTION ( 'NONE',  ( 0.000000000000000000, 0.000000000000000000, -1.000000000000000000 ) ) ;
#27470 = CARTESIAN_POINT ( 'NONE',  ( 0.5708661417322841158, -0.5400638737290845981, -0.3530559997133363437 ) ) ;
#27471 = CARTESIAN_POINT ( 'NONE',  ( 0.2925321140481932369, 0.2925321140481932369, 0.1003937007874015491 ) ) ;
#27472 = CARTESIAN_POINT ( 'NONE',  ( 1.561679790026247350, 0.05413385826771626580, -0.4176697321401330321 ) ) ;
#27473 = CARTESIAN_POINT ( 'NONE',  ( 1.272965879265092637, -0.4281496062992127816, -0.4176697321401328100 ) ) ;
#27474 = CARTESIAN_POINT ( 'NONE',  ( -1.410761154855642463, -0.08942795157527998196, 0.3641732283464567121 ) ) ;
#27475 = CARTESIAN_POINT ( 'NONE',  ( 1.292650918635171564, -0.5511811023622048555, -0.09757992244046775898 ) ) ;
#27476 = CARTESIAN_POINT ( 'NONE',  ( -1.463254593175852492, 0.1771653543307087630, 0.09757992244046791164 ) ) ;
#27477 = CARTESIAN_POINT ( 'NONE',  ( -0.7742782152230962556, -0.3690944881889765550, -0.3153832671262227771 ) ) ;
#27478 = CARTESIAN_POINT ( 'NONE',  ( 1.568241469816273437, -0.3162353388693405765, 0.4822834645669290543 ) ) ;
#27479 = CARTESIAN_POINT ( 'NONE',  ( 0.4724409448818904789, -0.1870078740157479769, 0.3641732283464567677 ) ) ;
#27480 = CARTESIAN_POINT ( 'NONE',  ( 0.6167979002624679463, 0.05413385826771626580, -0.4176697321401330321 ) ) ;
#27481 = CARTESIAN_POINT ( 'NONE',  ( 1.286089238845145033, 0.2306618581243848609, 0.2411417322834645549 ) ) ;
#27482 = CARTESIAN_POINT ( 'NONE',  ( 0.1049868766404206816, 0.2306618581243848609, 0.2411417322834645549 ) ) ;
#27483 = CARTESIAN_POINT ( 'NONE',  ( 0.3543307086614179147, 0.1771653543307087630, 0.000000000000000000 ) ) ;
#27484 = CARTESIAN_POINT ( 'NONE',  ( 1.371391076115485719, -0.6692913385826773087, -0.1292274648535924053 ) ) ;
#27485 = CARTESIAN_POINT ( 'NONE',  ( -1.568241469816272105, -0.3162353388693409650, -0.4822834645669289433 ) ) ;
#27486 = CARTESIAN_POINT ( 'NONE',  ( -0.8005249343832013809, -0.4281496062992124485, 0.4176697321401328655 ) ) ;
#27487 = CARTESIAN_POINT ( 'NONE',  ( 0.3996062992125986035, -0.1070741851644053111, -0.7414698162729659314 ) ) ;
#27488 = DIRECTION ( 'NONE',  ( -1.000000000000000000, -3.050063254464715288E-16, 0.000000000000000000 ) ) ;
#27489 = CARTESIAN_POINT ( 'NONE',  ( -0.03280839895013062252, -0.6692913385826771977, 0.1292274648535927661 ) ) ;
#27490 = CARTESIAN_POINT ( 'NONE',  ( -0.7611548556430438595, -0.6046776061558809534, -0.2411417322834644161 ) ) ;
#27491 = ADVANCED_FACE ( 'NONE', ( #10869 ), #47112, .F. ) ;
#27492 = CARTESIAN_POINT ( 'NONE',  ( -0.1574803149606292529, -0.1870078740157479769, 0.4822834645669291653 ) ) ;
#27493 = CARTESIAN_POINT ( 'NONE',  ( 0.1070741851644054915, -0.3996062992125986035, -2.447506561679789527 ) ) ;
#27494 = CARTESIAN_POINT ( 'NONE',  ( 0.3949938075777411073, -0.1058382717557499464, -1.843832020997375309 ) ) ;
#27495 = CARTESIAN_POINT ( 'NONE',  ( 0.3392501089628018884, -0.1958661417322834220, -0.4120734908136482466 ) ) ;
#27496 = AXIS2_PLACEMENT_3D ( 'NONE', #32485, #40066, #34165 ) ;
#27497 = CARTESIAN_POINT ( 'NONE',  ( 0.4177787735906991484, 1.312623414240987163, -1.404325600637324367 ) ) ;
#27498 = CARTESIAN_POINT ( 'NONE',  ( -1.417322834645668772, -0.1870078740157479769, 0.3641732283464567677 ) ) ;
#27499 = CARTESIAN_POINT ( 'NONE',  ( -0.3917322834645671215, 0.1049643490035301469, -1.127296587926509108 ) ) ;
#27500 = CARTESIAN_POINT ( 'NONE',  ( -1.450131233595799651, -0.6692913385826771977, 0.1292274648535927661 ) ) ;
#27501 = CARTESIAN_POINT ( 'NONE',  ( 0.3917322834645668994, 0.1049643490035304522, -0.04722477870634988334 ) ) ;
#27502 = EDGE_CURVE ( 'NONE', #59098, #47997, #54811, .T. ) ;
#27503 = CARTESIAN_POINT ( 'NONE',  ( 0.4461942257217856311, 0.2306618581243847221, -0.2411417322834647770 ) ) ;
#27504 = CARTESIAN_POINT ( 'NONE',  ( -0.6036745406824141069, 0.1283753931104748280, 0.1820866141732283561 ) ) ;
#27505 = CARTESIAN_POINT ( 'NONE',  ( 0.7217847769028878924, -0.4281496062992127816, -0.4176697321401328100 ) ) ;
#27506 = CARTESIAN_POINT ( 'NONE',  ( 0.1640419947506569498, -0.05778040916215522460, 0.4822834645669289988 ) ) ;
#27507 = CARTESIAN_POINT ( 'NONE',  ( 0.2899149735282853246, 1.161568142327694897, 1.084016376660781100 ) ) ;
#27508 = CARTESIAN_POINT ( 'NONE',  ( -0.2925321140481930704, -0.2925321140481933480, -2.421259842519684735 ) ) ;
#27509 = CARTESIAN_POINT ( 'NONE',  ( 0.3392501089628018329, 0.1958661417322835607, -1.072853961451130544 ) ) ;
#27510 = CARTESIAN_POINT ( 'NONE',  ( 1.095800524934383846, -0.05778040916215560624, -0.4822834645669293319 ) ) ;
#27511 = CARTESIAN_POINT ( 'NONE',  ( 0.1640419947506569498, -0.05778040916215522460, 0.4822834645669289988 ) ) ;
#27513 = CARTESIAN_POINT ( 'NONE',  ( 1.515748031496063186, -0.5400638737290845981, -0.3530559997133363437 ) ) ;
#27512 = VECTOR ( 'NONE', #76566, 39.37007874015748143 ) ;
#27514 = CARTESIAN_POINT ( 'NONE',  ( 0.8530183727034128527, -0.4281496062992124485, 0.4176697321401328655 ) ) ;
#27515 = CARTESIAN_POINT ( 'NONE',  ( -0.2867679344610365999, 0.2867679344610364889, -0.4192913385826772532 ) ) ;
#27516 = CARTESIAN_POINT ( 'NONE',  ( 0.2165354330708668673, 0.1660481256975883668, -0.3530559997133364547 ) ) ;
#27517 = CARTESIAN_POINT ( 'NONE',  ( 0.6496062992125991586, -0.5400638737290845981, -0.3530559997133363437 ) ) ;
#27518 = CARTESIAN_POINT ( 'NONE',  ( 0.1377952755905518800, 0.1660481256975883668, -0.3530559997133364547 ) ) ;
#27519 = CARTESIAN_POINT ( 'NONE',  ( 0.6364829396325465405, -0.2845877964562161244, -0.3641732283464567121 ) ) ;
#27520 = CARTESIAN_POINT ( 'NONE',  ( -1.233595800524933894, 0.2306618581243848609, 0.2411417322834645549 ) ) ;
#27521 = CARTESIAN_POINT ( 'NONE',  ( -1.541994750656167090, 0.2952755905511811885, 0.1292274648535926551 ) ) ;
#27522 = CARTESIAN_POINT ( 'NONE',  ( 0.6496062992125991586, 0.1660481256975885056, 0.3530559997133364547 ) ) ;
#27523 = CARTESIAN_POINT ( 'NONE',  ( -0.2417350488504524941, -0.3089825338629034746, -1.929133858267717772 ) ) ;
#27524 = CARTESIAN_POINT ( 'NONE',  ( -0.2867679344610364334, -0.2867679344610367109, -1.783464566929133577 ) ) ;
#27525 =( BOUNDED_SURFACE ( )  B_SPLINE_SURFACE ( 1, 2, ( 
 ( #56580, #57404, #76375, #63728, #25416, #64153, #69231, #18708, #70886, #50267, #63318, #6487, #56987, #82684, #12395, #5656, #62916, #56172, #11987, #57813, #75965, #11579, #83095, #180, #25833, #76778, #19110, #44350, #43947, #13235, #81875, #75556, #17895, #43532, #37238, #39725, #51916, #79295, #78041, #21203, #8577, #65831, #19956, #15314, #14899, #78463, #71717, #52755, #59081, #1849, #47273, #20788, #26680, #7323, #40559, #46444, #59495, #64988, #6901, #71300, #52335, #46858, #72552, #27928, #26257, #20371, #65418, #72135, #14493, #66240, #2263, #53586, #64564, #1436, #58234, #7754, #46023, #53167, #27092, #33829, #40146, #21613, #32572, #72963, #601, #77623, #14072, #45606, #8164, #13648, #34248, #27510, #39301, #78880, #32992, #59910, #58661, #1027, #33419, #16145, #80130, #80545, #29990, #74636, #75047, #2681, #60333, #61153, #3093, #29581, #61577, #15736, #28757, #60741, #74218, #73808, #41792, #36311, #8997, #35489, #16563, #34670, #10240, #42208, #3505, #67483, #79714, #41391, #55244, #29172, #40977, #22857, #35075, #28341, #54002, #55653, #80951, #3920, #9818, #22030, #10656, #66659, #47691, #54840, #73385, #35910, #67073, #48518, #9405, #81363, #23266, #67903, #16979, #48935, #42620, #54419, #68319, #23676, #22449, #48110, #61987, #4324, #49348, #44662, #63221, #44255, #50168, #75459, #17393, #82185, #82998, #37135, #24089, #12300, #12713, #57300, #50574, #82586, #37546, #69129, #5561, #62820, #70358, #25319, #17797, #50983, #75864, #4731, #32059, #30817, #76681, #38372, #18612, #56072, #51396, #19014, #6388, #64048, #43024, #62394, #36718, #31225, #5153, #5971, #37956, #43432, #56482, #24502, #76280, #18206, #43842, #57719, #68718, #11893, #69945, #11060, #63633, #31640, #56893, #69544, #81779, #11479, #82, #24905, #30405, #25735, #49759, #38789, #64466, #66147, #8075, #40055, #52241, #32474, #46769, #77100, #70787, #39631, #6803, #72043, #58136, #58991, #45508, #8484, #65742, #7659, #53074, #77945, #71622, #51819, #20274, #34153, #505, #931, #1756, #59398, #20697, #7226, #27413, #45924, #33738, #13548, #26997, #78785, #26158, #21110, #65321, #72461, #46348, #77524, #19859, #39204, #14810, #59814, #14399, #40469, #32898, #58565, #13974, #33329, #2169, #27835, #19432, #45083, #13138, #1347, #71205, #52660, #78366, #26588, #64887, #55145, #74538, #16884, #4227, #73712, #47180, #80034, #41296, #42112, #16052, #22760, #41698, #10559, #53496, #42522, #68225, #36217, #66981, #40880, #61061, #34572, #35811, #3412, #28246, #16467, #61886, #3825, #79205, #8895, #54745, #28664, #9314, #9725, #67809, #48013, #21521, #35396, #47597, #15220, #66562, #72872, #10146, #61477, #54325, #60239, #23168, #2587, #53906, #67391, #79620, #48422, #21937, #29074, #73291, #15639, #29486, #80450, #80856, #22353, #74121, #34984, #48837, #60648, #2998, #37036, #38990, #13337, #57925, #43328, #64673, #57512, #45297, #49662, #64259, #70993, #10960, #7012, #76888, #77307, #289, #36618, #55970, #75352, #19636, #13757, #51603, #32680, #69028, #11379, #83203, #31849, #25945, #58347, #26366, #55554, #708, #44867, #4633, #19218, #70566, #63837, #6174, #52025, #77731, #20060, #65098, #51190, #23578, #25525, #17700, #45713, #12921, #71410, #38578, #39414, #29891, #81263, #49249, #74952, #6593, #17298, #32264, #62296, #42925, #68620, #30304, #81683, #23994, #41086, #7435, #46136, #8688, #65936, #46552, #46966, #79826, #66775, #41501, #52440, #26784, #27619, #52863, #79403, #28036, #65527, #78573, #27199, #40665, #40253, #8272, #2792, #58772, #1957, #66349, #1134, #60024, #34358, #53282, #33937, #71830, #7859, #2379, #21722, #14180, #73076, #78993, #53694, #47385, #39838, #33524, #20899, #15425, #73504, #9108, #34781, #72250, #14599, #59602, #21313, #60440, #28451, #54111, #33105, #22142, #72660, #59187, #15008, #47800, #15852, #78151, #20482, #1545, #30522, #17909, #4028, #60850, #10356, #54947, #55766, #29693, #36423, #55355, #24198, #67186, #56184, #81887, #49869, #80653, #54528, #74742, #48221, #49462, #17091, #41904, #30104, #4847, #17501, #9517, #22559, #68423 ),
 ( #9929, #81061, #16258, #75156, #75568, #35189, #42313, #11176, #3203, #74327, #43132, #23377, #68012, #67598, #80243, #68829, #3617, #49045, #73917, #16674, #28866, #36016, #61687, #42727, #23790, #10763, #35601, #61263, #29283, #22966, #62096, #48632, #4438, #81473, #62509, #36836, #57416, #77209, #11998, #12825, #63741, #76791, #64166, #19538, #24611, #6080, #6914, #43958, #76386, #37652, #70898, #31754, #70468, #18719, #18316, #25015, #12407, #44361, #38482, #25845, #38897, #69244, #51505, #83109, #69654, #25428, #51093, #70053, #38065, #45195, #64576, #32585, #77635, #19122, #37252, #44771, #31334, #32169, #6499, #57825, #193, #613, #43545, #58248, #26269, #51930, #56999, #30925, #13248, #50278, #11592, #62927, #63330, #5261, #56592, #82292, #75976, #5667, #82696, #50688, #59093, #59507, #9010, #53598, #54014, #65000, #39312, #40158, #65433, #8590, #40570, #78054, #7766, #39737, #53178, #52767, #20800, #15327, #71312, #14505, #78893, #13660, #72563, #21214, #65842, #78476, #58673, #20384, #34261, #8175, #19967, #1860, #14085, #7335, #33003, #34682, #59922, #66251, #46456, #1038, #72975, #45618, #26692, #33841, #52347, #14910, #46035, #27522, #71730, #60345, #2277, #46869, #79307, #72149, #27940, #33432, #21625, #2693, #1448, #27105, #47285, #40992, #66671, #28353, #61999, #22869, #10669, #16157, #29593, #36325, #60753, #4336, #42220, #42634, #23278, #3105, #22464, #41804, #68331, #62406, #16991, #81375, #35502, #10252, #67085, #29186, #79726, #48530, #74230, #54854, #30002, #67916, #4745, #47703, #73399, #30418, #80557, #15749, #35923, #48122, #75059, #28770, #61589, #55666, #73820, #48948, #16575, #55256, #23688, #49362, #54432, #3935, #43036, #80142, #80963, #67495, #17406, #74649, #68732, #11072, #9831, #22043, #61166, #36731, #3517, #41403, #9417, #35087, #12725, #5984, #37969, #76293, #24514, #18624, #75877, #94, #64061, #56495, #38384, #31238, #43444, #70799, #69557, #6400, #25747, #57312, #11493, #6817, #32071, #69958, #63233, #44267, #50586, #76693, #38802, #12312, #18219, #82197, #57731, #63645, #50995, #50182, #81791, #62832, #43854, #51410, #77112, #19445, #17811, #11905, #56905, #31655, #83010, #69143, #25331, #37559, #19027, #5573, #13152, #45095, #64479, #49771, #44675, #75471, #70370, #82601, #56086, #24102, #24918, #37147, #5166, #30830, #13563, #72886, #58579, #52672, #64902, #40483, #21535, #15235, #7671, #59830, #79219, #39644, #66161, #72056, #33342, #32913, #45522, #34167, #52254, #32487, #13988, #14823, #77960, #39217, #27426, #27850, #72474, #65754, #14413, #78380, #944, #20710, #20289, #2183, #8501, #26602, #53511, #59004, #19873, #47195, #45938, #40895, #66576, #33751, #71218, #58150, #519, #46363, #65335, #40067, #27011, #53087, #26172, #8087, #71636, #1359, #51833, #59412, #78799, #1768, #77538, #7239, #21123, #46783, #16899, #55570, #53922, #54340, #67406, #74137, #48437, #21952, #80465, #73729, #10161, #3012, #49265, #68240, #61902, #2602, #22775, #28260, #16481, #60664, #42538, #60254, #16067, #42128, #79634, #4243, #73306, #74967, #34998, #29089, #41311, #10575, #81278, #17313, #9740, #36232, #23594, #41713, #29906, #67823, #35411, #9328, #47610, #42941, #28679, #35827, #15654, #61075, #8911, #3426, #54759, #61493, #48853, #3841, #34586, #66996, #80050, #22369, #29501, #48028, #55161, #80871, #23183, #74554, #82506, #18931, #37051, #37875, #5479, #18530, #5883, #44579, #49677, #31140, #31974, #69045, #18123, #62733, #12626, #56807, #12218, #43755, #43343, #51311, #31556, #70272, #24415, #50085, #37466, #69461, #63549, #50900, #63961, #10975, #76600, #24822, #11394, #50490, #76193, #11811, #63139, #38285, #6298, #57634, #19346, #44173, #62311, #69866, #56403, #57213, #82915, #25235, #22215, #25649, #68636, #77014, #36635, #4648, #82102, #55987, #30319, #75368, #81698, #24009, #5071, #17715, #30740, #75781, #44996, #415, #46261, #20185, #840, #1261, #34063, #78698, #79119, #6716, #64380, #65229, #7136, #33649, #65656, #19767, #32809, #64797, #78277, #77856, #45836, #40377, #13048, #39541, #20609, #38701, #14309 ) ),
 .UNSPECIFIED., .F., .F., .F. ) 
 B_SPLINE_SURFACE_WITH_KNOTS ( ( 2, 2 ),
 ( 3, 2, 2, 2, 2, 2, 2, 2, 2, 2, 2, 2, 2, 2, 2, 2, 2, 2, 2, 2, 2, 2, 2, 2, 2, 2, 2, 2, 2, 2, 2, 2, 2, 2, 2, 2, 2, 2, 2, 2, 2, 2, 2, 2, 2, 2, 2, 2, 2, 2, 2, 2, 2, 2, 2, 2, 2, 2, 2, 2, 2, 2, 2, 2, 2, 2, 2, 2, 2, 2, 2, 2, 2, 2, 2, 2, 2, 2, 2, 2, 2, 2, 2, 2, 2, 2, 2, 2, 2, 2, 2, 2, 2, 2, 2, 2, 2, 2, 2, 2, 2, 2, 2, 2, 2, 2, 2, 2, 2, 2, 2, 2, 2, 2, 2, 2, 2, 2, 2, 2, 2, 2, 2, 2, 2, 2, 2, 2, 2, 2, 2, 2, 2, 2, 2, 2, 2, 2, 2, 2, 2, 2, 2, 2, 2, 2, 2, 2, 2, 2, 2, 2, 2, 2, 2, 2, 2, 2, 2, 2, 2, 2, 2, 2, 2, 2, 2, 2, 2, 2, 2, 2, 2, 2, 2, 2, 2, 2, 2, 2, 2, 2, 2, 2, 2, 2, 2, 2, 2, 2, 2, 2, 2, 2, 2, 2, 2, 2, 2, 2, 2, 2, 2, 2, 2, 2, 2, 2, 2, 2, 2, 2, 2, 2, 2, 2, 2, 2, 2, 2, 2, 2, 2, 2, 2, 2, 2, 2, 2, 2, 2, 2, 2, 2, 2, 2, 2, 2, 2, 2, 2, 2, 2, 2, 2, 2, 2, 2, 2, 2, 2, 2, 2, 2, 2, 3 ),
 ( 0.000000000000000000, 1.000000000000000000 ),
 ( 0.000000000000000000, 0.003787878787878787984, 0.007575757575757575968, 0.01136363636363636395, 0.01515151515151515194, 0.01893939393939393992, 0.02272727272727272790, 0.02651515151515151589, 0.03030303030303030387, 0.03409090909090908839, 0.03787878787878787984, 0.04166666666666666435, 0.04545454545454545581, 0.04924242424242424032, 0.05303030303030303177, 0.05681818181818181629, 0.06060606060606060774, 0.06439393939393939226, 0.06818181818181817677, 0.07196969696969697516, 0.07575757575757575968, 0.07954545454545454419, 0.08333333333333332871, 0.08712121212121212710, 0.09090909090909091161, 0.09469696969696969613, 0.09848484848484848064, 0.1022727272727272790, 0.1060606060606060635, 0.1098484848484848481, 0.1136363636363636326, 0.1174242424242424310, 0.1212121212121212155, 0.1250000000000000000, 0.1287878787878787845, 0.1325757575757575690, 0.1363636363636363535, 0.1401515151515151381, 0.1439393939393939503, 0.1477272727272727348, 0.1515151515151515194, 0.1553030303030303039, 0.1590909090909090884, 0.1628787878787878729, 0.1666666666666666574, 0.1704545454545454419, 0.1742424242424242542, 0.1780303030303030387, 0.1818181818181818232, 0.1856060606060606077, 0.1893939393939393923, 0.1931818181818181768, 0.1969696969696969613, 0.2007575757575757458, 0.2045454545454545581, 0.2083333333333333426, 0.2121212121212121271, 0.2159090909090909116, 0.2196969696969696961, 0.2234848484848484806, 0.2272727272727272652, 0.2310606060606060497, 0.2348484848484848619, 0.2386363636363636465, 0.2424242424242424310, 0.2462121212121212155, 0.2500000000000000000, 0.2537878787878787845, 0.2575757575757575690, 0.2613636363636363535, 0.2651515151515151381, 0.2689393939393939226, 0.2727272727272727071, 0.2765151515151514916, 0.2803030303030302761, 0.2840909090909091161, 0.2878787878787879007, 0.2916666666666666852, 0.2954545454545454697, 0.2992424242424242542, 0.3030303030303030387, 0.3068181818181818232, 0.3106060606060606077, 0.3143939393939393923, 0.3181818181818181768, 0.3219696969696969613, 0.3257575757575757458, 0.3295454545454545303, 0.3333333333333333148, 0.3371212121212120993, 0.3409090909090908839, 0.3446969696969697239, 0.3484848484848485084, 0.3522727272727272929, 0.3560606060606060774, 0.3598484848484848619, 0.3636363636363636465, 0.3674242424242424310, 0.3712121212121212155, 0.3750000000000000000, 0.3787878787878787845, 0.3825757575757575690, 0.3863636363636363535, 0.3901515151515151381, 0.3939393939393939226, 0.3977272727272727071, 0.4015151515151514916, 0.4053030303030302761, 0.4090909090909091161, 0.4128787878787879007, 0.4166666666666666852, 0.4204545454545454697, 0.4242424242424242542, 0.4280303030303030387, 0.4318181818181818232, 0.4356060606060606077, 0.4393939393939393923, 0.4431818181818181768, 0.4469696969696969613, 0.4507575757575757458, 0.4545454545454545303, 0.4583333333333333148, 0.4621212121212120993, 0.4659090909090908839, 0.4696969696969697239, 0.4734848484848485084, 0.4772727272727272929, 0.4810606060606060774, 0.4848484848484848619, 0.4886363636363636465, 0.4924242424242424310, 0.4962121212121212155, 0.5000000000000000000, 0.5037878787878787845, 0.5075757575757575690, 0.5113636363636363535, 0.5151515151515151381, 0.5189393939393939226, 0.5227272727272727071, 0.5265151515151514916, 0.5303030303030302761, 0.5340909090909090606, 0.5378787878787878451, 0.5416666666666666297, 0.5454545454545454142, 0.5492424242424241987, 0.5530303030303029832, 0.5568181818181817677, 0.5606060606060605522, 0.5643939393939394478, 0.5681818181818182323, 0.5719696969696970168, 0.5757575757575758013, 0.5795454545454545858, 0.5833333333333333703, 0.5871212121212121549, 0.5909090909090909394, 0.5946969696969697239, 0.5984848484848485084, 0.6022727272727272929, 0.6060606060606060774, 0.6098484848484848619, 0.6136363636363636465, 0.6174242424242424310, 0.6212121212121212155, 0.6250000000000000000, 0.6287878787878787845, 0.6325757575757575690, 0.6363636363636363535, 0.6401515151515151381, 0.6439393939393939226, 0.6477272727272727071, 0.6515151515151514916, 0.6553030303030302761, 0.6590909090909090606, 0.6628787878787878451, 0.6666666666666666297, 0.6704545454545454142, 0.6742424242424241987, 0.6780303030303029832, 0.6818181818181817677, 0.6856060606060605522, 0.6893939393939394478, 0.6931818181818182323, 0.6969696969696970168, 0.7007575757575758013, 0.7045454545454545858, 0.7083333333333333703, 0.7121212121212121549, 0.7159090909090909394, 0.7196969696969697239, 0.7234848484848485084, 0.7272727272727272929, 0.7310606060606060774, 0.7348484848484848619, 0.7386363636363636465, 0.7424242424242424310, 0.7462121212121212155, 0.7500000000000000000, 0.7537878787878787845, 0.7575757575757575690, 0.7613636363636363535, 0.7651515151515151381, 0.7689393939393939226, 0.7727272727272727071, 0.7765151515151514916, 0.7803030303030302761, 0.7840909090909090606, 0.7878787878787878451, 0.7916666666666666297, 0.7954545454545454142, 0.7992424242424241987, 0.8030303030303029832, 0.8068181818181817677, 0.8106060606060605522, 0.8143939393939394478, 0.8181818181818182323, 0.8219696969696970168, 0.8257575757575758013, 0.8295454545454545858, 0.8333333333333333703, 0.8371212121212121549, 0.8409090909090909394, 0.8446969696969697239, 0.8484848484848485084, 0.8522727272727272929, 0.8560606060606060774, 0.8598484848484848619, 0.8636363636363636465, 0.8674242424242424310, 0.8712121212121212155, 0.8750000000000000000, 0.8787878787878787845, 0.8825757575757575690, 0.8863636363636363535, 0.8901515151515151381, 0.8939393939393939226, 0.8977272727272727071, 0.9015151515151514916, 0.9053030303030302761, 0.9090909090909090606, 0.9128787878787878451, 0.9166666666666666297, 0.9204545454545454142, 0.9242424242424241987, 0.9280303030303029832, 0.9318181818181817677, 0.9356060606060605522, 0.9393939393939394478, 0.9431818181818182323, 0.9469696969696970168, 0.9507575757575758013, 0.9545454545454545858, 0.9583333333333333703, 0.9621212121212121549, 0.9659090909090909394 ),
 .UNSPECIFIED. ) 
 GEOMETRIC_REPRESENTATION_ITEM ( )  RATIONAL_B_SPLINE_SURFACE ( (
 ( 1.000000000000000000, 0.9659258262890683122, 1.000000000000000000, 0.9659258262890683122, 1.000000000000000000, 0.9659258262890683122, 1.000000000000000000, 0.9659258262890683122, 1.000000000000000000, 0.9659258262890683122, 1.000000000000000000, 0.9659258262890683122, 1.000000000000000000, 0.9659258262890683122, 1.000000000000000000, 0.9659258262890683122, 1.000000000000000000, 0.9659258262890683122, 1.000000000000000000, 0.9659258262890683122, 1.000000000000000000, 0.9659258262890683122, 1.000000000000000000, 0.9659258262890683122, 1.000000000000000000, 0.9659258262890683122, 1.000000000000000000, 0.9659258262890683122, 1.000000000000000000, 0.9659258262890683122, 1.000000000000000000, 0.9659258262890683122, 1.000000000000000000, 0.9659258262890683122, 1.000000000000000000, 0.9659258262890683122, 1.000000000000000000, 0.9659258262890683122, 1.000000000000000000, 0.9659258262890683122, 1.000000000000000000, 0.9659258262890683122, 1.000000000000000000, 0.9659258262890683122, 1.000000000000000000, 0.9659258262890683122, 1.000000000000000000, 0.9659258262890683122, 1.000000000000000000, 0.9659258262890683122, 1.000000000000000000, 0.9659258262890683122, 1.000000000000000000, 0.9659258262890683122, 1.000000000000000000, 0.9659258262890683122, 1.000000000000000000, 0.9659258262890683122, 1.000000000000000000, 0.9659258262890683122, 1.000000000000000000, 0.9659258262890683122, 1.000000000000000000, 0.9659258262890683122, 1.000000000000000000, 0.9659258262890683122, 1.000000000000000000, 0.9659258262890683122, 1.000000000000000000, 0.9659258262890683122, 1.000000000000000000, 0.9659258262890683122, 1.000000000000000000, 0.9659258262890683122, 1.000000000000000000, 0.9659258262890683122, 1.000000000000000000, 0.9659258262890683122, 1.000000000000000000, 0.9659258262890683122, 1.000000000000000000, 0.9659258262890683122, 1.000000000000000000, 0.9659258262890683122, 1.000000000000000000, 0.9659258262890683122, 1.000000000000000000, 0.9659258262890683122, 1.000000000000000000, 0.9659258262890683122, 1.000000000000000000, 0.9659258262890683122, 1.000000000000000000, 0.9659258262890683122, 1.000000000000000000, 0.9659258262890683122, 1.000000000000000000, 0.9659258262890683122, 1.000000000000000000, 0.9659258262890683122, 1.000000000000000000, 0.9659258262890683122, 1.000000000000000000, 0.9659258262890683122, 1.000000000000000000, 0.9659258262890683122, 1.000000000000000000, 0.9659258262890683122, 1.000000000000000000, 0.9659258262890683122, 1.000000000000000000, 0.9659258262890683122, 1.000000000000000000, 0.9659258262890683122, 1.000000000000000000, 0.9659258262890683122, 1.000000000000000000, 0.9659258262890683122, 1.000000000000000000, 0.9659258262890683122, 1.000000000000000000, 0.9659258262890683122, 1.000000000000000000, 0.9659258262890683122, 1.000000000000000000, 0.9659258262890683122, 1.000000000000000000, 0.9659258262890683122, 1.000000000000000000, 0.9659258262890683122, 1.000000000000000000, 0.9659258262890683122, 1.000000000000000000, 0.9659258262890683122, 1.000000000000000000, 0.9659258262890683122, 1.000000000000000000, 0.9659258262890683122, 1.000000000000000000, 0.9659258262890683122, 1.000000000000000000, 0.9659258262890683122, 1.000000000000000000, 0.9659258262890683122, 1.000000000000000000, 0.9659258262890683122, 1.000000000000000000, 0.9659258262890683122, 1.000000000000000000, 0.9659258262890683122, 1.000000000000000000, 0.9659258262890683122, 1.000000000000000000, 0.9659258262890683122, 1.000000000000000000, 0.9659258262890683122, 1.000000000000000000, 0.9659258262890683122, 1.000000000000000000, 0.9659258262890683122, 1.000000000000000000, 0.9659258262890683122, 1.000000000000000000, 0.9659258262890683122, 1.000000000000000000, 0.9659258262890683122, 1.000000000000000000, 0.9659258262890683122, 1.000000000000000000, 0.9659258262890683122, 1.000000000000000000, 0.9659258262890683122, 1.000000000000000000, 0.9659258262890683122, 1.000000000000000000, 0.9659258262890683122, 1.000000000000000000, 0.9659258262890683122, 1.000000000000000000, 0.9659258262890683122, 1.000000000000000000, 0.9659258262890683122, 1.000000000000000000, 0.9659258262890683122, 1.000000000000000000, 0.9659258262890683122, 1.000000000000000000, 0.9659258262890683122, 1.000000000000000000, 0.9659258262890683122, 1.000000000000000000, 0.9659258262890683122, 1.000000000000000000, 0.9659258262890683122, 1.000000000000000000, 0.9659258262890683122, 1.000000000000000000, 0.9659258262890683122, 1.000000000000000000, 0.9659258262890683122, 1.000000000000000000, 0.9659258262890683122, 1.000000000000000000, 0.9659258262890683122, 1.000000000000000000, 0.9659258262890683122, 1.000000000000000000, 0.9659258262890683122, 1.000000000000000000, 0.9659258262890683122, 1.000000000000000000, 0.9659258262890683122, 1.000000000000000000, 0.9659258262890683122, 1.000000000000000000, 0.9659258262890683122, 1.000000000000000000, 0.9659258262890683122, 1.000000000000000000, 0.9659258262890683122, 1.000000000000000000, 0.9659258262890683122, 1.000000000000000000, 0.9659258262890683122, 1.000000000000000000, 0.9659258262890683122, 1.000000000000000000, 0.9659258262890683122, 1.000000000000000000, 0.9659258262890683122, 1.000000000000000000, 0.9659258262890683122, 1.000000000000000000, 0.9659258262890683122, 1.000000000000000000, 0.9659258262890683122, 1.000000000000000000, 0.9659258262890683122, 1.000000000000000000, 0.9659258262890683122, 1.000000000000000000, 0.9659258262890683122, 1.000000000000000000, 0.9659258262890683122, 1.000000000000000000, 0.9659258262890683122, 1.000000000000000000, 0.9659258262890683122, 1.000000000000000000, 0.9659258262890683122, 1.000000000000000000, 0.9659258262890683122, 1.000000000000000000, 0.9659258262890683122, 1.000000000000000000, 0.9659258262890683122, 1.000000000000000000, 0.9659258262890683122, 1.000000000000000000, 0.9659258262890683122, 1.000000000000000000, 0.9659258262890683122, 1.000000000000000000, 0.9659258262890683122, 1.000000000000000000, 0.9659258262890683122, 1.000000000000000000, 0.9659258262890683122, 1.000000000000000000, 0.9659258262890683122, 1.000000000000000000, 0.9659258262890683122, 1.000000000000000000, 0.9659258262890683122, 1.000000000000000000, 0.9659258262890683122, 1.000000000000000000, 0.9659258262890683122, 1.000000000000000000, 0.9659258262890683122, 1.000000000000000000, 0.9659258262890683122, 1.000000000000000000, 0.9659258262890683122, 1.000000000000000000, 0.9659258262890683122, 1.000000000000000000, 0.9659258262890683122, 1.000000000000000000, 0.9659258262890683122, 1.000000000000000000, 0.9659258262890683122, 1.000000000000000000, 0.9659258262890683122, 1.000000000000000000, 0.9659258262890683122, 1.000000000000000000, 0.9659258262890683122, 1.000000000000000000, 0.9659258262890683122, 1.000000000000000000, 0.9659258262890683122, 1.000000000000000000, 0.9659258262890683122, 1.000000000000000000, 0.9659258262890683122, 1.000000000000000000, 0.9659258262890683122, 1.000000000000000000, 0.9659258262890683122, 1.000000000000000000, 0.9659258262890683122, 1.000000000000000000, 0.9659258262890683122, 1.000000000000000000, 0.9659258262890683122, 1.000000000000000000, 0.9659258262890683122, 1.000000000000000000, 0.9659258262890683122, 1.000000000000000000, 0.9659258262890683122, 1.000000000000000000, 0.9659258262890683122, 1.000000000000000000, 0.9659258262890683122, 1.000000000000000000, 0.9659258262890683122, 1.000000000000000000, 0.9659258262890683122, 1.000000000000000000, 0.9659258262890683122, 1.000000000000000000, 0.9659258262890683122, 1.000000000000000000, 0.9659258262890683122, 1.000000000000000000, 0.9659258262890683122, 1.000000000000000000, 0.9659258262890683122, 1.000000000000000000, 0.9659258262890683122, 1.000000000000000000, 0.9659258262890683122, 1.000000000000000000, 0.9659258262890683122, 1.000000000000000000, 0.9659258262890683122, 1.000000000000000000, 0.9659258262890683122, 1.000000000000000000, 0.9659258262890683122, 1.000000000000000000, 0.9659258262890683122, 1.000000000000000000, 0.9659258262890683122, 1.000000000000000000, 0.9659258262890683122, 1.000000000000000000, 0.9659258262890683122, 1.000000000000000000, 0.9659258262890683122, 1.000000000000000000, 0.9659258262890683122, 1.000000000000000000, 0.9659258262890683122, 1.000000000000000000, 0.9659258262890683122, 1.000000000000000000, 0.9659258262890683122, 1.000000000000000000, 0.9659258262890683122, 1.000000000000000000, 0.9659258262890683122, 1.000000000000000000, 0.9659258262890683122, 1.000000000000000000, 0.9659258262890683122, 1.000000000000000000, 0.9659258262890683122, 1.000000000000000000, 0.9659258262890683122, 1.000000000000000000, 0.9659258262890683122, 1.000000000000000000, 0.9659258262890683122, 1.000000000000000000, 0.9659258262890683122, 1.000000000000000000, 0.9659258262890683122, 1.000000000000000000, 0.9659258262890683122, 1.000000000000000000, 0.9659258262890683122, 1.000000000000000000, 0.9659258262890683122, 1.000000000000000000, 0.9659258262890683122, 1.000000000000000000, 0.9659258262890683122, 1.000000000000000000, 0.9659258262890683122, 1.000000000000000000, 0.9659258262890683122, 1.000000000000000000, 0.9659258262890683122, 1.000000000000000000, 0.9659258262890683122, 1.000000000000000000, 0.9659258262890683122, 1.000000000000000000, 0.9659258262890683122, 1.000000000000000000, 0.9659258262890683122, 1.000000000000000000, 0.9659258262890683122, 1.000000000000000000, 0.9659258262890683122, 1.000000000000000000, 0.9659258262890683122, 1.000000000000000000, 0.9659258262890683122, 1.000000000000000000, 0.9659258262890683122, 1.000000000000000000, 0.9659258262890683122, 1.000000000000000000, 0.9659258262890683122, 1.000000000000000000, 0.9659258262890683122, 1.000000000000000000, 0.9659258262890683122, 1.000000000000000000, 0.9659258262890683122, 1.000000000000000000, 0.9659258262890683122, 1.000000000000000000, 0.9659258262890683122, 1.000000000000000000, 0.9659258262890683122, 1.000000000000000000, 0.9659258262890683122, 1.000000000000000000, 0.9659258262890683122, 1.000000000000000000, 0.9659258262890683122, 1.000000000000000000, 0.9659258262890683122, 1.000000000000000000, 0.9659258262890683122, 1.000000000000000000, 0.9659258262890683122, 1.000000000000000000, 0.9659258262890683122, 1.000000000000000000, 0.9659258262890683122, 1.000000000000000000, 0.9659258262890683122, 1.000000000000000000, 0.9659258262890683122, 1.000000000000000000, 0.9659258262890683122, 1.000000000000000000, 0.9659258262890683122, 1.000000000000000000, 0.9659258262890683122, 1.000000000000000000, 0.9659258262890683122, 1.000000000000000000, 0.9659258262890683122, 1.000000000000000000, 0.9659258262890683122, 1.000000000000000000, 0.9659258262890683122, 1.000000000000000000, 0.9659258262890683122, 1.000000000000000000, 0.9659258262890683122, 1.000000000000000000, 0.9659258262890683122, 1.000000000000000000, 0.9659258262890683122, 1.000000000000000000, 0.9659258262890683122, 1.000000000000000000, 0.9659258262890683122, 1.000000000000000000, 0.9659258262890683122, 1.000000000000000000, 0.9659258262890683122, 1.000000000000000000, 0.9659258262890683122, 1.000000000000000000, 0.9659258262890683122, 1.000000000000000000, 0.9659258262890683122, 1.000000000000000000, 0.9659258262890683122, 1.000000000000000000, 0.9659258262890683122, 1.000000000000000000, 0.9659258262890683122, 1.000000000000000000, 0.9659258262890683122, 1.000000000000000000, 0.9659258262890683122, 1.000000000000000000, 0.9659258262890683122, 1.000000000000000000, 0.9659258262890683122, 1.000000000000000000),
 ( 1.000000000000000000, 0.9659258262890683122, 1.000000000000000000, 0.9659258262890683122, 1.000000000000000000, 0.9659258262890683122, 1.000000000000000000, 0.9659258262890683122, 1.000000000000000000, 0.9659258262890683122, 1.000000000000000000, 0.9659258262890683122, 1.000000000000000000, 0.9659258262890683122, 1.000000000000000000, 0.9659258262890683122, 1.000000000000000000, 0.9659258262890683122, 1.000000000000000000, 0.9659258262890683122, 1.000000000000000000, 0.9659258262890683122, 1.000000000000000000, 0.9659258262890683122, 1.000000000000000000, 0.9659258262890683122, 1.000000000000000000, 0.9659258262890683122, 1.000000000000000000, 0.9659258262890683122, 1.000000000000000000, 0.9659258262890683122, 1.000000000000000000, 0.9659258262890683122, 1.000000000000000000, 0.9659258262890683122, 1.000000000000000000, 0.9659258262890683122, 1.000000000000000000, 0.9659258262890683122, 1.000000000000000000, 0.9659258262890683122, 1.000000000000000000, 0.9659258262890683122, 1.000000000000000000, 0.9659258262890683122, 1.000000000000000000, 0.9659258262890683122, 1.000000000000000000, 0.9659258262890683122, 1.000000000000000000, 0.9659258262890683122, 1.000000000000000000, 0.9659258262890683122, 1.000000000000000000, 0.9659258262890683122, 1.000000000000000000, 0.9659258262890683122, 1.000000000000000000, 0.9659258262890683122, 1.000000000000000000, 0.9659258262890683122, 1.000000000000000000, 0.9659258262890683122, 1.000000000000000000, 0.9659258262890683122, 1.000000000000000000, 0.9659258262890683122, 1.000000000000000000, 0.9659258262890683122, 1.000000000000000000, 0.9659258262890683122, 1.000000000000000000, 0.9659258262890683122, 1.000000000000000000, 0.9659258262890683122, 1.000000000000000000, 0.9659258262890683122, 1.000000000000000000, 0.9659258262890683122, 1.000000000000000000, 0.9659258262890683122, 1.000000000000000000, 0.9659258262890683122, 1.000000000000000000, 0.9659258262890683122, 1.000000000000000000, 0.9659258262890683122, 1.000000000000000000, 0.9659258262890683122, 1.000000000000000000, 0.9659258262890683122, 1.000000000000000000, 0.9659258262890683122, 1.000000000000000000, 0.9659258262890683122, 1.000000000000000000, 0.9659258262890683122, 1.000000000000000000, 0.9659258262890683122, 1.000000000000000000, 0.9659258262890683122, 1.000000000000000000, 0.9659258262890683122, 1.000000000000000000, 0.9659258262890683122, 1.000000000000000000, 0.9659258262890683122, 1.000000000000000000, 0.9659258262890683122, 1.000000000000000000, 0.9659258262890683122, 1.000000000000000000, 0.9659258262890683122, 1.000000000000000000, 0.9659258262890683122, 1.000000000000000000, 0.9659258262890683122, 1.000000000000000000, 0.9659258262890683122, 1.000000000000000000, 0.9659258262890683122, 1.000000000000000000, 0.9659258262890683122, 1.000000000000000000, 0.9659258262890683122, 1.000000000000000000, 0.9659258262890683122, 1.000000000000000000, 0.9659258262890683122, 1.000000000000000000, 0.9659258262890683122, 1.000000000000000000, 0.9659258262890683122, 1.000000000000000000, 0.9659258262890683122, 1.000000000000000000, 0.9659258262890683122, 1.000000000000000000, 0.9659258262890683122, 1.000000000000000000, 0.9659258262890683122, 1.000000000000000000, 0.9659258262890683122, 1.000000000000000000, 0.9659258262890683122, 1.000000000000000000, 0.9659258262890683122, 1.000000000000000000, 0.9659258262890683122, 1.000000000000000000, 0.9659258262890683122, 1.000000000000000000, 0.9659258262890683122, 1.000000000000000000, 0.9659258262890683122, 1.000000000000000000, 0.9659258262890683122, 1.000000000000000000, 0.9659258262890683122, 1.000000000000000000, 0.9659258262890683122, 1.000000000000000000, 0.9659258262890683122, 1.000000000000000000, 0.9659258262890683122, 1.000000000000000000, 0.9659258262890683122, 1.000000000000000000, 0.9659258262890683122, 1.000000000000000000, 0.9659258262890683122, 1.000000000000000000, 0.9659258262890683122, 1.000000000000000000, 0.9659258262890683122, 1.000000000000000000, 0.9659258262890683122, 1.000000000000000000, 0.9659258262890683122, 1.000000000000000000, 0.9659258262890683122, 1.000000000000000000, 0.9659258262890683122, 1.000000000000000000, 0.9659258262890683122, 1.000000000000000000, 0.9659258262890683122, 1.000000000000000000, 0.9659258262890683122, 1.000000000000000000, 0.9659258262890683122, 1.000000000000000000, 0.9659258262890683122, 1.000000000000000000, 0.9659258262890683122, 1.000000000000000000, 0.9659258262890683122, 1.000000000000000000, 0.9659258262890683122, 1.000000000000000000, 0.9659258262890683122, 1.000000000000000000, 0.9659258262890683122, 1.000000000000000000, 0.9659258262890683122, 1.000000000000000000, 0.9659258262890683122, 1.000000000000000000, 0.9659258262890683122, 1.000000000000000000, 0.9659258262890683122, 1.000000000000000000, 0.9659258262890683122, 1.000000000000000000, 0.9659258262890683122, 1.000000000000000000, 0.9659258262890683122, 1.000000000000000000, 0.9659258262890683122, 1.000000000000000000, 0.9659258262890683122, 1.000000000000000000, 0.9659258262890683122, 1.000000000000000000, 0.9659258262890683122, 1.000000000000000000, 0.9659258262890683122, 1.000000000000000000, 0.9659258262890683122, 1.000000000000000000, 0.9659258262890683122, 1.000000000000000000, 0.9659258262890683122, 1.000000000000000000, 0.9659258262890683122, 1.000000000000000000, 0.9659258262890683122, 1.000000000000000000, 0.9659258262890683122, 1.000000000000000000, 0.9659258262890683122, 1.000000000000000000, 0.9659258262890683122, 1.000000000000000000, 0.9659258262890683122, 1.000000000000000000, 0.9659258262890683122, 1.000000000000000000, 0.9659258262890683122, 1.000000000000000000, 0.9659258262890683122, 1.000000000000000000, 0.9659258262890683122, 1.000000000000000000, 0.9659258262890683122, 1.000000000000000000, 0.9659258262890683122, 1.000000000000000000, 0.9659258262890683122, 1.000000000000000000, 0.9659258262890683122, 1.000000000000000000, 0.9659258262890683122, 1.000000000000000000, 0.9659258262890683122, 1.000000000000000000, 0.9659258262890683122, 1.000000000000000000, 0.9659258262890683122, 1.000000000000000000, 0.9659258262890683122, 1.000000000000000000, 0.9659258262890683122, 1.000000000000000000, 0.9659258262890683122, 1.000000000000000000, 0.9659258262890683122, 1.000000000000000000, 0.9659258262890683122, 1.000000000000000000, 0.9659258262890683122, 1.000000000000000000, 0.9659258262890683122, 1.000000000000000000, 0.9659258262890683122, 1.000000000000000000, 0.9659258262890683122, 1.000000000000000000, 0.9659258262890683122, 1.000000000000000000, 0.9659258262890683122, 1.000000000000000000, 0.9659258262890683122, 1.000000000000000000, 0.9659258262890683122, 1.000000000000000000, 0.9659258262890683122, 1.000000000000000000, 0.9659258262890683122, 1.000000000000000000, 0.9659258262890683122, 1.000000000000000000, 0.9659258262890683122, 1.000000000000000000, 0.9659258262890683122, 1.000000000000000000, 0.9659258262890683122, 1.000000000000000000, 0.9659258262890683122, 1.000000000000000000, 0.9659258262890683122, 1.000000000000000000, 0.9659258262890683122, 1.000000000000000000, 0.9659258262890683122, 1.000000000000000000, 0.9659258262890683122, 1.000000000000000000, 0.9659258262890683122, 1.000000000000000000, 0.9659258262890683122, 1.000000000000000000, 0.9659258262890683122, 1.000000000000000000, 0.9659258262890683122, 1.000000000000000000, 0.9659258262890683122, 1.000000000000000000, 0.9659258262890683122, 1.000000000000000000, 0.9659258262890683122, 1.000000000000000000, 0.9659258262890683122, 1.000000000000000000, 0.9659258262890683122, 1.000000000000000000, 0.9659258262890683122, 1.000000000000000000, 0.9659258262890683122, 1.000000000000000000, 0.9659258262890683122, 1.000000000000000000, 0.9659258262890683122, 1.000000000000000000, 0.9659258262890683122, 1.000000000000000000, 0.9659258262890683122, 1.000000000000000000, 0.9659258262890683122, 1.000000000000000000, 0.9659258262890683122, 1.000000000000000000, 0.9659258262890683122, 1.000000000000000000, 0.9659258262890683122, 1.000000000000000000, 0.9659258262890683122, 1.000000000000000000, 0.9659258262890683122, 1.000000000000000000, 0.9659258262890683122, 1.000000000000000000, 0.9659258262890683122, 1.000000000000000000, 0.9659258262890683122, 1.000000000000000000, 0.9659258262890683122, 1.000000000000000000, 0.9659258262890683122, 1.000000000000000000, 0.9659258262890683122, 1.000000000000000000, 0.9659258262890683122, 1.000000000000000000, 0.9659258262890683122, 1.000000000000000000, 0.9659258262890683122, 1.000000000000000000, 0.9659258262890683122, 1.000000000000000000, 0.9659258262890683122, 1.000000000000000000, 0.9659258262890683122, 1.000000000000000000, 0.9659258262890683122, 1.000000000000000000, 0.9659258262890683122, 1.000000000000000000, 0.9659258262890683122, 1.000000000000000000, 0.9659258262890683122, 1.000000000000000000, 0.9659258262890683122, 1.000000000000000000, 0.9659258262890683122, 1.000000000000000000, 0.9659258262890683122, 1.000000000000000000, 0.9659258262890683122, 1.000000000000000000, 0.9659258262890683122, 1.000000000000000000, 0.9659258262890683122, 1.000000000000000000, 0.9659258262890683122, 1.000000000000000000, 0.9659258262890683122, 1.000000000000000000, 0.9659258262890683122, 1.000000000000000000, 0.9659258262890683122, 1.000000000000000000, 0.9659258262890683122, 1.000000000000000000, 0.9659258262890683122, 1.000000000000000000, 0.9659258262890683122, 1.000000000000000000, 0.9659258262890683122, 1.000000000000000000, 0.9659258262890683122, 1.000000000000000000, 0.9659258262890683122, 1.000000000000000000, 0.9659258262890683122, 1.000000000000000000, 0.9659258262890683122, 1.000000000000000000, 0.9659258262890683122, 1.000000000000000000, 0.9659258262890683122, 1.000000000000000000, 0.9659258262890683122, 1.000000000000000000, 0.9659258262890683122, 1.000000000000000000, 0.9659258262890683122, 1.000000000000000000, 0.9659258262890683122, 1.000000000000000000, 0.9659258262890683122, 1.000000000000000000, 0.9659258262890683122, 1.000000000000000000, 0.9659258262890683122, 1.000000000000000000, 0.9659258262890683122, 1.000000000000000000, 0.9659258262890683122, 1.000000000000000000, 0.9659258262890683122, 1.000000000000000000, 0.9659258262890683122, 1.000000000000000000, 0.9659258262890683122, 1.000000000000000000, 0.9659258262890683122, 1.000000000000000000, 0.9659258262890683122, 1.000000000000000000, 0.9659258262890683122, 1.000000000000000000, 0.9659258262890683122, 1.000000000000000000, 0.9659258262890683122, 1.000000000000000000, 0.9659258262890683122, 1.000000000000000000, 0.9659258262890683122, 1.000000000000000000, 0.9659258262890683122, 1.000000000000000000, 0.9659258262890683122, 1.000000000000000000, 0.9659258262890683122, 1.000000000000000000, 0.9659258262890683122, 1.000000000000000000, 0.9659258262890683122, 1.000000000000000000, 0.9659258262890683122, 1.000000000000000000, 0.9659258262890683122, 1.000000000000000000, 0.9659258262890683122, 1.000000000000000000, 0.9659258262890683122, 1.000000000000000000, 0.9659258262890683122, 1.000000000000000000, 0.9659258262890683122, 1.000000000000000000, 0.9659258262890683122, 1.000000000000000000, 0.9659258262890683122, 1.000000000000000000, 0.9659258262890683122, 1.000000000000000000, 0.9659258262890683122, 1.000000000000000000, 0.9659258262890683122, 1.000000000000000000, 0.9659258262890683122, 1.000000000000000000, 0.9659258262890683122, 1.000000000000000000, 0.9659258262890683122, 1.000000000000000000, 0.9659258262890683122, 1.000000000000000000) ) ) 
 REPRESENTATION_ITEM ( '' )  SURFACE ( )  );
#27526 = ORIENTED_EDGE ( 'NONE', *, *, #46673, .F. ) ;
#27527 = CARTESIAN_POINT ( 'NONE',  ( 0.3996062992125986035, 0.1070741851644054776, -0.2821522309711286258 ) ) ;
#27528 = ORIENTED_EDGE ( 'NONE', *, *, #2729, .T. ) ;
#27529 = CARTESIAN_POINT ( 'NONE',  ( 1.043307086614173818, 0.1660481256975885056, 0.3530559997133364547 ) ) ;
#27530 = CARTESIAN_POINT ( 'NONE',  ( 0.7677165354330716118, -0.4536011799217367080, 0.2665933059059888421 ) ) ;
#27531 = CARTESIAN_POINT ( 'NONE',  ( 0.2726377952755905665, 0.1938976377952755792, 0.1574803149606299191 ) ) ;
#27532 = CARTESIAN_POINT ( 'NONE',  ( 0.2362204724409451007, -0.4091458600556402980, -0.01115485564304462100 ) ) ;
#27533 = CARTESIAN_POINT ( 'NONE',  ( 0.000000000000000000, 2.755905511811024056, 0.000000000000000000 ) ) ;
#27534 = CARTESIAN_POINT ( 'NONE',  ( -0.1049643490035307020, 0.3917322834645669549, -1.193569553805774452 ) ) ;
#27535 = CARTESIAN_POINT ( 'NONE',  ( 1.450131233595801428, 0.2952755905511811885, 0.1292274648535926551 ) ) ;
#27536 = DIRECTION ( 'NONE',  ( -0.000000000000000000, -1.000000000000000000, -0.000000000000000000 ) ) ;
#27537 = CARTESIAN_POINT ( 'NONE',  ( -0.3543307086614165824, -0.6692913385826771977, 8.415575281601705876E-17 ) ) ;
#27538 = CARTESIAN_POINT ( 'NONE',  ( 1.167979002624672580, 0.05413385826771626580, -0.4176697321401330321 ) ) ;
#27539 = ORIENTED_EDGE ( 'NONE', *, *, #22805, .F. ) ;
#27540 = CARTESIAN_POINT ( 'NONE',  ( -1.555118110236219930, 0.1660481256975885056, 0.3530559997133364547 ) ) ;
#27541 = CARTESIAN_POINT ( 'NONE',  ( -1.018274559621366038, 1.474925757642550295, -0.4713314535542892925 ) ) ;
#27542 = DIRECTION ( 'NONE',  ( -3.491481338843133355E-15, 0.000000000000000000, 1.000000000000000000 ) ) ;
#27543 = FACE_OUTER_BOUND ( 'NONE', #39763, .T. ) ;
#27544 = PLANE ( 'NONE',  #62696 ) ;
#27545 = CARTESIAN_POINT ( 'NONE',  ( -0.7217847769028863381, -0.3690944881889763329, 0.3153832671262228327 ) ) ;
#27546 = CARTESIAN_POINT ( 'NONE',  ( -1.601049868766403650, 0.2306618581243847221, -0.2411417322834647770 ) ) ;
#27547 = CARTESIAN_POINT ( 'NONE',  ( 0.6627296587926517768, -0.6692913385826773087, -0.1292274648535924053 ) ) ;
#27548 = ORIENTED_EDGE ( 'NONE', *, *, #68575, .F. ) ;
#27550 = DIRECTION ( 'NONE',  ( 0.000000000000000000, -0.000000000000000000, -1.000000000000000000 ) ) ;
#27549 = CARTESIAN_POINT ( 'NONE',  ( 1.463254593175853824, -0.6692913385826771977, 0.1292274648535927661 ) ) ;
#27551 = CARTESIAN_POINT ( 'NONE',  ( -0.6102362204724400829, 0.07958543189024085140, 0.2665933059059887866 ) ) ;
#27552 = CARTESIAN_POINT ( 'NONE',  ( 0.8202099737532814183, -0.6692913385826773087, -0.1292274648535924053 ) ) ;
#27553 = CARTESIAN_POINT ( 'NONE',  ( -1.706036745406823485, 0.2306618581243848609, 0.2411417322834645549 ) ) ;
#27554 = CARTESIAN_POINT ( 'NONE',  ( -0.2867679344610366554, 0.2867679344610365444, -1.202080421750969741 ) ) ;
#27555 = CARTESIAN_POINT ( 'NONE',  ( -0.6496062992125976043, -0.4536011799217367080, 0.2665933059059888421 ) ) ;
#27556 = CARTESIAN_POINT ( 'NONE',  ( -1.633858267716534529, 0.07958543189024085140, 0.2665933059059887866 ) ) ;
#27557 = CARTESIAN_POINT ( 'NONE',  ( 0.2362204724409449064, 0.4091458600556404646, -0.7742782152230971437 ) ) ;
#27558 = AXIS2_PLACEMENT_3D ( 'NONE', #38088, #18342, #77231 ) ;
#27559 = CARTESIAN_POINT ( 'NONE',  ( 0.3805774278215230400, 0.05413385826771626580, -0.4176697321401330321 ) ) ;
#27560 = CARTESIAN_POINT ( 'NONE',  ( -0.8661417322834640276, -0.1870078740157479769, 0.3641732283464567677 ) ) ;
#27561 = CARTESIAN_POINT ( 'NONE',  ( -0.4986876640419942164, -0.5023911411419708095, 0.1820866141732285504 ) ) ;
#27562 = CARTESIAN_POINT ( 'NONE',  ( -0.1706036745406816491, -0.4281496062992124485, 0.4176697321401328655 ) ) ;
#27563 = CARTESIAN_POINT ( 'NONE',  ( -0.9645669291338575535, 0.07958543189024071263, -0.2665933059059888421 ) ) ;
#27564 = CARTESIAN_POINT ( 'NONE',  ( 0.3392501089628018329, 0.1958661417322835607, -0.1279720716873509745 ) ) ;
#27565 = CARTESIAN_POINT ( 'NONE',  ( 0.5905511811023629321, -0.6692913385826771977, 8.415575281601705876E-17 ) ) ;
#27566 = CARTESIAN_POINT ( 'NONE',  ( -0.6299212598425332210, 1.724409448818897905, 3.886287458032460229 ) ) ;
#27567 = CARTESIAN_POINT ( 'NONE',  ( -0.2362204724409451284, 0.4091458600556402425, -1.822178477690288512 ) ) ;
#27568 = CARTESIAN_POINT ( 'NONE',  ( -0.9645669291338575535, -0.5400638737290844871, 0.3530559997133364547 ) ) ;
#27569 = CARTESIAN_POINT ( 'NONE',  ( -0.09842519685039295696, 0.07958543189024071263, -0.2665933059059888421 ) ) ;
#27570 = EDGE_CURVE ( 'NONE', #30126, #69738, #68124, .T. ) ;
#27571 = CARTESIAN_POINT ( 'NONE',  ( -1.259842519685038686, -0.1870078740157480879, -0.4822834645669291653 ) ) ;
#27572 = CARTESIAN_POINT ( 'NONE',  ( 0.6561679790026253567, -0.5023911411419708095, -0.1820866141732282451 ) ) ;
#27573 = CIRCLE ( 'NONE', #2046, 1.122047244094488194 ) ;
#27574 = CARTESIAN_POINT ( 'NONE',  ( -0.6824146981627291497, -0.5023911411419708095, -0.1820866141732282451 ) ) ;
#27575 = CARTESIAN_POINT ( 'NONE',  ( -0.9580052493438311334, -0.4281496062992124485, 0.4176697321401328655 ) ) ;
#27576 = CARTESIAN_POINT ( 'NONE',  ( -1.509186351706035767, 0.05413385826771626580, -0.4176697321401330321 ) ) ;
#27577 = CARTESIAN_POINT ( 'NONE',  ( 1.614173228346457378, -0.6692913385826771977, 8.415575281601705876E-17 ) ) ;
#27578 = DIRECTION ( 'NONE',  ( -0.000000000000000000, -1.000000000000000000, -0.000000000000000000 ) ) ;
#27579 = CARTESIAN_POINT ( 'NONE',  ( 0.7545931758530189937, 0.1771653543307087075, -0.09757992244046823083 ) ) ;
#27580 = CARTESIAN_POINT ( 'NONE',  ( 0.3871391076115493490, -0.3162353388693405765, 0.4822834645669290543 ) ) ;
#27581 = EDGE_CURVE ( 'NONE', #11346, #71641, #22668, .T. ) ;
#27582 = DIRECTION ( 'NONE',  ( 0.000000000000000000, 0.000000000000000000, -1.000000000000000000 ) ) ;
#27583 = CARTESIAN_POINT ( 'NONE',  ( 1.240157480314961314, -0.4536011799217367080, 0.2665933059059888421 ) ) ;
#27584 = VERTEX_POINT ( 'NONE', #38178 ) ;
#27585 = CARTESIAN_POINT ( 'NONE',  ( -0.3949938075777408852, -0.1058382717557502933, 0.1922572178477690297 ) ) ;
#27586 = CARTESIAN_POINT ( 'NONE',  ( -1.410761154855641575, -0.2845877964562161244, -0.3641732283464567121 ) ) ;
#27587 = CARTESIAN_POINT ( 'NONE',  ( -0.6102362204724400829, -0.5400638737290845981, -0.3530559997133363437 ) ) ;
#27588 = CARTESIAN_POINT ( 'NONE',  ( 0.2099737532808405305, 0.2306618581243847221, -0.2411417322834647770 ) ) ;
#27589 = CARTESIAN_POINT ( 'NONE',  ( -1.417322834645668772, -0.1870078740157479769, 0.3641732283464567677 ) ) ;
#27590 = CARTESIAN_POINT ( 'NONE',  ( -0.3996062992125985480, -7.340648628747423112E-17, -2.005905511811023612 ) ) ;
#27591 = CARTESIAN_POINT ( 'NONE',  ( -1.391076115485563758, 0.2306618581243848609, 0.2411417322834645549 ) ) ;
#27592 = CARTESIAN_POINT ( 'NONE',  ( 0.4265091863517067594, 0.2952755905511811885, 0.1292274648535926551 ) ) ;
#27593 = CARTESIAN_POINT ( 'NONE',  ( -0.07874015748031421014, -0.1870078740157479769, 0.4822834645669291653 ) ) ;
#27594 = CARTESIAN_POINT ( 'NONE',  ( 1.017060367454068581, -0.05778040916215560624, -0.4822834645669293319 ) ) ;
#27595 = B_SPLINE_CURVE_WITH_KNOTS ( 'NONE', 3,
 ( #55934, #787, #45373, #45788, #56759, #31092, #83277 ),
 .UNSPECIFIED., .F., .F.,
 ( 4, 3, 4 ),
 ( 3.471140604459641645E-18, 0.001246230184515550706, 0.002492489877932668914 ),
 .UNSPECIFIED. ) ;
#27596 = CARTESIAN_POINT ( 'NONE',  ( -9.787531504996566615E-17, 0.3996062992125985480, -1.021653543307086576 ) ) ;
#27597 = CARTESIAN_POINT ( 'NONE',  ( 0.3996062992125986035, 0.1070741851644054776, -1.541994750656167978 ) ) ;
#27598 = CARTESIAN_POINT ( 'NONE',  ( -0.1974969037888706647, 0.3420746716998658843, -0.8005249343832020470 ) ) ;
#27599 = CARTESIAN_POINT ( 'NONE',  ( 0.4177787735907000366, 0.3937007874015748254, -1.874132239285499324 ) ) ;
#27600 = CARTESIAN_POINT ( 'NONE',  ( 0.3083989501312343062, -0.2845877964562159024, 0.3641732283464567677 ) ) ;
#27601 = CARTESIAN_POINT ( 'NONE',  ( -0.4724409448818890911, -0.1870078740157479769, 0.4822834645669291653 ) ) ;
#27602 = CARTESIAN_POINT ( 'NONE',  ( 1.213910761154856299, -0.6692913385826773087, -0.1292274648535924053 ) ) ;
#27603 = CARTESIAN_POINT ( 'NONE',  ( 0.2891555358219910499, -0.2891555358219909944, -1.592519685039370581 ) ) ;
#27604 = CARTESIAN_POINT ( 'NONE',  ( -0.1246719160104980823, -0.5511811023622048555, -0.09757992244046775898 ) ) ;
#27605 = CARTESIAN_POINT ( 'NONE',  ( -1.036745406824146176, -0.4281496062992124485, 0.4176697321401328655 ) ) ;
#27606 = CARTESIAN_POINT ( 'NONE',  ( 1.594488188976378673, 0.1660481256975885056, 0.3530559997133364547 ) ) ;
#27607 = CARTESIAN_POINT ( 'NONE',  ( -0.4091458600556402980, -0.2362204724409451284, -1.942257217847769057 ) ) ;
#27608 = CARTESIAN_POINT ( 'NONE',  ( 0.3876764156950328055, 0.05722014593897428725, -2.755905511811027164 ) ) ;
#27609 = ORIENTED_EDGE ( 'NONE', *, *, #73756, .F. ) ;
#27610 = ORIENTED_EDGE ( 'NONE', *, *, #40280, .T. ) ;
#27611 = CARTESIAN_POINT ( 'NONE',  ( -1.640419947506561060, -0.4281496062992127816, -0.4176697321401328100 ) ) ;
#27613 = CARTESIAN_POINT ( 'NONE',  ( -1.043307086614172041, -0.5400638737290844871, 0.3530559997133364547 ) ) ;
#27612 = CARTESIAN_POINT ( 'NONE',  ( -1.161417322834644716, 0.07958543189024085140, 0.2665933059059887866 ) ) ;
#27614 = CARTESIAN_POINT ( 'NONE',  ( -0.1958661417322836440, 0.3392501089628016664, -2.297880946685352033 ) ) ;
#27615 = CARTESIAN_POINT ( 'NONE',  ( -0.9576546141020345626, 0.004960608223778509643, -0.3437734562760191848 ) ) ;
#27616 = CARTESIAN_POINT ( 'NONE',  ( 1.069553805774278832, 0.2952755905511810774, -0.1292274648535930714 ) ) ;
#27617 = CARTESIAN_POINT ( 'NONE',  ( -1.200787401574802349, 0.1660481256975883668, -0.3530559997133364547 ) ) ;
#27618 = CARTESIAN_POINT ( 'NONE',  ( -0.1312335958005241554, 0.2306618581243848609, 0.2411417322834645549 ) ) ;
#27619 = CARTESIAN_POINT ( 'NONE',  ( -1.135170603674539924, 0.2952755905511810774, -0.1292274648535930714 ) ) ;
#27620 = CARTESIAN_POINT ( 'NONE',  ( -0.3917322834645669549, -0.1049643490035306603, 0.1843832020997374643 ) ) ;
#27621 = CARTESIAN_POINT ( 'NONE',  ( 0.4396325459317590445, -0.6692913385826771977, 0.1292274648535927661 ) ) ;
#27622 = CARTESIAN_POINT ( 'NONE',  ( -0.2867679344610365999, 0.2867679344610364889, -2.059055118110236116 ) ) ;
#27623 = CARTESIAN_POINT ( 'NONE',  ( -1.076115485564303809, -0.5023911411419708095, -0.1820866141732282451 ) ) ;
#27624 = ORIENTED_EDGE ( 'NONE', *, *, #40980, .F. ) ;
#27625 = CARTESIAN_POINT ( 'NONE',  ( -0.3420746716998659953, -0.1974969037888706647, -2.414698162729658648 ) ) ;
#27626 = ORIENTED_EDGE ( 'NONE', *, *, #72060, .F. ) ;
#27627 = DIRECTION ( 'NONE',  ( 0.000000000000000000, 1.000000000000000000, -0.000000000000000000 ) ) ;
#27628 = CIRCLE ( 'NONE', #65258, 0.2165354330708660069 ) ;
#27629 = CARTESIAN_POINT ( 'NONE',  ( -1.023622047244094002, -0.1870078740157480879, -0.4822834645669291653 ) ) ;
#27630 = CARTESIAN_POINT ( 'NONE',  ( -1.325459317585300889, 0.05413385826771666132, 0.4176697321401328100 ) ) ;
#27631 = CARTESIAN_POINT ( 'NONE',  ( 0.2925321140481932369, -0.2925321140481932369, -0.4133858267716534196 ) ) ;
#27632 = CARTESIAN_POINT ( 'NONE',  ( -1.489501312335957062, -0.3162353388693409650, -0.4822834645669289433 ) ) ;
#27633 = CARTESIAN_POINT ( 'NONE',  ( -1.535433070866141225, 0.2952755905511811885, 0.000000000000000000 ) ) ;
#27634 = CARTESIAN_POINT ( 'NONE',  ( -1.456692913385826182, 0.2952755905511811885, 0.000000000000000000 ) ) ;
#27635 = CARTESIAN_POINT ( 'NONE',  ( -1.646051170424378096, 0.000000000000000000, -0.3464511005275205946 ) ) ;
#27636 = CARTESIAN_POINT ( 'NONE',  ( 0.3917322834645670104, -0.1049643490035303411, -0.1961942257217848817 ) ) ;
#27637 = CARTESIAN_POINT ( 'NONE',  ( 0.006561679790026889343, -0.2845877964562161244, -0.3641732283464567121 ) ) ;
#27638 = CARTESIAN_POINT ( 'NONE',  ( -0.3392501089628019995, 0.1958661417322832277, -0.5833333333333334814 ) ) ;
#27639 = CARTESIAN_POINT ( 'NONE',  ( -0.8530183727034112984, -0.3690944881889765550, -0.3153832671262227771 ) ) ;
#27640 = CARTESIAN_POINT ( 'NONE',  ( -1.076115485564303809, -0.6046776061558809534, -0.2411417322834644161 ) ) ;
#27641 = CARTESIAN_POINT ( 'NONE',  ( 1.069553805774278610, -0.6692913385826771977, 0.1292274648535927661 ) ) ;
#27642 = CARTESIAN_POINT ( 'NONE',  ( -0.8267716535433065062, 0.2952755905511811885, 0.000000000000000000 ) ) ;
#27643 = CARTESIAN_POINT ( 'NONE',  ( 1.968503937007874072, 2.169649841009086334E-17, 5.524802951929911998 ) ) ;
#27644 = ORIENTED_EDGE ( 'NONE', *, *, #67069, .T. ) ;
#27645 = CARTESIAN_POINT ( 'NONE',  ( -0.8202099737532799750, 0.2952755905511810774, -0.1292274648535930714 ) ) ;
#27646 = CARTESIAN_POINT ( 'NONE',  ( 0.9580052493438326877, 0.05413385826771666132, 0.4176697321401328100 ) ) ;
#27647 = CARTESIAN_POINT ( 'NONE',  ( -1.430446194225721390, -0.3690944881889763329, 0.3153832671262228327 ) ) ;
#27648 = CARTESIAN_POINT ( 'NONE',  ( -1.614173228346456268, -0.6692913385826771977, 8.415575281601705876E-17 ) ) ;
#27649 = CARTESIAN_POINT ( 'NONE',  ( 0.4724409448818896462, 0.1265901696524990294, -1.384514435695537671 ) ) ;
#27650 = CARTESIAN_POINT ( 'NONE',  ( 2.131054703900698843, 1.408268389154267552, -0.4567427728026668410 ) ) ;
#27651 = CARTESIAN_POINT ( 'NONE',  ( -0.3917322834645669549, -0.1049643490035306603, -0.5104986876640419391 ) ) ;
#27652 = CARTESIAN_POINT ( 'NONE',  ( 0.3392501089628018329, 0.1958661417322835607, -2.578083989501311901 ) ) ;
#27653 = CARTESIAN_POINT ( 'NONE',  ( -0.2690288713910754526, -0.6692913385826771977, 0.1292274648535927661 ) ) ;
#27654 = CARTESIAN_POINT ( 'NONE',  ( -1.496062992125983815, -0.1870078740157479769, 0.3641732283464567677 ) ) ;
#27655 = CARTESIAN_POINT ( 'NONE',  ( -0.3996062992125985480, -7.340648628747423112E-17, -0.1161417322834645965 ) ) ;
#27657 = CARTESIAN_POINT ( 'NONE',  ( -0.4744094488189058989, 1.537401574803149984, 2.554262525012261253 ) ) ;
#27656 = CARTESIAN_POINT ( 'NONE',  ( -1.115485564304461219, -0.4281496062992124485, 0.4176697321401328655 ) ) ;
#27658 = CARTESIAN_POINT ( 'NONE',  ( -1.601049868766403650, -0.6046776061558807314, 0.2411417322834647770 ) ) ;
#27659 = CARTESIAN_POINT ( 'NONE',  ( -0.2821522309711278487, 0.2952755905511811885, 0.1292274648535926551 ) ) ;
#27660 = CARTESIAN_POINT ( 'NONE',  ( 0.3917322834645669549, 2.398668435337827645E-17, -0.04066309891632365059 ) ) ;
#27661 = CARTESIAN_POINT ( 'NONE',  ( 0.5183727034120741983, 0.1771653543307087075, -0.09757992244046823083 ) ) ;
#27662 = CARTESIAN_POINT ( 'NONE',  ( -0.3392501089628019995, 0.1958661417322832277, -0.1108923884514436548 ) ) ;
#27663 = CARTESIAN_POINT ( 'NONE',  ( 0.1706036745406830368, -0.3690944881889765550, -0.3153832671262227771 ) ) ;
#27664 = CARTESIAN_POINT ( 'NONE',  ( 0.7349081364829402885, -0.5023911411419708095, -0.1820866141732282451 ) ) ;
#27665 = CARTESIAN_POINT ( 'NONE',  ( 0.8727034120734912248, -0.3162353388693409650, -0.4822834645669289433 ) ) ;
#27666 = CARTESIAN_POINT ( 'NONE',  ( 0.3149606299212606708, -0.1870078740157480601, -0.3641732283464567677 ) ) ;
#27667 = CARTESIAN_POINT ( 'NONE',  ( -9.594673741351313045E-17, 0.3917322834645670104, -2.039370078740157410 ) ) ;
#27668 = CARTESIAN_POINT ( 'NONE',  ( -1.305774278215222184, 0.2952755905511811885, 0.1292274648535926551 ) ) ;
#27669 = CARTESIAN_POINT ( 'NONE',  ( -0.1902887139107604098, -0.5511811023622046335, 0.09757992244046803654 ) ) ;
#27670 = CARTESIAN_POINT ( 'NONE',  ( -1.115485564304461219, -0.004921259842519870586, -0.3153832671262229437 ) ) ;
#27671 = CARTESIAN_POINT ( 'NONE',  ( -0.3458507752293909498, 0.3458507752293907833, -0.4114173228346455491 ) ) ;
#27672 = VECTOR ( 'NONE', #36768, 39.37007874015748143 ) ;
#27673 = CARTESIAN_POINT ( 'NONE',  ( -0.5839895013123351797, -0.5511811023622046335, 0.09757992244046803654 ) ) ;
#27674 = CARTESIAN_POINT ( 'NONE',  ( 0.4410019072768808779, 1.362365694854143383, -1.490705430580310464 ) ) ;
#27675 = EDGE_CURVE ( 'NONE', #46125, #80970, #75677, .T. ) ;
#27676 = CARTESIAN_POINT ( 'NONE',  ( 0.04593175853018440641, -0.6692913385826771977, 0.1292274648535927661 ) ) ;
#27677 = CARTESIAN_POINT ( 'NONE',  ( -1.157146581871515012E-16, 0.4724409448818898682, -0.7066929133858268486 ) ) ;
#27678 = CARTESIAN_POINT ( 'NONE',  ( 0.6824146981627303710, 0.1283753931104746893, -0.1820866141732285504 ) ) ;
#27679 = CARTESIAN_POINT ( 'NONE',  ( -0.2427821522309703550, -0.08942795157528024563, -0.3641732283464568787 ) ) ;
#27680 = CARTESIAN_POINT ( 'NONE',  ( -0.1377952755905504645, -0.5400638737290845981, -0.3530559997133363437 ) ) ;
#27681 = CARTESIAN_POINT ( 'NONE',  ( -1.686351706036744558, 0.2952755905511810774, -0.1292274648535930714 ) ) ;
#27682 = CARTESIAN_POINT ( 'NONE',  ( -1.161417322834644716, 0.07958543189024085140, 0.2665933059059887866 ) ) ;
#27683 = CARTESIAN_POINT ( 'NONE',  ( -0.5314960629921123836, 2.559055118110236560, -3.900966923095591454 ) ) ;
#27684 = CARTESIAN_POINT ( 'NONE',  ( 0.4527559055118117182, 0.1660481256975883668, -0.3530559997133364547 ) ) ;
#27685 = ORIENTED_EDGE ( 'NONE', *, *, #70567, .F. ) ;
#27686 = CARTESIAN_POINT ( 'NONE',  ( -0.3996062992125984925, -0.1070741851644056858, -1.540026246719159886 ) ) ;
#27687 = CARTESIAN_POINT ( 'NONE',  ( 0.1958661417322836440, -0.3392501089628017219, -2.853674540682414662 ) ) ;
#27688 = B_SPLINE_CURVE_WITH_KNOTS ( 'NONE', 3,
 ( #24231, #69278, #36048, #35636 ),
 .UNSPECIFIED., .F., .F.,
 ( 4, 4 ),
 ( 1.999999999927407068E-07, 0.006970199999999936863 ),
 .UNSPECIFIED. ) ;
#27689 = CARTESIAN_POINT ( 'NONE',  ( -0.2427821522309703550, -0.08942795157528024563, -0.3641732283464568787 ) ) ;
#27690 = AXIS2_PLACEMENT_3D ( 'NONE', #36334, #4754, #48957 ) ;
#27691 = CARTESIAN_POINT ( 'NONE',  ( -1.423884514435694859, -0.05778040916215560624, -0.4822834645669293319 ) ) ;
#27692 = CARTESIAN_POINT ( 'NONE',  ( -1.614173228346455824, 0.1771653543307087630, 0.000000000000000000 ) ) ;
#27693 = CARTESIAN_POINT ( 'NONE',  ( -0.6299212598425332210, 2.755905511811024056, 3.886287458032460229 ) ) ;
#27694 = CARTESIAN_POINT ( 'NONE',  ( -0.7611548556430438595, 0.1283753931104748280, 0.1820866141732283561 ) ) ;
#27695 = CARTESIAN_POINT ( 'NONE',  ( -0.7742782152230965886, 0.009842519685039463617, 0.3409548833797002576 ) ) ;
#27696 = CARTESIAN_POINT ( 'NONE',  ( 0.6692913385826777528, 0.2952755905511811885, 0.000000000000000000 ) ) ;
#27697 = CARTESIAN_POINT ( 'NONE',  ( -9.787531504996567848E-17, 0.3996062992125986035, -8.919671568592925241E-18 ) ) ;
#27698 = CARTESIAN_POINT ( 'NONE',  ( -0.2867679344610365444, -0.2867679344610367664, -2.575478633367141779 ) ) ;
#27699 = CARTESIAN_POINT ( 'NONE',  ( -3.898836503597932435, 2.697992270790282365, -0.5314960629921259283 ) ) ;
#27700 = CARTESIAN_POINT ( 'NONE',  ( -1.627296587926508442, -0.6046776061558809534, -0.2411417322834644161 ) ) ;
#27701 = CARTESIAN_POINT ( 'NONE',  ( -1.167979002624671470, -0.4281496062992127816, -0.4176697321401328100 ) ) ;
#27702 = CARTESIAN_POINT ( 'NONE',  ( 1.417322834645670104, -0.1870078740157479769, 0.4822834645669291653 ) ) ;
#27703 = CARTESIAN_POINT ( 'NONE',  ( -0.3392501089628017219, -0.1958661417322836718, -2.499343832020997080 ) ) ;
#27704 = CARTESIAN_POINT ( 'NONE',  ( 1.456692913385827515, -0.5511811023622047445, 6.969142054262312111E-17 ) ) ;
#27705 = CARTESIAN_POINT ( 'NONE',  ( 0.4986876640419954376, -0.6046776061558809534, -0.2411417322834644161 ) ) ;
#27706 = CARTESIAN_POINT ( 'NONE',  ( -0.4921259842519677963, 0.1660481256975883668, -0.3530559997133364547 ) ) ;
#27707 = CARTESIAN_POINT ( 'NONE',  ( -2.530077749183804237, 2.729661042043246777, -0.5314960629921260393 ) ) ;
#27708 = CARTESIAN_POINT ( 'NONE',  ( 0.06764250034433770542, 1.722984403643211298E-16, -0.3954985857520063597 ) ) ;
#27709 = CARTESIAN_POINT ( 'NONE',  ( 0.9448818897637802916, -0.1870078740157479769, 0.3641732283464567677 ) ) ;
#27710 = VERTEX_POINT ( 'NONE', #12517 ) ;
#27711 = CARTESIAN_POINT ( 'NONE',  ( 0.2867679344610366554, -0.2867679344610365999, -0.2526439876978496257 ) ) ;
#27712 = ORIENTED_EDGE ( 'NONE', *, *, #9952, .T. ) ;
#27713 = CARTESIAN_POINT ( 'NONE',  ( -0.2362204724409442680, -0.1870078740157480879, -0.4822834645669291653 ) ) ;
#27714 = CARTESIAN_POINT ( 'NONE',  ( 1.358267716535433323, -0.5400638737290845981, -0.3530559997133363437 ) ) ;
#27715 = CARTESIAN_POINT ( 'NONE',  ( 0.07217847769028949700, -0.3162353388693405765, 0.4822834645669290543 ) ) ;
#27716 = CARTESIAN_POINT ( 'NONE',  ( -0.2690288713910754526, -0.5511811023622046335, 0.09757992244046803654 ) ) ;
#27717 = CARTESIAN_POINT ( 'NONE',  ( 1.043307086614173818, 0.1660481256975885056, 0.3530559997133364547 ) ) ;
#27718 = CARTESIAN_POINT ( 'NONE',  ( -0.7217847769028863381, -0.4281496062992124485, 0.4176697321401328655 ) ) ;
#27719 = CARTESIAN_POINT ( 'NONE',  ( -0.09186351706036689768, 0.05413385826771626580, -0.4176697321401330321 ) ) ;
#27720 = CARTESIAN_POINT ( 'NONE',  ( -0.7349081364829390672, 0.2306618581243847221, -0.2411417322834647770 ) ) ;
#27721 = CARTESIAN_POINT ( 'NONE',  ( 1.154855643044620184, 0.2306618581243847221, -0.2411417322834647770 ) ) ;
#27722 = CARTESIAN_POINT ( 'NONE',  ( 0.9776902887139113929, 0.2952755905511811885, 0.1292274648535926551 ) ) ;
#27723 = CARTESIAN_POINT ( 'NONE',  ( 1.141732283464567788, -0.6692913385826771977, 8.415575281601705876E-17 ) ) ;
#27724 = CARTESIAN_POINT ( 'NONE',  ( -0.1049643490035307020, 0.3917322834645669549, -0.7860892388451442558 ) ) ;
#27725 = CARTESIAN_POINT ( 'NONE',  ( -0.07874015748031421014, -0.1870078740157479769, 0.3641732283464567677 ) ) ;
#27726 = ORIENTED_EDGE ( 'NONE', *, *, #40829, .T. ) ;
#27727 = CARTESIAN_POINT ( 'NONE',  ( -0.2891555358219908833, -0.2891555358219912164, -1.003937007874015741 ) ) ;
#27728 = AXIS2_PLACEMENT_3D ( 'NONE', #38514, #6943, #12030 ) ;
#27729 = ORIENTED_EDGE ( 'NONE', *, *, #37854, .F. ) ;
#27730 = CARTESIAN_POINT ( 'NONE',  ( -0.9645669291338575535, -0.4536011799217367080, 0.2665933059059888421 ) ) ;
#27731 = AXIS2_PLACEMENT_3D ( 'NONE', #3126, #3955, #41011 ) ;
#27732 = CARTESIAN_POINT ( 'NONE',  ( -0.1115485564304453947, -0.6692913385826771977, 0.1292274648535927661 ) ) ;
#27733 = CARTESIAN_POINT ( 'NONE',  ( 1.595398199321655275, 0.4829664696085563258, -0.1559797534342493575 ) ) ;
#27734 = CARTESIAN_POINT ( 'NONE',  ( -0.2821522309711278487, 0.2952755905511811885, 0.1292274648535926551 ) ) ;
#27735 = CARTESIAN_POINT ( 'NONE',  ( -0.4527559055118102749, 0.1660481256975885056, 0.3530559997133364547 ) ) ;
#27736 = CARTESIAN_POINT ( 'NONE',  ( -0.6758530183727028406, 0.2952755905511811885, 0.1292274648535926551 ) ) ;
#27737 = CARTESIAN_POINT ( 'NONE',  ( -1.030183727034119867, -0.05778040916215560624, -0.4822834645669293319 ) ) ;
#27738 = CARTESIAN_POINT ( 'NONE',  ( 1.535433070866142558, 0.1771653543307087630, 0.000000000000000000 ) ) ;
#27739 = CARTESIAN_POINT ( 'NONE',  ( -1.476377952755905110, 0.1660481256975885056, 0.3530559997133364547 ) ) ;
#27740 = CARTESIAN_POINT ( 'NONE',  ( 0.2952755905511810774, 0.01196537350834422572, 5.524802951929911110 ) ) ;
#27741 = CARTESIAN_POINT ( 'NONE',  ( 0.3805774278215230400, -0.004921259842519870586, -0.3153832671262229437 ) ) ;
#27742 = CARTESIAN_POINT ( 'NONE',  ( 0.07217847769028949700, -0.3162353388693405765, 0.4822834645669290543 ) ) ;
#27743 = CARTESIAN_POINT ( 'NONE',  ( 0.4790026246719168435, -0.3162353388693409650, -0.4822834645669289433 ) ) ;
#27744 = ORIENTED_EDGE ( 'NONE', *, *, #4245, .T. ) ;
#27745 = CARTESIAN_POINT ( 'NONE',  ( 0.3460692066303959202, 0.1998031496062993295, -1.863517060367454015 ) ) ;
#27746 = CARTESIAN_POINT ( 'NONE',  ( -2.611754389584905578, 1.697151583350148041, 0.4469586986359056491 ) ) ;
#27747 = CARTESIAN_POINT ( 'NONE',  ( 0.1070741851644053388, 0.3996062992125986035, -1.015091863517060267 ) ) ;
#27748 = CARTESIAN_POINT ( 'NONE',  ( 0.3996062992125986035, -0.1070741851644052972, -0.3458005249343831244 ) ) ;
#27749 = CARTESIAN_POINT ( 'NONE',  ( -0.3674540682414692561, -0.6046776061558809534, -0.2411417322834644161 ) ) ;
#27750 = CARTESIAN_POINT ( 'NONE',  ( 0.1265901696524990294, -0.4724409448818896462, -0.08530183727034119923 ) ) ;
#27751 = CARTESIAN_POINT ( 'NONE',  ( 0.3917322834645669549, 0.1049643490035304660, -2.256561679790026531 ) ) ;
#27752 = CARTESIAN_POINT ( 'NONE',  ( -1.476377952755905110, 0.07958543189024085140, 0.2665933059059887866 ) ) ;
#27753 = CARTESIAN_POINT ( 'NONE',  ( 0.7742782152230978099, -0.4281496062992124485, 0.4176697321401328655 ) ) ;
#27754 = CARTESIAN_POINT ( 'NONE',  ( 0.8792650918635177559, 0.05413385826771666132, 0.4176697321401328100 ) ) ;
#27755 = CARTESIAN_POINT ( 'NONE',  ( -0.1706036745406816491, -0.004921259842519870586, -0.3153832671262229437 ) ) ;
#27756 = CARTESIAN_POINT ( 'NONE',  ( 0.3608923884514443348, 0.2952755905511810774, -0.1292274648535930714 ) ) ;
#27757 = CARTESIAN_POINT ( 'NONE',  ( 0.1265901696524989462, 0.4724409448818897572, -1.802493438320209584 ) ) ;
#27758 = CARTESIAN_POINT ( 'NONE',  ( 0.01312335958005323398, -0.3690944881889765550, -0.3153832671262227771 ) ) ;
#27759 = CARTESIAN_POINT ( 'NONE',  ( -0.1706036745406816491, -0.4281496062992124485, 0.4176697321401328655 ) ) ;
#27760 = CARTESIAN_POINT ( 'NONE',  ( -0.3420746716998660508, -0.1974969037888706924, -1.231627296587926468 ) ) ;
#27761 = CARTESIAN_POINT ( 'NONE',  ( -1.640419947506561060, -0.4281496062992127816, -0.4176697321401328100 ) ) ;
#27762 = CARTESIAN_POINT ( 'NONE',  ( -0.06561679790026180015, -0.3690944881889765550, -0.3153832671262227771 ) ) ;
#27763 = CARTESIAN_POINT ( 'NONE',  ( 1.561679790026247350, -0.004921259842519870586, -0.3153832671262229437 ) ) ;
#27764 = CARTESIAN_POINT ( 'NONE',  ( -0.9251968503937002541, 0.1660481256975885056, 0.3530559997133364547 ) ) ;
#27765 = CARTESIAN_POINT ( 'NONE',  ( -0.5708661417322825615, -0.4536011799217367080, 0.2665933059059888421 ) ) ;
#27766 = CARTESIAN_POINT ( 'NONE',  ( -1.157146581871515012E-16, 0.4724409448818898682, -2.281496062992125928 ) ) ;
#27767 = CARTESIAN_POINT ( 'NONE',  ( -0.8923884514435688198, 0.2306618581243847221, -0.2411417322834647770 ) ) ;
#27768 = CARTESIAN_POINT ( 'NONE',  ( -0.4724409448818890911, -0.1870078740157480879, -0.4822834645669291653 ) ) ;
#27769 = CARTESIAN_POINT ( 'NONE',  ( 0.1181102362204730916, 0.2952755905511811885, 0.000000000000000000 ) ) ;
#27770 = CARTESIAN_POINT ( 'NONE',  ( -0.2925321140481932369, 0.2925321140481931259, -2.616141732283464805 ) ) ;
#27771 = EDGE_CURVE ( 'NONE', #44890, #9475, #63273, .T. ) ;
#27772 = CARTESIAN_POINT ( 'NONE',  ( 0.1049643490035304522, -0.3917322834645668994, -1.897618479493751398 ) ) ;
#27773 = CARTESIAN_POINT ( 'NONE',  ( -2.001206130748376832, 1.231544801320217264, -0.3638227417423721133 ) ) ;
#27774 = CARTESIAN_POINT ( 'NONE',  ( 0.7283464566929143125, 0.07958543189024085140, 0.2665933059059887866 ) ) ;
#27775 = CARTESIAN_POINT ( 'NONE',  ( 1.496062992125984703, -0.1870078740157480879, -0.4822834645669291653 ) ) ;
#27776 = CARTESIAN_POINT ( 'NONE',  ( -1.036745406824146176, -0.004921259842519870586, -0.3153832671262229437 ) ) ;
#27777 = CARTESIAN_POINT ( 'NONE',  ( 1.102362204724410155, -0.1870078740157480879, -0.4822834645669291653 ) ) ;
#27778 = CARTESIAN_POINT ( 'NONE',  ( -1.312335958005248715, -0.5023911411419708095, -0.1820866141732282451 ) ) ;
#27779 = EDGE_CURVE ( 'NONE', #74332, #52953, #5373, .T. ) ;
#27780 = CARTESIAN_POINT ( 'NONE',  ( -0.3608923884514428360, -0.6692913385826773087, -0.1292274648535924053 ) ) ;
#27781 = CARTESIAN_POINT ( 'NONE',  ( 0.2165354330708668673, -0.4536011799217367080, 0.2665933059059888421 ) ) ;
#27782 = CARTESIAN_POINT ( 'NONE',  ( -1.948818897637795367, 0.000000000000000000, 5.701968306260621233 ) ) ;
#27783 = CARTESIAN_POINT ( 'NONE',  ( 1.253280839895013710, -0.2845877964562159024, 0.3641732283464567677 ) ) ;
#27784 = CARTESIAN_POINT ( 'NONE',  ( 0.1968503937007881344, -0.6692913385826771977, 8.415575281601705876E-17 ) ) ;
#27785 = CARTESIAN_POINT ( 'NONE',  ( 4.893765752498283308E-17, -0.3996062992125985480, -0.4704724409448819422 ) ) ;
#27786 = CARTESIAN_POINT ( 'NONE',  ( -0.5971128608923877978, 0.2952755905511811885, 0.1292274648535926551 ) ) ;
#27787 = VECTOR ( 'NONE', #22893, 39.37007874015748143 ) ;
#27788 = CARTESIAN_POINT ( 'NONE',  ( 0.3917322834645670104, 2.398668435337828261E-17, -1.620078740157480324 ) ) ;
#27789 = CARTESIAN_POINT ( 'NONE',  ( 1.161417322834646271, 0.07958543189024071263, -0.2665933059059888421 ) ) ;
#27791 = CARTESIAN_POINT ( 'NONE',  ( 0.3018372703412079971, 0.05413385826771626580, -0.4176697321401330321 ) ) ;
#27790 = AXIS2_PLACEMENT_3D ( 'NONE', #73286, #29480, #41693 ) ;
#27792 = VECTOR ( 'NONE', #4142, 39.37007874015748143 ) ;
#27793 = CARTESIAN_POINT ( 'NONE',  ( -0.2362204724409440182, -0.1870078740157479769, 0.4822834645669291653 ) ) ;
#27794 = CARTESIAN_POINT ( 'NONE',  ( 0.06561679790026316017, -0.3690944881889763329, 0.3153832671262228327 ) ) ;
#27795 = CARTESIAN_POINT ( 'NONE',  ( -1.559171609364246924, 0.000000000000000000, 0.1028181436694137613 ) ) ;
#27796 = CARTESIAN_POINT ( 'NONE',  ( -0.01312335958005186876, -0.004921259842519870586, -0.3153832671262229437 ) ) ;
#27797 = CARTESIAN_POINT ( 'NONE',  ( 0.1968503937007881344, -0.6692913385826771977, 8.415575281601705876E-17 ) ) ;
#27798 = CARTESIAN_POINT ( 'NONE',  ( -0.8792650918635160906, -0.004921259842519870586, -0.3153832671262229437 ) ) ;
#27799 = CARTESIAN_POINT ( 'NONE',  ( 0.1998031496062994128, -0.3460692066303957537, -1.113517060367454015 ) ) ;
#27800 = CARTESIAN_POINT ( 'NONE',  ( -1.187664041994749731, -0.3162353388693405765, 0.4822834645669290543 ) ) ;
#27801 = DIRECTION ( 'NONE',  ( 0.000000000000000000, -0.4999999999999998890, 0.8660254037844385966 ) ) ;
#27802 = ORIENTED_EDGE ( 'NONE', *, *, #10106, .F. ) ;
#27803 = CARTESIAN_POINT ( 'NONE',  ( -0.9186351706036736120, 0.1283753931104748280, 0.1820866141732283561 ) ) ;
#27804 = CARTESIAN_POINT ( 'NONE',  ( -0.07217847769028813698, -0.3162353388693409650, -0.4822834645669289433 ) ) ;
#27805 = CARTESIAN_POINT ( 'NONE',  ( -1.574803149606298636, -0.1870078740157479769, 0.4822834645669291653 ) ) ;
#27806 = CARTESIAN_POINT ( 'NONE',  ( -0.7283464566929126471, -0.5400638737290844871, 0.3530559997133364547 ) ) ;
#27807 = DIRECTION ( 'NONE',  ( 1.000000000000000000, 0.000000000000000000, 3.455050906509825972E-15 ) ) ;
#27809 = CARTESIAN_POINT ( 'NONE',  ( 1.128608923884514947, 0.2306618581243848609, 0.2411417322834645549 ) ) ;
#27808 = CARTESIAN_POINT ( 'NONE',  ( -0.8777275986338654024, 0.02791078216816347476, -0.4328096321851898631 ) ) ;
#27810 = CARTESIAN_POINT ( 'NONE',  ( 0.7677165354330716118, 0.1660481256975883668, -0.3530559997133364547 ) ) ;
#27811 = CARTESIAN_POINT ( 'NONE',  ( -0.3917322834645669549, -0.1049643490035306603, -2.715223097112860806 ) ) ;
#27812 = CARTESIAN_POINT ( 'NONE',  ( 1.482939632545932307, 0.05413385826771626580, -0.4176697321401330321 ) ) ;
#27813 = CARTESIAN_POINT ( 'NONE',  ( -1.233595800524933894, 0.2306618581243848609, 0.2411417322834645549 ) ) ;
#27814 = CARTESIAN_POINT ( 'NONE',  ( 0.1998031496062992740, 0.3460692066303959757, -0.4593175853018372501 ) ) ;
#27815 = ORIENTED_EDGE ( 'NONE', *, *, #57015, .T. ) ;
#27816 = CARTESIAN_POINT ( 'NONE',  ( -0.3083989501312330295, -0.2845877964562161244, -0.3641732283464567121 ) ) ;
#27817 = CARTESIAN_POINT ( 'NONE',  ( -0.1958661417322834220, -0.3392501089628018884, -2.262467191601049699 ) ) ;
#27818 = ORIENTED_EDGE ( 'NONE', *, *, #17674, .F. ) ;
#27819 = CARTESIAN_POINT ( 'NONE',  ( 0.9711286089238851948, 0.2306618581243848609, 0.2411417322834645549 ) ) ;
#27820 = CARTESIAN_POINT ( 'NONE',  ( 0.04593175853018440641, 0.2952755905511810774, -0.1292274648535930714 ) ) ;
#27821 = CARTESIAN_POINT ( 'NONE',  ( -0.6758530183727028406, 0.2952755905511811885, 0.1292274648535926551 ) ) ;
#27822 = CARTESIAN_POINT ( 'NONE',  ( 1.443569553805774897, -0.6046776061558809534, -0.2411417322834644161 ) ) ;
#27823 = CARTESIAN_POINT ( 'NONE',  ( -0.6692913385826764205, 0.1771653543307087630, 0.000000000000000000 ) ) ;
#27824 = CARTESIAN_POINT ( 'NONE',  ( -0.4418084573054544273, 1.710857756487497161, -2.620814421478965706 ) ) ;
#27825 = CARTESIAN_POINT ( 'NONE',  ( 0.1377952755905518800, 0.1660481256975883668, -0.3530559997133364547 ) ) ;
#27826 = CARTESIAN_POINT ( 'NONE',  ( 0.6955380577427828781, -0.004921259842519870586, -0.3153832671262229437 ) ) ;
#27827 = CARTESIAN_POINT ( 'NONE',  ( -0.5643044619422565855, -0.4281496062992124485, 0.4176697321401328655 ) ) ;
#27828 = CARTESIAN_POINT ( 'NONE',  ( -0.3392501089628018329, -0.1958661417322836440, -1.707329765582990211 ) ) ;
#27829 = CARTESIAN_POINT ( 'NONE',  ( -1.108923884514435132, -0.05778040916215560624, -0.4822834645669293319 ) ) ;
#27830 = CARTESIAN_POINT ( 'NONE',  ( 0.5314960629921349211, 2.729656593086051242, -2.556891438210025846 ) ) ;
#27831 = CARTESIAN_POINT ( 'NONE',  ( 1.246719160104987623, 0.05413385826771626580, -0.4176697321401330321 ) ) ;
#27832 = CARTESIAN_POINT ( 'NONE',  ( 1.384514435695538559, 0.1771653543307087075, -0.09757992244046823083 ) ) ;
#27833 = ORIENTED_EDGE ( 'NONE', *, *, #15253, .F. ) ;
#27834 = CARTESIAN_POINT ( 'NONE',  ( 0.1974969037888706369, -0.3420746716998659953, 0.06561679790026241077 ) ) ;
#27835 = CARTESIAN_POINT ( 'NONE',  ( -0.1509186351706028884, -0.3162353388693409650, -0.4822834645669289433 ) ) ;
#27836 = ORIENTED_EDGE ( 'NONE', *, *, #58308, .T. ) ;
#27837 = CARTESIAN_POINT ( 'NONE',  ( 0.7742782152230978099, -0.3690944881889763329, 0.3153832671262228327 ) ) ;
#27838 = CARTESIAN_POINT ( 'NONE',  ( -1.030183727034119867, -0.05778040916215560624, -0.4822834645669293319 ) ) ;
#27839 = CARTESIAN_POINT ( 'NONE',  ( 0.9973753280839902091, 0.2306618581243847221, -0.2411417322834647770 ) ) ;
#27840 = CARTESIAN_POINT ( 'NONE',  ( 0.7874015748031503170, -0.1870078740157479769, 0.4822834645669291653 ) ) ;
#27841 = CARTESIAN_POINT ( 'NONE',  ( 0.3608923884514443348, 0.2952755905511810774, -0.1292274648535930714 ) ) ;
#27842 = EDGE_CURVE ( 'NONE', #60402, #50774, #37729, .T. ) ;
#27843 = CARTESIAN_POINT ( 'NONE',  ( -0.4855643044619415427, 0.05413385826771626580, -0.4176697321401330321 ) ) ;
#27844 = CARTESIAN_POINT ( 'NONE',  ( -0.3917322834645669549, -0.1049643490035306603, -1.705380577427821898 ) ) ;
#27845 = CARTESIAN_POINT ( 'NONE',  ( 1.574803149606299746, -0.1870078740157479769, 0.3641732283464567677 ) ) ;
#27846 = CARTESIAN_POINT ( 'NONE',  ( -0.4461942257217840213, -0.6046776061558809534, -0.2411417322834644161 ) ) ;
#27847 = CARTESIAN_POINT ( 'NONE',  ( -0.5708661417322825615, -0.4536011799217367080, 0.2665933059059888421 ) ) ;
#27848 = CARTESIAN_POINT ( 'NONE',  ( 1.686351706036745890, 0.2952755905511811885, 0.1292274648535926551 ) ) ;
#27849 = CARTESIAN_POINT ( 'NONE',  ( 2.795275590551181466, 0.7480314960629931287, -2.695814348275282069E-16 ) ) ;
#27850 = CARTESIAN_POINT ( 'NONE',  ( -0.4658792650918627265, -0.05778040916215522460, 0.4822834645669289988 ) ) ;
#27851 = CARTESIAN_POINT ( 'NONE',  ( -0.5314960629921394730, 2.712230453466948799, 3.892840969167623566 ) ) ;
#27852 = AXIS2_PLACEMENT_3D ( 'NONE', #26983, #69930, #52228 ) ;
#27853 = CARTESIAN_POINT ( 'NONE',  ( 0.5183727034120741983, 0.2952755905511810774, -0.1292274648535930714 ) ) ;
#27854 = CARTESIAN_POINT ( 'NONE',  ( 0.1070741851644053527, 0.3996062992125986590, -2.040682414698162361 ) ) ;
#27855 = CARTESIAN_POINT ( 'NONE',  ( 3.935132539805148433, 1.078793357725790658, 0.1224154028705949776 ) ) ;
#27856 = AXIS2_PLACEMENT_3D ( 'NONE', #6318, #77454, #59332 ) ;
#27857 = CARTESIAN_POINT ( 'NONE',  ( -0.01312335958005186876, 0.05413385826771626580, -0.4176697321401330321 ) ) ;
#27858 = VECTOR ( 'NONE', #39218, 39.37007874015748143 ) ;
#27859 = CARTESIAN_POINT ( 'NONE',  ( 0.9842519685039378130, -0.5511811023622047445, 6.969142054262312111E-17 ) ) ;
#27860 = CARTESIAN_POINT ( 'NONE',  ( 0.2362204724409451007, -0.4091458600556402980, -0.7985564304461942875 ) ) ;
#27861 = CARTESIAN_POINT ( 'NONE',  ( 1.023622047244095334, -0.1870078740157479769, 0.3641732283464567677 ) ) ;
#27862 = CARTESIAN_POINT ( 'NONE',  ( 1.062992125984252745, -0.6692913385826771977, 8.415575281601705876E-17 ) ) ;
#27863 = CARTESIAN_POINT ( 'NONE',  ( 0.3420746716998660508, 0.1974969037888705814, -0.2080052493438320771 ) ) ;
#27864 = CARTESIAN_POINT ( 'NONE',  ( -0.4068241469816267775, 0.05413385826771626580, -0.4176697321401330321 ) ) ;
#27865 = CARTESIAN_POINT ( 'NONE',  ( -1.581364829396324945, -0.05778040916215560624, -0.4822834645669293319 ) ) ;
#27866 = CARTESIAN_POINT ( 'NONE',  ( -1.640419947506561060, -0.4281496062992127816, -0.4176697321401328100 ) ) ;
#27867 = CARTESIAN_POINT ( 'NONE',  ( -0.1312335958005241554, 0.2306618581243848609, 0.2411417322834645549 ) ) ;
#27868 = CARTESIAN_POINT ( 'NONE',  ( -0.2891555358219911054, 0.2891555358219909388, -0.5688976377952756902 ) ) ;
#27869 = CARTESIAN_POINT ( 'NONE',  ( 1.102362204724410155, -0.1870078740157480879, -0.4822834645669291653 ) ) ;
#27870 = CARTESIAN_POINT ( 'NONE',  ( 0.4461942257217855201, -0.6046776061558807314, 0.2411417322834647770 ) ) ;
#27871 = CARTESIAN_POINT ( 'NONE',  ( 0.6167979002624679463, -0.004921259842519870586, -0.3153832671262229437 ) ) ;
#27872 = CARTESIAN_POINT ( 'NONE',  ( -0.03156192328343619680, 1.063779846874849389, -1.121713509234345540 ) ) ;
#27873 = CARTESIAN_POINT ( 'NONE',  ( 0.2427821522309719648, -0.08942795157527998196, 0.3641732283464567121 ) ) ;
#27874 = CARTESIAN_POINT ( 'NONE',  ( -0.03443470937339728616, 0.2755905511811023723, -1.537015892239756099 ) ) ;
#27875 = CARTESIAN_POINT ( 'NONE',  ( 0.3460692066303958092, 0.1998031496062993018, -1.152887139107611425 ) ) ;
#27876 = CARTESIAN_POINT ( 'NONE',  ( 0.8989501312335964611, 0.2952755905511811885, 0.1292274648535926551 ) ) ;
#27877 = CARTESIAN_POINT ( 'NONE',  ( -0.1049643490035307020, 0.3917322834645669549, -1.258530183727033958 ) ) ;
#27878 = LINE ( 'NONE', #34194, #14350 ) ;
#27879 = CARTESIAN_POINT ( 'NONE',  ( -0.03443470937339727228, 0.2929341459200028863, -1.438590695389362573 ) ) ;
#27880 = CARTESIAN_POINT ( 'NONE',  ( 0.05249343832021075018, 0.1283753931104746893, -0.1820866141732285504 ) ) ;
#27881 = CARTESIAN_POINT ( 'NONE',  ( 0.3215223097112867578, -0.3162353388693409650, -0.4822834645669289433 ) ) ;
#27882 = CARTESIAN_POINT ( 'NONE',  ( 1.213910761154856299, 0.1771653543307087630, 0.09757992244046791164 ) ) ;
#27883 = CARTESIAN_POINT ( 'NONE',  ( -1.246719160104986512, -0.004921259842519576551, 0.3153832671262227771 ) ) ;
#27884 = CARTESIAN_POINT ( 'NONE',  ( -0.9317585301837263412, 0.05413385826771666132, 0.4176697321401328100 ) ) ;
#27885 = CARTESIAN_POINT ( 'NONE',  ( -1.548556430446193399, 0.2306618581243848609, 0.2411417322834645549 ) ) ;
#27886 = CARTESIAN_POINT ( 'NONE',  ( 0.4790026246719168435, -0.3162353388693409650, -0.4822834645669289433 ) ) ;
#27887 = CARTESIAN_POINT ( 'NONE',  ( 1.548556430446194954, 0.2306618581243847221, -0.2411417322834647770 ) ) ;
#27888 = DIRECTION ( 'NONE',  ( -1.000000000000000000, 0.000000000000000000, 0.000000000000000000 ) ) ;
#27889 = CARTESIAN_POINT ( 'NONE',  ( 0.7808398950131240079, -0.3162353388693405765, 0.4822834645669290543 ) ) ;
#27890 = CARTESIAN_POINT ( 'NONE',  ( 0.3458507752293908943, 0.3458507752293908943, -2.734251968503936148 ) ) ;
#27891 = CARTESIAN_POINT ( 'NONE',  ( 0.4585058784351956906, 1.414602624921270646, 3.910220467301401825 ) ) ;
#27892 = CARTESIAN_POINT ( 'NONE',  ( 1.253280839895013710, -0.05778040916215560624, -0.4822834645669293319 ) ) ;
#27893 = CARTESIAN_POINT ( 'NONE',  ( -1.364829396325458521, 0.1283753931104746893, -0.1820866141732285504 ) ) ;
#27894 = CARTESIAN_POINT ( 'NONE',  ( 1.082677165354331228, 0.07958543189024071263, -0.2665933059059888421 ) ) ;
#27895 = CARTESIAN_POINT ( 'NONE',  ( -1.286089238845143479, 0.1283753931104746893, -0.1820866141732285504 ) ) ;
#27896 = CARTESIAN_POINT ( 'NONE',  ( -0.8464566929133852113, 0.07958543189024085140, 0.2665933059059887866 ) ) ;
#27897 = CARTESIAN_POINT ( 'NONE',  ( 0.5643044619422579178, -0.3690944881889765550, -0.3153832671262227771 ) ) ;
#27898 = CARTESIAN_POINT ( 'NONE',  ( 0.2362204724409456558, -0.1870078740157479769, 0.4822834645669291653 ) ) ;
#27899 = CARTESIAN_POINT ( 'NONE',  ( 1.305774278215223960, 0.2952755905511810774, -0.1292274648535930714 ) ) ;
#27900 = CARTESIAN_POINT ( 'NONE',  ( 0.1246719160104994284, 0.2952755905511810774, -0.1292274648535930714 ) ) ;
#27901 = EDGE_CURVE ( 'NONE', #83014, #43155, #78358, .T. ) ;
#27902 = CARTESIAN_POINT ( 'NONE',  ( 0.2493438320209980519, -0.3690944881889765550, -0.3153832671262227771 ) ) ;
#27903 = CARTESIAN_POINT ( 'NONE',  ( 1.122047244094488860, 0.1660481256975885056, 0.3530559997133364547 ) ) ;
#27904 = CARTESIAN_POINT ( 'NONE',  ( -1.627296587926508442, 0.2306618581243848609, 0.2411417322834645549 ) ) ;
#27905 = CARTESIAN_POINT ( 'NONE',  ( -0.9645669291338575535, -0.5400638737290844871, 0.3530559997133364547 ) ) ;
#27906 = CARTESIAN_POINT ( 'NONE',  ( 0.2925321140481932369, -0.2925321140481931814, -0.7283464566929134243 ) ) ;
#27907 = CARTESIAN_POINT ( 'NONE',  ( -0.3104009647183427756, 1.295819047631763254, 0.04186094777090585556 ) ) ;
#27908 = CIRCLE ( 'NONE', #23873, 0.1771653543307085410 ) ;
#27909 = CARTESIAN_POINT ( 'NONE',  ( -0.7152230971128602510, -0.3162353388693405765, 0.4822834645669290543 ) ) ;
#27910 = CARTESIAN_POINT ( 'NONE',  ( -0.2034120734908131112, -0.6692913385826773087, -0.1292274648535924053 ) ) ;
#27911 = CARTESIAN_POINT ( 'NONE',  ( -0.2925321140481930704, -0.2925321140481933480, -2.578740157480315265 ) ) ;
#27912 = CARTESIAN_POINT ( 'NONE',  ( 0.3420746716998659953, 0.1974969037888705536, -2.178477690288714186 ) ) ;
#27913 = ORIENTED_EDGE ( 'NONE', *, *, #49898, .T. ) ;
#27914 = CARTESIAN_POINT ( 'NONE',  ( 0.1049643490035304938, -0.3917322834645669549, -0.8648293963254591876 ) ) ;
#27915 = DIRECTION ( 'NONE',  ( -2.956072690630991240E-16, 1.000000000000000000, 5.002896285981958034E-32 ) ) ;
#27916 = CARTESIAN_POINT ( 'NONE',  ( -1.292650918635170010, -0.5511811023622046335, 0.09757992244046803654 ) ) ;
#27917 = CARTESIAN_POINT ( 'NONE',  ( -0.1049643490035302024, -0.3917322834645671215, -1.166666666666666519 ) ) ;
#27918 = CARTESIAN_POINT ( 'NONE',  ( -1.456692913385826182, -0.6692913385826771977, 8.415575281601705876E-17 ) ) ;
#27919 = CARTESIAN_POINT ( 'NONE',  ( 0.3949938075777409963, 2.418639510665530743E-17, -2.872047244094488416 ) ) ;
#27920 = CARTESIAN_POINT ( 'NONE',  ( -0.1312335958005241554, -0.6046776061558809534, -0.2411417322834644161 ) ) ;
#27921 = CARTESIAN_POINT ( 'NONE',  ( -0.3937007874015740483, -0.1870078740157480601, -0.3641732283464567677 ) ) ;
#27922 = EDGE_CURVE ( 'NONE', #49068, #11380, #24057, .T. ) ;
#27923 = CARTESIAN_POINT ( 'NONE',  ( 0.8070866141732288002, 0.1660481256975885056, 0.3530559997133364547 ) ) ;
#27924 = CARTESIAN_POINT ( 'NONE',  ( 0.4724409448818904789, -0.1870078740157479769, 0.4822834645669291653 ) ) ;
#27925 = CARTESIAN_POINT ( 'NONE',  ( 0.06292302554185959240, 1.066149053166906002, 1.120702161501667238 ) ) ;
#27926 = CARTESIAN_POINT ( 'NONE',  ( 0.3996062992125986035, 2.446882876249141962E-17, -2.637795275590551380 ) ) ;
#27927 = CARTESIAN_POINT ( 'NONE',  ( 0.2867679344610366554, 0.2867679344610366554, -1.394376271162416359 ) ) ;
#27928 = CARTESIAN_POINT ( 'NONE',  ( 1.279527559055118724, -0.5400638737290845981, -0.3530559997133363437 ) ) ;
#27929 = CARTESIAN_POINT ( 'NONE',  ( -0.06561679790026180015, -0.4281496062992127816, -0.4176697321401328100 ) ) ;
#27930 = CARTESIAN_POINT ( 'NONE',  ( -1.095800524934382292, -0.3162353388693409650, -0.4822834645669289433 ) ) ;
#27931 = CARTESIAN_POINT ( 'NONE',  ( -1.561679790026246017, -0.4281496062992127816, -0.4176697321401328100 ) ) ;
#27932 = CARTESIAN_POINT ( 'NONE',  ( 0.8661417322834653598, -0.1870078740157479769, 0.4822834645669291653 ) ) ;
#27933 = CARTESIAN_POINT ( 'NONE',  ( -0.1049643490035302024, -0.3917322834645671215, -0.6292650918635172008 ) ) ;
#27934 = CARTESIAN_POINT ( 'NONE',  ( 0.1312335958005255154, -0.6046776061558807314, 0.2411417322834647770 ) ) ;
#27935 = CARTESIAN_POINT ( 'NONE',  ( 0.4921259842519691285, -0.5400638737290845981, -0.3530559997133363437 ) ) ;
#27936 = CARTESIAN_POINT ( 'NONE',  ( -0.02624671916010428221, 0.2306618581243847221, -0.2411417322834647770 ) ) ;
#27937 = CARTESIAN_POINT ( 'NONE',  ( 0.7217847769028878924, -0.004921259842519576551, 0.3153832671262227771 ) ) ;
#27938 = CARTESIAN_POINT ( 'NONE',  ( -1.391076115485563758, 0.2306618581243848609, 0.2411417322834645549 ) ) ;
#27939 = CARTESIAN_POINT ( 'NONE',  ( -1.620734908136482577, -0.6692913385826773087, -0.1292274648535924053 ) ) ;
#27940 = CARTESIAN_POINT ( 'NONE',  ( 0.6036745406824153282, -0.6046776061558807314, 0.2411417322834647770 ) ) ;
#27941 = CARTESIAN_POINT ( 'NONE',  ( -0.2362204724409451284, 0.4091458600556402425, -0.5623359580052492701 ) ) ;
#27942 = CARTESIAN_POINT ( 'NONE',  ( 0.2867679344610365999, -0.2867679344610365444, -1.980314960629921073 ) ) ;
#27943 = ORIENTED_EDGE ( 'NONE', *, *, #49631, .F. ) ;
#27944 = CARTESIAN_POINT ( 'NONE',  ( 4.893765752498283924E-17, -0.3996062992125986035, -0.3937007874015748254 ) ) ;
#27945 = ORIENTED_EDGE ( 'NONE', *, *, #31423, .T. ) ;
#27946 = CARTESIAN_POINT ( 'NONE',  ( 1.312335958005250269, -0.6046776061558807314, 0.2411417322834647770 ) ) ;
#27947 = CARTESIAN_POINT ( 'NONE',  ( 0.5643044619422579178, -0.3690944881889765550, -0.3153832671262227771 ) ) ;
#27948 = DIRECTION ( 'NONE',  ( -0.000000000000000000, -1.000000000000000000, -0.000000000000000000 ) ) ;
#27949 = CARTESIAN_POINT ( 'NONE',  ( -1.559171609364246924, 0.3937007874015748254, 0.4177787735906735578 ) ) ;
#27950 = CARTESIAN_POINT ( 'NONE',  ( 0.000000000000000000, 2.559055118110236560, 0.000000000000000000 ) ) ;
#27951 = CARTESIAN_POINT ( 'NONE',  ( -0.2867679344610364334, -0.2867679344610367109, -1.403543307086614123 ) ) ;
#27952 = CARTESIAN_POINT ( 'NONE',  ( 0.4423023948155340168, 1.709706175544221329, -3.912088937888734907 ) ) ;
#27953 = CARTESIAN_POINT ( 'NONE',  ( -0.1246719160104980823, 0.2952755905511811885, 0.1292274648535926551 ) ) ;
#27954 = CARTESIAN_POINT ( 'NONE',  ( 0.9251968503937015864, -0.5400638737290844871, 0.3530559997133364547 ) ) ;
#27955 = EDGE_LOOP ( 'NONE', ( #48820, #10817, #8979, #60911 ) ) ;
#27956 = CARTESIAN_POINT ( 'NONE',  ( -1.469816272965878357, -0.6046776061558809534, -0.2411417322834644161 ) ) ;
#27957 = CARTESIAN_POINT ( 'NONE',  ( 1.666666666666667185, -0.004921259842519576551, 0.3153832671262227771 ) ) ;
#27958 = DIRECTION ( 'NONE',  ( 0.5417801344272261677, 0.000000000000000000, 0.8405202471921882079 ) ) ;
#27959 = CARTESIAN_POINT ( 'NONE',  ( 1.594488188976378673, -0.4536011799217368745, -0.2665933059059886201 ) ) ;
#27960 = CARTESIAN_POINT ( 'NONE',  ( 0.3983403474834781299, 0.03178304480585100733, -1.929133858267716661 ) ) ;
#27961 = CARTESIAN_POINT ( 'NONE',  ( -1.154855643044618851, 0.1283753931104748280, 0.1820866141732283561 ) ) ;
#27962 = CARTESIAN_POINT ( 'NONE',  ( -1.417322834645668772, -0.1870078740157480879, -0.4822834645669291653 ) ) ;
#27963 = CARTESIAN_POINT ( 'NONE',  ( 0.1509186351706045259, -0.05778040916215560624, -0.4822834645669293319 ) ) ;
#27964 = AXIS2_PLACEMENT_3D ( 'NONE', #10922, #55929, #81645 ) ;
#27965 = VERTEX_POINT ( 'NONE', #56298 ) ;
#27967 = CARTESIAN_POINT ( 'NONE',  ( -0.03443470937339728616, 1.062992125984252079, -1.537015892239756099 ) ) ;
#27966 = CARTESIAN_POINT ( 'NONE',  ( 1.666666666666667185, 0.05413385826771666132, 0.4176697321401328100 ) ) ;
#27968 = CARTESIAN_POINT ( 'NONE',  ( -0.8661417322834640276, -0.1870078740157480601, -0.3641732283464567677 ) ) ;
#27969 = CARTESIAN_POINT ( 'NONE',  ( 0.9448818897637802916, -0.1870078740157480879, -0.4822834645669291653 ) ) ;
#27970 = CARTESIAN_POINT ( 'NONE',  ( 1.194225721784777594, -0.3690944881889765550, -0.3153832671262227771 ) ) ;
#27971 = CARTESIAN_POINT ( 'NONE',  ( -0.3917322834645669549, -7.196005306013483243E-17, -1.221765461121048224 ) ) ;
#27972 = CARTESIAN_POINT ( 'NONE',  ( -0.6955380577427815458, -0.3690944881889765550, -0.3153832671262227771 ) ) ;
#27973 = CARTESIAN_POINT ( 'NONE',  ( -1.450131233595799651, 0.1771653543307087075, -0.09757992244046823083 ) ) ;
#27974 = CARTESIAN_POINT ( 'NONE',  ( 0.4724409448818889246, 0.1265901696525005560, -0.7545931758530183275 ) ) ;
#27975 = CARTESIAN_POINT ( 'NONE',  ( 0.6758530183727039509, 0.2952755905511810774, -0.1292274648535930714 ) ) ;
#27976 = CARTESIAN_POINT ( 'NONE',  ( -1.030183727034119867, -0.2845877964562159024, 0.3641732283464567677 ) ) ;
#27977 = CARTESIAN_POINT ( 'NONE',  ( -0.3608923884514428360, -0.5511811023622048555, -0.09757992244046775898 ) ) ;
#27978 = CARTESIAN_POINT ( 'NONE',  ( -0.1443569553805768291, 0.05413385826771666132, 0.4176697321401328100 ) ) ;
#27979 = CARTESIAN_POINT ( 'NONE',  ( -1.496062992125983815, -0.1870078740157479769, 0.3641732283464567677 ) ) ;
#27980 = CARTESIAN_POINT ( 'NONE',  ( -0.2867679344610365444, -0.2867679344610367664, -0.05579359399706226158 ) ) ;
#27981 = CARTESIAN_POINT ( 'NONE',  ( 0.5577427821522314977, -0.3162353388693409650, -0.4822834645669289433 ) ) ;
#27982 = CARTESIAN_POINT ( 'NONE',  ( -0.4091458600556402980, -0.2362204724409451284, -0.2099737532808398921 ) ) ;
#27983 = CARTESIAN_POINT ( 'NONE',  ( 0.4091458600556404646, -0.2362204724409448231, -1.441601049868766582 ) ) ;
#27984 = CARTESIAN_POINT ( 'NONE',  ( -0.8070866141732276899, -0.5400638737290844871, 0.3530559997133364547 ) ) ;
#27985 = CARTESIAN_POINT ( 'NONE',  ( -0.3740157480314953431, -0.4536011799217368745, -0.2665933059059886201 ) ) ;
#27986 = CARTESIAN_POINT ( 'NONE',  ( -1.358267716535432434, -0.5400638737290844871, 0.3530559997133364547 ) ) ;
#27987 = CARTESIAN_POINT ( 'NONE',  ( 0.3740157480314966754, -0.4536011799217367080, 0.2665933059059888421 ) ) ;
#27988 = CARTESIAN_POINT ( 'NONE',  ( -0.5708661417322828946, 0.07958543189024071263, -0.2665933059059888421 ) ) ;
#27989 = CARTESIAN_POINT ( 'NONE',  ( -1.049868766404198794, 0.2306618581243847221, -0.2411417322834647770 ) ) ;
#27990 = CARTESIAN_POINT ( 'NONE',  ( -1.712598425196849572, 0.1660481256975885056, 0.3530559997133364547 ) ) ;
#27991 = CARTESIAN_POINT ( 'NONE',  ( 1.253280839895013710, -0.05778040916215560624, -0.4822834645669293319 ) ) ;
#27992 = FACE_OUTER_BOUND ( 'NONE', #40995, .T. ) ;
#27993 = CARTESIAN_POINT ( 'NONE',  ( 0.9973753280839902091, -0.5023911411419708095, 0.1820866141732285504 ) ) ;
#27994 = CARTESIAN_POINT ( 'NONE',  ( 0.2755905511811031494, 0.2952755905511811885, 0.000000000000000000 ) ) ;
#27995 = EDGE_CURVE ( 'NONE', #41294, #41264, #25092, .T. ) ;
#27996 = CARTESIAN_POINT ( 'NONE',  ( -1.364829396325458521, -0.6046776061558807314, 0.2411417322834647770 ) ) ;
#27997 = CARTESIAN_POINT ( 'NONE',  ( 1.450131233595801428, 0.1771653543307087630, 0.09757992244046791164 ) ) ;
#27998 = ORIENTED_EDGE ( 'NONE', *, *, #23876, .F. ) ;
#27999 = CARTESIAN_POINT ( 'NONE',  ( 0.1998031496062994128, -0.3460692066303957537, -2.845800524934383624 ) ) ;
#28000 = CARTESIAN_POINT ( 'NONE',  ( -1.338582677165353729, -0.1870078740157479769, 0.3641732283464567677 ) ) ;
#28001 = CARTESIAN_POINT ( 'NONE',  ( -0.3608923884514428360, 0.2952755905511811885, 0.1292274648535926551 ) ) ;
#28002 = CARTESIAN_POINT ( 'NONE',  ( 0.2427821522309716595, -0.3162353388693409650, -0.4822834645669289433 ) ) ;
#28003 = CARTESIAN_POINT ( 'NONE',  ( -1.673228346456691717, 0.07958543189024071263, -0.2665933059059888421 ) ) ;
#28004 = CARTESIAN_POINT ( 'NONE',  ( -0.3996062992125986590, 0.1070741851644051723, -1.841863517060367661 ) ) ;
#28005 = CARTESIAN_POINT ( 'NONE',  ( -1.233595800524933894, 0.2306618581243848609, 0.2411417322834645549 ) ) ;
#28006 = CARTESIAN_POINT ( 'NONE',  ( 0.5511811023622055217, -0.1870078740157479769, 0.4822834645669291653 ) ) ;
#28007 = CARTESIAN_POINT ( 'NONE',  ( -0.02624671916010428221, 0.2306618581243847221, -0.2411417322834647770 ) ) ;
#28008 = CARTESIAN_POINT ( 'NONE',  ( 1.259842519685040019, -0.1870078740157479769, 0.4822834645669291653 ) ) ;
#28009 = CARTESIAN_POINT ( 'NONE',  ( 0.2925321140481931814, 0.2925321140481931814, -1.159448818897637734 ) ) ;
#28010 = CARTESIAN_POINT ( 'NONE',  ( 0.1998031496062992740, 0.3460692066303959757, -1.404199475065616820 ) ) ;
#28011 = CARTESIAN_POINT ( 'NONE',  ( -0.1974969037888706647, 0.3420746716998658843, -1.115485564304461885 ) ) ;
#28012 = CARTESIAN_POINT ( 'NONE',  ( 0.2867679344610366554, -0.2867679344610365444, -0.2480314960629920740 ) ) ;
#28013 = CARTESIAN_POINT ( 'NONE',  ( 0.02624671916010564918, 0.1283753931104748280, 0.1820866141732283561 ) ) ;
#28014 = CARTESIAN_POINT ( 'NONE',  ( -0.1509186351706028884, -0.05778040916215522460, 0.4822834645669289988 ) ) ;
#28015 = CARTESIAN_POINT ( 'NONE',  ( 0.7611548556430451917, -0.6046776061558807314, 0.2411417322834647770 ) ) ;
#28016 = CARTESIAN_POINT ( 'NONE',  ( 0.3949938075777408852, 0.1058382717557500435, -1.618766404199474929 ) ) ;
#28017 = CARTESIAN_POINT ( 'NONE',  ( -0.2165354330708654795, 0.07958543189024085140, 0.2665933059059887866 ) ) ;
#28018 =( BOUNDED_SURFACE ( )  B_SPLINE_SURFACE ( 1, 2, ( 
 ( #37853, #18510, #48830, #44153, #63530, #24395, #5861, #31537, #57193, #74531, #61880, #42514, #68217, #13439, #70249, #32366, #82895, #26050, #51708, #58029, #39519, #71096, #65633, #50881, #76581, #33626, #392, #18909, #39095, #25627, #78256, #63940, #64777, #20165, #65207, #7115, #6696, #32786, #45815, #58880, #6277, #19745, #46239, #83305, #77410, #51290, #58455, #7544, #70671, #45399, #57614, #25215, #64359, #33216, #19323, #31953, #77835, #20587, #1238, #814, #26477, #71935, #71514, #52127, #52547, #26887, #14284, #76993, #39948, #13860, #7964, #44560, #44975, #12605, #38262, #13027, #38681, #10030, #9615, #73177, #66450, #21415, #15527, #47068, #35286, #47484, #72760, #2058, #60947, #78677, #22653, #16356, #54627, #66036, #15110, #41592, #67282, #27722, #46660, #42001, #27304, #80339, #8375, #48312, #34040, #34459, #74009, #40357, #8786, #3298, #28962, #2890, #28553, #22241, #72354, #79505, #79096, #9205, #73604, #59703, #67695, #21822, #47896, #54209, #53389, #40765, #60128, #15946, #41185, #66875, #2479, #59289, #28138, #53794, #34878, #79925, #60539, #1647, #14701, #52963, #20998, #10453, #81570, #75248, #68514, #10854, #38476, #57819, #74424, #74843, #17593, #80745, #62191, #23472, #25422, #55860, #16771, #31748, #32163, #51087, #186, #25839, #77203, #49139, #44765, #42820, #6493, #12401, #68922, #19116, #42408, #23059, #70462, #35695, #68106, #38058, #36515, #17188, #43224, #51498, #12819, #70892, #48727, #55038, #23888, #4528, #6074, #45189, #36108, #81156, #55447, #63735, #30198, #49554, #19532, #3714, #57410, #83103, #61779, #76784, #64160, #61361, #29377, #4120, #29785, #1854, #7760, #13242, #78469, #7329, #58241, #607, #2271, #27516, #59501, #71723, #51924, #66245, #38891, #6907, #59087, #26263, #8169, #77629, #20794, #64993, #27934, #53172, #72557, #78887, #46450, #21208, #1442, #8583, #40564, #46863, #13653, #14904, #72143, #52761, #14499, #71306, #34255, #59916, #40152, #19961, #47279, #53592, #27099, #20377, #58667, #65836, #1032, #79301, #33834, #26686, #39306, #21619, #32579, #64570, #45612, #32997, #52341, #78048, #46029, #14079, #39731, #65427, #33426, #40985, #68325, #22037, #66665, #9411, #54426, #74224, #67079, #29996, #48941, #42628, #9004, #61160, #34676, #3511, #41397, #80957, #55659, #79720, #80136, #81369, #10663, #54008, #23682, #15743, #9825, #47697, #23272, #61993, #10246, #15320, #61583, #36318, #22457, #74643, #29180, #73814, #73392, #2687, #16985, #35081, #54847, #60339, #48116, #72969, #16151, #41798, #67489, #29587, #80551, #28347, #60747, #3099, #28763, #35495, #22863, #48524, #16569, #4330, #42214, #67910, #35917, #55250, #3928, #56490, #82594, #69953, #25326, #30412, #69552, #12720, #49765, #82192, #75465, #24913, #57307, #37141, #24509, #24096, #49356, #30825, #31649, #69135, #56080, #44262, #44670, #5978, #50581, #31233, #38380, #62826, #37964, #11900, #81785, #12307, #70365, #63640, #64056, #6396, #32066, #5161, #83005, #50176, #19022, #76288, #18619, #50990, #17804, #36724, #76688, #75053, #4739, #57727, #75871, #18214, #5568, #90, #17400, #43030, #11066, #68725, #37554, #43849, #62400, #43438, #11487, #63228, #56900, #58999, #58574, #26597, #21119, #77108, #52668, #45517, #13147, #71213, #1355, #71631, #939, #64474, #26167, #14409, #20283, #25743, #7667, #19868, #70795, #38798, #14819, #40063, #72052, #52249, #6811, #78795, #51406, #19440, #13983, #32482, #20706, #58145, #33338, #77533, #40478, #65750, #1764, #8083, #27006, #46779, #514, #77954, #66156, #51828, #32907, #33746, #59407, #78375, #46358, #27421, #13556, #45932, #39212, #53082, #72470, #64897, #8495, #39639, #34162, #59823, #7234, #65330, #45091, #48433, #41709, #48023, #28255, #61488, #66991, #54335, #3007, #29085, #9323, #80461, #40889, #53916, #16062, #60249, #73723, #67401, #34993, #60658, #3836, #23178, #66571, #41305, #9736, #47189, #28674, #80045, #73300, #74132, #22364, #8905, #22770, #80866, #16477, #48848, #74549, #42533, #15649, #10156, #35407, #55155, #61071, #3422, #67819, #34581, #72881, #35822, #2178, #2597, #54755 ),
 ( #79629, #42124, #21947, #29496, #16894, #68235, #27845, #10570, #36227, #53506, #79214, #21530, #15230, #47606, #74962, #63545, #81693, #75776, #49260, #11389, #61896, #5066, #30735, #37046, #18525, #50080, #44575, #29901, #55565, #12622, #62728, #81273, #18117, #4643, #57209, #42936, #43750, #82501, #44168, #69456, #69039, #11806, #24817, #37870, #68630, #82096, #25231, #62306, #56398, #30314, #37461, #69861, #49672, #24410, #36629, #4237, #43338, #12212, #24004, #10970, #56802, #82910, #5879, #63134, #5473, #50896, #50484, #31135, #31552, #76596, #18926, #55982, #70267, #76188, #23589, #17308, #75362, #17710, #65652, #39537, #77009, #72371, #71952, #52146, #45416, #410, #77852, #26067, #14305, #1257, #39965, #52564, #45831, #59307, #13044, #13455, #27320, #19342, #71112, #46257, #20604, #65225, #7563, #26905, #51307, #58472, #58045, #71530, #78273, #44992, #7981, #836, #33645, #33235, #70691, #64375, #51726, #1664, #20181, #26494, #6712, #52981, #19763, #7131, #39111, #58897, #64793, #78694, #38697, #32381, #13877, #77428, #21017, #46678, #32805, #38281, #63957, #6294, #31969, #57630, #36925, #25644, #41204, #2496, #3316, #34895, #79114, #9633, #10049, #28980, #61382, #3731, #55054, #28156, #22670, #21839, #67712, #73621, #47916, #80357, #21432, #2076, #48329, #14720, #53406, #15963, #73195, #53811, #54227, #29395, #74026, #48744, #59721, #34057, #2907, #79524, #67299, #23076, #72777, #60145, #34479, #41610, #47502, #15545, #35712, #66055, #35303, #66892, #27741, #9222, #60965, #60557, #28571, #47087, #15127, #54647, #79944, #40373, #22258, #8803, #40782, #66468, #80762, #16372, #42019, #8392, #29802, #44073, #74442, #68126, #36948, #61797, #69356, #55463, #56300, #42837, #5779, #62625, #10471, #4968, #68530, #82403, #57112, #81172, #81589, #82806, #69765, #23490, #31448, #17204, #11288, #49156, #24721, #63443, #11710, #16789, #63037, #12110, #23906, #50390, #30635, #75267, #74862, #4137, #76087, #10871, #81997, #36531, #49571, #42426, #17610, #43241, #68939, #31036, #24311, #25130, #36124, #62207, #4544, #49981, #30215, #75679, #55877, #37768, #18019, #43654, #37365, #56704, #5375, #18431, #729, #71429, #26805, #31870, #71011, #14201, #51208, #307, #13355, #44885, #76501, #33544, #70585, #26387, #65119, #57530, #33126, #39008, #13776, #77750, #83221, #76905, #12939, #39433, #7031, #64692, #19235, #52463, #32281, #19654, #51620, #20083, #57941, #45733, #6192, #38597, #32700, #25542, #58366, #52045, #25962, #77325, #78171, #71851, #64275, #6610, #7456, #12519, #45316, #58796, #1154, #20502, #46156, #39858, #65549, #7880, #59206, #1567, #50800, #18829, #44475, #70166, #38180, #63855, #60458, #9535, #8291, #14618, #60868, #27221, #65955, #28468, #2398, #66369, #66793, #9128, #60042, #28055, #28885, #48238, #33959, #8706, #34799, #72270, #53713, #15027, #15870, #47405, #59621, #22160, #22577, #41518, #73934, #16277, #67616, #40683, #35206, #34377, #80261, #2809, #54129, #3221, #1975, #40272, #54546, #52882, #27639, #79844, #79420, #21740, #47820, #41922, #9946, #61282, #53301, #46572, #15445, #73094, #73521, #35618, #79013, #72679, #46985, #67203, #41105, #78593, #20918, #21333, #30539, #23395, #74346, #49062, #36854, #49480, #62113, #42330, #4045, #75587, #81491, #3634, #68847, #81079, #48650, #16691, #75993, #17926, #49886, #4456, #68029, #56609, #29302, #80671, #75173, #10374, #81904, #36031, #11195, #55373, #18335, #43562, #62945, #69263, #62527, #24629, #61705, #30121, #43975, #29710, #10780, #11610, #37269, #56203, #17518, #74761, #54964, #69672, #17110, #4865, #5280, #42745, #30942, #43150, #82309, #24215, #68440, #36440, #55783, #50295, #12015, #37670, #23807, #22984, #44788, #32186, #64182, #6929, #70484, #58263, #18735, #6097, #77225, #38082, #25862, #12841, #6516, #58686, #31351, #32600, #83125, #50705, #25444, #13263, #51522, #38500, #44377, #63756, #51944, #57841, #63347, #45213, #57432, #25032, #76403, #52361, #77649, #26283, #209, #70069, #33016, #5682, #57017, #19554, #12424, #627, #31771, #70914, #51110, #78067, #19982, #39327, #45632 ) ),
 .UNSPECIFIED., .F., .F., .F. ) 
 B_SPLINE_SURFACE_WITH_KNOTS ( ( 2, 2 ),
 ( 3, 2, 2, 2, 2, 2, 2, 2, 2, 2, 2, 2, 2, 2, 2, 2, 2, 2, 2, 2, 2, 2, 2, 2, 2, 2, 2, 2, 2, 2, 2, 2, 2, 2, 2, 2, 2, 2, 2, 2, 2, 2, 2, 2, 2, 2, 2, 2, 2, 2, 2, 2, 2, 2, 2, 2, 2, 2, 2, 2, 2, 2, 2, 2, 2, 2, 2, 2, 2, 2, 2, 2, 2, 2, 2, 2, 2, 2, 2, 2, 2, 2, 2, 2, 2, 2, 2, 2, 2, 2, 2, 2, 2, 2, 2, 2, 2, 2, 2, 2, 2, 2, 2, 2, 2, 2, 2, 2, 2, 2, 2, 2, 2, 2, 2, 2, 2, 2, 2, 2, 2, 2, 2, 2, 2, 2, 2, 2, 2, 2, 2, 2, 2, 2, 2, 2, 2, 2, 2, 2, 2, 2, 2, 2, 2, 2, 2, 2, 2, 2, 2, 2, 2, 2, 2, 2, 2, 2, 2, 2, 2, 2, 2, 2, 2, 2, 2, 2, 2, 2, 2, 2, 2, 2, 2, 2, 2, 2, 2, 2, 2, 2, 2, 2, 2, 2, 2, 2, 2, 2, 2, 2, 2, 2, 2, 2, 2, 2, 2, 2, 2, 2, 2, 2, 2, 2, 2, 2, 2, 2, 2, 2, 2, 2, 2, 2, 2, 2, 2, 2, 2, 2, 2, 2, 2, 2, 2, 2, 2, 2, 2, 2, 2, 2, 2, 2, 2, 2, 2, 2, 2, 2, 2, 2, 2, 2, 2, 2, 2, 2, 2, 2, 2, 2, 2, 3 ),
 ( 0.000000000000000000, 1.000000000000000000 ),
 ( 0.000000000000000000, 0.003787878787878787984, 0.007575757575757575968, 0.01136363636363636395, 0.01515151515151515194, 0.01893939393939393992, 0.02272727272727272790, 0.02651515151515151589, 0.03030303030303030387, 0.03409090909090908839, 0.03787878787878787984, 0.04166666666666666435, 0.04545454545454545581, 0.04924242424242424032, 0.05303030303030303177, 0.05681818181818181629, 0.06060606060606060774, 0.06439393939393939226, 0.06818181818181817677, 0.07196969696969697516, 0.07575757575757575968, 0.07954545454545454419, 0.08333333333333332871, 0.08712121212121212710, 0.09090909090909091161, 0.09469696969696969613, 0.09848484848484848064, 0.1022727272727272790, 0.1060606060606060635, 0.1098484848484848481, 0.1136363636363636326, 0.1174242424242424310, 0.1212121212121212155, 0.1250000000000000000, 0.1287878787878787845, 0.1325757575757575690, 0.1363636363636363535, 0.1401515151515151381, 0.1439393939393939503, 0.1477272727272727348, 0.1515151515151515194, 0.1553030303030303039, 0.1590909090909090884, 0.1628787878787878729, 0.1666666666666666574, 0.1704545454545454419, 0.1742424242424242542, 0.1780303030303030387, 0.1818181818181818232, 0.1856060606060606077, 0.1893939393939393923, 0.1931818181818181768, 0.1969696969696969613, 0.2007575757575757458, 0.2045454545454545581, 0.2083333333333333426, 0.2121212121212121271, 0.2159090909090909116, 0.2196969696969696961, 0.2234848484848484806, 0.2272727272727272652, 0.2310606060606060497, 0.2348484848484848619, 0.2386363636363636465, 0.2424242424242424310, 0.2462121212121212155, 0.2500000000000000000, 0.2537878787878787845, 0.2575757575757575690, 0.2613636363636363535, 0.2651515151515151381, 0.2689393939393939226, 0.2727272727272727071, 0.2765151515151514916, 0.2803030303030302761, 0.2840909090909091161, 0.2878787878787879007, 0.2916666666666666852, 0.2954545454545454697, 0.2992424242424242542, 0.3030303030303030387, 0.3068181818181818232, 0.3106060606060606077, 0.3143939393939393923, 0.3181818181818181768, 0.3219696969696969613, 0.3257575757575757458, 0.3295454545454545303, 0.3333333333333333148, 0.3371212121212120993, 0.3409090909090908839, 0.3446969696969697239, 0.3484848484848485084, 0.3522727272727272929, 0.3560606060606060774, 0.3598484848484848619, 0.3636363636363636465, 0.3674242424242424310, 0.3712121212121212155, 0.3750000000000000000, 0.3787878787878787845, 0.3825757575757575690, 0.3863636363636363535, 0.3901515151515151381, 0.3939393939393939226, 0.3977272727272727071, 0.4015151515151514916, 0.4053030303030302761, 0.4090909090909091161, 0.4128787878787879007, 0.4166666666666666852, 0.4204545454545454697, 0.4242424242424242542, 0.4280303030303030387, 0.4318181818181818232, 0.4356060606060606077, 0.4393939393939393923, 0.4431818181818181768, 0.4469696969696969613, 0.4507575757575757458, 0.4545454545454545303, 0.4583333333333333148, 0.4621212121212120993, 0.4659090909090908839, 0.4696969696969697239, 0.4734848484848485084, 0.4772727272727272929, 0.4810606060606060774, 0.4848484848484848619, 0.4886363636363636465, 0.4924242424242424310, 0.4962121212121212155, 0.5000000000000000000, 0.5037878787878787845, 0.5075757575757575690, 0.5113636363636363535, 0.5151515151515151381, 0.5189393939393939226, 0.5227272727272727071, 0.5265151515151514916, 0.5303030303030302761, 0.5340909090909090606, 0.5378787878787878451, 0.5416666666666666297, 0.5454545454545454142, 0.5492424242424241987, 0.5530303030303029832, 0.5568181818181817677, 0.5606060606060605522, 0.5643939393939394478, 0.5681818181818182323, 0.5719696969696970168, 0.5757575757575758013, 0.5795454545454545858, 0.5833333333333333703, 0.5871212121212121549, 0.5909090909090909394, 0.5946969696969697239, 0.5984848484848485084, 0.6022727272727272929, 0.6060606060606060774, 0.6098484848484848619, 0.6136363636363636465, 0.6174242424242424310, 0.6212121212121212155, 0.6250000000000000000, 0.6287878787878787845, 0.6325757575757575690, 0.6363636363636363535, 0.6401515151515151381, 0.6439393939393939226, 0.6477272727272727071, 0.6515151515151514916, 0.6553030303030302761, 0.6590909090909090606, 0.6628787878787878451, 0.6666666666666666297, 0.6704545454545454142, 0.6742424242424241987, 0.6780303030303029832, 0.6818181818181817677, 0.6856060606060605522, 0.6893939393939394478, 0.6931818181818182323, 0.6969696969696970168, 0.7007575757575758013, 0.7045454545454545858, 0.7083333333333333703, 0.7121212121212121549, 0.7159090909090909394, 0.7196969696969697239, 0.7234848484848485084, 0.7272727272727272929, 0.7310606060606060774, 0.7348484848484848619, 0.7386363636363636465, 0.7424242424242424310, 0.7462121212121212155, 0.7500000000000000000, 0.7537878787878787845, 0.7575757575757575690, 0.7613636363636363535, 0.7651515151515151381, 0.7689393939393939226, 0.7727272727272727071, 0.7765151515151514916, 0.7803030303030302761, 0.7840909090909090606, 0.7878787878787878451, 0.7916666666666666297, 0.7954545454545454142, 0.7992424242424241987, 0.8030303030303029832, 0.8068181818181817677, 0.8106060606060605522, 0.8143939393939394478, 0.8181818181818182323, 0.8219696969696970168, 0.8257575757575758013, 0.8295454545454545858, 0.8333333333333333703, 0.8371212121212121549, 0.8409090909090909394, 0.8446969696969697239, 0.8484848484848485084, 0.8522727272727272929, 0.8560606060606060774, 0.8598484848484848619, 0.8636363636363636465, 0.8674242424242424310, 0.8712121212121212155, 0.8750000000000000000, 0.8787878787878787845, 0.8825757575757575690, 0.8863636363636363535, 0.8901515151515151381, 0.8939393939393939226, 0.8977272727272727071, 0.9015151515151514916, 0.9053030303030302761, 0.9090909090909090606, 0.9128787878787878451, 0.9166666666666666297, 0.9204545454545454142, 0.9242424242424241987, 0.9280303030303029832, 0.9318181818181817677, 0.9356060606060605522, 0.9393939393939394478, 0.9431818181818182323, 0.9469696969696970168, 0.9507575757575758013, 0.9545454545454545858, 0.9583333333333333703, 0.9621212121212121549, 0.9659090909090909394 ),
 .UNSPECIFIED. ) 
 GEOMETRIC_REPRESENTATION_ITEM ( )  RATIONAL_B_SPLINE_SURFACE ( (
 ( 1.000000000000000000, 0.9659258262890683122, 1.000000000000000000, 0.9659258262890683122, 1.000000000000000000, 0.9659258262890683122, 1.000000000000000000, 0.9659258262890683122, 1.000000000000000000, 0.9659258262890683122, 1.000000000000000000, 0.9659258262890683122, 1.000000000000000000, 0.9659258262890683122, 1.000000000000000000, 0.9659258262890683122, 1.000000000000000000, 0.9659258262890683122, 1.000000000000000000, 0.9659258262890683122, 1.000000000000000000, 0.9659258262890683122, 1.000000000000000000, 0.9659258262890683122, 1.000000000000000000, 0.9659258262890683122, 1.000000000000000000, 0.9659258262890683122, 1.000000000000000000, 0.9659258262890683122, 1.000000000000000000, 0.9659258262890683122, 1.000000000000000000, 0.9659258262890683122, 1.000000000000000000, 0.9659258262890683122, 1.000000000000000000, 0.9659258262890683122, 1.000000000000000000, 0.9659258262890683122, 1.000000000000000000, 0.9659258262890683122, 1.000000000000000000, 0.9659258262890683122, 1.000000000000000000, 0.9659258262890683122, 1.000000000000000000, 0.9659258262890683122, 1.000000000000000000, 0.9659258262890683122, 1.000000000000000000, 0.9659258262890683122, 1.000000000000000000, 0.9659258262890683122, 1.000000000000000000, 0.9659258262890683122, 1.000000000000000000, 0.9659258262890683122, 1.000000000000000000, 0.9659258262890683122, 1.000000000000000000, 0.9659258262890683122, 1.000000000000000000, 0.9659258262890683122, 1.000000000000000000, 0.9659258262890683122, 1.000000000000000000, 0.9659258262890683122, 1.000000000000000000, 0.9659258262890683122, 1.000000000000000000, 0.9659258262890683122, 1.000000000000000000, 0.9659258262890683122, 1.000000000000000000, 0.9659258262890683122, 1.000000000000000000, 0.9659258262890683122, 1.000000000000000000, 0.9659258262890683122, 1.000000000000000000, 0.9659258262890683122, 1.000000000000000000, 0.9659258262890683122, 1.000000000000000000, 0.9659258262890683122, 1.000000000000000000, 0.9659258262890683122, 1.000000000000000000, 0.9659258262890683122, 1.000000000000000000, 0.9659258262890683122, 1.000000000000000000, 0.9659258262890683122, 1.000000000000000000, 0.9659258262890683122, 1.000000000000000000, 0.9659258262890683122, 1.000000000000000000, 0.9659258262890683122, 1.000000000000000000, 0.9659258262890683122, 1.000000000000000000, 0.9659258262890683122, 1.000000000000000000, 0.9659258262890683122, 1.000000000000000000, 0.9659258262890683122, 1.000000000000000000, 0.9659258262890683122, 1.000000000000000000, 0.9659258262890683122, 1.000000000000000000, 0.9659258262890683122, 1.000000000000000000, 0.9659258262890683122, 1.000000000000000000, 0.9659258262890683122, 1.000000000000000000, 0.9659258262890683122, 1.000000000000000000, 0.9659258262890683122, 1.000000000000000000, 0.9659258262890683122, 1.000000000000000000, 0.9659258262890683122, 1.000000000000000000, 0.9659258262890683122, 1.000000000000000000, 0.9659258262890683122, 1.000000000000000000, 0.9659258262890683122, 1.000000000000000000, 0.9659258262890683122, 1.000000000000000000, 0.9659258262890683122, 1.000000000000000000, 0.9659258262890683122, 1.000000000000000000, 0.9659258262890683122, 1.000000000000000000, 0.9659258262890683122, 1.000000000000000000, 0.9659258262890683122, 1.000000000000000000, 0.9659258262890683122, 1.000000000000000000, 0.9659258262890683122, 1.000000000000000000, 0.9659258262890683122, 1.000000000000000000, 0.9659258262890683122, 1.000000000000000000, 0.9659258262890683122, 1.000000000000000000, 0.9659258262890683122, 1.000000000000000000, 0.9659258262890683122, 1.000000000000000000, 0.9659258262890683122, 1.000000000000000000, 0.9659258262890683122, 1.000000000000000000, 0.9659258262890683122, 1.000000000000000000, 0.9659258262890683122, 1.000000000000000000, 0.9659258262890683122, 1.000000000000000000, 0.9659258262890683122, 1.000000000000000000, 0.9659258262890683122, 1.000000000000000000, 0.9659258262890683122, 1.000000000000000000, 0.9659258262890683122, 1.000000000000000000, 0.9659258262890683122, 1.000000000000000000, 0.9659258262890683122, 1.000000000000000000, 0.9659258262890683122, 1.000000000000000000, 0.9659258262890683122, 1.000000000000000000, 0.9659258262890683122, 1.000000000000000000, 0.9659258262890683122, 1.000000000000000000, 0.9659258262890683122, 1.000000000000000000, 0.9659258262890683122, 1.000000000000000000, 0.9659258262890683122, 1.000000000000000000, 0.9659258262890683122, 1.000000000000000000, 0.9659258262890683122, 1.000000000000000000, 0.9659258262890683122, 1.000000000000000000, 0.9659258262890683122, 1.000000000000000000, 0.9659258262890683122, 1.000000000000000000, 0.9659258262890683122, 1.000000000000000000, 0.9659258262890683122, 1.000000000000000000, 0.9659258262890683122, 1.000000000000000000, 0.9659258262890683122, 1.000000000000000000, 0.9659258262890683122, 1.000000000000000000, 0.9659258262890683122, 1.000000000000000000, 0.9659258262890683122, 1.000000000000000000, 0.9659258262890683122, 1.000000000000000000, 0.9659258262890683122, 1.000000000000000000, 0.9659258262890683122, 1.000000000000000000, 0.9659258262890683122, 1.000000000000000000, 0.9659258262890683122, 1.000000000000000000, 0.9659258262890683122, 1.000000000000000000, 0.9659258262890683122, 1.000000000000000000, 0.9659258262890683122, 1.000000000000000000, 0.9659258262890683122, 1.000000000000000000, 0.9659258262890683122, 1.000000000000000000, 0.9659258262890683122, 1.000000000000000000, 0.9659258262890683122, 1.000000000000000000, 0.9659258262890683122, 1.000000000000000000, 0.9659258262890683122, 1.000000000000000000, 0.9659258262890683122, 1.000000000000000000, 0.9659258262890683122, 1.000000000000000000, 0.9659258262890683122, 1.000000000000000000, 0.9659258262890683122, 1.000000000000000000, 0.9659258262890683122, 1.000000000000000000, 0.9659258262890683122, 1.000000000000000000, 0.9659258262890683122, 1.000000000000000000, 0.9659258262890683122, 1.000000000000000000, 0.9659258262890683122, 1.000000000000000000, 0.9659258262890683122, 1.000000000000000000, 0.9659258262890683122, 1.000000000000000000, 0.9659258262890683122, 1.000000000000000000, 0.9659258262890683122, 1.000000000000000000, 0.9659258262890683122, 1.000000000000000000, 0.9659258262890683122, 1.000000000000000000, 0.9659258262890683122, 1.000000000000000000, 0.9659258262890683122, 1.000000000000000000, 0.9659258262890683122, 1.000000000000000000, 0.9659258262890683122, 1.000000000000000000, 0.9659258262890683122, 1.000000000000000000, 0.9659258262890683122, 1.000000000000000000, 0.9659258262890683122, 1.000000000000000000, 0.9659258262890683122, 1.000000000000000000, 0.9659258262890683122, 1.000000000000000000, 0.9659258262890683122, 1.000000000000000000, 0.9659258262890683122, 1.000000000000000000, 0.9659258262890683122, 1.000000000000000000, 0.9659258262890683122, 1.000000000000000000, 0.9659258262890683122, 1.000000000000000000, 0.9659258262890683122, 1.000000000000000000, 0.9659258262890683122, 1.000000000000000000, 0.9659258262890683122, 1.000000000000000000, 0.9659258262890683122, 1.000000000000000000, 0.9659258262890683122, 1.000000000000000000, 0.9659258262890683122, 1.000000000000000000, 0.9659258262890683122, 1.000000000000000000, 0.9659258262890683122, 1.000000000000000000, 0.9659258262890683122, 1.000000000000000000, 0.9659258262890683122, 1.000000000000000000, 0.9659258262890683122, 1.000000000000000000, 0.9659258262890683122, 1.000000000000000000, 0.9659258262890683122, 1.000000000000000000, 0.9659258262890683122, 1.000000000000000000, 0.9659258262890683122, 1.000000000000000000, 0.9659258262890683122, 1.000000000000000000, 0.9659258262890683122, 1.000000000000000000, 0.9659258262890683122, 1.000000000000000000, 0.9659258262890683122, 1.000000000000000000, 0.9659258262890683122, 1.000000000000000000, 0.9659258262890683122, 1.000000000000000000, 0.9659258262890683122, 1.000000000000000000, 0.9659258262890683122, 1.000000000000000000, 0.9659258262890683122, 1.000000000000000000, 0.9659258262890683122, 1.000000000000000000, 0.9659258262890683122, 1.000000000000000000, 0.9659258262890683122, 1.000000000000000000, 0.9659258262890683122, 1.000000000000000000, 0.9659258262890683122, 1.000000000000000000, 0.9659258262890683122, 1.000000000000000000, 0.9659258262890683122, 1.000000000000000000, 0.9659258262890683122, 1.000000000000000000, 0.9659258262890683122, 1.000000000000000000, 0.9659258262890683122, 1.000000000000000000, 0.9659258262890683122, 1.000000000000000000, 0.9659258262890683122, 1.000000000000000000, 0.9659258262890683122, 1.000000000000000000, 0.9659258262890683122, 1.000000000000000000, 0.9659258262890683122, 1.000000000000000000, 0.9659258262890683122, 1.000000000000000000, 0.9659258262890683122, 1.000000000000000000, 0.9659258262890683122, 1.000000000000000000, 0.9659258262890683122, 1.000000000000000000, 0.9659258262890683122, 1.000000000000000000, 0.9659258262890683122, 1.000000000000000000, 0.9659258262890683122, 1.000000000000000000, 0.9659258262890683122, 1.000000000000000000, 0.9659258262890683122, 1.000000000000000000, 0.9659258262890683122, 1.000000000000000000, 0.9659258262890683122, 1.000000000000000000, 0.9659258262890683122, 1.000000000000000000, 0.9659258262890683122, 1.000000000000000000, 0.9659258262890683122, 1.000000000000000000, 0.9659258262890683122, 1.000000000000000000, 0.9659258262890683122, 1.000000000000000000, 0.9659258262890683122, 1.000000000000000000, 0.9659258262890683122, 1.000000000000000000, 0.9659258262890683122, 1.000000000000000000, 0.9659258262890683122, 1.000000000000000000, 0.9659258262890683122, 1.000000000000000000, 0.9659258262890683122, 1.000000000000000000, 0.9659258262890683122, 1.000000000000000000, 0.9659258262890683122, 1.000000000000000000, 0.9659258262890683122, 1.000000000000000000, 0.9659258262890683122, 1.000000000000000000, 0.9659258262890683122, 1.000000000000000000, 0.9659258262890683122, 1.000000000000000000, 0.9659258262890683122, 1.000000000000000000, 0.9659258262890683122, 1.000000000000000000, 0.9659258262890683122, 1.000000000000000000, 0.9659258262890683122, 1.000000000000000000, 0.9659258262890683122, 1.000000000000000000, 0.9659258262890683122, 1.000000000000000000, 0.9659258262890683122, 1.000000000000000000, 0.9659258262890683122, 1.000000000000000000, 0.9659258262890683122, 1.000000000000000000, 0.9659258262890683122, 1.000000000000000000, 0.9659258262890683122, 1.000000000000000000, 0.9659258262890683122, 1.000000000000000000, 0.9659258262890683122, 1.000000000000000000, 0.9659258262890683122, 1.000000000000000000, 0.9659258262890683122, 1.000000000000000000, 0.9659258262890683122, 1.000000000000000000, 0.9659258262890683122, 1.000000000000000000, 0.9659258262890683122, 1.000000000000000000, 0.9659258262890683122, 1.000000000000000000, 0.9659258262890683122, 1.000000000000000000, 0.9659258262890683122, 1.000000000000000000, 0.9659258262890683122, 1.000000000000000000, 0.9659258262890683122, 1.000000000000000000, 0.9659258262890683122, 1.000000000000000000, 0.9659258262890683122, 1.000000000000000000, 0.9659258262890683122, 1.000000000000000000, 0.9659258262890683122, 1.000000000000000000, 0.9659258262890683122, 1.000000000000000000, 0.9659258262890683122, 1.000000000000000000, 0.9659258262890683122, 1.000000000000000000, 0.9659258262890683122, 1.000000000000000000, 0.9659258262890683122, 1.000000000000000000, 0.9659258262890683122, 1.000000000000000000, 0.9659258262890683122, 1.000000000000000000, 0.9659258262890683122, 1.000000000000000000, 0.9659258262890683122, 1.000000000000000000),
 ( 1.000000000000000000, 0.9659258262890683122, 1.000000000000000000, 0.9659258262890683122, 1.000000000000000000, 0.9659258262890683122, 1.000000000000000000, 0.9659258262890683122, 1.000000000000000000, 0.9659258262890683122, 1.000000000000000000, 0.9659258262890683122, 1.000000000000000000, 0.9659258262890683122, 1.000000000000000000, 0.9659258262890683122, 1.000000000000000000, 0.9659258262890683122, 1.000000000000000000, 0.9659258262890683122, 1.000000000000000000, 0.9659258262890683122, 1.000000000000000000, 0.9659258262890683122, 1.000000000000000000, 0.9659258262890683122, 1.000000000000000000, 0.9659258262890683122, 1.000000000000000000, 0.9659258262890683122, 1.000000000000000000, 0.9659258262890683122, 1.000000000000000000, 0.9659258262890683122, 1.000000000000000000, 0.9659258262890683122, 1.000000000000000000, 0.9659258262890683122, 1.000000000000000000, 0.9659258262890683122, 1.000000000000000000, 0.9659258262890683122, 1.000000000000000000, 0.9659258262890683122, 1.000000000000000000, 0.9659258262890683122, 1.000000000000000000, 0.9659258262890683122, 1.000000000000000000, 0.9659258262890683122, 1.000000000000000000, 0.9659258262890683122, 1.000000000000000000, 0.9659258262890683122, 1.000000000000000000, 0.9659258262890683122, 1.000000000000000000, 0.9659258262890683122, 1.000000000000000000, 0.9659258262890683122, 1.000000000000000000, 0.9659258262890683122, 1.000000000000000000, 0.9659258262890683122, 1.000000000000000000, 0.9659258262890683122, 1.000000000000000000, 0.9659258262890683122, 1.000000000000000000, 0.9659258262890683122, 1.000000000000000000, 0.9659258262890683122, 1.000000000000000000, 0.9659258262890683122, 1.000000000000000000, 0.9659258262890683122, 1.000000000000000000, 0.9659258262890683122, 1.000000000000000000, 0.9659258262890683122, 1.000000000000000000, 0.9659258262890683122, 1.000000000000000000, 0.9659258262890683122, 1.000000000000000000, 0.9659258262890683122, 1.000000000000000000, 0.9659258262890683122, 1.000000000000000000, 0.9659258262890683122, 1.000000000000000000, 0.9659258262890683122, 1.000000000000000000, 0.9659258262890683122, 1.000000000000000000, 0.9659258262890683122, 1.000000000000000000, 0.9659258262890683122, 1.000000000000000000, 0.9659258262890683122, 1.000000000000000000, 0.9659258262890683122, 1.000000000000000000, 0.9659258262890683122, 1.000000000000000000, 0.9659258262890683122, 1.000000000000000000, 0.9659258262890683122, 1.000000000000000000, 0.9659258262890683122, 1.000000000000000000, 0.9659258262890683122, 1.000000000000000000, 0.9659258262890683122, 1.000000000000000000, 0.9659258262890683122, 1.000000000000000000, 0.9659258262890683122, 1.000000000000000000, 0.9659258262890683122, 1.000000000000000000, 0.9659258262890683122, 1.000000000000000000, 0.9659258262890683122, 1.000000000000000000, 0.9659258262890683122, 1.000000000000000000, 0.9659258262890683122, 1.000000000000000000, 0.9659258262890683122, 1.000000000000000000, 0.9659258262890683122, 1.000000000000000000, 0.9659258262890683122, 1.000000000000000000, 0.9659258262890683122, 1.000000000000000000, 0.9659258262890683122, 1.000000000000000000, 0.9659258262890683122, 1.000000000000000000, 0.9659258262890683122, 1.000000000000000000, 0.9659258262890683122, 1.000000000000000000, 0.9659258262890683122, 1.000000000000000000, 0.9659258262890683122, 1.000000000000000000, 0.9659258262890683122, 1.000000000000000000, 0.9659258262890683122, 1.000000000000000000, 0.9659258262890683122, 1.000000000000000000, 0.9659258262890683122, 1.000000000000000000, 0.9659258262890683122, 1.000000000000000000, 0.9659258262890683122, 1.000000000000000000, 0.9659258262890683122, 1.000000000000000000, 0.9659258262890683122, 1.000000000000000000, 0.9659258262890683122, 1.000000000000000000, 0.9659258262890683122, 1.000000000000000000, 0.9659258262890683122, 1.000000000000000000, 0.9659258262890683122, 1.000000000000000000, 0.9659258262890683122, 1.000000000000000000, 0.9659258262890683122, 1.000000000000000000, 0.9659258262890683122, 1.000000000000000000, 0.9659258262890683122, 1.000000000000000000, 0.9659258262890683122, 1.000000000000000000, 0.9659258262890683122, 1.000000000000000000, 0.9659258262890683122, 1.000000000000000000, 0.9659258262890683122, 1.000000000000000000, 0.9659258262890683122, 1.000000000000000000, 0.9659258262890683122, 1.000000000000000000, 0.9659258262890683122, 1.000000000000000000, 0.9659258262890683122, 1.000000000000000000, 0.9659258262890683122, 1.000000000000000000, 0.9659258262890683122, 1.000000000000000000, 0.9659258262890683122, 1.000000000000000000, 0.9659258262890683122, 1.000000000000000000, 0.9659258262890683122, 1.000000000000000000, 0.9659258262890683122, 1.000000000000000000, 0.9659258262890683122, 1.000000000000000000, 0.9659258262890683122, 1.000000000000000000, 0.9659258262890683122, 1.000000000000000000, 0.9659258262890683122, 1.000000000000000000, 0.9659258262890683122, 1.000000000000000000, 0.9659258262890683122, 1.000000000000000000, 0.9659258262890683122, 1.000000000000000000, 0.9659258262890683122, 1.000000000000000000, 0.9659258262890683122, 1.000000000000000000, 0.9659258262890683122, 1.000000000000000000, 0.9659258262890683122, 1.000000000000000000, 0.9659258262890683122, 1.000000000000000000, 0.9659258262890683122, 1.000000000000000000, 0.9659258262890683122, 1.000000000000000000, 0.9659258262890683122, 1.000000000000000000, 0.9659258262890683122, 1.000000000000000000, 0.9659258262890683122, 1.000000000000000000, 0.9659258262890683122, 1.000000000000000000, 0.9659258262890683122, 1.000000000000000000, 0.9659258262890683122, 1.000000000000000000, 0.9659258262890683122, 1.000000000000000000, 0.9659258262890683122, 1.000000000000000000, 0.9659258262890683122, 1.000000000000000000, 0.9659258262890683122, 1.000000000000000000, 0.9659258262890683122, 1.000000000000000000, 0.9659258262890683122, 1.000000000000000000, 0.9659258262890683122, 1.000000000000000000, 0.9659258262890683122, 1.000000000000000000, 0.9659258262890683122, 1.000000000000000000, 0.9659258262890683122, 1.000000000000000000, 0.9659258262890683122, 1.000000000000000000, 0.9659258262890683122, 1.000000000000000000, 0.9659258262890683122, 1.000000000000000000, 0.9659258262890683122, 1.000000000000000000, 0.9659258262890683122, 1.000000000000000000, 0.9659258262890683122, 1.000000000000000000, 0.9659258262890683122, 1.000000000000000000, 0.9659258262890683122, 1.000000000000000000, 0.9659258262890683122, 1.000000000000000000, 0.9659258262890683122, 1.000000000000000000, 0.9659258262890683122, 1.000000000000000000, 0.9659258262890683122, 1.000000000000000000, 0.9659258262890683122, 1.000000000000000000, 0.9659258262890683122, 1.000000000000000000, 0.9659258262890683122, 1.000000000000000000, 0.9659258262890683122, 1.000000000000000000, 0.9659258262890683122, 1.000000000000000000, 0.9659258262890683122, 1.000000000000000000, 0.9659258262890683122, 1.000000000000000000, 0.9659258262890683122, 1.000000000000000000, 0.9659258262890683122, 1.000000000000000000, 0.9659258262890683122, 1.000000000000000000, 0.9659258262890683122, 1.000000000000000000, 0.9659258262890683122, 1.000000000000000000, 0.9659258262890683122, 1.000000000000000000, 0.9659258262890683122, 1.000000000000000000, 0.9659258262890683122, 1.000000000000000000, 0.9659258262890683122, 1.000000000000000000, 0.9659258262890683122, 1.000000000000000000, 0.9659258262890683122, 1.000000000000000000, 0.9659258262890683122, 1.000000000000000000, 0.9659258262890683122, 1.000000000000000000, 0.9659258262890683122, 1.000000000000000000, 0.9659258262890683122, 1.000000000000000000, 0.9659258262890683122, 1.000000000000000000, 0.9659258262890683122, 1.000000000000000000, 0.9659258262890683122, 1.000000000000000000, 0.9659258262890683122, 1.000000000000000000, 0.9659258262890683122, 1.000000000000000000, 0.9659258262890683122, 1.000000000000000000, 0.9659258262890683122, 1.000000000000000000, 0.9659258262890683122, 1.000000000000000000, 0.9659258262890683122, 1.000000000000000000, 0.9659258262890683122, 1.000000000000000000, 0.9659258262890683122, 1.000000000000000000, 0.9659258262890683122, 1.000000000000000000, 0.9659258262890683122, 1.000000000000000000, 0.9659258262890683122, 1.000000000000000000, 0.9659258262890683122, 1.000000000000000000, 0.9659258262890683122, 1.000000000000000000, 0.9659258262890683122, 1.000000000000000000, 0.9659258262890683122, 1.000000000000000000, 0.9659258262890683122, 1.000000000000000000, 0.9659258262890683122, 1.000000000000000000, 0.9659258262890683122, 1.000000000000000000, 0.9659258262890683122, 1.000000000000000000, 0.9659258262890683122, 1.000000000000000000, 0.9659258262890683122, 1.000000000000000000, 0.9659258262890683122, 1.000000000000000000, 0.9659258262890683122, 1.000000000000000000, 0.9659258262890683122, 1.000000000000000000, 0.9659258262890683122, 1.000000000000000000, 0.9659258262890683122, 1.000000000000000000, 0.9659258262890683122, 1.000000000000000000, 0.9659258262890683122, 1.000000000000000000, 0.9659258262890683122, 1.000000000000000000, 0.9659258262890683122, 1.000000000000000000, 0.9659258262890683122, 1.000000000000000000, 0.9659258262890683122, 1.000000000000000000, 0.9659258262890683122, 1.000000000000000000, 0.9659258262890683122, 1.000000000000000000, 0.9659258262890683122, 1.000000000000000000, 0.9659258262890683122, 1.000000000000000000, 0.9659258262890683122, 1.000000000000000000, 0.9659258262890683122, 1.000000000000000000, 0.9659258262890683122, 1.000000000000000000, 0.9659258262890683122, 1.000000000000000000, 0.9659258262890683122, 1.000000000000000000, 0.9659258262890683122, 1.000000000000000000, 0.9659258262890683122, 1.000000000000000000, 0.9659258262890683122, 1.000000000000000000, 0.9659258262890683122, 1.000000000000000000, 0.9659258262890683122, 1.000000000000000000, 0.9659258262890683122, 1.000000000000000000, 0.9659258262890683122, 1.000000000000000000, 0.9659258262890683122, 1.000000000000000000, 0.9659258262890683122, 1.000000000000000000, 0.9659258262890683122, 1.000000000000000000, 0.9659258262890683122, 1.000000000000000000, 0.9659258262890683122, 1.000000000000000000, 0.9659258262890683122, 1.000000000000000000, 0.9659258262890683122, 1.000000000000000000, 0.9659258262890683122, 1.000000000000000000, 0.9659258262890683122, 1.000000000000000000, 0.9659258262890683122, 1.000000000000000000, 0.9659258262890683122, 1.000000000000000000, 0.9659258262890683122, 1.000000000000000000, 0.9659258262890683122, 1.000000000000000000, 0.9659258262890683122, 1.000000000000000000, 0.9659258262890683122, 1.000000000000000000, 0.9659258262890683122, 1.000000000000000000, 0.9659258262890683122, 1.000000000000000000, 0.9659258262890683122, 1.000000000000000000, 0.9659258262890683122, 1.000000000000000000, 0.9659258262890683122, 1.000000000000000000, 0.9659258262890683122, 1.000000000000000000, 0.9659258262890683122, 1.000000000000000000, 0.9659258262890683122, 1.000000000000000000, 0.9659258262890683122, 1.000000000000000000, 0.9659258262890683122, 1.000000000000000000, 0.9659258262890683122, 1.000000000000000000, 0.9659258262890683122, 1.000000000000000000, 0.9659258262890683122, 1.000000000000000000, 0.9659258262890683122, 1.000000000000000000, 0.9659258262890683122, 1.000000000000000000, 0.9659258262890683122, 1.000000000000000000, 0.9659258262890683122, 1.000000000000000000, 0.9659258262890683122, 1.000000000000000000, 0.9659258262890683122, 1.000000000000000000, 0.9659258262890683122, 1.000000000000000000, 0.9659258262890683122, 1.000000000000000000) ) ) 
 REPRESENTATION_ITEM ( '' )  SURFACE ( )  );
#28019 = CARTESIAN_POINT ( 'NONE',  ( -0.9908136482939626788, 0.2952755905511811885, 0.1292274648535926551 ) ) ;
#28020 = CARTESIAN_POINT ( 'NONE',  ( -1.653543307086613234, -0.1870078740157479769, 0.4822834645669291653 ) ) ;
#28021 = CARTESIAN_POINT ( 'NONE',  ( 0.4724409448818897572, -0.1265901696524988906, -2.158792650918635037 ) ) ;
#28022 = CARTESIAN_POINT ( 'NONE',  ( 1.614173228346456712, 1.496062992125984037, -0.1372047244094475871 ) ) ;
#28023 = ORIENTED_EDGE ( 'NONE', *, *, #13917, .F. ) ;
#28024 = ORIENTED_EDGE ( 'NONE', *, *, #42584, .F. ) ;
#28025 = CARTESIAN_POINT ( 'NONE',  ( 0.8136482939632553313, 0.2306618581243848609, 0.2411417322834645549 ) ) ;
#28026 = CARTESIAN_POINT ( 'NONE',  ( 1.522309711286089939, -0.5023911411419708095, -0.1820866141732282451 ) ) ;
#28027 = EDGE_CURVE ( 'NONE', #74430, #43140, #26988, .T. ) ;
#28029 = CARTESIAN_POINT ( 'NONE',  ( -1.122047244094487306, 0.1660481256975883668, -0.3530559997133364547 ) ) ;
#28028 = CARTESIAN_POINT ( 'NONE',  ( -1.246719160104985846, -0.3690944881889765550, -0.3153832671262227771 ) ) ;
#28030 = CARTESIAN_POINT ( 'NONE',  ( -9.594673741351310580E-17, 0.3917322834645669549, -2.599718217026559586 ) ) ;
#28031 = CARTESIAN_POINT ( 'NONE',  ( -0.9645669291338576645, 0.1012011053420775880, -0.2882089793578256898 ) ) ;
#28032 = CARTESIAN_POINT ( 'NONE',  ( 1.030183727034121421, -0.05778040916215522460, 0.4822834645669289988 ) ) ;
#28033 = CARTESIAN_POINT ( 'NONE',  ( -1.515748031496062076, 0.1660481256975883668, -0.3530559997133364547 ) ) ;
#28034 = CARTESIAN_POINT ( 'NONE',  ( -0.2690288713910754526, 0.2952755905511810774, -0.1292274648535930714 ) ) ;
#28035 = CARTESIAN_POINT ( 'NONE',  ( -0.3412073490813641308, -0.6046776061558807314, 0.2411417322834647770 ) ) ;
#28036 = CARTESIAN_POINT ( 'NONE',  ( -1.154855643044618851, 0.2306618581243848609, 0.2411417322834645549 ) ) ;
#28037 = CARTESIAN_POINT ( 'NONE',  ( -9.594673741351313045E-17, 0.3917322834645670104, 0.2303149606299211838 ) ) ;
#28038 = CARTESIAN_POINT ( 'NONE',  ( 0.6299212598425204535, -0.1870078740157479769, 0.4822834645669291653 ) ) ;
#28039 = CARTESIAN_POINT ( 'NONE',  ( -0.3392501089628019995, 0.1958661417322832277, -2.065616797900262647 ) ) ;
#28040 = CARTESIAN_POINT ( 'NONE',  ( -1.154855643044618851, 0.1283753931104748280, 0.1820866141732283561 ) ) ;
#28041 = ORIENTED_EDGE ( 'NONE', *, *, #19278, .T. ) ;
#28042 = CARTESIAN_POINT ( 'NONE',  ( -0.2891555358219908833, -0.2891555358219912164, -2.106299212598425452 ) ) ;
#28043 = ORIENTED_EDGE ( 'NONE', *, *, #30705, .T. ) ;
#28044 = CARTESIAN_POINT ( 'NONE',  ( 0.000000000000000000, 2.716535433070866645, 0.000000000000000000 ) ) ;
#28045 = CARTESIAN_POINT ( 'NONE',  ( -1.627296587926508442, -0.6046776061558809534, -0.2411417322834644161 ) ) ;
#28046 = CARTESIAN_POINT ( 'NONE',  ( -1.338582677165353729, -0.1870078740157479769, 0.4822834645669291653 ) ) ;
#28047 = CARTESIAN_POINT ( 'NONE',  ( 0.3996062992125986035, 2.446882876249141962E-17, -0.5905511811023621549 ) ) ;
#28048 = CARTESIAN_POINT ( 'NONE',  ( -1.384514435695537005, 0.2952755905511811885, 0.1292274648535926551 ) ) ;
#28049 = CARTESIAN_POINT ( 'NONE',  ( 1.018715732779042815, 1.601535527459639452, -0.4703312907311759106 ) ) ;
#28050 = CARTESIAN_POINT ( 'NONE',  ( -1.012036180893692183, 0.02791078216816064370, 0.4328096321851915285 ) ) ;
#28051 = CARTESIAN_POINT ( 'NONE',  ( -0.3346456692913378217, 0.1660481256975883391, -0.3530559997133364547 ) ) ;
#28052 = ADVANCED_FACE ( 'NONE', ( #44071 ), #12108, .F. ) ;
#28053 = CARTESIAN_POINT ( 'NONE',  ( -0.2867679344610365999, 0.2867679344610364889, 0.05314960629921249707 ) ) ;
#28054 = CARTESIAN_POINT ( 'NONE',  ( -0.09186351706036663400, -0.3690944881889763329, 0.3153832671262228327 ) ) ;
#28055 = CARTESIAN_POINT ( 'NONE',  ( -0.6627296587926503335, -0.5511811023622046335, 0.09757992244046803654 ) ) ;
#28056 = CARTESIAN_POINT ( 'NONE',  ( -1.384514435695537005, -0.6692913385826773087, -0.1292274648535924053 ) ) ;
#28057 = EDGE_CURVE ( 'NONE', #41276, #31528, #14989, .T. ) ;
#28058 = CARTESIAN_POINT ( 'NONE',  ( 0.9908136482939640111, 0.2952755905511810774, -0.1292274648535930714 ) ) ;
#28059 = CARTESIAN_POINT ( 'NONE',  ( -0.7808398950131222316, -0.3162353388693409650, -0.4822834645669289433 ) ) ;
#28060 = CARTESIAN_POINT ( 'NONE',  ( -0.1958661417322834220, -0.3392501089628018884, 0.09973753280839897650 ) ) ;
#28061 = VERTEX_POINT ( 'NONE', #23904 ) ;
#28062 = CARTESIAN_POINT ( 'NONE',  ( -1.555118110236219930, -0.5400638737290845981, -0.3530559997133363437 ) ) ;
#28063 = CARTESIAN_POINT ( 'NONE',  ( -1.410761154855642463, -0.08942795157527998196, 0.3641732283464567121 ) ) ;
#28064 = DIRECTION ( 'NONE',  ( 1.000000000000000000, 0.000000000000000000, 0.000000000000000000 ) ) ;
#28065 = CARTESIAN_POINT ( 'NONE',  ( -0.1265901696524993347, 0.4724409448818895907, -1.423884514435695525 ) ) ;
#28066 = DIRECTION ( 'NONE',  ( -0.000000000000000000, -0.000000000000000000, 1.000000000000000000 ) ) ;
#28067 = CARTESIAN_POINT ( 'NONE',  ( 0.3917322834645670104, 2.398668435337828261E-17, -0.7401574803149605364 ) ) ;
#28068 = CARTESIAN_POINT ( 'NONE',  ( 0.1958661417322834775, 0.3392501089628018884, -2.433727034120734878 ) ) ;
#28069 = CARTESIAN_POINT ( 'NONE',  ( -0.5314960629921250401, 0.1660481256975885056, 0.3530559997133364547 ) ) ;
#28070 = CARTESIAN_POINT ( 'NONE',  ( -1.463254593175852492, 0.1771653543307087630, 0.09757992244046791164 ) ) ;
#28071 = CARTESIAN_POINT ( 'NONE',  ( 0.1998031496062992463, 0.3460692066303959202, -0.06364829396325462352 ) ) ;
#28073 = CARTESIAN_POINT ( 'NONE',  ( -0.6426939841807746134, 0.004960608223778509643, -0.3437734562760191848 ) ) ;
#28072 = CARTESIAN_POINT ( 'NONE',  ( -0.7443564586553569340, 2.201272808259610692, -0.5309055118110235227 ) ) ;
#28074 = CARTESIAN_POINT ( 'NONE',  ( -1.259842519685038686, -0.1870078740157479769, 0.4822834645669291653 ) ) ;
#28075 = CARTESIAN_POINT ( 'NONE',  ( -0.2034120734908131112, -0.6692913385826773087, -0.1292274648535924053 ) ) ;
#28076 = CARTESIAN_POINT ( 'NONE',  ( 4.797336870675655290E-17, -0.3917322834645669549, -0.001293020176166160412 ) ) ;
#28077 = CARTESIAN_POINT ( 'NONE',  ( 0.4002624671916016896, -0.2845877964562161244, -0.3641732283464567121 ) ) ;
#28078 = CARTESIAN_POINT ( 'NONE',  ( 0.1049643490035303689, 0.3917322834645670104, -0.07808398950131241467 ) ) ;
#28079 = CARTESIAN_POINT ( 'NONE',  ( 0.4921259842519691285, -0.4536011799217368745, -0.2665933059059886201 ) ) ;
#28080 = CARTESIAN_POINT ( 'NONE',  ( 0.7611548556430451917, -0.5023911411419708095, 0.1820866141732285504 ) ) ;
#28081 = CARTESIAN_POINT ( 'NONE',  ( 0.9645669291338588858, 0.1660481256975885056, 0.3530559997133364547 ) ) ;
#28082 = CARTESIAN_POINT ( 'NONE',  ( -0.4396325459317577122, -0.5511811023622048555, -0.09757992244046775898 ) ) ;
#28083 = CARTESIAN_POINT ( 'NONE',  ( -0.2867679344610364334, -0.2867679344610367109, -2.098425196850393526 ) ) ;
#28084 = CARTESIAN_POINT ( 'NONE',  ( -1.227034120734907141, -0.6692913385826773087, -0.1292274648535924053 ) ) ;
#28085 = CARTESIAN_POINT ( 'NONE',  ( -0.1181102362204717315, 0.1771653543307087630, 0.000000000000000000 ) ) ;
#28086 = EDGE_CURVE ( 'NONE', #16126, #30161, #49569, .T. ) ;
#28087 = CARTESIAN_POINT ( 'NONE',  ( -1.443569553805773564, 0.1283753931104746893, -0.1820866141732285504 ) ) ;
#28088 = CARTESIAN_POINT ( 'NONE',  ( 0.4724409448818897572, -0.1265901696524988906, -0.5032808398950130435 ) ) ;
#28089 = CARTESIAN_POINT ( 'NONE',  ( -0.8398950131233585692, 0.1283753931104748280, 0.1820866141732283561 ) ) ;
#28090 = DIRECTION ( 'NONE',  ( -1.000000000000000000, -0.000000000000000000, -0.000000000000000000 ) ) ;
#28091 = CARTESIAN_POINT ( 'NONE',  ( 0.1049868766404206816, 0.2306618581243848609, 0.2411417322834645549 ) ) ;
#28092 = CARTESIAN_POINT ( 'NONE',  ( 1.469816272965879911, -0.5023911411419708095, 0.1820866141732285504 ) ) ;
#28093 = ADVANCED_FACE ( 'NONE', ( #50798 ), #10832, .T. ) ;
#28094 = CARTESIAN_POINT ( 'NONE',  ( 0.6102362204724416372, -0.4536011799217367080, 0.2665933059059888421 ) ) ;
#28095 = CARTESIAN_POINT ( 'NONE',  ( -0.07217847769028813698, -0.2845877964562161244, -0.3641732283464567121 ) ) ;
#28096 = CARTESIAN_POINT ( 'NONE',  ( -0.3346456692913377662, 0.1660481256975883668, -0.3530559997133364547 ) ) ;
#28097 = CARTESIAN_POINT ( 'NONE',  ( -1.220472440944882386, 0.000000000000000000, 0.4445507791589061175 ) ) ;
#28098 = CARTESIAN_POINT ( 'NONE',  ( -1.017060367454067249, -0.08942795157527998196, 0.3641732283464567121 ) ) ;
#28099 = CARTESIAN_POINT ( 'NONE',  ( -0.2362204724409451284, 0.4091458600556402425, -1.979658792650918597 ) ) ;
#28100 = CARTESIAN_POINT ( 'NONE',  ( 0.5380577427821529035, -0.4281496062992124485, 0.4176697321401328655 ) ) ;
#28101 = VERTEX_POINT ( 'NONE', #68937 ) ;
#28102 = CARTESIAN_POINT ( 'NONE',  ( -0.2925321140481930149, -0.2925321140481933480, -1.553149606299212726 ) ) ;
#28103 = EDGE_CURVE ( 'NONE', #23065, #58545, #49979, .T. ) ;
#28104 = CARTESIAN_POINT ( 'NONE',  ( 1.482939632545932307, 0.05413385826771626580, -0.4176697321401330321 ) ) ;
#28105 = CARTESIAN_POINT ( 'NONE',  ( -0.3018372703412066094, -0.004921259842519576551, 0.3153832671262227771 ) ) ;
#28106 = CARTESIAN_POINT ( 'NONE',  ( -0.01968503937007793844, -0.5400638737290844871, 0.3530559997133364547 ) ) ;
#28107 = CARTESIAN_POINT ( 'NONE',  ( -1.397637795275589623, -0.5400638737290845981, -0.3530559997133363437 ) ) ;
#28108 = CARTESIAN_POINT ( 'NONE',  ( 1.561679790026247350, 0.05413385826771626580, -0.4176697321401330321 ) ) ;
#28109 = CARTESIAN_POINT ( 'NONE',  ( 1.299212598425197429, -0.6692913385826771977, 8.415575281601705876E-17 ) ) ;
#28110 = CARTESIAN_POINT ( 'NONE',  ( -0.7152230971128602510, -0.08942795157528024563, -0.3641732283464568787 ) ) ;
#28111 = CYLINDRICAL_SURFACE ( 'NONE', #80269, 0.4724409448818898682 ) ;
#28112 = CARTESIAN_POINT ( 'NONE',  ( 0.3460692066303959757, -0.1998031496062991907, 0.05249343832020996609 ) ) ;
#28113 = CARTESIAN_POINT ( 'NONE',  ( 0.1049643490035303967, 0.3917322834645670659, -2.352381520506248602 ) ) ;
#28114 = CARTESIAN_POINT ( 'NONE',  ( -3.892840969167625786, 2.712230453466949687, -0.5314960629921260393 ) ) ;
#28115 = CARTESIAN_POINT ( 'NONE',  ( 1.128608923884514947, 0.1283753931104748280, 0.1820866141732283561 ) ) ;
#28116 = CARTESIAN_POINT ( 'NONE',  ( 0.4064735117398315944, 0.004960608223780119466, 0.3437734562760182411 ) ) ;
#28117 = CARTESIAN_POINT ( 'NONE',  ( 0.9186351706036751663, -0.6046776061558807314, 0.2411417322834647770 ) ) ;
#28118 = CARTESIAN_POINT ( 'NONE',  ( -0.1049643490035307020, 0.3917322834645669549, -2.453412073490813139 ) ) ;
#28119 = CARTESIAN_POINT ( 'NONE',  ( 1.128608923884515169, -0.5023911411419708095, -0.1820866141732282451 ) ) ;
#28120 = CARTESIAN_POINT ( 'NONE',  ( 0.2559055118110243332, 0.1660481256975885056, 0.3530559997133364547 ) ) ;
#28121 = CARTESIAN_POINT ( 'NONE',  ( -0.2887139107611542133, -0.6046776061558809534, -0.2411417322834644161 ) ) ;
#28122 = CARTESIAN_POINT ( 'NONE',  ( 1.646981627296588035, -0.3162353388693405765, 0.4822834645669290543 ) ) ;
#28123 = CARTESIAN_POINT ( 'NONE',  ( 0.1998031496062992740, 0.3460692066303959757, -2.034120734908136718 ) ) ;
#28124 = CARTESIAN_POINT ( 'NONE',  ( 0.2427821522309716595, -0.2845877964562161244, -0.3641732283464567121 ) ) ;
#28125 = COLOUR_RGB ( '', 0.66274510, 0.83137255, 0.94901961) ;
#28126 = EDGE_LOOP ( 'NONE', ( #82376, #26606, #9619, #77399 ) ) ;
#28127 = CARTESIAN_POINT ( 'NONE',  ( 0.2867679344610366554, -0.2867679344610365999, -0.5676046176191095194 ) ) ;
#28128 = ORIENTED_EDGE ( 'NONE', *, *, #15253, .T. ) ;
#28129 = CARTESIAN_POINT ( 'NONE',  ( -0.5380577427821514602, -0.4281496062992127816, -0.4176697321401328100 ) ) ;
#28130 = CARTESIAN_POINT ( 'NONE',  ( 1.227034120734908917, -0.6692913385826771977, 0.1292274648535927661 ) ) ;
#28131 = CARTESIAN_POINT ( 'NONE',  ( 0.1246719160104994284, 0.2952755905511810774, -0.1292274648535930714 ) ) ;
#28132 = CARTESIAN_POINT ( 'NONE',  ( -0.3215223097112853146, -0.08942795157528024563, -0.3641732283464568787 ) ) ;
#28133 = CARTESIAN_POINT ( 'NONE',  ( 0.8595800524934390507, -0.3162353388693405765, 0.4822834645669290543 ) ) ;
#28134 = CARTESIAN_POINT ( 'NONE',  ( -0.9514435695538050464, -0.05778040916215560624, -0.4822834645669293319 ) ) ;
#28135 = CARTESIAN_POINT ( 'NONE',  ( -0.2690288713910754526, 0.2952755905511810774, -0.1292274648535930714 ) ) ;
#28136 = CARTESIAN_POINT ( 'NONE',  ( -0.8858267716535425107, 0.1660481256975883668, -0.3530559997133364547 ) ) ;
#28137 = CARTESIAN_POINT ( 'NONE',  ( 1.102362204724410155, -0.1870078740157479769, 0.4822834645669291653 ) ) ;
#28138 = CARTESIAN_POINT ( 'NONE',  ( 0.7480314960629927956, -0.6692913385826771977, 8.415575281601705876E-17 ) ) ;
#28139 = CARTESIAN_POINT ( 'NONE',  ( 0.9383202099737538715, -0.05778040916215560624, -0.4822834645669293319 ) ) ;
#28140 = CARTESIAN_POINT ( 'NONE',  ( 0.1958661417322834775, 0.3392501089628018884, -0.6089238845144356871 ) ) ;
#28141 = CARTESIAN_POINT ( 'NONE',  ( 0.1837270341207357105, -0.5023911411419708095, -0.1820866141732282451 ) ) ;
#28142 = ORIENTED_EDGE ( 'NONE', *, *, #28554, .F. ) ;
#28143 = CARTESIAN_POINT ( 'NONE',  ( -0.2891555358219911054, 0.2891555358219909388, -1.122047244094488194 ) ) ;
#28144 = ORIENTED_EDGE ( 'NONE', *, *, #53636, .F. ) ;
#28145 = CARTESIAN_POINT ( 'NONE',  ( -0.7808398950131225646, -0.08942795157527998196, 0.3641732283464567121 ) ) ;
#28146 = CARTESIAN_POINT ( 'NONE',  ( 0.1377952755905518800, 0.1660481256975883668, -0.3530559997133364547 ) ) ;
#28147 = CARTESIAN_POINT ( 'NONE',  ( 2.872342878167411406, 1.064797240280315194, 0.04222672046126994816 ) ) ;
#28148 = CARTESIAN_POINT ( 'NONE',  ( -0.1771653543307080136, -0.5400638737290844871, 0.3530559997133364547 ) ) ;
#28149 = CARTESIAN_POINT ( 'NONE',  ( -0.4133858267716528645, 0.1660481256975883668, -0.3530559997133364547 ) ) ;
#28150 = CARTESIAN_POINT ( 'NONE',  ( -1.496062992125983815, -0.1870078740157479769, 0.4822834645669291653 ) ) ;
#28151 = EDGE_CURVE ( 'NONE', #21435, #25849, #45776, .T. ) ;
#28152 = CARTESIAN_POINT ( 'NONE',  ( -1.266404199475064773, -0.3162353388693405765, 0.4822834645669290543 ) ) ;
#28153 = CARTESIAN_POINT ( 'NONE',  ( 1.272965879265092637, -0.3690944881889765550, -0.3153832671262227771 ) ) ;
#28154 = CARTESIAN_POINT ( 'NONE',  ( -1.607611548556429737, 0.2952755905511810774, -0.1292274648535930714 ) ) ;
#28155 = CARTESIAN_POINT ( 'NONE',  ( 0.2524556255358376688, 0.1533185143264484962, 5.612478741320920506 ) ) ;
#28156 = CARTESIAN_POINT ( 'NONE',  ( 0.6102362204724416372, -0.4536011799217367080, 0.2665933059059888421 ) ) ;
#28157 = CARTESIAN_POINT ( 'NONE',  ( 0.2165354330708668673, -0.5400638737290844871, 0.3530559997133364547 ) ) ;
#28158 = CARTESIAN_POINT ( 'NONE',  ( 0.2099737532808405305, -0.6046776061558807314, 0.2411417322834647770 ) ) ;
#28159 = ORIENTED_EDGE ( 'NONE', *, *, #3251, .F. ) ;
#28160 = CARTESIAN_POINT ( 'NONE',  ( 0.2925321140481932369, 0.2925321140481932369, -1.555118110236220597 ) ) ;
#28161 = CARTESIAN_POINT ( 'NONE',  ( -0.5905511811023615998, 0.2066929133858268208, 0.000000000000000000 ) ) ;
#28162 = CARTESIAN_POINT ( 'NONE',  ( 0.2925321140481932369, -0.2925321140481931814, -1.277559055118109965 ) ) ;
#28163 = CARTESIAN_POINT ( 'NONE',  ( 0.2925321140481932369, -0.2925321140481931814, -0.4901574803149606474 ) ) ;
#28164 = CARTESIAN_POINT ( 'NONE',  ( -0.5839895013123351797, 0.2952755905511810774, -0.1292274648535930714 ) ) ;
#28165 = CARTESIAN_POINT ( 'NONE',  ( 0.1265901696524990294, -0.4724409448818896462, 0.07217847769028870597 ) ) ;
#28166 = CARTESIAN_POINT ( 'NONE',  ( -0.3392501089628017219, -0.1958661417322836718, -2.341863517060367439 ) ) ;
#28167 = CARTESIAN_POINT ( 'NONE',  ( -1.646981627296586703, -0.08942795157527998196, 0.3641732283464567121 ) ) ;
#28168 = CARTESIAN_POINT ( 'NONE',  ( 0.7545931758530188826, -0.6692913385826771977, 0.1292274648535927661 ) ) ;
#28169 = CARTESIAN_POINT ( 'NONE',  ( 0.7545931758530189937, 0.2952755905511810774, -0.1292274648535930714 ) ) ;
#28170 = CARTESIAN_POINT ( 'NONE',  ( -0.3871391076115476282, -0.08942795157527998196, 0.3641732283464567121 ) ) ;
#28171 = CARTESIAN_POINT ( 'NONE',  ( -0.01968503937007793844, -0.5400638737290844871, 0.3530559997133364547 ) ) ;
#28172 = CARTESIAN_POINT ( 'NONE',  ( 0.1265901696524990294, -0.4724409448818896462, -1.736876640419947604 ) ) ;
#28173 = CARTESIAN_POINT ( 'NONE',  ( -0.2493438320209966919, -0.3690944881889763329, 0.3153832671262228327 ) ) ;
#28174 = CARTESIAN_POINT ( 'NONE',  ( -0.5052493438320203589, -0.6692913385826771977, 0.1292274648535927661 ) ) ;
#28175 = CARTESIAN_POINT ( 'NONE',  ( -0.2891555358219909388, -0.2891555358219912164, -1.710629921259842590 ) ) ;
#28176 = CARTESIAN_POINT ( 'NONE',  ( -1.699475065616797398, 0.2952755905511811885, 0.1292274648535926551 ) ) ;
#28177 = CARTESIAN_POINT ( 'NONE',  ( 0.1640419947506569498, -0.08942795157527998196, 0.3641732283464567121 ) ) ;
#28178 = CARTESIAN_POINT ( 'NONE',  ( 1.679790026246720025, 0.1283753931104748280, 0.1820866141732283561 ) ) ;
#28179 = CARTESIAN_POINT ( 'NONE',  ( -1.108923884514435132, -0.3162353388693405765, 0.4822834645669290543 ) ) ;
#28180 = CARTESIAN_POINT ( 'NONE',  ( -0.6627296587926501115, 0.1771653543307087075, -0.09757992244046823083 ) ) ;
#28181 = DIRECTION ( 'NONE',  ( 0.000000000000000000, -0.6427876096865392519, -0.7660444431189781245 ) ) ;
#28182 = CARTESIAN_POINT ( 'NONE',  ( -1.338582677165353729, -0.1870078740157480879, -0.4822834645669291653 ) ) ;
#28183 = CARTESIAN_POINT ( 'NONE',  ( -0.6430446194225712953, 0.05413385826771626580, -0.4176697321401330321 ) ) ;
#28184 = CARTESIAN_POINT ( 'NONE',  ( -0.1377952755905504645, -0.5400638737290845981, -0.3530559997133363437 ) ) ;
#28185 = CARTESIAN_POINT ( 'NONE',  ( 0.3996062992125984925, 0.1070741851644054637, -2.406167979002624246 ) ) ;
#28186 = CARTESIAN_POINT ( 'NONE',  ( -0.3917322834645669549, -7.196005306013483243E-17, -2.481607980806087799 ) ) ;
#28187 = CARTESIAN_POINT ( 'NONE',  ( -2.105021046755463754, 1.366082762360717018, -0.4426340671871326071 ) ) ;
#28188 = CARTESIAN_POINT ( 'NONE',  ( 0.5314960629921267055, -0.4536011799217367080, 0.2665933059059888421 ) ) ;
#28189 = CARTESIAN_POINT ( 'NONE',  ( 1.049868766404200127, -0.6046776061558809534, -0.2411417322834644161 ) ) ;
#28190 = CARTESIAN_POINT ( 'NONE',  ( -1.043307086614172707, 0.07958543189024071263, -0.2665933059059888421 ) ) ;
#28191 = CARTESIAN_POINT ( 'NONE',  ( 1.332020997375329197, -0.3162353388693405765, 0.4822834645669290543 ) ) ;
#28192 = CARTESIAN_POINT ( 'NONE',  ( -1.450131233595799651, -0.5511811023622046335, 0.09757992244046803654 ) ) ;
#28193 = CARTESIAN_POINT ( 'NONE',  ( -0.3740157480314953431, -0.5400638737290845981, -0.3530559997133363437 ) ) ;
#28194 = CARTESIAN_POINT ( 'NONE',  ( 0.2887139107611556010, 0.1283753931104746893, -0.1820866141732285504 ) ) ;
#28195 = DIRECTION ( 'NONE',  ( -1.000000000000000000, -0.000000000000000000, -0.000000000000000000 ) ) ;
#28196 = CARTESIAN_POINT ( 'NONE',  ( 0.5708661417322841158, -0.4536011799217368745, -0.2665933059059886201 ) ) ;
#28197 = CARTESIAN_POINT ( 'NONE',  ( 0.2034120734908144990, -0.6692913385826771977, 0.1292274648535927661 ) ) ;
#28198 = CARTESIAN_POINT ( 'NONE',  ( 0.1070741851644054776, -0.3996062992125984925, -0.1620734908136483021 ) ) ;
#28199 = CARTESIAN_POINT ( 'NONE',  ( -0.5446194225721777693, -0.3162353388693409650, -0.4822834645669289433 ) ) ;
#28200 = CARTESIAN_POINT ( 'NONE',  ( -0.3917322834645671215, 0.1049643490035301469, -2.007217847769029007 ) ) ;
#28201 = CARTESIAN_POINT ( 'NONE',  ( 1.167979002624672580, -0.004921259842519870586, -0.3153832671262229437 ) ) ;
#28202 = CARTESIAN_POINT ( 'NONE',  ( 0.05249343832021075018, -0.6046776061558807314, 0.2411417322834647770 ) ) ;
#28203 = CARTESIAN_POINT ( 'NONE',  ( -0.4921259842519677963, 0.1660481256975883668, -0.3530559997133364547 ) ) ;
#28204 = CARTESIAN_POINT ( 'NONE',  ( -0.4855643044619415427, -0.004921259842519870586, -0.3153832671262229437 ) ) ;
#28205 = CARTESIAN_POINT ( 'NONE',  ( -1.586052503253848167, 1.023622047244095556, 0.1653254495020564929 ) ) ;
#28206 = CARTESIAN_POINT ( 'NONE',  ( -0.03937007874015669567, 0.1771653543307087630, 0.000000000000000000 ) ) ;
#28207 = CARTESIAN_POINT ( 'NONE',  ( 0.4002624671916016896, -0.05778040916215522460, 0.4822834645669289988 ) ) ;
#28208 = CARTESIAN_POINT ( 'NONE',  ( -0.7414698162729651543, 0.1771653543307087075, -0.09757992244046823083 ) ) ;
#28209 = CARTESIAN_POINT ( 'NONE',  ( 0.2925321140481932369, 0.2925321140481932369, -0.8444881889763780070 ) ) ;
#28210 = CARTESIAN_POINT ( 'NONE',  ( -1.266404199475064773, -0.05778040916215560624, -0.4822834645669293319 ) ) ;
#28211 = DIRECTION ( 'NONE',  ( -0.000000000000000000, -1.000000000000000000, -1.408710688920637755E-15 ) ) ;
#28212 = ORIENTED_EDGE ( 'NONE', *, *, #4866, .T. ) ;
#28213 = CARTESIAN_POINT ( 'NONE',  ( -1.115485564304461219, -0.3690944881889763329, 0.3153832671262228327 ) ) ;
#28214 = CARTESIAN_POINT ( 'NONE',  ( -0.1115485564304456306, 0.2952755905511810774, -0.1292274648535930714 ) ) ;
#28215 = CARTESIAN_POINT ( 'NONE',  ( 0.3948464311378731550, 0.01987007963502800123, -1.220472440944882608 ) ) ;
#28216 = CARTESIAN_POINT ( 'NONE',  ( -0.7020997375328074108, -0.05778040916215522460, 0.4822834645669289988 ) ) ;
#28217 = LINE ( 'NONE', #47987, #14949 ) ;
#28218 = CARTESIAN_POINT ( 'NONE',  ( 1.292650918635171564, -0.6692913385826773087, -0.1292274648535924053 ) ) ;
#28219 = CARTESIAN_POINT ( 'NONE',  ( 0.6758530183727039509, -0.6692913385826771977, 0.1292274648535927661 ) ) ;
#28220 = CARTESIAN_POINT ( 'NONE',  ( -0.2489931967792003153, 0.004960608223781096116, -0.3437734562760177970 ) ) ;
#28221 = DIRECTION ( 'NONE',  ( -0.000000000000000000, -1.000000000000000000, -0.000000000000000000 ) ) ;
#28222 = CARTESIAN_POINT ( 'NONE',  ( 0.2896989933648236315, -0.05817964957694448519, 5.534220241493013503 ) ) ;
#28223 = B_SPLINE_CURVE_WITH_KNOTS ( 'NONE', 3,
 ( #20247, #45896, #47152, #15192 ),
 .UNSPECIFIED., .F., .F.,
 ( 4, 4 ),
 ( 0.02768037499106720811, 0.02925281078410804994 ),
 .UNSPECIFIED. ) ;
#28224 = CARTESIAN_POINT ( 'NONE',  ( -1.601049868766403650, -0.6046776061558807314, 0.2411417322834647770 ) ) ;
#28225 = CARTESIAN_POINT ( 'NONE',  ( 0.2925321140481932369, -0.2925321140481932369, -0.4133858267716534196 ) ) ;
#28226 = EDGE_LOOP ( 'NONE', ( #77924, #41682, #38583, #57737 ) ) ;
#28227 = CARTESIAN_POINT ( 'NONE',  ( -0.4724409448818890911, -0.1870078740157480601, -0.3641732283464567677 ) ) ;
#28228 = CARTESIAN_POINT ( 'NONE',  ( -0.3917322834645671215, 0.1049643490035301469, -2.072178477690288734 ) ) ;
#28229 = VERTEX_POINT ( 'NONE', #63441 ) ;
#28230 = CARTESIAN_POINT ( 'NONE',  ( 0.7086614173228352742, -0.1870078740157480879, -0.4822834645669291653 ) ) ;
#28231 = CARTESIAN_POINT ( 'NONE',  ( -0.05905511811023545637, -0.5400638737290845981, -0.3530559997133363437 ) ) ;
#28232 = CARTESIAN_POINT ( 'NONE',  ( -0.8923884514435688198, -0.6046776061558807314, 0.2411417322834647770 ) ) ;
#28233 = CARTESIAN_POINT ( 'NONE',  ( 1.450131233595801428, -0.6692913385826773087, -0.1292274648535924053 ) ) ;
#28234 = CARTESIAN_POINT ( 'NONE',  ( -0.7611548556430438595, -0.5023911411419708095, -0.1820866141732282451 ) ) ;
#28235 = CARTESIAN_POINT ( 'NONE',  ( 0.03775315452881272682, 1.064486638582849531, -1.473643470224546892 ) ) ;
#28236 = CARTESIAN_POINT ( 'NONE',  ( 0.4133858267716541968, 0.1660481256975885056, 0.3530559997133364547 ) ) ;
#28237 = CARTESIAN_POINT ( 'NONE',  ( 0.3740157480314966754, 0.07958543189024071263, -0.2665933059059888421 ) ) ;
#28238 = CARTESIAN_POINT ( 'NONE',  ( -0.6627296587926501115, 0.2952755905511810774, -0.1292274648535930714 ) ) ;
#28239 = CARTESIAN_POINT ( 'NONE',  ( -0.3917322834645668994, -0.1049643490035306742, -1.700768085792964346 ) ) ;
#28240 = CARTESIAN_POINT ( 'NONE',  ( -1.207349081364828436, -0.6046776061558807314, 0.2411417322834647770 ) ) ;
#28241 = CARTESIAN_POINT ( 'NONE',  ( 0.5314960629921349211, 2.716535433070866645, -2.543486866223387377 ) ) ;
#28242 = CARTESIAN_POINT ( 'NONE',  ( 0.9251968503937015864, 0.1660481256975883668, -0.3530559997133364547 ) ) ;
#28243 = CARTESIAN_POINT ( 'NONE',  ( 1.141732283464567788, -0.5511811023622047445, 6.969142054262312111E-17 ) ) ;
#28244 = ORIENTED_EDGE ( 'NONE', *, *, #73800, .F. ) ;
#28245 = CARTESIAN_POINT ( 'NONE',  ( 0.3917322834645670659, -0.1049643490035303273, -2.785452386647981449 ) ) ;
#28246 = CARTESIAN_POINT ( 'NONE',  ( -0.3674540682414689785, 0.2306618581243848609, 0.2411417322834645549 ) ) ;
#28247 = ORIENTED_EDGE ( 'NONE', *, *, #43470, .T. ) ;
#28248 = CARTESIAN_POINT ( 'NONE',  ( 0.3477690288713918276, 0.1771653543307087630, 0.09757992244046791164 ) ) ;
#28249 = CARTESIAN_POINT ( 'NONE',  ( -1.397637795275589623, 0.1660481256975885056, 0.3530559997133364547 ) ) ;
#28250 = CARTESIAN_POINT ( 'NONE',  ( 0.8202099737532813073, 0.2952755905511811885, 0.1292274648535926551 ) ) ;
#28251 = CARTESIAN_POINT ( 'NONE',  ( 0.9842519685039375910, 0.2952755905511811885, 0.000000000000000000 ) ) ;
#28252 = CARTESIAN_POINT ( 'NONE',  ( -0.3280839895013117347, -0.4281496062992124485, 0.4176697321401328655 ) ) ;
#28253 = CARTESIAN_POINT ( 'NONE',  ( -0.2624671916010490880, -0.6046776061558807314, 0.2411417322834647770 ) ) ;
#28254 = CARTESIAN_POINT ( 'NONE',  ( 0.3917322834645669549, 0.1049643490035304660, -2.099081364829396446 ) ) ;
#28255 = CARTESIAN_POINT ( 'NONE',  ( -1.430446194225721390, -0.4281496062992124485, 0.4176697321401328655 ) ) ;
#28256 = CARTESIAN_POINT ( 'NONE',  ( -0.6496062992125976043, 0.1660481256975883668, -0.3530559997133364547 ) ) ;
#28257 = CARTESIAN_POINT ( 'NONE',  ( -0.4199475065616791736, -0.5023911411419708095, 0.1820866141732285504 ) ) ;
#28258 = CARTESIAN_POINT ( 'NONE',  ( 1.108923884514436686, -0.3162353388693409650, -0.4822834645669289433 ) ) ;
#28259 = CARTESIAN_POINT ( 'NONE',  ( 0.2867679344610365999, -0.2867679344610365444, -2.925196850393700920 ) ) ;
#28260 = CARTESIAN_POINT ( 'NONE',  ( -0.8333333333333323711, -0.6692913385826773087, -0.1292274648535924053 ) ) ;
#28261 = CARTESIAN_POINT ( 'NONE',  ( -0.1998031496062991630, -0.3460692066303959202, 0.01509186351706036204 ) ) ;
#28262 = CARTESIAN_POINT ( 'NONE',  ( 0.8136482939632553313, 0.2306618581243848609, 0.2411417322834645549 ) ) ;
#28263 = CARTESIAN_POINT ( 'NONE',  ( -0.1998031496062994683, 0.3460692066303958092, -2.060367454068241511 ) ) ;
#28264 = CARTESIAN_POINT ( 'NONE',  ( 3.934091615812861154, 1.087812615256082083, 0.1522392691923797337 ) ) ;
#28265 = CARTESIAN_POINT ( 'NONE',  ( -0.05905511811023545637, 0.1660481256975885056, 0.3530559997133364547 ) ) ;
#28266 = CARTESIAN_POINT ( 'NONE',  ( -1.345144356955379816, -0.2845877964562159024, 0.3641732283464567677 ) ) ;
#28268 = CARTESIAN_POINT ( 'NONE',  ( -1.603475055217291612, 0.7793870273546338323, 0.04573490813648253134 ) ) ;
#28267 = CARTESIAN_POINT ( 'NONE',  ( 1.108923884514436686, -0.2845877964562161244, -0.3641732283464567121 ) ) ;
#28269 = CARTESIAN_POINT ( 'NONE',  ( 0.4091458600556403535, 0.2362204724409449896, -0.5229658792650918597 ) ) ;
#28270 = CARTESIAN_POINT ( 'NONE',  ( 1.135170603674541256, -0.5511811023622048555, -0.09757992244046775898 ) ) ;
#28271 = CARTESIAN_POINT ( 'NONE',  ( 0.7742782152230978099, -0.4281496062992124485, 0.4176697321401328655 ) ) ;
#28272 = CARTESIAN_POINT ( 'NONE',  ( 0.1058382717557500852, -0.3949938075777408852, -0.6345144356955381149 ) ) ;
#28273 = CARTESIAN_POINT ( 'NONE',  ( -0.4527559055118102749, 0.1660481256975885056, 0.3530559997133364547 ) ) ;
#28274 = PLANE ( 'NONE',  #82173 ) ;
#28275 = CARTESIAN_POINT ( 'NONE',  ( 1.318897637795276356, 0.07958543189024071263, -0.2665933059059888421 ) ) ;
#28276 = CARTESIAN_POINT ( 'NONE',  ( -0.2624671916010490880, 0.2306618581243847221, -0.2411417322834647770 ) ) ;
#28277 = CARTESIAN_POINT ( 'NONE',  ( 0.3420746716998660508, -0.1974969037888704149, -0.4967191601049869010 ) ) ;
#28278 = CARTESIAN_POINT ( 'NONE',  ( 1.069553805774278832, 0.2952755905511810774, -0.1292274648535930714 ) ) ;
#28279 = CARTESIAN_POINT ( 'NONE',  ( -0.06561679790026180015, -0.4281496062992127816, -0.4176697321401328100 ) ) ;
#28280 = CARTESIAN_POINT ( 'NONE',  ( 0.6233595800524942554, -0.08942795157528024563, -0.3641732283464568787 ) ) ;
#28281 = CARTESIAN_POINT ( 'NONE',  ( -0.2362204724409447953, -0.4091458600556404646, -0.1423884514435695414 ) ) ;
#28282 = CARTESIAN_POINT ( 'NONE',  ( 0.6102362204724416372, 0.07958543189024071263, -0.2665933059059888421 ) ) ;
#28283 = CARTESIAN_POINT ( 'NONE',  ( -1.574803149606298192, -0.1870078740157480879, -0.4822834645669291653 ) ) ;
#28284 = CARTESIAN_POINT ( 'NONE',  ( -0.3460692066303960313, 0.1998031496062989965, -1.205380577427821454 ) ) ;
#28285 = CARTESIAN_POINT ( 'NONE',  ( 0.9186351706036752773, 0.2306618581243847221, -0.2411417322834647770 ) ) ;
#28286 = CARTESIAN_POINT ( 'NONE',  ( -0.2867679344610364334, -0.2867679344610367109, -0.9960629921259842590 ) ) ;
#28287 = CARTESIAN_POINT ( 'NONE',  ( 1.686351706036745890, 0.1771653543307087630, 0.09757992244046791164 ) ) ;
#28288 = CARTESIAN_POINT ( 'NONE',  ( 0.08874907683610111508, -2.191421614605370878E-15, 0.4445507791589071167 ) ) ;
#28289 = CARTESIAN_POINT ( 'NONE',  ( 0.1574803149606306130, -0.1870078740157479769, 0.3641732283464567677 ) ) ;
#28290 = CARTESIAN_POINT ( 'NONE',  ( 0.1312335958005257930, 0.2306618581243847221, -0.2411417322834647770 ) ) ;
#28291 =( REPRESENTATION_RELATIONSHIP ('NONE','NONE', #79348, #33107 ) REPRESENTATION_RELATIONSHIP_WITH_TRANSFORMATION ( #82621 )SHAPE_REPRESENTATION_RELATIONSHIP( ) );
#28292 = CARTESIAN_POINT ( 'NONE',  ( 1.601049868766404982, -0.5023911411419708095, -0.1820866141732282451 ) ) ;
#28293 = CARTESIAN_POINT ( 'NONE',  ( -1.515748031496062076, 0.07958543189024071263, -0.2665933059059888421 ) ) ;
#28294 = CARTESIAN_POINT ( 'NONE',  ( -1.259842519685038686, -0.1870078740157479769, 0.4822834645669291653 ) ) ;
#28295 = CARTESIAN_POINT ( 'NONE',  ( 0.5577427821522316087, -0.05778040916215522460, 0.4822834645669289988 ) ) ;
#28296 = CARTESIAN_POINT ( 'NONE',  ( 1.397637795275591177, 0.1660481256975883668, -0.3530559997133364547 ) ) ;
#28297 = CARTESIAN_POINT ( 'NONE',  ( 6.267877385347666114E-17, 1.062992125984252745, 2.874015748031495843 ) ) ;
#28298 = CARTESIAN_POINT ( 'NONE',  ( 0.3805774278215230400, 0.05413385826771626580, -0.4176697321401330321 ) ) ;
#28299 = CARTESIAN_POINT ( 'NONE',  ( -9.787531504996566615E-17, 0.3996062992125985480, 0.2381889763779527491 ) ) ;
#28300 = CARTESIAN_POINT ( 'NONE',  ( 1.168682819302787168, 2.409604939980833412E-17, -0.3464511005275205946 ) ) ;
#28301 = CARTESIAN_POINT ( 'NONE',  ( 0.9514435695538062676, -0.3162353388693409650, -0.4822834645669289433 ) ) ;
#28302 = CARTESIAN_POINT ( 'NONE',  ( -1.607611548556429737, -0.5511811023622046335, 0.09757992244046803654 ) ) ;
#28303 = CARTESIAN_POINT ( 'NONE',  ( 1.194225721784777594, -0.004921259842519576551, 0.3153832671262227771 ) ) ;
#28304 = CARTESIAN_POINT ( 'NONE',  ( -1.640419947506561060, -0.004921259842519576551, 0.3153832671262227771 ) ) ;
#28305 = CARTESIAN_POINT ( 'NONE',  ( -0.7086614173228339419, -0.1870078740157479769, 0.3641732283464567677 ) ) ;
#28306 = DIRECTION ( 'NONE',  ( -1.000000000000000000, 0.000000000000000000, 0.000000000000000000 ) ) ;
#28307 = CARTESIAN_POINT ( 'NONE',  ( 0.6758530183727039509, 0.1771653543307087075, -0.09757992244046823083 ) ) ;
#28308 = CARTESIAN_POINT ( 'NONE',  ( 0.09842519685039434474, 0.1660481256975885056, 0.3530559997133364547 ) ) ;
#28309 = CARTESIAN_POINT ( 'NONE',  ( 0.6036745406824153282, -0.6046776061558807314, 0.2411417322834647770 ) ) ;
#28310 = B_SPLINE_CURVE_WITH_KNOTS ( 'NONE', 3,
 ( #46058, #20407, #77234, #52368 ),
 .UNSPECIFIED., .F., .F.,
 ( 4, 4 ),
 ( 1.999999999910059834E-07, 0.006970199999999936863 ),
 .UNSPECIFIED. ) ;
#28311 = CARTESIAN_POINT ( 'NONE',  ( -0.3740157480314953431, 0.1660481256975885056, 0.3530559997133364547 ) ) ;
#28312 = CARTESIAN_POINT ( 'NONE',  ( 0.3346456692913390985, 0.07958543189024085140, 0.2665933059059887866 ) ) ;
#28313 = AXIS2_PLACEMENT_3D ( 'NONE', #2905, #74440, #47914 ) ;
#28314 = CARTESIAN_POINT ( 'NONE',  ( 1.017060367454068581, -0.05778040916215560624, -0.4822834645669293319 ) ) ;
#28315 = DIRECTION ( 'NONE',  ( 0.000000000000000000, 0.000000000000000000, 1.000000000000000000 ) ) ;
#28316 = CARTESIAN_POINT ( 'NONE',  ( -0.9055118110236215490, 0.2952755905511811885, 0.000000000000000000 ) ) ;
#28318 = CARTESIAN_POINT ( 'NONE',  ( -0.1070741851644051862, -0.3996062992125986590, -0.7020997375328084100 ) ) ;
#28317 = CARTESIAN_POINT ( 'NONE',  ( -1.574803149606298636, -0.1870078740157479769, 0.3641732283464567677 ) ) ;
#28319 = CARTESIAN_POINT ( 'NONE',  ( -0.1341536278048670039, 1.050682278017461835, 0.2827841492639485144 ) ) ;
#28320 = CARTESIAN_POINT ( 'NONE',  ( -0.9645669291338575535, 0.1660481256975883668, -0.3530559997133364547 ) ) ;
#28321 = CARTESIAN_POINT ( 'NONE',  ( 0.07217847769028949700, -0.05778040916215560624, -0.4822834645669293319 ) ) ;
#28322 = CARTESIAN_POINT ( 'NONE',  ( -0.4724409448818899238, 0.1265901696524986686, 0.1246719160104986929 ) ) ;
#28323 = CARTESIAN_POINT ( 'NONE',  ( -9.674558042662121740E-17, 0.3949938075777409963, -2.362204724409449064 ) ) ;
#28324 = ORIENTED_EDGE ( 'NONE', *, *, #24847, .T. ) ;
#28325 = CARTESIAN_POINT ( 'NONE',  ( 0.7677165354330716118, 0.07958543189024071263, -0.2665933059059888421 ) ) ;
#28326 = CARTESIAN_POINT ( 'NONE',  ( -0.3917322834645669549, -0.1049643490035306603, -0.8254593175853015552 ) ) ;
#28327 = CARTESIAN_POINT ( 'NONE',  ( 1.069553805774278610, -0.6692913385826771977, 0.1292274648535927661 ) ) ;
#28328 = CARTESIAN_POINT ( 'NONE',  ( 6.267877318470707138E-17, 0.000000000000000000, -1.850393700787401619 ) ) ;
#28329 = CARTESIAN_POINT ( 'NONE',  ( -1.522309711286088607, 0.1283753931104746893, -0.1820866141732285504 ) ) ;
#28330 = CARTESIAN_POINT ( 'NONE',  ( 1.515748031496063408, 0.1660481256975885056, 0.3530559997133364547 ) ) ;
#28331 = CARTESIAN_POINT ( 'NONE',  ( -1.535433070866141225, 0.2952755905511811885, 0.000000000000000000 ) ) ;
#28332 = CARTESIAN_POINT ( 'NONE',  ( -0.3392501089628019439, 0.1958661417322832554, -0.2637602117772160915 ) ) ;
#28333 = CARTESIAN_POINT ( 'NONE',  ( 8.195543980992789655E-16, -0.1870078740157480879, -0.4822834645669291653 ) ) ;
#28334 = CARTESIAN_POINT ( 'NONE',  ( -0.4658792650918627265, -0.08942795157527998196, 0.3641732283464567121 ) ) ;
#28336 = ADVANCED_FACE ( 'NONE', ( #18827 ), #5777, .F. ) ;
#28335 = CARTESIAN_POINT ( 'NONE',  ( 0.9842519685039375910, 0.2952755905511811885, 0.000000000000000000 ) ) ;
#28337 = CARTESIAN_POINT ( 'NONE',  ( -0.1443569553805768291, 0.05413385826771666132, 0.4176697321401328100 ) ) ;
#28338 = DIRECTION ( 'NONE',  ( 0.000000000000000000, 0.000000000000000000, 1.000000000000000000 ) ) ;
#28339 = CARTESIAN_POINT ( 'NONE',  ( -0.3996062992125987146, 0.1070741851644051862, -2.867454068241469756 ) ) ;
#28340 = CARTESIAN_POINT ( 'NONE',  ( 0.3917322834645670104, 0.1049643490035304660, -1.538733226542994048 ) ) ;
#28341 = CARTESIAN_POINT ( 'NONE',  ( 0.8202099737532814183, -0.6692913385826773087, -0.1292274648535924053 ) ) ;
#28342 = CARTESIAN_POINT ( 'NONE',  ( -0.01968503937007793844, -0.5400638737290844871, 0.3530559997133364547 ) ) ;
#28343 = CARTESIAN_POINT ( 'NONE',  ( -0.9383202099737524282, -0.3162353388693409650, -0.4822834645669289433 ) ) ;
#28344 = CARTESIAN_POINT ( 'NONE',  ( 1.555118110236221041, -0.5400638737290844871, 0.3530559997133364547 ) ) ;
#28345 = CARTESIAN_POINT ( 'NONE',  ( 0.8333333333333340365, -0.6692913385826771977, 0.1292274648535927661 ) ) ;
#28346 = CARTESIAN_POINT ( 'NONE',  ( -0.3917322834645669549, -0.1049643490035306603, -1.075459317585301777 ) ) ;
#28347 = CARTESIAN_POINT ( 'NONE',  ( -0.4790026246719154557, -0.3162353388693405765, 0.4822834645669290543 ) ) ;
#28348 = CARTESIAN_POINT ( 'NONE',  ( 0.7545931758530189937, 0.2952755905511810774, -0.1292274648535930714 ) ) ;
#28349 = CARTESIAN_POINT ( 'NONE',  ( -0.1115485564304453947, -0.6692913385826771977, 0.1292274648535927661 ) ) ;
#28350 = CARTESIAN_POINT ( 'NONE',  ( 0.5314960629921267055, -0.4536011799217367080, 0.2665933059059888421 ) ) ;
#28351 = CARTESIAN_POINT ( 'NONE',  ( -1.174540682414697335, -0.3162353388693409650, -0.4822834645669289433 ) ) ;
#28352 = DIRECTION ( 'NONE',  ( 0.8660254037844363761, 0.000000000000000000, 0.5000000000000038858 ) ) ;
#28353 = CARTESIAN_POINT ( 'NONE',  ( 0.5446194225721792126, -0.05778040916215560624, -0.4822834645669293319 ) ) ;
#28354 =( CONVERSION_BASED_UNIT ( 'INCH', #54433 ) LENGTH_UNIT ( ) NAMED_UNIT ( #81973 ) );
#28355 = CARTESIAN_POINT ( 'NONE',  ( 0.3917322834645670104, -0.1049643490035303411, -2.465879265091863282 ) ) ;
#28356 = ORIENTED_EDGE ( 'NONE', *, *, #76928, .F. ) ;
#28357 = ORIENTED_EDGE ( 'NONE', *, *, #66673, .T. ) ;
#28358 = CARTESIAN_POINT ( 'NONE',  ( 1.318897637795276356, -0.5400638737290844871, 0.3530559997133364547 ) ) ;
#28359 = CARTESIAN_POINT ( 'NONE',  ( 0.4921259842519691285, 0.07958543189024085140, 0.2665933059059887866 ) ) ;
#28360 = CARTESIAN_POINT ( 'NONE',  ( 0.5708661417322842269, 0.1660481256975885056, 0.3530559997133364547 ) ) ;
#28361 = DIRECTION ( 'NONE',  ( 0.000000000000000000, 0.000000000000000000, 1.000000000000000000 ) ) ;
#28362 = DIRECTION ( 'NONE',  ( 0.000000000000000000, 0.000000000000000000, -1.000000000000000000 ) ) ;
#28363 = CARTESIAN_POINT ( 'NONE',  ( -9.594673741351313045E-17, 0.3917322834645670104, -1.187007874015748143 ) ) ;
#28364 = CARTESIAN_POINT ( 'NONE',  ( -0.3460692066303960313, 0.1998031496062989965, -2.150262467191601079 ) ) ;
#28365 = CARTESIAN_POINT ( 'NONE',  ( -0.9711286089238838626, 0.2306618581243847221, -0.2411417322834647770 ) ) ;
#28366 = CARTESIAN_POINT ( 'NONE',  ( -0.8136482939632537770, -0.6046776061558807314, 0.2411417322834647770 ) ) ;
#28367 = CARTESIAN_POINT ( 'NONE',  ( 1.233595800524935227, -0.6046776061558807314, 0.2411417322834647770 ) ) ;
#28368 = VERTEX_POINT ( 'NONE', #25960 ) ;
#28369 = VECTOR ( 'NONE', #21737, 39.37007874015748143 ) ;
#28370 = CARTESIAN_POINT ( 'NONE',  ( -1.607611548556429737, -0.6692913385826771977, 0.1292274648535927661 ) ) ;
#28371 = CARTESIAN_POINT ( 'NONE',  ( -1.096639669977155007, 1.126360982307443415, 0.2389055636428836504 ) ) ;
#28372 = DIRECTION ( 'NONE',  ( 0.000000000000000000, 1.000000000000000000, 0.000000000000000000 ) ) ;
#28373 = CARTESIAN_POINT ( 'NONE',  ( 0.1998031496062992463, 0.3460692066303959202, -2.110892388451443669 ) ) ;
#28374 = CARTESIAN_POINT ( 'NONE',  ( -1.312335958005248715, 0.1283753931104748280, 0.1820866141732283561 ) ) ;
#28375 = DIRECTION ( 'NONE',  ( -0.000000000000000000, 1.000000000000000000, -0.000000000000000000 ) ) ;
#28376 = CARTESIAN_POINT ( 'NONE',  ( 0.2690288713910767848, 0.2952755905511811885, 0.1292274648535926551 ) ) ;
#28378 = DIRECTION ( 'NONE',  ( 0.000000000000000000, 0.000000000000000000, -1.000000000000000000 ) ) ;
#28377 = CARTESIAN_POINT ( 'NONE',  ( 1.391076115485564868, 0.2306618581243847221, -0.2411417322834647770 ) ) ;
#28379 = CARTESIAN_POINT ( 'NONE',  ( -0.6561679790026240244, -0.5023911411419708095, 0.1820866141732285504 ) ) ;
#28380 =( BOUNDED_CURVE ( )  B_SPLINE_CURVE ( 2, ( #49604, #75711, #30248, #43685, #4170, #10904, #18052, #36562, #82434, #11742, #81624, #75298, #50420 ),
 .UNSPECIFIED., .F., .F. ) 
 B_SPLINE_CURVE_WITH_KNOTS ( ( 3, 2, 2, 2, 2, 2, 3 ),
 ( 0.4006038219075281348, 0.4015151515151514916, 0.4053030303030302761, 0.4090909090909091161, 0.4128787878787879007, 0.4166666666666666852, 0.4175779962742901530 ),
 .UNSPECIFIED. ) 
 CURVE ( )  GEOMETRIC_REPRESENTATION_ITEM ( )  RATIONAL_B_SPLINE_CURVE ( ( 0.9875488213027530104, 0.9918020599134685922, 1.000000000000000000, 0.9659258262890683122, 1.000000000000000000, 0.9659258262890683122, 1.000000000000000000, 0.9659258262890683122, 1.000000000000000000, 0.9659258262890683122, 1.000000000000000000, 0.9918020599134675930, 0.9875488213027519002 ) ) 
 REPRESENTATION_ITEM ( '' )  );
#28381 = CARTESIAN_POINT ( 'NONE',  ( 0.9842519685039378130, -0.6692913385826771977, 8.415575281601705876E-17 ) ) ;
#28382 = CARTESIAN_POINT ( 'NONE',  ( 1.450131233595801428, 0.1771653543307087630, 0.09757992244046791164 ) ) ;
#28383 = CARTESIAN_POINT ( 'NONE',  ( 0.3917322834645668994, -0.1049643490035303134, -1.293943938811336958 ) ) ;
#28384 = CARTESIAN_POINT ( 'NONE',  ( -0.8661417322834640276, -0.1870078740157480601, -0.3641732283464567677 ) ) ;
#28385 = CARTESIAN_POINT ( 'NONE',  ( 1.181102362204725198, -0.1870078740157479769, 0.4822834645669291653 ) ) ;
#28386 = DIRECTION ( 'NONE',  ( 0.000000000000000000, -0.000000000000000000, -1.000000000000000000 ) ) ;
#28387 = CARTESIAN_POINT ( 'NONE',  ( 0.3346456692913390985, 0.1660481256975885056, 0.3530559997133364547 ) ) ;
#28388 = CARTESIAN_POINT ( 'NONE',  ( -1.102362204724408601, -0.1870078740157480601, -0.3641732283464567677 ) ) ;
#28389 = CARTESIAN_POINT ( 'NONE',  ( -0.3083989501312330295, -0.08942795157527998196, 0.3641732283464567121 ) ) ;
#28390 = AXIS2_PLACEMENT_3D ( 'NONE', #16080, #36246, #22790 ) ;
#28391 = CARTESIAN_POINT ( 'NONE',  ( -0.3871391076115479057, -0.3162353388693409650, -0.4822834645669289433 ) ) ;
#28392 = CARTESIAN_POINT ( 'NONE',  ( -1.417322834645668772, -0.1870078740157480601, -0.3641732283464567677 ) ) ;
#28393 = CARTESIAN_POINT ( 'NONE',  ( -0.3917322834645671770, 0.1049643490035302024, -0.5019878197188469837 ) ) ;
#28394 = CARTESIAN_POINT ( 'NONE',  ( 0.4855643044619428750, 0.05413385826771666132, 0.4176697321401328100 ) ) ;
#28395 = EDGE_CURVE ( 'NONE', #30126, #36535, #13538, .T. ) ;
#28396 = PLANE ( 'NONE',  #4095 ) ;
#28397 = CARTESIAN_POINT ( 'NONE',  ( 0.3458507752293908943, -0.3458507752293908943, -1.750000000000000222 ) ) ;
#28398 = CARTESIAN_POINT ( 'NONE',  ( -0.9973753280839886548, -0.6046776061558809534, -0.2411417322834644161 ) ) ;
#28399 = CARTESIAN_POINT ( 'NONE',  ( -0.06561679790026180015, -0.3690944881889765550, -0.3153832671262227771 ) ) ;
#28400 = CARTESIAN_POINT ( 'NONE',  ( -1.286089238845143479, 0.2306618581243847221, -0.2411417322834647770 ) ) ;
#28401 = CARTESIAN_POINT ( 'NONE',  ( -0.07874015748031421014, -0.1870078740157479769, 0.4822834645669291653 ) ) ;
#28402 = CARTESIAN_POINT ( 'NONE',  ( 0.5052493438320218022, -0.5511811023622048555, -0.09757992244046775898 ) ) ;
#28403 = CARTESIAN_POINT ( 'NONE',  ( -0.6627296587926503335, -0.5511811023622046335, 0.09757992244046803654 ) ) ;
#28404 = CARTESIAN_POINT ( 'NONE',  ( -1.200787401574802349, 0.1660481256975883668, -0.3530559997133364547 ) ) ;
#28405 = CARTESIAN_POINT ( 'NONE',  ( 1.607611548556431069, 0.1771653543307087630, 0.09757992244046791164 ) ) ;
#28406 = CARTESIAN_POINT ( 'NONE',  ( 1.194225721784777594, 0.05413385826771666132, 0.4176697321401328100 ) ) ;
#28407 = CYLINDRICAL_SURFACE ( 'NONE', #74386, 1.181102362204724310 ) ;
#28408 = CARTESIAN_POINT ( 'NONE',  ( 0.8398950131233602345, -0.5023911411419708095, 0.1820866141732285504 ) ) ;
#28409 = CARTESIAN_POINT ( 'NONE',  ( 0.7349081364829403995, 0.2306618581243848609, 0.2411417322834645549 ) ) ;
#28410 = CARTESIAN_POINT ( 'NONE',  ( -0.03443470937339727228, 1.062992125984252079, -1.438590695389362573 ) ) ;
#28411 = CARTESIAN_POINT ( 'NONE',  ( 1.417322834645670104, -0.1870078740157479769, 0.3641732283464567677 ) ) ;
#28412 = ORIENTED_EDGE ( 'NONE', *, *, #36496, .F. ) ;
#28413 = CARTESIAN_POINT ( 'NONE',  ( 0.1058382717557500852, -0.3949938075777408852, 0.1528871391076115638 ) ) ;
#28414 = CARTESIAN_POINT ( 'NONE',  ( -1.194225721784776262, -0.3690944881889763329, 0.3153832671262228327 ) ) ;
#28415 = CARTESIAN_POINT ( 'NONE',  ( -0.4986876640419939388, 0.2306618581243847221, -0.2411417322834647770 ) ) ;
#28416 = CARTESIAN_POINT ( 'NONE',  ( 0.1640419947506569498, -0.05778040916215522460, 0.4822834645669289988 ) ) ;
#28417 = CARTESIAN_POINT ( 'NONE',  ( -1.587926509186350810, -0.3690944881889763329, 0.3153832671262228327 ) ) ;
#28418 = CARTESIAN_POINT ( 'NONE',  ( 0.1070741851644054776, -0.3996062992125984925, -2.209317585301837639 ) ) ;
#28419 = CARTESIAN_POINT ( 'NONE',  ( -1.417322834645668772, -0.1870078740157479769, 0.4822834645669291653 ) ) ;
#28420 = CARTESIAN_POINT ( 'NONE',  ( 0.4527559055118117182, 0.1660481256975883668, -0.3530559997133364547 ) ) ;
#28421 = CARTESIAN_POINT ( 'NONE',  ( -0.1181102362204717315, -0.6692913385826771977, 8.415575281601705876E-17 ) ) ;
#28422 = CARTESIAN_POINT ( 'NONE',  ( 1.003937007874016185, 0.1660481256975883668, -0.3530559997133364547 ) ) ;
#28423 = CARTESIAN_POINT ( 'NONE',  ( 1.509186351706037543, 0.05413385826771666132, 0.4176697321401328100 ) ) ;
#28424 = CARTESIAN_POINT ( 'NONE',  ( 0.3996062992125986590, -0.1070741851644053111, -1.843832020997375309 ) ) ;
#28425 = CARTESIAN_POINT ( 'NONE',  ( 4.837279021331060870E-17, -0.3949938075777409963, -1.181102362204724532 ) ) ;
#28426 = CARTESIAN_POINT ( 'NONE',  ( -0.1070741851644056997, 0.3996062992125986035, -2.526246719160104792 ) ) ;
#28427 = CARTESIAN_POINT ( 'NONE',  ( -2.503252890251015828, 2.755905511811024056, 0.5314960629921260393 ) ) ;
#28428 = CARTESIAN_POINT ( 'NONE',  ( -0.3917322834645669549, -0.1049643490035306603, -0.3530183727034120755 ) ) ;
#28429 = CARTESIAN_POINT ( 'NONE',  ( -0.1509186351706028884, -0.08942795157527998196, 0.3641732283464567121 ) ) ;
#28430 = CIRCLE ( 'NONE', #75490, 0.2952755905511810774 ) ;
#28431 = CARTESIAN_POINT ( 'NONE',  ( -0.2624671916010490880, 0.2306618581243847221, -0.2411417322834647770 ) ) ;
#28432 = CARTESIAN_POINT ( 'NONE',  ( 0.7217847769028878924, -0.4281496062992127816, -0.4176697321401328100 ) ) ;
#28433 = CARTESIAN_POINT ( 'NONE',  ( 0.1974969037888706092, -0.3420746716998660508, -2.215879265091863726 ) ) ;
#28434 = CARTESIAN_POINT ( 'NONE',  ( -0.2427821522309703550, -0.2845877964562159024, 0.3641732283464567677 ) ) ;
#28435 = CARTESIAN_POINT ( 'NONE',  ( -0.9580052493438311334, 0.05413385826771626580, -0.4176697321401330321 ) ) ;
#28436 = CARTESIAN_POINT ( 'NONE',  ( 1.463254593175853824, 0.2952755905511810774, -0.1292274648535930714 ) ) ;
#28437 = CARTESIAN_POINT ( 'NONE',  ( -0.3458507752293909498, 0.3458507752293907833, -1.909448818897637512 ) ) ;
#28438 = CARTESIAN_POINT ( 'NONE',  ( 1.115485564304462551, 0.05413385826771666132, 0.4176697321401328100 ) ) ;
#28439 = VERTEX_POINT ( 'NONE', #52461 ) ;
#28440 = ORIENTED_EDGE ( 'NONE', *, *, #23397, .F. ) ;
#28441 = CARTESIAN_POINT ( 'NONE',  ( 0.9580052493438326877, 0.05413385826771666132, 0.4176697321401328100 ) ) ;
#28442 = CARTESIAN_POINT ( 'NONE',  ( -1.646981627296586703, -0.3162353388693409650, -0.4822834645669289433 ) ) ;
#28444 = CARTESIAN_POINT ( 'NONE',  ( -1.030183727034119867, -0.3162353388693405765, 0.4822834645669290543 ) ) ;
#28443 = CARTESIAN_POINT ( 'NONE',  ( -1.397637795275589623, -0.4536011799217368745, -0.2665933059059886201 ) ) ;
#28445 = CARTESIAN_POINT ( 'NONE',  ( 0.1958661417322834497, 0.3392501089628018329, -2.271634227525247685 ) ) ;
#28446 = CARTESIAN_POINT ( 'NONE',  ( 1.191111281560510715, -4.927456884911482678E-16, 0.4445507791589062840 ) ) ;
#28447 = CARTESIAN_POINT ( 'NONE',  ( 1.082677165354331228, 0.1660481256975883668, -0.3530559997133364547 ) ) ;
#28448 = CARTESIAN_POINT ( 'NONE',  ( 5.785732909357575061E-17, -0.4724409448818898682, -2.440944881889763884 ) ) ;
#28449 = CARTESIAN_POINT ( 'NONE',  ( -0.1574803149606292529, -0.1870078740157479769, 0.4822834645669291653 ) ) ;
#28450 = CARTESIAN_POINT ( 'NONE',  ( -0.06561679790026180015, -0.4281496062992127816, -0.4176697321401328100 ) ) ;
#28451 = CARTESIAN_POINT ( 'NONE',  ( -1.397637795275589623, -0.5400638737290845981, -0.3530559997133363437 ) ) ;
#28452 = CARTESIAN_POINT ( 'NONE',  ( -0.1958661417322836718, 0.3392501089628017219, 0.2171916010498686767 ) ) ;
#28453 = CARTESIAN_POINT ( 'NONE',  ( 0.09186351706036799403, -0.4281496062992127816, -0.4176697321401328100 ) ) ;
#28454 = CARTESIAN_POINT ( 'NONE',  ( 0.3392501089628018329, 0.1958661417322835607, -1.855643044619422533 ) ) ;
#28455 = CARTESIAN_POINT ( 'NONE',  ( -1.102362204724408601, -0.1870078740157480601, -0.3641732283464567677 ) ) ;
#28456 = ORIENTED_EDGE ( 'NONE', *, *, #56394, .T. ) ;
#28457 = CARTESIAN_POINT ( 'NONE',  ( 0.3420746716998659953, 0.1974969037888705536, -2.493438320209973469 ) ) ;
#28458 = ORIENTED_EDGE ( 'NONE', *, *, #11019, .F. ) ;
#28459 = CARTESIAN_POINT ( 'NONE',  ( -2.118110236220467790, 0.000000000000000000, -0.4498537592783120598 ) ) ;
#28460 = CARTESIAN_POINT ( 'NONE',  ( -1.397637795275589623, 0.1660481256975885056, 0.3530559997133364547 ) ) ;
#28461 = CARTESIAN_POINT ( 'NONE',  ( 0.3996062992125986035, 2.446882876249141962E-17, -0.9055118110236221041 ) ) ;
#28462 = CARTESIAN_POINT ( 'NONE',  ( -1.509186351706035767, 0.05413385826771626580, -0.4176697321401330321 ) ) ;
#28463 = CARTESIAN_POINT ( 'NONE',  ( -1.679790026246718693, 0.2306618581243847221, -0.2411417322834647770 ) ) ;
#28464 = CARTESIAN_POINT ( 'NONE',  ( 0.4199475065616805614, 0.2306618581243848609, 0.2411417322834645549 ) ) ;
#28465 = CARTESIAN_POINT ( 'NONE',  ( -0.3821149210511725069, 0.02791078216816064370, 0.4328096321851915285 ) ) ;
#28466 = CARTESIAN_POINT ( 'NONE',  ( 4.797336870675656522E-17, -0.3917322834645670104, -0.005905511811023714773 ) ) ;
#28467 = CARTESIAN_POINT ( 'NONE',  ( -0.3871391076115476282, -0.08942795157527998196, 0.3641732283464567121 ) ) ;
#28468 = CARTESIAN_POINT ( 'NONE',  ( -0.6233595800524928121, -0.08942795157527998196, 0.3641732283464567121 ) ) ;
#28469 = CARTESIAN_POINT ( 'NONE',  ( -1.417322834645668772, -0.1870078740157480879, -0.4822834645669291653 ) ) ;
#28470 = CARTESIAN_POINT ( 'NONE',  ( 0.9448818897637802916, -0.1870078740157479769, 0.4822834645669291653 ) ) ;
#28471 = CARTESIAN_POINT ( 'NONE',  ( -1.049868766404198794, -0.6046776061558807314, 0.2411417322834647770 ) ) ;
#28472 = CARTESIAN_POINT ( 'NONE',  ( 0.5314960629921393620, 2.755400581649068315, -3.831845081856512181 ) ) ;
#28473 = ORIENTED_EDGE ( 'NONE', *, *, #7888, .F. ) ;
#28474 = ADVANCED_FACE ( 'NONE', ( #65117 ), #41410, .F. ) ;
#28475 = CARTESIAN_POINT ( 'NONE',  ( -1.482939632545930975, 0.05413385826771666132, 0.4176697321401328100 ) ) ;
#28476 = CARTESIAN_POINT ( 'NONE',  ( 2.795275590551181466, 2.793565526369266916, 0.000000000000000000 ) ) ;
#28477 =( CONVERSION_BASED_UNIT ( 'INCH', #10382 ) LENGTH_UNIT ( ) NAMED_UNIT ( #56680 ) );
#28478 = CARTESIAN_POINT ( 'NONE',  ( 0.3458507752293908943, 0.3458507752293908943, -1.397637795275590067 ) ) ;
#28479 = DIRECTION ( 'NONE',  ( 3.096699300667737957E-16, -1.000000000000000000, 0.000000000000000000 ) ) ;
#28480 = EDGE_CURVE ( 'NONE', #36616, #11962, #31154, .T. ) ;
#28481 = CARTESIAN_POINT ( 'NONE',  ( 0.2867679344610365999, 0.2867679344610365999, -0.7598425196850391306 ) ) ;
#28482 = CARTESIAN_POINT ( 'NONE',  ( 0.3917322834645670104, 2.398668435337828261E-17, -2.564960629921259727 ) ) ;
#28483 = CARTESIAN_POINT ( 'NONE',  ( -0.5643044619422565855, -0.4281496062992124485, 0.4176697321401328655 ) ) ;
#28484 = CARTESIAN_POINT ( 'NONE',  ( 1.410761154855643795, -0.05778040916215560624, -0.4822834645669293319 ) ) ;
#28485 = CARTESIAN_POINT ( 'NONE',  ( 0.3460692066303958092, 0.1998031496062993018, -0.2080052493438320771 ) ) ;
#28487 = CARTESIAN_POINT ( 'NONE',  ( 0.1938976377952756069, 0.1938976377952756069, 0.09542247959850377881 ) ) ;
#28486 = CARTESIAN_POINT ( 'NONE',  ( -1.725721784776902190, -0.05778040916215522460, 0.4822834645669289988 ) ) ;
#28488 = CARTESIAN_POINT ( 'NONE',  ( -1.213910761154854745, 0.2952755905511810774, -0.1292274648535930714 ) ) ;
#28489 = CARTESIAN_POINT ( 'NONE',  ( -0.7545931758530177724, 0.2952755905511811885, 0.1292274648535926551 ) ) ;
#28490 = CARTESIAN_POINT ( 'NONE',  ( -0.3917322834645670659, 0.1049643490035301607, -0.1128415766066123566 ) ) ;
#28491 = CARTESIAN_POINT ( 'NONE',  ( 0.4527559055118117182, -0.4536011799217367080, 0.2665933059059888421 ) ) ;
#28492 = CARTESIAN_POINT ( 'NONE',  ( 0.3392501089628018884, -0.1958661417322834220, -0.3471128608923885195 ) ) ;
#28493 = CARTESIAN_POINT ( 'NONE',  ( 0.1837270341207357105, -0.5023911411419708095, -0.1820866141732282451 ) ) ;
#28494 = CARTESIAN_POINT ( 'NONE',  ( 1.122047244094488860, 0.07958543189024085140, 0.2665933059059887866 ) ) ;
#28495 = CARTESIAN_POINT ( 'NONE',  ( 0.8858267716535438430, -0.5400638737290845981, -0.3530559997133363437 ) ) ;
#28497 = AXIS2_PLACEMENT_3D ( 'NONE', #56833, #24034, #5099 ) ;
#28496 = UNCERTAINTY_MEASURE_WITH_UNIT (LENGTH_MEASURE( 1.000000000000000082E-05 ), #81468, 'distance_accuracy_value', 'NONE');
#28498 = CARTESIAN_POINT ( 'NONE',  ( -0.4986876640419939388, 0.1283753931104746893, -0.1820866141732285504 ) ) ;
#28499 = CARTESIAN_POINT ( 'NONE',  ( -0.2867679344610364334, -0.2867679344610367109, -1.940944881889763884 ) ) ;
#28500 = CARTESIAN_POINT ( 'NONE',  ( -1.318897637795274802, 0.1660481256975885056, 0.3530559997133364547 ) ) ;
#28501 = EDGE_CURVE ( 'NONE', #74653, #25219, #41811, .T. ) ;
#28502 = CARTESIAN_POINT ( 'NONE',  ( -1.312335958005248715, 0.1283753931104748280, 0.1820866141732283561 ) ) ;
#28503 = CARTESIAN_POINT ( 'NONE',  ( -1.157146581871515012E-16, 0.4724409448818898682, -0.5492125984251968740 ) ) ;
#28504 = CARTESIAN_POINT ( 'NONE',  ( -0.7611548556430438595, -0.5023911411419708095, -0.1820866141732282451 ) ) ;
#28505 = EDGE_CURVE ( 'NONE', #63201, #53272, #68215, .T. ) ;
#28506 = CARTESIAN_POINT ( 'NONE',  ( -0.1181102362204717315, -0.6692913385826771977, 8.415575281601705876E-17 ) ) ;
#28507 = CARTESIAN_POINT ( 'NONE',  ( 1.607611548556431069, -0.5511811023622048555, -0.09757992244046775898 ) ) ;
#28508 = CARTESIAN_POINT ( 'NONE',  ( 0.7086614173228352742, -0.1870078740157480601, -0.3641732283464567677 ) ) ;
#28509 = CARTESIAN_POINT ( 'NONE',  ( -0.05905511811023545637, -0.4536011799217368745, -0.2665933059059886201 ) ) ;
#28510 = CARTESIAN_POINT ( 'NONE',  ( -0.7152230971128602510, -0.3162353388693405765, 0.4822834645669290543 ) ) ;
#28511 = CARTESIAN_POINT ( 'NONE',  ( -1.587926509186350810, -0.4281496062992124485, 0.4176697321401328655 ) ) ;
#28512 = LINE ( 'NONE', #73563, #40783 ) ;
#28513 = CARTESIAN_POINT ( 'NONE',  ( 0.07217847769028949700, -0.3162353388693405765, 0.4822834645669290543 ) ) ;
#28514 = ORIENTED_EDGE ( 'NONE', *, *, #10113, .F. ) ;
#28515 = CARTESIAN_POINT ( 'NONE',  ( -0.1070741851644051862, -0.3996062992125986590, -1.723753280839894986 ) ) ;
#28516 =( BOUNDED_SURFACE ( )  B_SPLINE_SURFACE ( 1, 2, ( 
 ( #75602, #62546, #43577, #9966, #4883, #30557, #81094, #43165, #24232, #16707, #17941, #55799, #56223, #81921, #42348, #4059, #23411, #49904, #49077, #69279, #24644, #76009, #18351, #74778, #17129, #35637, #61298, #3656, #29319, #54980, #23828, #42761, #49496, #75189, #10795, #36455, #23001, #62129, #30137, #17533, #13276, #31368, #7364, #57033, #39343, #25876, #38928, #6532, #26721, #69688, #33034, #58702, #52375, #83140, #82728, #77241, #50722, #51959, #1068, #643, #76420, #77665, #32202, #32616, #64608, #18749, #12438, #31785, #58278, #44393, #19571, #26300, #65029, #19996, #70085, #57448, #6945, #45647, #78083, #12031, #71342, #226, #38098, #57859, #51538, #19153, #44804, #13689, #20415, #37688, #63363, #5697, #25047, #63772, #6113, #25460, #45230, #51127, #70931, #76821, #70499, #12857, #38515, #64198, #59535, #33460, #53627, #27133, #28381, #9445, #15779, #80175, #40187, #59953, #27969, #54461, #46483, #21244, #1892, #2308, #35116, #79754, #46067, #7794, #65461, #1479, #53211, #47731, #20830, #40599, #3134, #8206, #66281, #27552, #46899, #47315, #8621, #34292, #21655, #39766, #15357, #2720, #67114, #78922, #41431, #72593, #78507, #71760, #72178, #79335, #65871, #59122, #52797, #14940, #73005, #14113, #60782, #14536, #41018, #66704, #33871, #9037, #28798, #34711, #60372, #54041, #22071, #73429, #11106, #30034, #43476, #35532, #81821, #80588, #80995, #11523, #3550, #29625, #30451, #4775, #49393, #56115, #56525, #23722, #75087, #42247, #55697, #75502, #55285, #22895, #22490, #3962, #24131, #67942, #29216, #17434, #17841, #62438, #81405, #4366, #35950, #48563, #17023, #61620, #43065, #68762, #36354, #10284, #23308, #9862, #37180, #48978, #49800, #69172, #36762, #61194, #48153, #62859, #62030, #74677, #5195, #30860, #73848, #16188, #41835, #42662, #74261, #67525, #54883, #16603, #68360, #10699, #11933, #56935, #12759, #38417, #25781, #75909, #82631, #18653, #69587, #64098, #19059, #37588, #19478, #6434, #63261, #44297, #32105, #57764, #50211, #63675, #18248, #6016, #31269, #126, #50618, #5602, #43890, #31687, #25365, #24945, #76323, #69988, #51442, #77145, #12343, #37999, #45130, #57346, #82227, #24547, #83042, #51028, #76727, #44707, #70403, #49132, #10024, #82381, #81563, #10447, #61355, #3709, #23465, #29780, #24698, #63014, #50367, #49547, #68508, #80740, #10848, #31011, #4115, #68916, #61774, #23882, #5352, #4943, #75242, #37341, #29372, #75656, #74419, #74837, #56679, #23054, #17181, #24287, #81972, #43218, #49959, #16351, #17586, #69334, #17996, #48722, #55442, #11266, #43630, #11684, #41995, #67689, #30191, #16764, #62185, #55854, #42814, #36509, #35690, #55033, #42403, #36924, #62601, #68101, #36103, #81150, #4522, #30612, #56276, #12915, #33099, #76064, #39408, #65091, #58765, #6168, #63419, #283, #57088, #58340, #7429, #45707, #26778, #70142, #6587, #57919, #1128, #76478, #51183, #31843, #32258, #18407, #26359, #44050, #37744, #12087, #31426, #83196, #77725, #50778, #70559, #69742, #38157, #38572, #57505, #76881, #77299, #64253, #25938, #51597, #5756, #45291, #32674, #13751, #25518, #71403, #19212, #44860, #82784, #25105, #19630, #12494, #18805, #44450, #70987, #13331, #63830, #38984, #64667, #7006, #702, #52019, #20054, #67180, #40246, #21714, #14593, #60017, #15845, #41079, #2372, #73497, #65521, #28444, #27193, #27613, #41494, #33518, #59596, #60433, #34774, #79395, #2784, #3195, #53687, #47378, #72244, #28029, #66768, #59181, #54103, #15001, #15418, #73069, #1538, #78567, #65929, #9101, #52857, #79819, #22135, #47793, #9509, #35182, #60843, #52434, #14174, #78144, #39832, #20476, #8681, #46130, #72651, #71824, #7852, #20893, #46546, #8266, #33931, #1951, #53276, #78986, #21306, #46959, #40658, #66343, #34351, #42720, #10756, #37245, #29276, #4021, #68004, #68416, #17901, #62502, #62921, #73910, #48214, #67591, #36010, #30515, #3610, #23370, #69237, #74320, #49038, #10349, #29685, #30097, #74735, #17083, #4431, #22552, #81466, #68823, #49861, #61680, #81880, #55348, #81054, #16250, #11585, #36416, #22959, #41897, #9922, #62089, #42306 ),
 ( #56177, #55760, #24192, #23784, #49455, #4840, #35593, #75149, #75561, #54940, #17494, #43125, #61256, #11168, #43538, #36829, #80646, #28859, #54521, #80236, #48625, #16667, #1351, #1760, #46352, #39635, #71626, #19864, #64470, #935, #45512, #65326, #13978, #20278, #51824, #64891, #77104, #21115, #71209, #72048, #33742, #7663, #45087, #40474, #40059, #27001, #57723, #53078, #30918, #5254, #27417, #26593, #52664, #70791, #59402, #52245, #78790, #45928, #33334, #46775, #32478, #86, #72466, #13552, #8079, #58995, #78370, #65746, #13142, #77949, #14815, #6807, #39208, #20702, #38794, #14404, #25739, #7230, #58140, #51400, #32902, #19436, #26162, #509, #77528, #58570, #22765, #16057, #48018, #79625, #40885, #60653, #21942, #41703, #73718, #80039, #28251, #41301, #53502, #80861, #47602, #48427, #10151, #67396, #21526, #16889, #16472, #22359, #73296, #9730, #35817, #35401, #61066, #61482, #3003, #66567, #42117, #3417, #29080, #8901, #8489, #72877, #53911, #74126, #67814, #29491, #27840, #15645, #66987, #47185, #3831, #54750, #15225, #48842, #55150, #34577, #9319, #23173, #74543, #59819, #54330, #2174, #80456, #60245, #66152, #34989, #2592, #28669, #34158, #79210, #42930, #62301, #17303, #31547, #12206, #29896, #4638, #82905, #17705, #69855, #5871, #68625, #43745, #10965, #4232, #5060, #61891, #50891, #36624, #56392, #55559, #75357, #42528, #81688, #43333, #69451, #62723, #37041, #18112, #36222, #11801, #82496, #63540, #23999, #37864, #69033, #11384, #81268, #25226, #24405, #30309, #23583, #49255, #49667, #55976, #76591, #57204, #68230, #75770, #30730, #74957, #82091, #10564, #50075, #37455, #63129, #5467, #31129, #56796, #24812, #50479, #76183, #18520, #44163, #77423, #7975, #62468, #26061, #26899, #1250, #45826, #52558, #52974, #20176, #71525, #38692, #52140, #33228, #25638, #78267, #64788, #65218, #13871, #51301, #44987, #64370, #7557, #77004, #77847, #58891, #71946, #20598, #19335, #6707, #39530, #46250, #14298, #44570, #39959, #32798, #70685, #7126, #58467, #51720, #19757, #65645, #33638, #59301, #1658, #27315, #63952, #18920, #6289, #70261, #830, #12616, #39106, #38274, #31964, #57625, #13039, #32376, #58040, #404, #26489, #45411, #71107, #13450, #48323, #29389, #72771, #9216, #60550, #3725, #79107, #53805, #34473, #34889, #67706, #28974, #78688, #40368, #14713, #34051, #2490, #80351, #53400, #73188, #35706, #40776, #15538, #21426, #66048, #41198, #8386, #21011, #47080, #2901, #59714, #28149, #46671, #15957, #72365, #42012, #2069, #27735, #74020, #66886, #41603, #15122, #16366, #28565, #10042, #54221, #79937, #61375, #66461, #8797, #22664, #79518, #60139, #22252, #67293, #54641, #21833, #47910, #47496, #73615, #9626, #35297, #60959, #3309, #24715, #4538, #29796, #55049, #36525, #37358, #74856, #61791, #49975, #50383, #11704, #4961, #36941, #68524, #55457, #49566, #10865, #30629, #62619, #68933, #17198, #30208, #42420, #69758, #62201, #63031, #82397, #56294, #10465, #5773, #5369, #11282, #55870, #81991, #76081, #24305, #75673, #18425, #75260, #81166, #31030, #18013, #43647, #23482, #80756, #4131, #42831, #56698, #44066, #12104, #16782, #81583, #23900, #36118, #37762, #69350, #49149, #63437, #23070, #17604, #43236, #48738, #74435, #68120, #19649, #50794, #45310, #83214, #39427, #12932, #6186, #70160, #71005, #7024, #31864, #51201, #57523, #20495, #1147, #18822, #76899, #71844, #6604, #58789, #78164, #25536, #32692, #44879, #71423, #26797, #58359, #12513, #65542, #65111, #13348, #38592, #39002, #52454, #64685, #721, #46149, #51614, #19229, #7449, #26379, #52039, #70578, #57105, #38174, #64270, #13770, #33119, #14194, #76495, #32276, #57936, #63848, #39851, #77743, #300, #31442, #82800, #25956, #77319, #25124, #44469, #20074, #45726, #27213, #79416, #59615, #15865, #72673, #65949, #46565, #21735, #66788, #8285, #27633, #33951, #80256, #60862, #78586, #53295, #48233, #66363, #35201, #54541, #1970, #9123, #79007, #52876, #53707, #20912, #16271, #21326, #47398, #72264, #40678, #7873, #28463, #59200, #22573, #33537, #41916, #3216, #2393, #54124, #14612 ) ),
 .UNSPECIFIED., .F., .F., .F. ) 
 B_SPLINE_SURFACE_WITH_KNOTS ( ( 2, 2 ),
 ( 3, 2, 2, 2, 2, 2, 2, 2, 2, 2, 2, 2, 2, 2, 2, 2, 2, 2, 2, 2, 2, 2, 2, 2, 2, 2, 2, 2, 2, 2, 2, 2, 2, 2, 2, 2, 2, 2, 2, 2, 2, 2, 2, 2, 2, 2, 2, 2, 2, 2, 2, 2, 2, 2, 2, 2, 2, 2, 2, 2, 2, 2, 2, 2, 2, 2, 2, 2, 2, 2, 2, 2, 2, 2, 2, 2, 2, 2, 2, 2, 2, 2, 2, 2, 2, 2, 2, 2, 2, 2, 2, 2, 2, 2, 2, 2, 2, 2, 2, 2, 2, 2, 2, 2, 2, 2, 2, 2, 2, 2, 2, 2, 2, 2, 2, 2, 2, 2, 2, 2, 2, 2, 2, 2, 2, 2, 2, 2, 2, 2, 2, 2, 2, 2, 2, 2, 2, 2, 2, 2, 2, 2, 2, 2, 2, 2, 2, 2, 2, 2, 2, 2, 2, 2, 2, 2, 2, 2, 2, 2, 2, 2, 2, 2, 2, 2, 2, 2, 2, 2, 2, 2, 2, 2, 2, 2, 2, 2, 2, 2, 2, 2, 2, 2, 2, 2, 2, 2, 2, 2, 2, 2, 2, 2, 2, 2, 2, 2, 2, 2, 2, 2, 2, 2, 2, 2, 2, 2, 2, 2, 2, 2, 2, 2, 2, 2, 2, 2, 2, 2, 2, 2, 2, 2, 2, 2, 2, 2, 2, 2, 2, 2, 2, 2, 2, 2, 2, 2, 2, 2, 2, 2, 2, 2, 2, 2, 2, 2, 2, 2, 2, 2, 2, 2, 2, 3 ),
 ( 0.000000000000000000, 1.000000000000000000 ),
 ( 0.000000000000000000, 0.003787878787878787984, 0.007575757575757575968, 0.01136363636363636395, 0.01515151515151515194, 0.01893939393939393992, 0.02272727272727272790, 0.02651515151515151589, 0.03030303030303030387, 0.03409090909090908839, 0.03787878787878787984, 0.04166666666666666435, 0.04545454545454545581, 0.04924242424242424032, 0.05303030303030303177, 0.05681818181818181629, 0.06060606060606060774, 0.06439393939393939226, 0.06818181818181817677, 0.07196969696969697516, 0.07575757575757575968, 0.07954545454545454419, 0.08333333333333332871, 0.08712121212121212710, 0.09090909090909091161, 0.09469696969696969613, 0.09848484848484848064, 0.1022727272727272790, 0.1060606060606060635, 0.1098484848484848481, 0.1136363636363636326, 0.1174242424242424310, 0.1212121212121212155, 0.1250000000000000000, 0.1287878787878787845, 0.1325757575757575690, 0.1363636363636363535, 0.1401515151515151381, 0.1439393939393939503, 0.1477272727272727348, 0.1515151515151515194, 0.1553030303030303039, 0.1590909090909090884, 0.1628787878787878729, 0.1666666666666666574, 0.1704545454545454419, 0.1742424242424242542, 0.1780303030303030387, 0.1818181818181818232, 0.1856060606060606077, 0.1893939393939393923, 0.1931818181818181768, 0.1969696969696969613, 0.2007575757575757458, 0.2045454545454545581, 0.2083333333333333426, 0.2121212121212121271, 0.2159090909090909116, 0.2196969696969696961, 0.2234848484848484806, 0.2272727272727272652, 0.2310606060606060497, 0.2348484848484848619, 0.2386363636363636465, 0.2424242424242424310, 0.2462121212121212155, 0.2500000000000000000, 0.2537878787878787845, 0.2575757575757575690, 0.2613636363636363535, 0.2651515151515151381, 0.2689393939393939226, 0.2727272727272727071, 0.2765151515151514916, 0.2803030303030302761, 0.2840909090909091161, 0.2878787878787879007, 0.2916666666666666852, 0.2954545454545454697, 0.2992424242424242542, 0.3030303030303030387, 0.3068181818181818232, 0.3106060606060606077, 0.3143939393939393923, 0.3181818181818181768, 0.3219696969696969613, 0.3257575757575757458, 0.3295454545454545303, 0.3333333333333333148, 0.3371212121212120993, 0.3409090909090908839, 0.3446969696969697239, 0.3484848484848485084, 0.3522727272727272929, 0.3560606060606060774, 0.3598484848484848619, 0.3636363636363636465, 0.3674242424242424310, 0.3712121212121212155, 0.3750000000000000000, 0.3787878787878787845, 0.3825757575757575690, 0.3863636363636363535, 0.3901515151515151381, 0.3939393939393939226, 0.3977272727272727071, 0.4015151515151514916, 0.4053030303030302761, 0.4090909090909091161, 0.4128787878787879007, 0.4166666666666666852, 0.4204545454545454697, 0.4242424242424242542, 0.4280303030303030387, 0.4318181818181818232, 0.4356060606060606077, 0.4393939393939393923, 0.4431818181818181768, 0.4469696969696969613, 0.4507575757575757458, 0.4545454545454545303, 0.4583333333333333148, 0.4621212121212120993, 0.4659090909090908839, 0.4696969696969697239, 0.4734848484848485084, 0.4772727272727272929, 0.4810606060606060774, 0.4848484848484848619, 0.4886363636363636465, 0.4924242424242424310, 0.4962121212121212155, 0.5000000000000000000, 0.5037878787878787845, 0.5075757575757575690, 0.5113636363636363535, 0.5151515151515151381, 0.5189393939393939226, 0.5227272727272727071, 0.5265151515151514916, 0.5303030303030302761, 0.5340909090909090606, 0.5378787878787878451, 0.5416666666666666297, 0.5454545454545454142, 0.5492424242424241987, 0.5530303030303029832, 0.5568181818181817677, 0.5606060606060605522, 0.5643939393939394478, 0.5681818181818182323, 0.5719696969696970168, 0.5757575757575758013, 0.5795454545454545858, 0.5833333333333333703, 0.5871212121212121549, 0.5909090909090909394, 0.5946969696969697239, 0.5984848484848485084, 0.6022727272727272929, 0.6060606060606060774, 0.6098484848484848619, 0.6136363636363636465, 0.6174242424242424310, 0.6212121212121212155, 0.6250000000000000000, 0.6287878787878787845, 0.6325757575757575690, 0.6363636363636363535, 0.6401515151515151381, 0.6439393939393939226, 0.6477272727272727071, 0.6515151515151514916, 0.6553030303030302761, 0.6590909090909090606, 0.6628787878787878451, 0.6666666666666666297, 0.6704545454545454142, 0.6742424242424241987, 0.6780303030303029832, 0.6818181818181817677, 0.6856060606060605522, 0.6893939393939394478, 0.6931818181818182323, 0.6969696969696970168, 0.7007575757575758013, 0.7045454545454545858, 0.7083333333333333703, 0.7121212121212121549, 0.7159090909090909394, 0.7196969696969697239, 0.7234848484848485084, 0.7272727272727272929, 0.7310606060606060774, 0.7348484848484848619, 0.7386363636363636465, 0.7424242424242424310, 0.7462121212121212155, 0.7500000000000000000, 0.7537878787878787845, 0.7575757575757575690, 0.7613636363636363535, 0.7651515151515151381, 0.7689393939393939226, 0.7727272727272727071, 0.7765151515151514916, 0.7803030303030302761, 0.7840909090909090606, 0.7878787878787878451, 0.7916666666666666297, 0.7954545454545454142, 0.7992424242424241987, 0.8030303030303029832, 0.8068181818181817677, 0.8106060606060605522, 0.8143939393939394478, 0.8181818181818182323, 0.8219696969696970168, 0.8257575757575758013, 0.8295454545454545858, 0.8333333333333333703, 0.8371212121212121549, 0.8409090909090909394, 0.8446969696969697239, 0.8484848484848485084, 0.8522727272727272929, 0.8560606060606060774, 0.8598484848484848619, 0.8636363636363636465, 0.8674242424242424310, 0.8712121212121212155, 0.8750000000000000000, 0.8787878787878787845, 0.8825757575757575690, 0.8863636363636363535, 0.8901515151515151381, 0.8939393939393939226, 0.8977272727272727071, 0.9015151515151514916, 0.9053030303030302761, 0.9090909090909090606, 0.9128787878787878451, 0.9166666666666666297, 0.9204545454545454142, 0.9242424242424241987, 0.9280303030303029832, 0.9318181818181817677, 0.9356060606060605522, 0.9393939393939394478, 0.9431818181818182323, 0.9469696969696970168, 0.9507575757575758013, 0.9545454545454545858, 0.9583333333333333703, 0.9621212121212121549, 0.9659090909090909394 ),
 .UNSPECIFIED. ) 
 GEOMETRIC_REPRESENTATION_ITEM ( )  RATIONAL_B_SPLINE_SURFACE ( (
 ( 1.000000000000000000, 0.9659258262890683122, 1.000000000000000000, 0.9659258262890683122, 1.000000000000000000, 0.9659258262890683122, 1.000000000000000000, 0.9659258262890683122, 1.000000000000000000, 0.9659258262890683122, 1.000000000000000000, 0.9659258262890683122, 1.000000000000000000, 0.9659258262890683122, 1.000000000000000000, 0.9659258262890683122, 1.000000000000000000, 0.9659258262890683122, 1.000000000000000000, 0.9659258262890683122, 1.000000000000000000, 0.9659258262890683122, 1.000000000000000000, 0.9659258262890683122, 1.000000000000000000, 0.9659258262890683122, 1.000000000000000000, 0.9659258262890683122, 1.000000000000000000, 0.9659258262890683122, 1.000000000000000000, 0.9659258262890683122, 1.000000000000000000, 0.9659258262890683122, 1.000000000000000000, 0.9659258262890683122, 1.000000000000000000, 0.9659258262890683122, 1.000000000000000000, 0.9659258262890683122, 1.000000000000000000, 0.9659258262890683122, 1.000000000000000000, 0.9659258262890683122, 1.000000000000000000, 0.9659258262890683122, 1.000000000000000000, 0.9659258262890683122, 1.000000000000000000, 0.9659258262890683122, 1.000000000000000000, 0.9659258262890683122, 1.000000000000000000, 0.9659258262890683122, 1.000000000000000000, 0.9659258262890683122, 1.000000000000000000, 0.9659258262890683122, 1.000000000000000000, 0.9659258262890683122, 1.000000000000000000, 0.9659258262890683122, 1.000000000000000000, 0.9659258262890683122, 1.000000000000000000, 0.9659258262890683122, 1.000000000000000000, 0.9659258262890683122, 1.000000000000000000, 0.9659258262890683122, 1.000000000000000000, 0.9659258262890683122, 1.000000000000000000, 0.9659258262890683122, 1.000000000000000000, 0.9659258262890683122, 1.000000000000000000, 0.9659258262890683122, 1.000000000000000000, 0.9659258262890683122, 1.000000000000000000, 0.9659258262890683122, 1.000000000000000000, 0.9659258262890683122, 1.000000000000000000, 0.9659258262890683122, 1.000000000000000000, 0.9659258262890683122, 1.000000000000000000, 0.9659258262890683122, 1.000000000000000000, 0.9659258262890683122, 1.000000000000000000, 0.9659258262890683122, 1.000000000000000000, 0.9659258262890683122, 1.000000000000000000, 0.9659258262890683122, 1.000000000000000000, 0.9659258262890683122, 1.000000000000000000, 0.9659258262890683122, 1.000000000000000000, 0.9659258262890683122, 1.000000000000000000, 0.9659258262890683122, 1.000000000000000000, 0.9659258262890683122, 1.000000000000000000, 0.9659258262890683122, 1.000000000000000000, 0.9659258262890683122, 1.000000000000000000, 0.9659258262890683122, 1.000000000000000000, 0.9659258262890683122, 1.000000000000000000, 0.9659258262890683122, 1.000000000000000000, 0.9659258262890683122, 1.000000000000000000, 0.9659258262890683122, 1.000000000000000000, 0.9659258262890683122, 1.000000000000000000, 0.9659258262890683122, 1.000000000000000000, 0.9659258262890683122, 1.000000000000000000, 0.9659258262890683122, 1.000000000000000000, 0.9659258262890683122, 1.000000000000000000, 0.9659258262890683122, 1.000000000000000000, 0.9659258262890683122, 1.000000000000000000, 0.9659258262890683122, 1.000000000000000000, 0.9659258262890683122, 1.000000000000000000, 0.9659258262890683122, 1.000000000000000000, 0.9659258262890683122, 1.000000000000000000, 0.9659258262890683122, 1.000000000000000000, 0.9659258262890683122, 1.000000000000000000, 0.9659258262890683122, 1.000000000000000000, 0.9659258262890683122, 1.000000000000000000, 0.9659258262890683122, 1.000000000000000000, 0.9659258262890683122, 1.000000000000000000, 0.9659258262890683122, 1.000000000000000000, 0.9659258262890683122, 1.000000000000000000, 0.9659258262890683122, 1.000000000000000000, 0.9659258262890683122, 1.000000000000000000, 0.9659258262890683122, 1.000000000000000000, 0.9659258262890683122, 1.000000000000000000, 0.9659258262890683122, 1.000000000000000000, 0.9659258262890683122, 1.000000000000000000, 0.9659258262890683122, 1.000000000000000000, 0.9659258262890683122, 1.000000000000000000, 0.9659258262890683122, 1.000000000000000000, 0.9659258262890683122, 1.000000000000000000, 0.9659258262890683122, 1.000000000000000000, 0.9659258262890683122, 1.000000000000000000, 0.9659258262890683122, 1.000000000000000000, 0.9659258262890683122, 1.000000000000000000, 0.9659258262890683122, 1.000000000000000000, 0.9659258262890683122, 1.000000000000000000, 0.9659258262890683122, 1.000000000000000000, 0.9659258262890683122, 1.000000000000000000, 0.9659258262890683122, 1.000000000000000000, 0.9659258262890683122, 1.000000000000000000, 0.9659258262890683122, 1.000000000000000000, 0.9659258262890683122, 1.000000000000000000, 0.9659258262890683122, 1.000000000000000000, 0.9659258262890683122, 1.000000000000000000, 0.9659258262890683122, 1.000000000000000000, 0.9659258262890683122, 1.000000000000000000, 0.9659258262890683122, 1.000000000000000000, 0.9659258262890683122, 1.000000000000000000, 0.9659258262890683122, 1.000000000000000000, 0.9659258262890683122, 1.000000000000000000, 0.9659258262890683122, 1.000000000000000000, 0.9659258262890683122, 1.000000000000000000, 0.9659258262890683122, 1.000000000000000000, 0.9659258262890683122, 1.000000000000000000, 0.9659258262890683122, 1.000000000000000000, 0.9659258262890683122, 1.000000000000000000, 0.9659258262890683122, 1.000000000000000000, 0.9659258262890683122, 1.000000000000000000, 0.9659258262890683122, 1.000000000000000000, 0.9659258262890683122, 1.000000000000000000, 0.9659258262890683122, 1.000000000000000000, 0.9659258262890683122, 1.000000000000000000, 0.9659258262890683122, 1.000000000000000000, 0.9659258262890683122, 1.000000000000000000, 0.9659258262890683122, 1.000000000000000000, 0.9659258262890683122, 1.000000000000000000, 0.9659258262890683122, 1.000000000000000000, 0.9659258262890683122, 1.000000000000000000, 0.9659258262890683122, 1.000000000000000000, 0.9659258262890683122, 1.000000000000000000, 0.9659258262890683122, 1.000000000000000000, 0.9659258262890683122, 1.000000000000000000, 0.9659258262890683122, 1.000000000000000000, 0.9659258262890683122, 1.000000000000000000, 0.9659258262890683122, 1.000000000000000000, 0.9659258262890683122, 1.000000000000000000, 0.9659258262890683122, 1.000000000000000000, 0.9659258262890683122, 1.000000000000000000, 0.9659258262890683122, 1.000000000000000000, 0.9659258262890683122, 1.000000000000000000, 0.9659258262890683122, 1.000000000000000000, 0.9659258262890683122, 1.000000000000000000, 0.9659258262890683122, 1.000000000000000000, 0.9659258262890683122, 1.000000000000000000, 0.9659258262890683122, 1.000000000000000000, 0.9659258262890683122, 1.000000000000000000, 0.9659258262890683122, 1.000000000000000000, 0.9659258262890683122, 1.000000000000000000, 0.9659258262890683122, 1.000000000000000000, 0.9659258262890683122, 1.000000000000000000, 0.9659258262890683122, 1.000000000000000000, 0.9659258262890683122, 1.000000000000000000, 0.9659258262890683122, 1.000000000000000000, 0.9659258262890683122, 1.000000000000000000, 0.9659258262890683122, 1.000000000000000000, 0.9659258262890683122, 1.000000000000000000, 0.9659258262890683122, 1.000000000000000000, 0.9659258262890683122, 1.000000000000000000, 0.9659258262890683122, 1.000000000000000000, 0.9659258262890683122, 1.000000000000000000, 0.9659258262890683122, 1.000000000000000000, 0.9659258262890683122, 1.000000000000000000, 0.9659258262890683122, 1.000000000000000000, 0.9659258262890683122, 1.000000000000000000, 0.9659258262890683122, 1.000000000000000000, 0.9659258262890683122, 1.000000000000000000, 0.9659258262890683122, 1.000000000000000000, 0.9659258262890683122, 1.000000000000000000, 0.9659258262890683122, 1.000000000000000000, 0.9659258262890683122, 1.000000000000000000, 0.9659258262890683122, 1.000000000000000000, 0.9659258262890683122, 1.000000000000000000, 0.9659258262890683122, 1.000000000000000000, 0.9659258262890683122, 1.000000000000000000, 0.9659258262890683122, 1.000000000000000000, 0.9659258262890683122, 1.000000000000000000, 0.9659258262890683122, 1.000000000000000000, 0.9659258262890683122, 1.000000000000000000, 0.9659258262890683122, 1.000000000000000000, 0.9659258262890683122, 1.000000000000000000, 0.9659258262890683122, 1.000000000000000000, 0.9659258262890683122, 1.000000000000000000, 0.9659258262890683122, 1.000000000000000000, 0.9659258262890683122, 1.000000000000000000, 0.9659258262890683122, 1.000000000000000000, 0.9659258262890683122, 1.000000000000000000, 0.9659258262890683122, 1.000000000000000000, 0.9659258262890683122, 1.000000000000000000, 0.9659258262890683122, 1.000000000000000000, 0.9659258262890683122, 1.000000000000000000, 0.9659258262890683122, 1.000000000000000000, 0.9659258262890683122, 1.000000000000000000, 0.9659258262890683122, 1.000000000000000000, 0.9659258262890683122, 1.000000000000000000, 0.9659258262890683122, 1.000000000000000000, 0.9659258262890683122, 1.000000000000000000, 0.9659258262890683122, 1.000000000000000000, 0.9659258262890683122, 1.000000000000000000, 0.9659258262890683122, 1.000000000000000000, 0.9659258262890683122, 1.000000000000000000, 0.9659258262890683122, 1.000000000000000000, 0.9659258262890683122, 1.000000000000000000, 0.9659258262890683122, 1.000000000000000000, 0.9659258262890683122, 1.000000000000000000, 0.9659258262890683122, 1.000000000000000000, 0.9659258262890683122, 1.000000000000000000, 0.9659258262890683122, 1.000000000000000000, 0.9659258262890683122, 1.000000000000000000, 0.9659258262890683122, 1.000000000000000000, 0.9659258262890683122, 1.000000000000000000, 0.9659258262890683122, 1.000000000000000000, 0.9659258262890683122, 1.000000000000000000, 0.9659258262890683122, 1.000000000000000000, 0.9659258262890683122, 1.000000000000000000, 0.9659258262890683122, 1.000000000000000000, 0.9659258262890683122, 1.000000000000000000, 0.9659258262890683122, 1.000000000000000000, 0.9659258262890683122, 1.000000000000000000, 0.9659258262890683122, 1.000000000000000000, 0.9659258262890683122, 1.000000000000000000, 0.9659258262890683122, 1.000000000000000000, 0.9659258262890683122, 1.000000000000000000, 0.9659258262890683122, 1.000000000000000000, 0.9659258262890683122, 1.000000000000000000, 0.9659258262890683122, 1.000000000000000000, 0.9659258262890683122, 1.000000000000000000, 0.9659258262890683122, 1.000000000000000000, 0.9659258262890683122, 1.000000000000000000, 0.9659258262890683122, 1.000000000000000000, 0.9659258262890683122, 1.000000000000000000, 0.9659258262890683122, 1.000000000000000000, 0.9659258262890683122, 1.000000000000000000, 0.9659258262890683122, 1.000000000000000000, 0.9659258262890683122, 1.000000000000000000, 0.9659258262890683122, 1.000000000000000000, 0.9659258262890683122, 1.000000000000000000, 0.9659258262890683122, 1.000000000000000000, 0.9659258262890683122, 1.000000000000000000, 0.9659258262890683122, 1.000000000000000000, 0.9659258262890683122, 1.000000000000000000, 0.9659258262890683122, 1.000000000000000000, 0.9659258262890683122, 1.000000000000000000, 0.9659258262890683122, 1.000000000000000000, 0.9659258262890683122, 1.000000000000000000, 0.9659258262890683122, 1.000000000000000000, 0.9659258262890683122, 1.000000000000000000, 0.9659258262890683122, 1.000000000000000000, 0.9659258262890683122, 1.000000000000000000, 0.9659258262890683122, 1.000000000000000000, 0.9659258262890683122, 1.000000000000000000, 0.9659258262890683122, 1.000000000000000000, 0.9659258262890683122, 1.000000000000000000, 0.9659258262890683122, 1.000000000000000000, 0.9659258262890683122, 1.000000000000000000, 0.9659258262890683122, 1.000000000000000000),
 ( 1.000000000000000000, 0.9659258262890683122, 1.000000000000000000, 0.9659258262890683122, 1.000000000000000000, 0.9659258262890683122, 1.000000000000000000, 0.9659258262890683122, 1.000000000000000000, 0.9659258262890683122, 1.000000000000000000, 0.9659258262890683122, 1.000000000000000000, 0.9659258262890683122, 1.000000000000000000, 0.9659258262890683122, 1.000000000000000000, 0.9659258262890683122, 1.000000000000000000, 0.9659258262890683122, 1.000000000000000000, 0.9659258262890683122, 1.000000000000000000, 0.9659258262890683122, 1.000000000000000000, 0.9659258262890683122, 1.000000000000000000, 0.9659258262890683122, 1.000000000000000000, 0.9659258262890683122, 1.000000000000000000, 0.9659258262890683122, 1.000000000000000000, 0.9659258262890683122, 1.000000000000000000, 0.9659258262890683122, 1.000000000000000000, 0.9659258262890683122, 1.000000000000000000, 0.9659258262890683122, 1.000000000000000000, 0.9659258262890683122, 1.000000000000000000, 0.9659258262890683122, 1.000000000000000000, 0.9659258262890683122, 1.000000000000000000, 0.9659258262890683122, 1.000000000000000000, 0.9659258262890683122, 1.000000000000000000, 0.9659258262890683122, 1.000000000000000000, 0.9659258262890683122, 1.000000000000000000, 0.9659258262890683122, 1.000000000000000000, 0.9659258262890683122, 1.000000000000000000, 0.9659258262890683122, 1.000000000000000000, 0.9659258262890683122, 1.000000000000000000, 0.9659258262890683122, 1.000000000000000000, 0.9659258262890683122, 1.000000000000000000, 0.9659258262890683122, 1.000000000000000000, 0.9659258262890683122, 1.000000000000000000, 0.9659258262890683122, 1.000000000000000000, 0.9659258262890683122, 1.000000000000000000, 0.9659258262890683122, 1.000000000000000000, 0.9659258262890683122, 1.000000000000000000, 0.9659258262890683122, 1.000000000000000000, 0.9659258262890683122, 1.000000000000000000, 0.9659258262890683122, 1.000000000000000000, 0.9659258262890683122, 1.000000000000000000, 0.9659258262890683122, 1.000000000000000000, 0.9659258262890683122, 1.000000000000000000, 0.9659258262890683122, 1.000000000000000000, 0.9659258262890683122, 1.000000000000000000, 0.9659258262890683122, 1.000000000000000000, 0.9659258262890683122, 1.000000000000000000, 0.9659258262890683122, 1.000000000000000000, 0.9659258262890683122, 1.000000000000000000, 0.9659258262890683122, 1.000000000000000000, 0.9659258262890683122, 1.000000000000000000, 0.9659258262890683122, 1.000000000000000000, 0.9659258262890683122, 1.000000000000000000, 0.9659258262890683122, 1.000000000000000000, 0.9659258262890683122, 1.000000000000000000, 0.9659258262890683122, 1.000000000000000000, 0.9659258262890683122, 1.000000000000000000, 0.9659258262890683122, 1.000000000000000000, 0.9659258262890683122, 1.000000000000000000, 0.9659258262890683122, 1.000000000000000000, 0.9659258262890683122, 1.000000000000000000, 0.9659258262890683122, 1.000000000000000000, 0.9659258262890683122, 1.000000000000000000, 0.9659258262890683122, 1.000000000000000000, 0.9659258262890683122, 1.000000000000000000, 0.9659258262890683122, 1.000000000000000000, 0.9659258262890683122, 1.000000000000000000, 0.9659258262890683122, 1.000000000000000000, 0.9659258262890683122, 1.000000000000000000, 0.9659258262890683122, 1.000000000000000000, 0.9659258262890683122, 1.000000000000000000, 0.9659258262890683122, 1.000000000000000000, 0.9659258262890683122, 1.000000000000000000, 0.9659258262890683122, 1.000000000000000000, 0.9659258262890683122, 1.000000000000000000, 0.9659258262890683122, 1.000000000000000000, 0.9659258262890683122, 1.000000000000000000, 0.9659258262890683122, 1.000000000000000000, 0.9659258262890683122, 1.000000000000000000, 0.9659258262890683122, 1.000000000000000000, 0.9659258262890683122, 1.000000000000000000, 0.9659258262890683122, 1.000000000000000000, 0.9659258262890683122, 1.000000000000000000, 0.9659258262890683122, 1.000000000000000000, 0.9659258262890683122, 1.000000000000000000, 0.9659258262890683122, 1.000000000000000000, 0.9659258262890683122, 1.000000000000000000, 0.9659258262890683122, 1.000000000000000000, 0.9659258262890683122, 1.000000000000000000, 0.9659258262890683122, 1.000000000000000000, 0.9659258262890683122, 1.000000000000000000, 0.9659258262890683122, 1.000000000000000000, 0.9659258262890683122, 1.000000000000000000, 0.9659258262890683122, 1.000000000000000000, 0.9659258262890683122, 1.000000000000000000, 0.9659258262890683122, 1.000000000000000000, 0.9659258262890683122, 1.000000000000000000, 0.9659258262890683122, 1.000000000000000000, 0.9659258262890683122, 1.000000000000000000, 0.9659258262890683122, 1.000000000000000000, 0.9659258262890683122, 1.000000000000000000, 0.9659258262890683122, 1.000000000000000000, 0.9659258262890683122, 1.000000000000000000, 0.9659258262890683122, 1.000000000000000000, 0.9659258262890683122, 1.000000000000000000, 0.9659258262890683122, 1.000000000000000000, 0.9659258262890683122, 1.000000000000000000, 0.9659258262890683122, 1.000000000000000000, 0.9659258262890683122, 1.000000000000000000, 0.9659258262890683122, 1.000000000000000000, 0.9659258262890683122, 1.000000000000000000, 0.9659258262890683122, 1.000000000000000000, 0.9659258262890683122, 1.000000000000000000, 0.9659258262890683122, 1.000000000000000000, 0.9659258262890683122, 1.000000000000000000, 0.9659258262890683122, 1.000000000000000000, 0.9659258262890683122, 1.000000000000000000, 0.9659258262890683122, 1.000000000000000000, 0.9659258262890683122, 1.000000000000000000, 0.9659258262890683122, 1.000000000000000000, 0.9659258262890683122, 1.000000000000000000, 0.9659258262890683122, 1.000000000000000000, 0.9659258262890683122, 1.000000000000000000, 0.9659258262890683122, 1.000000000000000000, 0.9659258262890683122, 1.000000000000000000, 0.9659258262890683122, 1.000000000000000000, 0.9659258262890683122, 1.000000000000000000, 0.9659258262890683122, 1.000000000000000000, 0.9659258262890683122, 1.000000000000000000, 0.9659258262890683122, 1.000000000000000000, 0.9659258262890683122, 1.000000000000000000, 0.9659258262890683122, 1.000000000000000000, 0.9659258262890683122, 1.000000000000000000, 0.9659258262890683122, 1.000000000000000000, 0.9659258262890683122, 1.000000000000000000, 0.9659258262890683122, 1.000000000000000000, 0.9659258262890683122, 1.000000000000000000, 0.9659258262890683122, 1.000000000000000000, 0.9659258262890683122, 1.000000000000000000, 0.9659258262890683122, 1.000000000000000000, 0.9659258262890683122, 1.000000000000000000, 0.9659258262890683122, 1.000000000000000000, 0.9659258262890683122, 1.000000000000000000, 0.9659258262890683122, 1.000000000000000000, 0.9659258262890683122, 1.000000000000000000, 0.9659258262890683122, 1.000000000000000000, 0.9659258262890683122, 1.000000000000000000, 0.9659258262890683122, 1.000000000000000000, 0.9659258262890683122, 1.000000000000000000, 0.9659258262890683122, 1.000000000000000000, 0.9659258262890683122, 1.000000000000000000, 0.9659258262890683122, 1.000000000000000000, 0.9659258262890683122, 1.000000000000000000, 0.9659258262890683122, 1.000000000000000000, 0.9659258262890683122, 1.000000000000000000, 0.9659258262890683122, 1.000000000000000000, 0.9659258262890683122, 1.000000000000000000, 0.9659258262890683122, 1.000000000000000000, 0.9659258262890683122, 1.000000000000000000, 0.9659258262890683122, 1.000000000000000000, 0.9659258262890683122, 1.000000000000000000, 0.9659258262890683122, 1.000000000000000000, 0.9659258262890683122, 1.000000000000000000, 0.9659258262890683122, 1.000000000000000000, 0.9659258262890683122, 1.000000000000000000, 0.9659258262890683122, 1.000000000000000000, 0.9659258262890683122, 1.000000000000000000, 0.9659258262890683122, 1.000000000000000000, 0.9659258262890683122, 1.000000000000000000, 0.9659258262890683122, 1.000000000000000000, 0.9659258262890683122, 1.000000000000000000, 0.9659258262890683122, 1.000000000000000000, 0.9659258262890683122, 1.000000000000000000, 0.9659258262890683122, 1.000000000000000000, 0.9659258262890683122, 1.000000000000000000, 0.9659258262890683122, 1.000000000000000000, 0.9659258262890683122, 1.000000000000000000, 0.9659258262890683122, 1.000000000000000000, 0.9659258262890683122, 1.000000000000000000, 0.9659258262890683122, 1.000000000000000000, 0.9659258262890683122, 1.000000000000000000, 0.9659258262890683122, 1.000000000000000000, 0.9659258262890683122, 1.000000000000000000, 0.9659258262890683122, 1.000000000000000000, 0.9659258262890683122, 1.000000000000000000, 0.9659258262890683122, 1.000000000000000000, 0.9659258262890683122, 1.000000000000000000, 0.9659258262890683122, 1.000000000000000000, 0.9659258262890683122, 1.000000000000000000, 0.9659258262890683122, 1.000000000000000000, 0.9659258262890683122, 1.000000000000000000, 0.9659258262890683122, 1.000000000000000000, 0.9659258262890683122, 1.000000000000000000, 0.9659258262890683122, 1.000000000000000000, 0.9659258262890683122, 1.000000000000000000, 0.9659258262890683122, 1.000000000000000000, 0.9659258262890683122, 1.000000000000000000, 0.9659258262890683122, 1.000000000000000000, 0.9659258262890683122, 1.000000000000000000, 0.9659258262890683122, 1.000000000000000000, 0.9659258262890683122, 1.000000000000000000, 0.9659258262890683122, 1.000000000000000000, 0.9659258262890683122, 1.000000000000000000, 0.9659258262890683122, 1.000000000000000000, 0.9659258262890683122, 1.000000000000000000, 0.9659258262890683122, 1.000000000000000000, 0.9659258262890683122, 1.000000000000000000, 0.9659258262890683122, 1.000000000000000000, 0.9659258262890683122, 1.000000000000000000, 0.9659258262890683122, 1.000000000000000000, 0.9659258262890683122, 1.000000000000000000, 0.9659258262890683122, 1.000000000000000000, 0.9659258262890683122, 1.000000000000000000, 0.9659258262890683122, 1.000000000000000000, 0.9659258262890683122, 1.000000000000000000, 0.9659258262890683122, 1.000000000000000000, 0.9659258262890683122, 1.000000000000000000, 0.9659258262890683122, 1.000000000000000000, 0.9659258262890683122, 1.000000000000000000, 0.9659258262890683122, 1.000000000000000000, 0.9659258262890683122, 1.000000000000000000, 0.9659258262890683122, 1.000000000000000000, 0.9659258262890683122, 1.000000000000000000, 0.9659258262890683122, 1.000000000000000000, 0.9659258262890683122, 1.000000000000000000, 0.9659258262890683122, 1.000000000000000000, 0.9659258262890683122, 1.000000000000000000, 0.9659258262890683122, 1.000000000000000000, 0.9659258262890683122, 1.000000000000000000, 0.9659258262890683122, 1.000000000000000000, 0.9659258262890683122, 1.000000000000000000, 0.9659258262890683122, 1.000000000000000000, 0.9659258262890683122, 1.000000000000000000, 0.9659258262890683122, 1.000000000000000000, 0.9659258262890683122, 1.000000000000000000, 0.9659258262890683122, 1.000000000000000000, 0.9659258262890683122, 1.000000000000000000, 0.9659258262890683122, 1.000000000000000000, 0.9659258262890683122, 1.000000000000000000, 0.9659258262890683122, 1.000000000000000000, 0.9659258262890683122, 1.000000000000000000, 0.9659258262890683122, 1.000000000000000000, 0.9659258262890683122, 1.000000000000000000, 0.9659258262890683122, 1.000000000000000000, 0.9659258262890683122, 1.000000000000000000, 0.9659258262890683122, 1.000000000000000000, 0.9659258262890683122, 1.000000000000000000, 0.9659258262890683122, 1.000000000000000000, 0.9659258262890683122, 1.000000000000000000, 0.9659258262890683122, 1.000000000000000000, 0.9659258262890683122, 1.000000000000000000, 0.9659258262890683122, 1.000000000000000000, 0.9659258262890683122, 1.000000000000000000) ) ) 
 REPRESENTATION_ITEM ( '' )  SURFACE ( )  );
#28517 = CARTESIAN_POINT ( 'NONE',  ( 1.371391076115485719, -0.6692913385826773087, -0.1292274648535924053 ) ) ;
#28518 = CARTESIAN_POINT ( 'NONE',  ( -0.02624671916010428221, -0.5023911411419708095, 0.1820866141732285504 ) ) ;
#28519 = CARTESIAN_POINT ( 'NONE',  ( 0.01968503937007930540, 0.1660481256975885056, 0.3530559997133364547 ) ) ;
#28520 = CARTESIAN_POINT ( 'NONE',  ( -1.633858267716534529, 0.1660481256975885056, 0.3530559997133364547 ) ) ;
#28521 = CARTESIAN_POINT ( 'NONE',  ( 1.620734908136483465, -0.6692913385826771977, 0.1292274648535927661 ) ) ;
#28522 = CARTESIAN_POINT ( 'NONE',  ( 1.135170603674541256, -0.6692913385826773087, -0.1292274648535924053 ) ) ;
#28523 = CARTESIAN_POINT ( 'NONE',  ( -0.7742782152230965886, -0.004921259842519576551, 0.3153832671262227771 ) ) ;
#28524 = CARTESIAN_POINT ( 'NONE',  ( 0.1070741851644053527, 0.3996062992125986590, -0.3083989501312335846 ) ) ;
#28525 = CARTESIAN_POINT ( 'NONE',  ( -0.3949938075777411628, 0.1058382717557497937, -0.03280839895013128865 ) ) ;
#28526 = EDGE_CURVE ( 'NONE', #26176, #62181, #80152, .T. ) ;
#28527 = CARTESIAN_POINT ( 'NONE',  ( -0.009287274676460672077, -0.3937527723457948658, -2.032323646524292649E-15 ) ) ;
#28528 = CARTESIAN_POINT ( 'NONE',  ( 1.292650918635171564, 0.1771653543307087630, 0.09757992244046791164 ) ) ;
#28529 = CARTESIAN_POINT ( 'NONE',  ( 0.000000000000000000, 2.559055118110236560, 0.000000000000000000 ) ) ;
#28530 = CARTESIAN_POINT ( 'NONE',  ( 0.8070866141732288002, 0.1660481256975885056, 0.3530559997133364547 ) ) ;
#28531 = CARTESIAN_POINT ( 'NONE',  ( -0.3917322834645671215, 0.1049643490035301469, -2.479658792650918375 ) ) ;
#28532 = CARTESIAN_POINT ( 'NONE',  ( 1.404199475065617708, -0.004921259842519870586, -0.3153832671262229437 ) ) ;
#28533 = CARTESIAN_POINT ( 'NONE',  ( 0.05249343832021075018, -0.6046776061558807314, 0.2411417322834647770 ) ) ;
#28534 = CARTESIAN_POINT ( 'NONE',  ( -0.3083989501312330295, -0.3162353388693409650, -0.4822834645669289433 ) ) ;
#28535 = DIRECTION ( 'NONE',  ( 0.000000000000000000, 1.000000000000000000, -8.673617379884024625E-16 ) ) ;
#28536 = CARTESIAN_POINT ( 'NONE',  ( 0.2362204724409449064, 0.4091458600556404646, -0.7742782152230971437 ) ) ;
#28537 = CARTESIAN_POINT ( 'NONE',  ( -0.3996062992125986035, -1.273259842764937629E-12, -1.929133858267794599 ) ) ;
#28538 = CARTESIAN_POINT ( 'NONE',  ( 0.4265091863517067039, -0.5511811023622048555, -0.09757992244046775898 ) ) ;
#28539 = ORIENTED_EDGE ( 'NONE', *, *, #238, .F. ) ;
#28540 = CARTESIAN_POINT ( 'NONE',  ( 0.1958661417322834775, 0.3392501089628018884, -0.2985757462280333452 ) ) ;
#28541 = VERTEX_POINT ( 'NONE', #1152 ) ;
#28542 = CARTESIAN_POINT ( 'NONE',  ( -0.4921259842519677963, -0.5400638737290844871, 0.3530559997133364547 ) ) ;
#28543 = PRODUCT_DEFINITION_SHAPE ( 'NONE', 'NONE',  #5877 ) ;
#28544 = CARTESIAN_POINT ( 'NONE',  ( 0.8858267716535438430, -0.5400638737290845981, -0.3530559997133363437 ) ) ;
#28545 = CARTESIAN_POINT ( 'NONE',  ( 0.03280839895013198948, -0.6692913385826773087, -0.1292274648535924053 ) ) ;
#28546 = CARTESIAN_POINT ( 'NONE',  ( -0.3543307086614165824, 0.1771653543307087630, 0.000000000000000000 ) ) ;
#28547 = CARTESIAN_POINT ( 'NONE',  ( 0.7808398950131241190, -0.05778040916215560624, -0.4822834645669293319 ) ) ;
#28548 = CARTESIAN_POINT ( 'NONE',  ( -0.7677165354330699465, -0.5400638737290845981, -0.3530559997133363437 ) ) ;
#28549 = CARTESIAN_POINT ( 'NONE',  ( -0.2034120734908131112, -0.6692913385826773087, -0.1292274648535924053 ) ) ;
#28550 = CARTESIAN_POINT ( 'NONE',  ( -0.9776902887139098386, -0.6692913385826771977, 0.1292274648535927661 ) ) ;
#28551 = CARTESIAN_POINT ( 'NONE',  ( 1.345144356955381593, -0.3162353388693409650, -0.4822834645669289433 ) ) ;
#28552 = AXIS2_PLACEMENT_3D ( 'NONE', #64963, #8556, #34224 ) ;
#28553 = CARTESIAN_POINT ( 'NONE',  ( 0.8792650918635177559, -0.4281496062992127816, -0.4176697321401328100 ) ) ;
#28554 = EDGE_CURVE ( 'NONE', #53885, #21217, #61900, .T. ) ;
#28555 = CARTESIAN_POINT ( 'NONE',  ( 0.7808398950131241190, -0.05778040916215560624, -0.4822834645669293319 ) ) ;
#28556 = CARTESIAN_POINT ( 'NONE',  ( -9.594673741351313045E-17, 0.3917322834645670104, -0.4645669291338582751 ) ) ;
#28557 = CARTESIAN_POINT ( 'NONE',  ( -0.05249343832020911260, 0.1283753931104748280, 0.1820866141732283561 ) ) ;
#28558 = ORIENTED_EDGE ( 'NONE', *, *, #4397, .T. ) ;
#28559 = CARTESIAN_POINT ( 'NONE',  ( -0.3949938075777409408, -0.1058382717557502933, -0.9908136482939633449 ) ) ;
#28560 = VERTEX_POINT ( 'NONE', #727 ) ;
#28561 = CARTESIAN_POINT ( 'NONE',  ( -0.9055118110236215490, 0.1771653543307087630, 0.000000000000000000 ) ) ;
#28562 = CARTESIAN_POINT ( 'NONE',  ( -0.4986876640419939388, 0.2306618581243847221, -0.2411417322834647770 ) ) ;
#28563 = CARTESIAN_POINT ( 'NONE',  ( 2.874027875014219635, 1.062979042929935503, 0.007789085821686646954 ) ) ;
#28564 = CARTESIAN_POINT ( 'NONE',  ( -0.09186351706036689768, 0.05413385826771626580, -0.4176697321401330321 ) ) ;
#28565 = CARTESIAN_POINT ( 'NONE',  ( -0.4921259842519677963, -0.5400638737290844871, 0.3530559997133364547 ) ) ;
#28566 = CARTESIAN_POINT ( 'NONE',  ( -1.410761154855641575, -0.3162353388693409650, -0.4822834645669289433 ) ) ;
#28567 = CARTESIAN_POINT ( 'NONE',  ( -1.528871391076114250, 0.2952755905511810774, -0.1292274648535930714 ) ) ;
#28568 = CARTESIAN_POINT ( 'NONE',  ( 1.043307086614173818, 0.07958543189024085140, 0.2665933059059887866 ) ) ;
#28569 = CARTESIAN_POINT ( 'NONE',  ( -0.4677827689124922084, 0.03937007874015747977, 2.154527559055118946 ) ) ;
#28570 = CARTESIAN_POINT ( 'NONE',  ( 0.2364516566766633465, 0.1768582946180018156, 5.689955017551601379 ) ) ;
#28571 = CARTESIAN_POINT ( 'NONE',  ( 0.3543307086614179147, 0.1771653543307087630, 0.000000000000000000 ) ) ;
#28572 = CARTESIAN_POINT ( 'NONE',  ( -0.01968503937007793844, 0.1660481256975883668, -0.3530559997133364547 ) ) ;
#28573 = CARTESIAN_POINT ( 'NONE',  ( 0.4133858267716541968, 0.1660481256975885056, 0.3530559997133364547 ) ) ;
#28574 = ORIENTED_EDGE ( 'NONE', *, *, #40435, .T. ) ;
#28575 = CARTESIAN_POINT ( 'NONE',  ( -0.3460692066303960868, 0.1998031496062990242, -1.758530183727034180 ) ) ;
#28576 = CARTESIAN_POINT ( 'NONE',  ( -2.795275590551184131, 1.062992125984252079, -2.654250759839014936E-16 ) ) ;
#28577 = ORIENTED_EDGE ( 'NONE', *, *, #22453, .T. ) ;
#28578 = CARTESIAN_POINT ( 'NONE',  ( -0.1070741851644051862, -0.3996062992125986590, -1.251312335958005173 ) ) ;
#28579 = CARTESIAN_POINT ( 'NONE',  ( 4.893765752498283308E-17, -0.3996062992125985480, -0.6279527559055118058 ) ) ;
#28580 = CARTESIAN_POINT ( 'NONE',  ( -0.6692913385826764205, -0.5511811023622047445, 6.969142054262312111E-17 ) ) ;
#28581 = CARTESIAN_POINT ( 'NONE',  ( -0.6233595800524928121, -0.05778040916215522460, 0.4822834645669289988 ) ) ;
#28582 = CARTESIAN_POINT ( 'NONE',  ( 0.4724409448818897572, -0.1265901696524988906, 0.04593175853018372640 ) ) ;
#28583 = EDGE_CURVE ( 'NONE', #1453, #8617, #30996, .T. ) ;
#28584 = CARTESIAN_POINT ( 'NONE',  ( -0.2867679344610364334, -0.2867679344610367109, -2.663385826771653253 ) ) ;
#28585 = CARTESIAN_POINT ( 'NONE',  ( 1.581364829396326277, -0.3162353388693409650, -0.4822834645669289433 ) ) ;
#28586 = CARTESIAN_POINT ( 'NONE',  ( 0.8136482939632553313, 0.2306618581243848609, 0.2411417322834645549 ) ) ;
#28587 = CARTESIAN_POINT ( 'NONE',  ( 1.010498687664042716, -0.4281496062992124485, 0.4176697321401328655 ) ) ;
#28588 = CARTESIAN_POINT ( 'NONE',  ( -0.5708661417322825615, -0.4536011799217367080, 0.2665933059059888421 ) ) ;
#28589 = CARTESIAN_POINT ( 'NONE',  ( 0.1837270341207354329, 0.2306618581243848609, 0.2411417322834645549 ) ) ;
#28590 = CARTESIAN_POINT ( 'NONE',  ( 0.2362204724409451007, -0.4091458600556402980, -1.743438320209973469 ) ) ;
#28591 = CARTESIAN_POINT ( 'NONE',  ( -0.06561679790026180015, -0.004921259842519576551, 0.3153832671262227771 ) ) ;
#28592 = CARTESIAN_POINT ( 'NONE',  ( -0.6496062992125976043, -0.5400638737290844871, 0.3530559997133364547 ) ) ;
#28593 = CARTESIAN_POINT ( 'NONE',  ( -0.3949938075777408852, -0.1058382717557502933, -1.854986876640420501 ) ) ;
#28594 = CARTESIAN_POINT ( 'NONE',  ( 1.515748031496063186, -0.4536011799217368745, -0.2665933059059886201 ) ) ;
#28595 = CARTESIAN_POINT ( 'NONE',  ( -0.05249343832020938322, -0.5023911411419708095, -0.1820866141732282451 ) ) ;
#28596 = CARTESIAN_POINT ( 'NONE',  ( 1.463254593175853824, -0.5511811023622046335, 0.09757992244046803654 ) ) ;
#28597 = CARTESIAN_POINT ( 'NONE',  ( -1.194225721784776262, 0.05413385826771626580, -0.4176697321401330321 ) ) ;
#28598 = CARTESIAN_POINT ( 'NONE',  ( -0.6496062992125976043, 0.07958543189024071263, -0.2665933059059888421 ) ) ;
#28599 = CARTESIAN_POINT ( 'NONE',  ( -1.168682819302786058, -2.294479370626195693E-15, 0.3464511005275217603 ) ) ;
#28600 = CARTESIAN_POINT ( 'NONE',  ( -1.062992125984250968, 0.2952755905511811885, 0.000000000000000000 ) ) ;
#28601 = CARTESIAN_POINT ( 'NONE',  ( -0.2034120734908128059, 0.2952755905511811885, 0.1292274648535926551 ) ) ;
#28602 = CARTESIAN_POINT ( 'NONE',  ( -0.1070741851644051862, -0.3996062992125986590, -2.668635170603674833 ) ) ;
#28603 = CARTESIAN_POINT ( 'NONE',  ( 0.1958661417322836162, -0.3392501089628018329, -2.376621104165667298 ) ) ;
#28604 = CARTESIAN_POINT ( 'NONE',  ( -1.964921794496046648, 1.189595890467119776, -0.3229789317950364502 ) ) ;
#28605 = CARTESIAN_POINT ( 'NONE',  ( 0.4330708661417329575, 0.1771653543307087630, 0.000000000000000000 ) ) ;
#28606 = CARTESIAN_POINT ( 'NONE',  ( 0.8727034120734912248, -0.3162353388693409650, -0.4822834645669289433 ) ) ;
#28607 = CARTESIAN_POINT ( 'NONE',  ( -1.279527559055116948, -0.4536011799217367080, 0.2665933059059888421 ) ) ;
#28608 = CARTESIAN_POINT ( 'NONE',  ( 1.358267716535433323, 0.1660481256975885056, 0.3530559997133364547 ) ) ;
#28609 = CARTESIAN_POINT ( 'NONE',  ( -1.456692913385826182, -0.5511811023622047445, 6.969142054262312111E-17 ) ) ;
#28610 = AXIS2_PLACEMENT_3D ( 'NONE', #26088, #45014, #71133 ) ;
#28611 = CARTESIAN_POINT ( 'NONE',  ( -0.4724409448818890911, -0.1870078740157479769, 0.4822834645669291653 ) ) ;
#28612 = CARTESIAN_POINT ( 'NONE',  ( 0.07874015748031558404, -0.1870078740157479769, 0.3641732283464567677 ) ) ;
#28613 = DIRECTION ( 'NONE',  ( 0.7071067811865495711, 0.000000000000000000, -0.7071067811865454633 ) ) ;
#28614 = CARTESIAN_POINT ( 'NONE',  ( 0.6036745406824153282, -0.5023911411419708095, 0.1820866141732285504 ) ) ;
#28615 = CARTESIAN_POINT ( 'NONE',  ( 0.05905511811023709395, -0.5400638737290844871, 0.3530559997133364547 ) ) ;
#28616 = CARTESIAN_POINT ( 'NONE',  ( -0.3460692066303957537, -0.1998031496062994405, -0.1292650918635170620 ) ) ;
#28617 = CARTESIAN_POINT ( 'NONE',  ( -1.069553805774277722, 0.2952755905511811885, 0.1292274648535926551 ) ) ;
#28618 = CARTESIAN_POINT ( 'NONE',  ( -0.1958661417322834220, -0.3392501089628018884, -1.725065616797900381 ) ) ;
#28619 = CARTESIAN_POINT ( 'NONE',  ( 1.056430446194226436, -0.5511811023622048555, -0.09757992244046775898 ) ) ;
#28620 = CARTESIAN_POINT ( 'NONE',  ( -0.05249343832020911260, 0.2306618581243848609, 0.2411417322834645549 ) ) ;
#28621 = CARTESIAN_POINT ( 'NONE',  ( -0.4330708661417315697, -0.6692913385826771977, 8.415575281601705876E-17 ) ) ;
#28622 = CARTESIAN_POINT ( 'NONE',  ( -0.4593175853018364174, -0.3690944881889765550, -0.3153832671262227771 ) ) ;
#28623 = CARTESIAN_POINT ( 'NONE',  ( 1.192688228555126795, 0.02791078216816225699, 0.4328096321851905293 ) ) ;
#28624 = CARTESIAN_POINT ( 'NONE',  ( -0.4199475065616791736, -0.5023911411419708095, 0.1820866141732285504 ) ) ;
#28625 = CARTESIAN_POINT ( 'NONE',  ( 0.2821522309711292364, 0.2952755905511810774, -0.1292274648535930714 ) ) ;
#28626 = EDGE_CURVE ( 'NONE', #58699, #36200, #23108, .T. ) ;
#28627 = CARTESIAN_POINT ( 'NONE',  ( -0.5380577427821514602, -0.3690944881889765550, -0.3153832671262227771 ) ) ;
#28628 = CARTESIAN_POINT ( 'NONE',  ( -9.787531504996566615E-17, 0.3996062992125985480, -1.021653543307086576 ) ) ;
#28629 = CARTESIAN_POINT ( 'NONE',  ( -1.292650918635170010, 0.2952755905511810774, -0.1292274648535930714 ) ) ;
#28630 = CARTESIAN_POINT ( 'NONE',  ( -0.6299212598425062426, 2.755905511811024056, -3.886287458032464226 ) ) ;
#28631 = ORIENTED_EDGE ( 'NONE', *, *, #35272, .T. ) ;
#28632 = ADVANCED_FACE ( 'NONE', ( #51618 ), #60583, .F. ) ;
#28633 = CARTESIAN_POINT ( 'NONE',  ( -0.9580052493438311334, -0.3690944881889763329, 0.3153832671262228327 ) ) ;
#28634 = CARTESIAN_POINT ( 'NONE',  ( -0.4921259842519677963, -0.5400638737290844871, 0.3530559997133364547 ) ) ;
#28635 = CARTESIAN_POINT ( 'NONE',  ( -1.614173228346456268, -0.6692913385826771977, 8.415575281601705876E-17 ) ) ;
#28636 = CARTESIAN_POINT ( 'NONE',  ( -1.371391076115484609, -0.6692913385826771977, 0.1292274648535927661 ) ) ;
#28637 = DIRECTION ( 'NONE',  ( 0.000000000000000000, 0.000000000000000000, -1.000000000000000000 ) ) ;
#28638 = CARTESIAN_POINT ( 'NONE',  ( 1.423884514435696413, -0.3162353388693409650, -0.4822834645669289433 ) ) ;
#28639 = CARTESIAN_POINT ( 'NONE',  ( 1.062992125984252745, 0.2952755905511811885, 0.000000000000000000 ) ) ;
#28640 = CARTESIAN_POINT ( 'NONE',  ( 0.9881811337016640495, 2.559055118110236560, -0.5314960629921260393 ) ) ;
#28641 = CARTESIAN_POINT ( 'NONE',  ( 0.2635443281053753695, -0.1334515064332121859, 5.819037890265706281 ) ) ;
#28642 = CARTESIAN_POINT ( 'NONE',  ( 1.430446194225722500, -0.004921259842519576551, 0.3153832671262227771 ) ) ;
#28643 = CARTESIAN_POINT ( 'NONE',  ( -0.1998031496062991907, -0.3460692066303959757, -0.6955380577427822120 ) ) ;
#28644 = VERTEX_POINT ( 'NONE', #39006 ) ;
#28645 = CARTESIAN_POINT ( 'NONE',  ( -0.6955380577427815458, -0.004921259842519576551, 0.3153832671262227771 ) ) ;
#28646 = CARTESIAN_POINT ( 'NONE',  ( -0.2867679344610364334, -0.2867679344610367109, -2.098425196850393526 ) ) ;
#28647 = ORIENTED_EDGE ( 'NONE', *, *, #53516, .T. ) ;
#28648 = CARTESIAN_POINT ( 'NONE',  ( 0.6364829396325465405, -0.05778040916215522460, 0.4822834645669289988 ) ) ;
#28649 = CARTESIAN_POINT ( 'NONE',  ( -0.4330708661417315697, 0.2952755905511811885, 0.000000000000000000 ) ) ;
#28650 = CARTESIAN_POINT ( 'NONE',  ( -0.5249343832020990641, 0.2306618581243848609, 0.2411417322834645549 ) ) ;
#28651 = CARTESIAN_POINT ( 'NONE',  ( 1.594488188976378673, -0.5400638737290845981, -0.3530559997133363437 ) ) ;
#28652 = AXIS2_PLACEMENT_3D ( 'NONE', #82345, #50332, #37709 ) ;
#28653 = CARTESIAN_POINT ( 'NONE',  ( -1.253280839895012377, -0.2845877964562161244, -0.3641732283464567121 ) ) ;
#28654 = CARTESIAN_POINT ( 'NONE',  ( 0.05186593092965807728, 1.065829223649503277, -1.574764142214714946 ) ) ;
#28655 = CARTESIAN_POINT ( 'NONE',  ( 0.2362204724409456558, -0.1870078740157479769, 0.4822834645669291653 ) ) ;
#28656 = CARTESIAN_POINT ( 'NONE',  ( -0.8202099737532799750, 0.2952755905511810774, -0.1292274648535930714 ) ) ;
#28657 = CARTESIAN_POINT ( 'NONE',  ( 0.1958661417322836162, -0.3392501089628018329, -1.589219529362517758 ) ) ;
#28658 = CARTESIAN_POINT ( 'NONE',  ( -1.397637795275589623, -0.5400638737290845981, -0.3530559997133363437 ) ) ;
#28659 = DIRECTION ( 'NONE',  ( 0.000000000000000000, -0.000000000000000000, 1.000000000000000000 ) ) ;
#28660 = CARTESIAN_POINT ( 'NONE',  ( 1.128608923884515169, -0.6046776061558809534, -0.2411417322834644161 ) ) ;
#28661 = CARTESIAN_POINT ( 'NONE',  ( 1.332020997375329197, -0.2845877964562159024, 0.3641732283464567677 ) ) ;
#28662 = EDGE_LOOP ( 'NONE', ( #44564, #36197, #82410, #80642 ) ) ;
#28663 = CARTESIAN_POINT ( 'NONE',  ( 0.2891555358219910499, 0.2891555358219910499, 0.01968503937007868437 ) ) ;
#28664 = CARTESIAN_POINT ( 'NONE',  ( -0.4133858267716528645, -0.5400638737290844871, 0.3530559997133364547 ) ) ;
#28665 = ORIENTED_EDGE ( 'NONE', *, *, #45132, .T. ) ;
#28666 = CARTESIAN_POINT ( 'NONE',  ( 0.4133858267716541968, -0.4536011799217368745, -0.2665933059059886201 ) ) ;
#28667 = CARTESIAN_POINT ( 'NONE',  ( -1.108923884514435132, -0.3162353388693405765, 0.4822834645669290543 ) ) ;
#28668 = CARTESIAN_POINT ( 'NONE',  ( 0.8070866141732288002, 0.1660481256975885056, 0.3530559997133364547 ) ) ;
#28669 = CARTESIAN_POINT ( 'NONE',  ( 0.6496062992125991586, 0.1660481256975885056, 0.3530559997133364547 ) ) ;
#28670 = CARTESIAN_POINT ( 'NONE',  ( -0.1771653543307080136, -0.5400638737290844871, 0.3530559997133364547 ) ) ;
#28671 = AXIS2_PLACEMENT_3D ( 'NONE', #25600, #37825, #51263 ) ;
#28672 = CARTESIAN_POINT ( 'NONE',  ( -0.6955380577427815458, 0.05413385826771666132, 0.4176697321401328100 ) ) ;
#28673 = CARTESIAN_POINT ( 'NONE',  ( 4.797336870675656522E-17, -0.3917322834645670104, -2.368110236220472675 ) ) ;
#28674 = CARTESIAN_POINT ( 'NONE',  ( -1.574803149606298636, -0.1870078740157479769, 0.4822834645669291653 ) ) ;
#28675 = CARTESIAN_POINT ( 'NONE',  ( -0.6627296587926501115, 0.2952755905511810774, -0.1292274648535930714 ) ) ;
#28676 = CARTESIAN_POINT ( 'NONE',  ( -0.3477690288713902178, 0.1771653543307087075, -0.09757992244046823083 ) ) ;
#28677 = CARTESIAN_POINT ( 'NONE',  ( 1.469816272965879911, -0.6046776061558807314, 0.2411417322834647770 ) ) ;
#28678 = CARTESIAN_POINT ( 'NONE',  ( 1.437007874015748810, -0.5400638737290845981, -0.3530559997133363437 ) ) ;
#28679 = CARTESIAN_POINT ( 'NONE',  ( -1.010498687664041384, -0.4281496062992127816, -0.4176697321401328100 ) ) ;
#28680 = CARTESIAN_POINT ( 'NONE',  ( 0.2925321140481932369, 0.2925321140481932369, -0.05708661417322836301 ) ) ;
#28681 = CARTESIAN_POINT ( 'NONE',  ( 0.7611548556430451917, -0.6046776061558807314, 0.2411417322834647770 ) ) ;
#28682 = CARTESIAN_POINT ( 'NONE',  ( -0.1998031496062994683, 0.3460692066303958092, -1.902887139107611647 ) ) ;
#28683 = CARTESIAN_POINT ( 'NONE',  ( 3.927338144698056421, 1.151278041681430553, 0.2760671784697421582 ) ) ;
#28684 = CARTESIAN_POINT ( 'NONE',  ( -0.2690288713910754526, -0.6692913385826771977, 0.1292274648535927661 ) ) ;
#28685 = CARTESIAN_POINT ( 'NONE',  ( -0.9645669291338575535, 0.07958543189024071263, -0.2665933059059888421 ) ) ;
#28686 = CARTESIAN_POINT ( 'NONE',  ( 1.141732283464567788, -0.5511811023622047445, 6.969142054262312111E-17 ) ) ;
#28687 = CARTESIAN_POINT ( 'NONE',  ( 0.1265901696524990294, -0.4724409448818896462, -0.4770341207349080848 ) ) ;
#28688 = CARTESIAN_POINT ( 'NONE',  ( 1.148293963254593875, -0.5511811023622046335, 0.09757992244046803654 ) ) ;
#28689 = CARTESIAN_POINT ( 'NONE',  ( 0.6299212598425204535, -0.1870078740157479769, 0.4822834645669291653 ) ) ;
#28690 = CARTESIAN_POINT ( 'NONE',  ( 0.3420746716998660508, -0.1974969037888704149, -0.6541994750656167090 ) ) ;
#28691 = CARTESIAN_POINT ( 'NONE',  ( -0.5249343832020990641, -0.6046776061558809534, -0.2411417322834644161 ) ) ;
#28692 = CARTESIAN_POINT ( 'NONE',  ( -0.3812812444996365180, -2.294479370626195693E-15, 0.3464511005275217603 ) ) ;
#28693 = CARTESIAN_POINT ( 'NONE',  ( 1.305774278215223960, 0.1771653543307087075, -0.09757992244046823083 ) ) ;
#28694 = CARTESIAN_POINT ( 'NONE',  ( -0.4658792650918627265, -0.05778040916215522460, 0.4822834645669289988 ) ) ;
#28695 = CARTESIAN_POINT ( 'NONE',  ( 4.837279021331061486E-17, -0.3949938075777409963, -0.6279527559055118058 ) ) ;
#28696 = CARTESIAN_POINT ( 'NONE',  ( 1.122047244094488860, -0.5400638737290845981, -0.3530559997133363437 ) ) ;
#28697 = CARTESIAN_POINT ( 'NONE',  ( 0.1771653543307093182, 0.1660481256975885056, 0.3530559997133364547 ) ) ;
#28698 = CARTESIAN_POINT ( 'NONE',  ( 0.7086614173228353852, -0.1870078740157479769, 0.3641732283464567677 ) ) ;
#28699 = CARTESIAN_POINT ( 'NONE',  ( -0.3575568722600962479, 1.224102705420558435, -1.063793812528210703 ) ) ;
#28700 = CARTESIAN_POINT ( 'NONE',  ( 0.2952755905511819101, 0.07958543189024071263, -0.2665933059059888421 ) ) ;
#28701 = CARTESIAN_POINT ( 'NONE',  ( -1.089589480386152998, 0.004960608223778174841, 0.3437734562760193513 ) ) ;
#28702 = CARTESIAN_POINT ( 'NONE',  ( 0.1998031496062994128, -0.3460692066303957537, -1.428477690288713964 ) ) ;
#28703 = CARTESIAN_POINT ( 'NONE',  ( 0.8398950131233602345, -0.6046776061558807314, 0.2411417322834647770 ) ) ;
#28704 = CARTESIAN_POINT ( 'NONE',  ( -0.2867679344610364334, -0.2867679344610367109, -1.153543307086613900 ) ) ;
#28705 = CARTESIAN_POINT ( 'NONE',  ( 1.502624671916010790, -0.08942795157527998196, 0.3641732283464567121 ) ) ;
#28706 = CARTESIAN_POINT ( 'NONE',  ( -0.3272402980636380243, 0.2155943732411919889, 6.867566722516314874E-18 ) ) ;
#28707 = CARTESIAN_POINT ( 'NONE',  ( 0.2099737532808405305, 0.1283753931104746893, -0.1820866141732285504 ) ) ;
#28708 = CARTESIAN_POINT ( 'NONE',  ( 0.05249343832021075018, -0.6046776061558807314, 0.2411417322834647770 ) ) ;
#28709 = CARTESIAN_POINT ( 'NONE',  ( 1.371391076115485941, 0.1771653543307087630, 0.09757992244046791164 ) ) ;
#28710 = CARTESIAN_POINT ( 'NONE',  ( -1.292650918635170010, -0.5511811023622046335, 0.09757992244046803654 ) ) ;
#28711 = CARTESIAN_POINT ( 'NONE',  ( -1.522309711286088607, 0.2306618581243847221, -0.2411417322834647770 ) ) ;
#28712 = AXIS2_PLACEMENT_3D ( 'NONE', #57572, #58840, #83264 ) ;
#28713 = CARTESIAN_POINT ( 'NONE',  ( 0.3805774278215230400, -0.4281496062992124485, 0.4176697321401328655 ) ) ;
#28714 = CARTESIAN_POINT ( 'NONE',  ( 1.246719160104987623, 0.05413385826771626580, -0.4176697321401330321 ) ) ;
#28715 = CARTESIAN_POINT ( 'NONE',  ( 1.348312163386739426, 0.000000000000000000, 0.7386866130305692613 ) ) ;
#28716 = CARTESIAN_POINT ( 'NONE',  ( 0.5052493438320215802, 0.2952755905511811885, 0.1292274648535926551 ) ) ;
#28717 = CARTESIAN_POINT ( 'NONE',  ( 1.345144356955381593, -0.05778040916215522460, 0.4822834645669289988 ) ) ;
#28718 = CARTESIAN_POINT ( 'NONE',  ( 0.8070866141732289112, -0.5400638737290845981, -0.3530559997133363437 ) ) ;
#28719 = CARTESIAN_POINT ( 'NONE',  ( 5.785732909357575061E-17, -0.4724409448818898682, -0.3129921259842520231 ) ) ;
#28720 = CARTESIAN_POINT ( 'NONE',  ( 0.6299212598425204535, -0.1870078740157480601, -0.3641732283464567677 ) ) ;
#28721 = CARTESIAN_POINT ( 'NONE',  ( -1.633858267716534529, 0.07958543189024085140, 0.2665933059059887866 ) ) ;
#28722 = CARTESIAN_POINT ( 'NONE',  ( -0.9580052493438311334, -0.004921259842519870586, -0.3153832671262229437 ) ) ;
#28723 = ADVANCED_FACE ( 'NONE', ( #35094 ), #2791, .T. ) ;
#28724 = CARTESIAN_POINT ( 'NONE',  ( 0.6364829396325465405, -0.08942795157527998196, 0.3641732283464567121 ) ) ;
#28725 = VECTOR ( 'NONE', #81989, 39.37007874015748143 ) ;
#28726 = CARTESIAN_POINT ( 'NONE',  ( -0.01968503937007793844, 0.1660481256975883668, -0.3530559997133364547 ) ) ;
#28727 = CARTESIAN_POINT ( 'NONE',  ( 0.6496062992125991586, 0.1660481256975885056, 0.3530559997133364547 ) ) ;
#28728 = CARTESIAN_POINT ( 'NONE',  ( -0.4658792650918627265, -0.3162353388693409650, -0.4822834645669289433 ) ) ;
#28729 = CARTESIAN_POINT ( 'NONE',  ( 0.2952755905511816326, -0.4536011799217367080, 0.2665933059059888421 ) ) ;
#28730 = CARTESIAN_POINT ( 'NONE',  ( 0.8595800524934390507, -0.05778040916215560624, -0.4822834645669293319 ) ) ;
#28731 = LINE ( 'NONE', #79688, #35285 ) ;
#28732 = CARTESIAN_POINT ( 'NONE',  ( -0.8727034120734901146, -0.05778040916215560624, -0.4822834645669293319 ) ) ;
#28734 = CARTESIAN_POINT ( 'NONE',  ( 0.3996062992125985480, 0.1070741851644054637, -0.9120734908136483021 ) ) ;
#28733 = CARTESIAN_POINT ( 'NONE',  ( -1.089238845144356427, 0.05413385826771666132, 0.4176697321401328100 ) ) ;
#28735 = DIRECTION ( 'NONE',  ( 0.000000000000000000, 0.000000000000000000, -1.000000000000000000 ) ) ;
#28736 = CARTESIAN_POINT ( 'NONE',  ( -0.7939632545931750718, -0.05778040916215560624, -0.4822834645669293319 ) ) ;
#28737 = CARTESIAN_POINT ( 'NONE',  ( -0.6364829396325453192, -0.3162353388693405765, 0.4822834645669290543 ) ) ;
#28738 = CARTESIAN_POINT ( 'NONE',  ( 0.1265901696524990294, -0.4724409448818896462, 0.07217847769028870597 ) ) ;
#28739 = CARTESIAN_POINT ( 'NONE',  ( 0.2891555358219910499, -0.2891555358219909944, -2.303149606299212504 ) ) ;
#28740 = EDGE_LOOP ( 'NONE', ( #32604, #37021, #56090, #698, #55412, #55823, #71331, #55002 ) ) ;
#28741 = CARTESIAN_POINT ( 'NONE',  ( 0.8464566929133866546, -0.4536011799217367080, 0.2665933059059888421 ) ) ;
#28742 = CARTESIAN_POINT ( 'NONE',  ( 0.3392501089628018884, -0.1958661417322834220, -0.8845144356955378928 ) ) ;
#28743 = CARTESIAN_POINT ( 'NONE',  ( 1.233595800524935227, -0.6046776061558807314, 0.2411417322834647770 ) ) ;
#28744 = CARTESIAN_POINT ( 'NONE',  ( 3.896872718254346779, 2.702643891907236640, -0.5314960629921260393 ) ) ;
#28745 = CARTESIAN_POINT ( 'NONE',  ( -1.167979002624671470, -0.3690944881889765550, -0.3153832671262227771 ) ) ;
#28746 = CARTESIAN_POINT ( 'NONE',  ( 1.522309711286089939, 0.2306618581243848609, 0.2411417322834645549 ) ) ;
#28747 = CARTESIAN_POINT ( 'NONE',  ( -1.692913385826770645, 0.2952755905511811885, 0.000000000000000000 ) ) ;
#28748 = CARTESIAN_POINT ( 'NONE',  ( 0.5052493438320218022, -0.6692913385826773087, -0.1292274648535924053 ) ) ;
#28749 = CARTESIAN_POINT ( 'NONE',  ( 0.3392501089628018329, -0.1958661417322834497, -0.3425003692575309677 ) ) ;
#28750 = CARTESIAN_POINT ( 'NONE',  ( -0.06561679790026180015, 0.05413385826771666132, 0.4176697321401328100 ) ) ;
#28751 = CARTESIAN_POINT ( 'NONE',  ( -0.8595800524934373854, -0.2845877964562161244, -0.3641732283464567121 ) ) ;
#28752 = CARTESIAN_POINT ( 'NONE',  ( 0.7480314960629927956, -0.6692913385826771977, 8.415575281601705876E-17 ) ) ;
#28753 = CARTESIAN_POINT ( 'NONE',  ( -0.01312335958005186876, -0.4281496062992124485, 0.4176697321401328655 ) ) ;
#28754 = CARTESIAN_POINT ( 'NONE',  ( -1.157146581871515012E-16, 0.4724409448818898682, 0.000000000000000000 ) ) ;
#28755 = CARTESIAN_POINT ( 'NONE',  ( -0.1070741851644056997, 0.3996062992125986035, -2.841207349081364963 ) ) ;
#28756 = CARTESIAN_POINT ( 'NONE',  ( 4.797336870675656522E-17, -0.3917322834645670659, -1.650281782973440192 ) ) ;
#28757 = CARTESIAN_POINT ( 'NONE',  ( 0.9580052493438327987, -0.4281496062992127816, -0.4176697321401328100 ) ) ;
#28758 = CARTESIAN_POINT ( 'NONE',  ( -0.04593175853018302557, -0.6692913385826773087, -0.1292274648535924053 ) ) ;
#28759 = CARTESIAN_POINT ( 'NONE',  ( -1.069553805774277722, -0.6692913385826773087, -0.1292274648535924053 ) ) ;
#28760 = CARTESIAN_POINT ( 'NONE',  ( 0.9973753280839902091, 0.2306618581243847221, -0.2411417322834647770 ) ) ;
#28761 = CARTESIAN_POINT ( 'NONE',  ( 0.3871391076115493490, -0.3162353388693405765, 0.4822834645669290543 ) ) ;
#28762 = CARTESIAN_POINT ( 'NONE',  ( 0.3917322834645669549, 0.1049643490035304660, -1.154199475065616820 ) ) ;
#28763 = CARTESIAN_POINT ( 'NONE',  ( -0.4986876640419942164, -0.6046776061558807314, 0.2411417322834647770 ) ) ;
#28764 = CARTESIAN_POINT ( 'NONE',  ( 0.8005249343832028242, -0.4281496062992127816, -0.4176697321401328100 ) ) ;
#28765 = CARTESIAN_POINT ( 'NONE',  ( 0.1181102362204730916, 0.2952755905511811885, 0.000000000000000000 ) ) ;
#28766 = CIRCLE ( 'NONE', #65055, 3.937007874015748143 ) ;
#28767 = CARTESIAN_POINT ( 'NONE',  ( 0.8136482939632553313, -0.5023911411419708095, -0.1820866141732282451 ) ) ;
#28768 = CARTESIAN_POINT ( 'NONE',  ( -1.404199475065615932, 0.05413385826771666132, 0.4176697321401328100 ) ) ;
#28769 = CARTESIAN_POINT ( 'NONE',  ( -0.1181161979004358292, 1.077624259009879459, -2.860481230828558985 ) ) ;
#28770 = CARTESIAN_POINT ( 'NONE',  ( 0.2952755905511816326, -0.5400638737290844871, 0.3530559997133364547 ) ) ;
#28771 = B_SPLINE_CURVE_WITH_KNOTS ( 'NONE', 3,
 ( #81450, #11150, #75132, #17477, #36808, #30497, #70030, #17883, #5237, #56568, #24587, #75952, #43936, #69630, #11975, #37630, #5644, #50664, #76364, #61976, #41380, #10645, #55232, #16552, #9806, #68308 ),
 .UNSPECIFIED., .F., .F.,
 ( 4, 2, 2, 2, 2, 2, 2, 2, 2, 2, 2, 2, 4 ),
 ( 0.05717903794320495364, 0.05955951868967798712, 0.06193999943615102061, 0.06313023980938753388, 0.06432048018262405409, 0.06670096092909708063, 0.06789120130233358696, 0.06908144167557010717, 0.07027168204880662739, 0.07146192242204313372, 0.07384240316851617414, 0.07503264354175269435, 0.07622288391498921456 ),
 .UNSPECIFIED. ) ;
#28772 = CARTESIAN_POINT ( 'NONE',  ( -0.2867679344610364334, -0.2867679344610367109, -2.255905511811023612 ) ) ;
#28773 = EDGE_LOOP ( 'NONE', ( #52014, #63798, #9434, #80249, #47903 ) ) ;
#28774 = ORIENTED_EDGE ( 'NONE', *, *, #75224, .T. ) ;
#28775 = CARTESIAN_POINT ( 'NONE',  ( 1.279527559055118724, -0.5400638737290845981, -0.3530559997133363437 ) ) ;
#28776 = CARTESIAN_POINT ( 'NONE',  ( 0.5314960629921264834, 0.07958543189024071263, -0.2665933059059888421 ) ) ;
#28778 = CARTESIAN_POINT ( 'NONE',  ( 0.2238009295390077091, 2.409604939980833412E-17, -0.3464511005275205946 ) ) ;
#28777 = CARTESIAN_POINT ( 'NONE',  ( 0.6889763779527560139, 0.000000000000000000, 0.000000000000000000 ) ) ;
#28779 = DIRECTION ( 'NONE',  ( 0.8660254037844362651, 0.000000000000000000, 0.5000000000000041078 ) ) ;
#28780 = DIRECTION ( 'NONE',  ( -0.000000000000000000, 1.000000000000000000, -0.000000000000000000 ) ) ;
#28781 = CARTESIAN_POINT ( 'NONE',  ( -0.2867679344610365999, 0.2867679344610364889, -1.206692913385826627 ) ) ;
#28782 = TOROIDAL_SURFACE ( 'NONE', #46253, 3.858267716535433323, 0.07874015748031495954 ) ;
#28783 = CARTESIAN_POINT ( 'NONE',  ( 0.1998031496062994128, -0.3460692066303957537, -2.373359580052493367 ) ) ;
#28784 = CARTESIAN_POINT ( 'NONE',  ( -0.7742782152230962556, -0.4281496062992127816, -0.4176697321401328100 ) ) ;
#28785 = CARTESIAN_POINT ( 'NONE',  ( -0.5774278215223089816, 0.2306618581243847221, -0.2411417322834647770 ) ) ;
#28786 = CARTESIAN_POINT ( 'NONE',  ( 0.8202099737532813073, 0.2952755905511811885, 0.1292274648535926551 ) ) ;
#28787 = ORIENTED_EDGE ( 'NONE', *, *, #61511, .F. ) ;
#28788 = CARTESIAN_POINT ( 'NONE',  ( 1.417322834645670104, -0.1870078740157479769, 0.4822834645669291653 ) ) ;
#28789 = FACE_OUTER_BOUND ( 'NONE', #29455, .T. ) ;
#28790 = CARTESIAN_POINT ( 'NONE',  ( 6.267877318470705905E-17, 1.929133858267716661, -1.850393700787401619 ) ) ;
#28791 = CARTESIAN_POINT ( 'NONE',  ( 0.1998031496062994128, -0.3460692066303957537, -2.058398950131233640 ) ) ;
#28792 = CARTESIAN_POINT ( 'NONE',  ( -1.253280839895012377, -0.2845877964562161244, -0.3641732283464567121 ) ) ;
#28793 = CARTESIAN_POINT ( 'NONE',  ( 0.1958661417322834775, 0.3392501089628018884, 0.02099737532808403431 ) ) ;
#28794 = CARTESIAN_POINT ( 'NONE',  ( 0.1640419947506569498, -0.3162353388693409650, -0.4822834645669289433 ) ) ;
#28796 = FACE_OUTER_BOUND ( 'NONE', #68835, .T. ) ;
#28795 = CARTESIAN_POINT ( 'NONE',  ( 1.496062992125985147, -0.1870078740157479769, 0.4822834645669291653 ) ) ;
#28797 = CARTESIAN_POINT ( 'NONE',  ( -1.292650918635170010, -0.5511811023622046335, 0.09757992244046803654 ) ) ;
#28798 = CARTESIAN_POINT ( 'NONE',  ( 0.6299212598425204535, -0.1870078740157480879, -0.4822834645669291653 ) ) ;
#28799 = CARTESIAN_POINT ( 'NONE',  ( 1.200787401574803681, -0.4536011799217368745, -0.2665933059059886201 ) ) ;
#28800 = CARTESIAN_POINT ( 'NONE',  ( 0.3392501089628018329, -0.1958661417322834497, -1.287382259021310427 ) ) ;
#28801 = CARTESIAN_POINT ( 'NONE',  ( -1.430446194225721390, -0.3690944881889763329, 0.3153832671262228327 ) ) ;
#28802 = CARTESIAN_POINT ( 'NONE',  ( 1.430446194225722500, -0.4281496062992127816, -0.4176697321401328100 ) ) ;
#28803 = CARTESIAN_POINT ( 'NONE',  ( 0.2570685524539542688, 1.875513320822418839, 0.1786727789893264307 ) ) ;
#28804 = CARTESIAN_POINT ( 'NONE',  ( -0.01312335958005186876, -0.4281496062992124485, 0.4176697321401328655 ) ) ;
#28805 = CARTESIAN_POINT ( 'NONE',  ( -1.259842519685038686, -0.1870078740157480601, -0.3641732283464567677 ) ) ;
#28806 = CARTESIAN_POINT ( 'NONE',  ( -0.4724409448818890911, -0.1870078740157479769, 0.3641732283464567677 ) ) ;
#28807 = CARTESIAN_POINT ( 'NONE',  ( -0.6627296587926503335, -0.6692913385826771977, 0.1292274648535927661 ) ) ;
#28808 = CARTESIAN_POINT ( 'NONE',  ( -1.391076115485563314, -0.5023911411419708095, -0.1820866141732282451 ) ) ;
#28809 = CARTESIAN_POINT ( 'NONE',  ( -9.594673741351313045E-17, 0.3917322834645670659, -0.4691794207687158269 ) ) ;
#28810 = CARTESIAN_POINT ( 'NONE',  ( 0.3215223097112867578, -0.05778040916215522460, 0.4822834645669289988 ) ) ;
#28811 = EDGE_CURVE ( 'NONE', #55851, #52658, #64690, .T. ) ;
#28812 = DIRECTION ( 'NONE',  ( 0.7071067811865376918, 0.000000000000000000, 0.7071067811865573427 ) ) ;
#28813 = CARTESIAN_POINT ( 'NONE',  ( 0.3458507752293908943, 0.3458507752293908943, -1.789370078740157410 ) ) ;
#28814 = CARTESIAN_POINT ( 'NONE',  ( -1.089238845144356427, 0.05413385826771666132, 0.4176697321401328100 ) ) ;
#28815 = CARTESIAN_POINT ( 'NONE',  ( -0.4068241469816267775, -0.004921259842519870586, -0.3153832671262229437 ) ) ;
#28816 = CARTESIAN_POINT ( 'NONE',  ( 0.1115485564304470323, 0.2952755905511811885, 0.1292274648535926551 ) ) ;
#28817 = CARTESIAN_POINT ( 'NONE',  ( 0.3937007874015754361, -0.1870078740157479769, 0.3641732283464567677 ) ) ;
#28818 = CARTESIAN_POINT ( 'NONE',  ( -0.5446194225721777693, -0.2845877964562161244, -0.3641732283464567121 ) ) ;
#28819 = CARTESIAN_POINT ( 'NONE',  ( -1.128608923884513837, -0.6046776061558807314, 0.2411417322834647770 ) ) ;
#28820 = CARTESIAN_POINT ( 'NONE',  ( -1.430446194225721390, -0.4281496062992124485, 0.4176697321401328655 ) ) ;
#28821 = EDGE_CURVE ( 'NONE', #50709, #19542, #40078, .T. ) ;
#28822 = CARTESIAN_POINT ( 'NONE',  ( 1.423884514435696413, -0.3162353388693409650, -0.4822834645669289433 ) ) ;
#28823 = DIRECTION ( 'NONE',  ( -0.000000000000000000, -1.000000000000000000, -0.000000000000000000 ) ) ;
#28824 = CARTESIAN_POINT ( 'NONE',  ( 1.049868766404200349, 0.1283753931104748280, 0.1820866141732283561 ) ) ;
#28825 = CARTESIAN_POINT ( 'NONE',  ( 0.9251968503937015864, 0.1660481256975883668, -0.3530559997133364547 ) ) ;
#28826 = LINE ( 'NONE', #5524, #52800 ) ;
#28827 = CARTESIAN_POINT ( 'NONE',  ( 1.456692913385827515, 0.1771653543307087630, 0.000000000000000000 ) ) ;
#28828 = ORIENTED_EDGE ( 'NONE', *, *, #46568, .F. ) ;
#28829 = CARTESIAN_POINT ( 'NONE',  ( -0.9120734908136475250, -0.6692913385826773087, -0.1292274648535924053 ) ) ;
#28830 = CARTESIAN_POINT ( 'NONE',  ( -1.003937007874014853, 0.1660481256975885056, 0.3530559997133364547 ) ) ;
#28831 = CARTESIAN_POINT ( 'NONE',  ( 0.3149606299212603933, -0.1870078740157479769, 0.4822834645669291653 ) ) ;
#28832 = CARTESIAN_POINT ( 'NONE',  ( -1.607611548556429737, -0.5511811023622046335, 0.09757992244046803654 ) ) ;
#28833 = CARTESIAN_POINT ( 'NONE',  ( 4.893765752498283308E-17, -0.3996062992125985480, -2.360236220472441193 ) ) ;
#28834 = CARTESIAN_POINT ( 'NONE',  ( 1.384514435695538337, -0.5511811023622046335, 0.09757992244046803654 ) ) ;
#28835 = CARTESIAN_POINT ( 'NONE',  ( 0.6167979002624679463, 0.05413385826771626580, -0.4176697321401330321 ) ) ;
#28836 = CARTESIAN_POINT ( 'NONE',  ( 0.9317585301837276734, -0.4281496062992124485, 0.4176697321401328655 ) ) ;
#28837 = CARTESIAN_POINT ( 'NONE',  ( -1.604771003085130099, 1.278209470906376932, -0.1466069496707745889 ) ) ;
#28838 = CARTESIAN_POINT ( 'NONE',  ( -0.3996062992125987146, 0.1070741851644051862, -1.922572178477689908 ) ) ;
#28839 = AXIS2_PLACEMENT_3D ( 'NONE', #34373, #4041, #41917 ) ;
#28840 = CARTESIAN_POINT ( 'NONE',  ( -0.2891555358219911054, 0.2891555358219909388, -1.122047244094488194 ) ) ;
#28841 = CARTESIAN_POINT ( 'NONE',  ( 0.3460692066303959202, 0.1998031496062993295, -2.335958005249343827 ) ) ;
#28842 = CARTESIAN_POINT ( 'NONE',  ( -0.4359958488159628165, 1.724409448818897905, -2.630268417803939940 ) ) ;
#28843 = CARTESIAN_POINT ( 'NONE',  ( -0.1049643490035301885, -0.3917322834645671215, -0.3792650918635169788 ) ) ;
#28844 = CARTESIAN_POINT ( 'NONE',  ( -0.2493438320209966919, -0.004921259842519870586, -0.3153832671262229437 ) ) ;
#28845 = CARTESIAN_POINT ( 'NONE',  ( -0.5052493438320203589, -0.6692913385826771977, 0.1292274648535927661 ) ) ;
#28846 = CARTESIAN_POINT ( 'NONE',  ( 1.056430446194226436, -0.6692913385826773087, -0.1292274648535924053 ) ) ;
#28847 = CARTESIAN_POINT ( 'NONE',  ( 4.837279021331061486E-17, -0.3949938075777409963, -2.202755905511811108 ) ) ;
#28848 = CARTESIAN_POINT ( 'NONE',  ( 0.1049868766404206816, 0.1283753931104748280, 0.1820866141732283561 ) ) ;
#28849 = CARTESIAN_POINT ( 'NONE',  ( -1.312335958005248715, 0.2306618581243848609, 0.2411417322834645549 ) ) ;
#28850 = CARTESIAN_POINT ( 'NONE',  ( 1.259842519685040019, -0.1870078740157479769, 0.4822834645669291653 ) ) ;
#28851 = CARTESIAN_POINT ( 'NONE',  ( 0.4724409448818897572, -0.1265901696524988906, -2.473753280839894764 ) ) ;
#28852 = CARTESIAN_POINT ( 'NONE',  ( -0.1998031496062994683, 0.3460692066303958092, -1.902887139107611647 ) ) ;
#28853 = CARTESIAN_POINT ( 'NONE',  ( 0.5314960629921395840, 2.677165354330708791, -3.900966923095588346 ) ) ;
#28854 = ORIENTED_EDGE ( 'NONE', *, *, #26244, .F. ) ;
#28855 = ORIENTED_EDGE ( 'NONE', *, *, #59902, .F. ) ;
#28856 = CARTESIAN_POINT ( 'NONE',  ( 1.194225721784777594, -0.4281496062992127816, -0.4176697321401328100 ) ) ;
#28857 = CARTESIAN_POINT ( 'NONE',  ( -1.509186351706035767, 0.05413385826771626580, -0.4176697321401330321 ) ) ;
#28859 = CARTESIAN_POINT ( 'NONE',  ( 1.502624671916010790, -0.3162353388693409650, -0.4822834645669289433 ) ) ;
#28858 = CARTESIAN_POINT ( 'NONE',  ( -1.227034120734907141, -0.5511811023622048555, -0.09757992244046775898 ) ) ;
#28860 = CARTESIAN_POINT ( 'NONE',  ( 0.2867679344610365999, -0.2867679344610365444, 0.1318897637795274913 ) ) ;
#28861 = CARTESIAN_POINT ( 'NONE',  ( -1.011202504342156416, -2.294479370626195693E-15, 0.3464511005275217603 ) ) ;
#28862 = CARTESIAN_POINT ( 'NONE',  ( 1.259842519685040019, -0.1870078740157480879, -0.4822834645669291653 ) ) ;
#28863 = CARTESIAN_POINT ( 'NONE',  ( 0.4724409448818898682, 2.892866454678787531E-17, -2.480314960629921295 ) ) ;
#28864 = CARTESIAN_POINT ( 'NONE',  ( -0.1509186351706028884, -0.05778040916215522460, 0.4822834645669289988 ) ) ;
#28865 = CARTESIAN_POINT ( 'NONE',  ( -0.5511811023622041894, -0.1870078740157480879, -0.4822834645669291653 ) ) ;
#28866 = CARTESIAN_POINT ( 'NONE',  ( 1.482939632545932307, 0.05413385826771626580, -0.4176697321401330321 ) ) ;
#28867 = CARTESIAN_POINT ( 'NONE',  ( 0.3392501089628018329, 0.1958661417322835607, -0.05839895013123368173 ) ) ;
#28868 = CARTESIAN_POINT ( 'NONE',  ( 0.4002624671916016896, -0.3162353388693409650, -0.4822834645669289433 ) ) ;
#28869 = CARTESIAN_POINT ( 'NONE',  ( 0.2867679344610365999, 0.2867679344610365999, -2.334645669291338432 ) ) ;
#28870 = CARTESIAN_POINT ( 'NONE',  ( -1.187664041994749731, -0.2845877964562159024, 0.3641732283464567677 ) ) ;
#28871 = VERTEX_POINT ( 'NONE', #45314 ) ;
#28872 = CARTESIAN_POINT ( 'NONE',  ( 0.2891555358219910499, -0.2891555358219909944, -2.460629921259842590 ) ) ;
#28873 = ORIENTED_EDGE ( 'NONE', *, *, #38110, .F. ) ;
#28874 = CARTESIAN_POINT ( 'NONE',  ( -1.637380676922836731, 1.357125752008925268, 0.4389107506287909244 ) ) ;
#28875 = CARTESIAN_POINT ( 'NONE',  ( -1.601049868766403650, -0.6046776061558807314, 0.2411417322834647770 ) ) ;
#28876 = CARTESIAN_POINT ( 'NONE',  ( -0.3460692066303958092, -0.1998031496062994683, -1.154855643044619518 ) ) ;
#28877 = CARTESIAN_POINT ( 'NONE',  ( -0.7874015748031497619, 1.968503937007873850, 0.000000000000000000 ) ) ;
#28878 = CARTESIAN_POINT ( 'NONE',  ( 1.016821367227983774, 1.553403318890016704, -0.4744094488188971281 ) ) ;
#28879 = CARTESIAN_POINT ( 'NONE',  ( 0.4133858267716541968, 0.1660481256975885056, 0.3530559997133364547 ) ) ;
#28880 = FACE_OUTER_BOUND ( 'NONE', #81084, .T. ) ;
#28881 = CARTESIAN_POINT ( 'NONE',  ( -0.3917322834645669549, -0.1049643490035306603, -0.1305774278215224293 ) ) ;
#28882 =( BOUNDED_SURFACE ( )  B_SPLINE_SURFACE ( 1, 2, ( 
 ( #78645, #7933, #26857, #78224, #45369, #20136, #51675, #782, #26443, #64326, #20968, #33594, #45784, #71483, #66005, #1616, #7513, #33181, #14669, #6662, #32334, #57996, #360, #26017, #42378, #10421, #10000, #21790, #54178, #61329, #15077, #80715, #73571, #35254, #15916, #23030, #67253, #47867, #16738, #74394, #48282, #9585, #47037, #73980, #3269, #40735, #66419, #53763, #61750, #22623, #29755, #8755, #60096, #9176, #34847, #80308, #55007, #16326, #67663, #48696, #28109, #79892, #41970, #60918, #72731, #47452, #2451, #34431, #81125, #79474, #68077, #73147, #60510, #29348, #66842, #15496, #35665, #4087, #41154, #36079, #54599, #55418, #3683, #28930, #2858, #28522, #22210, #41564, #5729, #82356, #62990, #5329, #81538, #4918, #4500, #49524, #23857, #57479, #57065, #37317, #30586, #43194, #18781, #24674, #56252, #75632, #56655, #17970, #12470, #42790, #70119, #63806, #44424, #38132, #69718, #75217, #81948, #37720, #74812, #82759, #49934, #11659, #43607, #24261, #63394, #17157, #6145, #31400, #69309, #36900, #31819, #68485, #10824, #36484, #30987, #17562, #25080, #62159, #30167, #50754, #23442, #68890, #50342, #76039, #18384, #49106, #44025, #55830, #11240, #12062, #62576, #76454, #260, #38960, #19187, #38549, #76854, #7831, #59160, #33498, #72223, #46524, #1518, #13728, #1105, #83173, #65908, #51159, #57893, #58315, #14574, #64229, #25912, #51572, #77275, #32235, #6563, #19605, #14152, #65067, #26756, #71799, #45267, #70963, #65499, #45682, #46106, #52411, #13308, #58743, #39808, #27172, #39382, #71378, #64644, #52834, #6981, #51996, #680, #78120, #32650, #20453, #26335, #77701, #78546, #20871, #40226, #44836, #20031, #7405, #8245, #33910, #33076, #25493, #70534, #12890, #41471, #81334, #62363, #81749, #40638, #55625, #56041, #49319, #75427, #23648, #17769, #69100, #4701, #30374, #66320, #54081, #15822, #78965, #21284, #46939, #11031, #2351, #29960, #4297, #34751, #79796, #8659, #67156, #36688, #11448, #72631, #14979, #53253, #34330, #60820, #75020, #9485, #41056, #17366, #66744, #59995, #43401, #59574, #42994, #24060, #49729, #28007, #35160, #53667, #68689, #79374, #1930, #21693, #47356, #27593, #73045, #9080, #15394, #60411, #2762, #28421, #22112, #47772, #73473, #70328, #77492, #45477, #44225, #12269, #31610, #50955, #57689, #71174, #77069, #6771, #64436, #38342, #57271, #37104, #64017, #76652, #30790, #5123, #43810, #51788, #12684, #19827, #56454, #50138, #82558, #24876, #6358, #45053, #32030, #51, #13105, #18177, #69915, #25705, #82969, #62789, #11863, #75836, #82156, #24471, #69514, #38759, #37516, #50544, #19402, #56861, #63191, #51365, #5531, #31195, #32443, #44632, #26127, #70754, #25287, #58105, #471, #76248, #18582, #37927, #63604, #18984, #5940, #71591, #78336, #77914, #39600, #13943, #47567, #47150, #27383, #20667, #33299, #8864, #72431, #46320, #65714, #46739, #8045, #2558, #32866, #60208, #53875, #34542, #28216, #59784, #65289, #72013, #27806, #64856, #72841, #40026, #1726, #33707, #14369, #53466, #7194, #79590, #79175, #59368, #26966, #21905, #58534, #900, #26557, #53044, #7627, #21491, #52210, #20245, #15190, #13515, #58960, #78756, #40437, #21081, #39172, #34123, #45894, #1317, #14781, #52631, #66117, #8452, #2138, #40847, #66533, #66954, #81234, #49218, #23550, #62267, #36589, #74924, #17269, #10116, #74092, #42897, #23965, #4604, #68193, #23139, #30276, #48808, #55939, #81654, #80422, #48392, #67778, #3794, #10531, #73260, #29863, #68591, #29458, #74507, #15609, #41268, #9286, #47986, #16438, #34957, #54294, #73685, #16025, #41672, #22322, #80009, #67364, #4199, #55116, #16854, #61858, #9697, #35367, #55525, #35778, #36186, #42489, #61032, #10932, #60620, #2970, #80825, #61447, #3382, #28636, #54715, #42083, #29044, #22733, #31098, #44538, #5029, #75739, #19301, #50861, #51269, #43302, #82464, #24780, #76971, #70649, #82060, #50044, #57593, #50448, #31515, #70229, #44953, #13004, #30697, #12584, #38660, #38242, #64337, #63919, #6674, #58007, #32346, #372, #56361, #44133, #5840, #69000, #11351, #37009, #83283, #18080, #18889 ),
 ( #56765, #6254, #76150, #24373, #49632, #75325, #76561, #17671, #62687, #43715, #25195, #69417, #31931, #11772, #25606, #37425, #63098, #5437, #18490, #69825, #12174, #37832, #63510, #57173, #82871, #20977, #64756, #52107, #79076, #27282, #27702, #19721, #58861, #1218, #53366, #47048, #58432, #26455, #34021, #26867, #7944, #46637, #21392, #72740, #7095, #72332, #15087, #14680, #40745, #40337, #66429, #34439, #8764, #60106, #32765, #20568, #65613, #45379, #71076, #13418, #59681, #77815, #78656, #52942, #52528, #46219, #794, #33605, #2037, #26027, #39075, #20146, #45795, #71493, #66017, #8353, #59268, #7523, #51687, #33193, #13841, #77390, #39499, #65187, #78235, #71915, #14265, #1625, #39924, #16337, #9184, #29358, #60518, #66852, #67674, #29766, #73579, #2867, #61760, #2459, #36089, #35675, #73990, #10432, #41980, #4098, #28117, #41572, #9595, #3278, #22632, #61340, #53772, #23040, #68087, #48293, #10010, #79484, #21798, #15504, #54187, #28942, #47462, #28530, #79902, #47875, #15925, #22219, #67262, #35263, #74405, #3693, #55017, #48707, #60928, #54608, #42388, #80726, #16749, #73154, #80317, #41162, #34856, #27975, #33877, #40194, #20421, #53633, #59128, #46489, #8627, #59543, #78928, #66288, #1074, #78090, #59959, #65877, #40605, #21250, #46074, #53217, #34298, #79341, #1898, #8212, #71766, #21661, #1485, #72184, #78513, #46905, #27139, #72600, #33040, #14120, #47321, #14946, #73012, #71348, #52803, #20836, #15363, #41024, #26727, #39772, #2314, #14542, #27559, #66710, #9043, #34717, #58709, #60378, #2726, #28387, #77672, #20002, #45653, #13695, #39350, #65035, #52381, #7371, #65467, #7801, #33466, #73964, #22607, #55814, #81109, #68062, #69292, #48267, #16310, #41954, #42774, #23014, #62561, #67648, #61314, #4900, #37300, #74378, #36063, #81522, #4072, #43591, #75202, #3669, #9983, #17142, #16721, #80701, #54993, #10406, #35651, #29332, #48682, #30571, #56237, #81934, #11642, #17954, #24245, #49918, #74794, #55402, #75616, #62974, #23842, #68470, #54583, #49509, #10808, #42362, #61735, #29739, #5313, #30152, #80293, #23426, #49091, #36468, #62143, #4482, #17546, #43178, #68875, #11224, #36883, #63787, #6545, #51141, #30971, #5712, #69702, #76835, #77256, #57874, #82741, #32215, #19586, #64623, #70514, #19169, #57047, #6960, #12452, #83154, #31801, #241, #38113, #25893, #12045, #25062, #659, #51553, #32631, #24657, #6126, #57461, #58294, #51976, #63376, #31382, #38942, #25474, #12871, #45248, #26315, #77681, #37703, #70945, #20011, #13290, #45662, #71358, #13705, #39360, #65045, #56638, #50735, #44817, #38530, #50325, #76023, #18367, #64211, #82339, #44008, #76434, #18763, #44406, #70100, #46915, #41033, #41446, #52390, #26736, #1084, #78099, #8636, #79352, #72609, #72199, #47332, #14552, #65478, #47747, #7382, #34307, #9055, #54056, #14130, #66297, #39783, #59968, #7810, #73022, #33476, #59138, #2328, #33050, #40203, #1496, #73446, #58721, #79771, #27984, #40614, #22087, #53644, #15796, #20430, #65887, #8222, #1907, #21261, #21671, #46083, #15372, #60387, #14957, #66719, #71776, #27148, #52812, #78522, #33886, #20846, #46499, #59552, #27568, #53227, #78943, #34728, #2738, #28398, #48994, #68376, #55713, #73863, #67543, #49411, #4383, #42262, #3977, #48168, #23324, #17451, #17857, #28814, #3150, #60796, #54478, #10715, #81423, #74693, #48579, #23738, #74276, #41851, #24148, #67130, #36372, #68778, #30468, #16204, #42678, #9878, #62046, #35547, #75104, #61210, #3565, #30051, #9460, #16620, #29232, #49818, #35134, #56132, #43081, #17038, #81837, #11122, #75518, #80190, #67958, #10300, #61636, #81010, #36779, #22507, #62455, #4791, #54896, #80602, #22911, #35966, #29641, #55302, #18668, #32532, #24562, #18264, #69603, #11949, #75924, #50228, #43905, #57777, #25379, #44721, #32119, #37604, #63278, #25796, #6031, #6449, #70419, #5619, #19073, #140, #77159, #83057, #31703, #31285, #19491, #24962, #12358, #44313, #12774, #50633, #38431, #82243, #56950, #13199, #64114, #45145, #37195, #76338, #70003, #70848, #64526, #82647, #38016, #51456, #63692, #51042 ) ),
 .UNSPECIFIED., .F., .F., .F. ) 
 B_SPLINE_SURFACE_WITH_KNOTS ( ( 2, 2 ),
 ( 3, 2, 2, 2, 2, 2, 2, 2, 2, 2, 2, 2, 2, 2, 2, 2, 2, 2, 2, 2, 2, 2, 2, 2, 2, 2, 2, 2, 2, 2, 2, 2, 2, 2, 2, 2, 2, 2, 2, 2, 2, 2, 2, 2, 2, 2, 2, 2, 2, 2, 2, 2, 2, 2, 2, 2, 2, 2, 2, 2, 2, 2, 2, 2, 2, 2, 2, 2, 2, 2, 2, 2, 2, 2, 2, 2, 2, 2, 2, 2, 2, 2, 2, 2, 2, 2, 2, 2, 2, 2, 2, 2, 2, 2, 2, 2, 2, 2, 2, 2, 2, 2, 2, 2, 2, 2, 2, 2, 2, 2, 2, 2, 2, 2, 2, 2, 2, 2, 2, 2, 2, 2, 2, 2, 2, 2, 2, 2, 2, 2, 2, 2, 2, 2, 2, 2, 2, 2, 2, 2, 2, 2, 2, 2, 2, 2, 2, 2, 2, 2, 2, 2, 2, 2, 2, 2, 2, 2, 2, 2, 2, 2, 2, 2, 2, 2, 2, 2, 2, 2, 2, 2, 2, 2, 2, 2, 2, 2, 2, 2, 2, 2, 2, 2, 2, 2, 2, 2, 2, 2, 2, 2, 2, 2, 2, 2, 2, 2, 2, 2, 2, 2, 2, 2, 2, 2, 2, 2, 2, 2, 2, 2, 2, 2, 2, 2, 2, 2, 2, 2, 2, 2, 2, 2, 2, 2, 2, 2, 2, 2, 2, 2, 2, 2, 2, 2, 2, 2, 2, 2, 2, 2, 2, 2, 2, 2, 2, 2, 2, 2, 2, 2, 2, 2, 2, 3 ),
 ( 0.000000000000000000, 1.000000000000000000 ),
 ( 0.000000000000000000, 0.003787878787878787984, 0.007575757575757575968, 0.01136363636363636395, 0.01515151515151515194, 0.01893939393939393992, 0.02272727272727272790, 0.02651515151515151589, 0.03030303030303030387, 0.03409090909090908839, 0.03787878787878787984, 0.04166666666666666435, 0.04545454545454545581, 0.04924242424242424032, 0.05303030303030303177, 0.05681818181818181629, 0.06060606060606060774, 0.06439393939393939226, 0.06818181818181817677, 0.07196969696969697516, 0.07575757575757575968, 0.07954545454545454419, 0.08333333333333332871, 0.08712121212121212710, 0.09090909090909091161, 0.09469696969696969613, 0.09848484848484848064, 0.1022727272727272790, 0.1060606060606060635, 0.1098484848484848481, 0.1136363636363636326, 0.1174242424242424310, 0.1212121212121212155, 0.1250000000000000000, 0.1287878787878787845, 0.1325757575757575690, 0.1363636363636363535, 0.1401515151515151381, 0.1439393939393939503, 0.1477272727272727348, 0.1515151515151515194, 0.1553030303030303039, 0.1590909090909090884, 0.1628787878787878729, 0.1666666666666666574, 0.1704545454545454419, 0.1742424242424242542, 0.1780303030303030387, 0.1818181818181818232, 0.1856060606060606077, 0.1893939393939393923, 0.1931818181818181768, 0.1969696969696969613, 0.2007575757575757458, 0.2045454545454545581, 0.2083333333333333426, 0.2121212121212121271, 0.2159090909090909116, 0.2196969696969696961, 0.2234848484848484806, 0.2272727272727272652, 0.2310606060606060497, 0.2348484848484848619, 0.2386363636363636465, 0.2424242424242424310, 0.2462121212121212155, 0.2500000000000000000, 0.2537878787878787845, 0.2575757575757575690, 0.2613636363636363535, 0.2651515151515151381, 0.2689393939393939226, 0.2727272727272727071, 0.2765151515151514916, 0.2803030303030302761, 0.2840909090909091161, 0.2878787878787879007, 0.2916666666666666852, 0.2954545454545454697, 0.2992424242424242542, 0.3030303030303030387, 0.3068181818181818232, 0.3106060606060606077, 0.3143939393939393923, 0.3181818181818181768, 0.3219696969696969613, 0.3257575757575757458, 0.3295454545454545303, 0.3333333333333333148, 0.3371212121212120993, 0.3409090909090908839, 0.3446969696969697239, 0.3484848484848485084, 0.3522727272727272929, 0.3560606060606060774, 0.3598484848484848619, 0.3636363636363636465, 0.3674242424242424310, 0.3712121212121212155, 0.3750000000000000000, 0.3787878787878787845, 0.3825757575757575690, 0.3863636363636363535, 0.3901515151515151381, 0.3939393939393939226, 0.3977272727272727071, 0.4015151515151514916, 0.4053030303030302761, 0.4090909090909091161, 0.4128787878787879007, 0.4166666666666666852, 0.4204545454545454697, 0.4242424242424242542, 0.4280303030303030387, 0.4318181818181818232, 0.4356060606060606077, 0.4393939393939393923, 0.4431818181818181768, 0.4469696969696969613, 0.4507575757575757458, 0.4545454545454545303, 0.4583333333333333148, 0.4621212121212120993, 0.4659090909090908839, 0.4696969696969697239, 0.4734848484848485084, 0.4772727272727272929, 0.4810606060606060774, 0.4848484848484848619, 0.4886363636363636465, 0.4924242424242424310, 0.4962121212121212155, 0.5000000000000000000, 0.5037878787878787845, 0.5075757575757575690, 0.5113636363636363535, 0.5151515151515151381, 0.5189393939393939226, 0.5227272727272727071, 0.5265151515151514916, 0.5303030303030302761, 0.5340909090909090606, 0.5378787878787878451, 0.5416666666666666297, 0.5454545454545454142, 0.5492424242424241987, 0.5530303030303029832, 0.5568181818181817677, 0.5606060606060605522, 0.5643939393939394478, 0.5681818181818182323, 0.5719696969696970168, 0.5757575757575758013, 0.5795454545454545858, 0.5833333333333333703, 0.5871212121212121549, 0.5909090909090909394, 0.5946969696969697239, 0.5984848484848485084, 0.6022727272727272929, 0.6060606060606060774, 0.6098484848484848619, 0.6136363636363636465, 0.6174242424242424310, 0.6212121212121212155, 0.6250000000000000000, 0.6287878787878787845, 0.6325757575757575690, 0.6363636363636363535, 0.6401515151515151381, 0.6439393939393939226, 0.6477272727272727071, 0.6515151515151514916, 0.6553030303030302761, 0.6590909090909090606, 0.6628787878787878451, 0.6666666666666666297, 0.6704545454545454142, 0.6742424242424241987, 0.6780303030303029832, 0.6818181818181817677, 0.6856060606060605522, 0.6893939393939394478, 0.6931818181818182323, 0.6969696969696970168, 0.7007575757575758013, 0.7045454545454545858, 0.7083333333333333703, 0.7121212121212121549, 0.7159090909090909394, 0.7196969696969697239, 0.7234848484848485084, 0.7272727272727272929, 0.7310606060606060774, 0.7348484848484848619, 0.7386363636363636465, 0.7424242424242424310, 0.7462121212121212155, 0.7500000000000000000, 0.7537878787878787845, 0.7575757575757575690, 0.7613636363636363535, 0.7651515151515151381, 0.7689393939393939226, 0.7727272727272727071, 0.7765151515151514916, 0.7803030303030302761, 0.7840909090909090606, 0.7878787878787878451, 0.7916666666666666297, 0.7954545454545454142, 0.7992424242424241987, 0.8030303030303029832, 0.8068181818181817677, 0.8106060606060605522, 0.8143939393939394478, 0.8181818181818182323, 0.8219696969696970168, 0.8257575757575758013, 0.8295454545454545858, 0.8333333333333333703, 0.8371212121212121549, 0.8409090909090909394, 0.8446969696969697239, 0.8484848484848485084, 0.8522727272727272929, 0.8560606060606060774, 0.8598484848484848619, 0.8636363636363636465, 0.8674242424242424310, 0.8712121212121212155, 0.8750000000000000000, 0.8787878787878787845, 0.8825757575757575690, 0.8863636363636363535, 0.8901515151515151381, 0.8939393939393939226, 0.8977272727272727071, 0.9015151515151514916, 0.9053030303030302761, 0.9090909090909090606, 0.9128787878787878451, 0.9166666666666666297, 0.9204545454545454142, 0.9242424242424241987, 0.9280303030303029832, 0.9318181818181817677, 0.9356060606060605522, 0.9393939393939394478, 0.9431818181818182323, 0.9469696969696970168, 0.9507575757575758013, 0.9545454545454545858, 0.9583333333333333703, 0.9621212121212121549, 0.9659090909090909394 ),
 .UNSPECIFIED. ) 
 GEOMETRIC_REPRESENTATION_ITEM ( )  RATIONAL_B_SPLINE_SURFACE ( (
 ( 1.000000000000000000, 0.9659258262890683122, 1.000000000000000000, 0.9659258262890683122, 1.000000000000000000, 0.9659258262890683122, 1.000000000000000000, 0.9659258262890683122, 1.000000000000000000, 0.9659258262890683122, 1.000000000000000000, 0.9659258262890683122, 1.000000000000000000, 0.9659258262890683122, 1.000000000000000000, 0.9659258262890683122, 1.000000000000000000, 0.9659258262890683122, 1.000000000000000000, 0.9659258262890683122, 1.000000000000000000, 0.9659258262890683122, 1.000000000000000000, 0.9659258262890683122, 1.000000000000000000, 0.9659258262890683122, 1.000000000000000000, 0.9659258262890683122, 1.000000000000000000, 0.9659258262890683122, 1.000000000000000000, 0.9659258262890683122, 1.000000000000000000, 0.9659258262890683122, 1.000000000000000000, 0.9659258262890683122, 1.000000000000000000, 0.9659258262890683122, 1.000000000000000000, 0.9659258262890683122, 1.000000000000000000, 0.9659258262890683122, 1.000000000000000000, 0.9659258262890683122, 1.000000000000000000, 0.9659258262890683122, 1.000000000000000000, 0.9659258262890683122, 1.000000000000000000, 0.9659258262890683122, 1.000000000000000000, 0.9659258262890683122, 1.000000000000000000, 0.9659258262890683122, 1.000000000000000000, 0.9659258262890683122, 1.000000000000000000, 0.9659258262890683122, 1.000000000000000000, 0.9659258262890683122, 1.000000000000000000, 0.9659258262890683122, 1.000000000000000000, 0.9659258262890683122, 1.000000000000000000, 0.9659258262890683122, 1.000000000000000000, 0.9659258262890683122, 1.000000000000000000, 0.9659258262890683122, 1.000000000000000000, 0.9659258262890683122, 1.000000000000000000, 0.9659258262890683122, 1.000000000000000000, 0.9659258262890683122, 1.000000000000000000, 0.9659258262890683122, 1.000000000000000000, 0.9659258262890683122, 1.000000000000000000, 0.9659258262890683122, 1.000000000000000000, 0.9659258262890683122, 1.000000000000000000, 0.9659258262890683122, 1.000000000000000000, 0.9659258262890683122, 1.000000000000000000, 0.9659258262890683122, 1.000000000000000000, 0.9659258262890683122, 1.000000000000000000, 0.9659258262890683122, 1.000000000000000000, 0.9659258262890683122, 1.000000000000000000, 0.9659258262890683122, 1.000000000000000000, 0.9659258262890683122, 1.000000000000000000, 0.9659258262890683122, 1.000000000000000000, 0.9659258262890683122, 1.000000000000000000, 0.9659258262890683122, 1.000000000000000000, 0.9659258262890683122, 1.000000000000000000, 0.9659258262890683122, 1.000000000000000000, 0.9659258262890683122, 1.000000000000000000, 0.9659258262890683122, 1.000000000000000000, 0.9659258262890683122, 1.000000000000000000, 0.9659258262890683122, 1.000000000000000000, 0.9659258262890683122, 1.000000000000000000, 0.9659258262890683122, 1.000000000000000000, 0.9659258262890683122, 1.000000000000000000, 0.9659258262890683122, 1.000000000000000000, 0.9659258262890683122, 1.000000000000000000, 0.9659258262890683122, 1.000000000000000000, 0.9659258262890683122, 1.000000000000000000, 0.9659258262890683122, 1.000000000000000000, 0.9659258262890683122, 1.000000000000000000, 0.9659258262890683122, 1.000000000000000000, 0.9659258262890683122, 1.000000000000000000, 0.9659258262890683122, 1.000000000000000000, 0.9659258262890683122, 1.000000000000000000, 0.9659258262890683122, 1.000000000000000000, 0.9659258262890683122, 1.000000000000000000, 0.9659258262890683122, 1.000000000000000000, 0.9659258262890683122, 1.000000000000000000, 0.9659258262890683122, 1.000000000000000000, 0.9659258262890683122, 1.000000000000000000, 0.9659258262890683122, 1.000000000000000000, 0.9659258262890683122, 1.000000000000000000, 0.9659258262890683122, 1.000000000000000000, 0.9659258262890683122, 1.000000000000000000, 0.9659258262890683122, 1.000000000000000000, 0.9659258262890683122, 1.000000000000000000, 0.9659258262890683122, 1.000000000000000000, 0.9659258262890683122, 1.000000000000000000, 0.9659258262890683122, 1.000000000000000000, 0.9659258262890683122, 1.000000000000000000, 0.9659258262890683122, 1.000000000000000000, 0.9659258262890683122, 1.000000000000000000, 0.9659258262890683122, 1.000000000000000000, 0.9659258262890683122, 1.000000000000000000, 0.9659258262890683122, 1.000000000000000000, 0.9659258262890683122, 1.000000000000000000, 0.9659258262890683122, 1.000000000000000000, 0.9659258262890683122, 1.000000000000000000, 0.9659258262890683122, 1.000000000000000000, 0.9659258262890683122, 1.000000000000000000, 0.9659258262890683122, 1.000000000000000000, 0.9659258262890683122, 1.000000000000000000, 0.9659258262890683122, 1.000000000000000000, 0.9659258262890683122, 1.000000000000000000, 0.9659258262890683122, 1.000000000000000000, 0.9659258262890683122, 1.000000000000000000, 0.9659258262890683122, 1.000000000000000000, 0.9659258262890683122, 1.000000000000000000, 0.9659258262890683122, 1.000000000000000000, 0.9659258262890683122, 1.000000000000000000, 0.9659258262890683122, 1.000000000000000000, 0.9659258262890683122, 1.000000000000000000, 0.9659258262890683122, 1.000000000000000000, 0.9659258262890683122, 1.000000000000000000, 0.9659258262890683122, 1.000000000000000000, 0.9659258262890683122, 1.000000000000000000, 0.9659258262890683122, 1.000000000000000000, 0.9659258262890683122, 1.000000000000000000, 0.9659258262890683122, 1.000000000000000000, 0.9659258262890683122, 1.000000000000000000, 0.9659258262890683122, 1.000000000000000000, 0.9659258262890683122, 1.000000000000000000, 0.9659258262890683122, 1.000000000000000000, 0.9659258262890683122, 1.000000000000000000, 0.9659258262890683122, 1.000000000000000000, 0.9659258262890683122, 1.000000000000000000, 0.9659258262890683122, 1.000000000000000000, 0.9659258262890683122, 1.000000000000000000, 0.9659258262890683122, 1.000000000000000000, 0.9659258262890683122, 1.000000000000000000, 0.9659258262890683122, 1.000000000000000000, 0.9659258262890683122, 1.000000000000000000, 0.9659258262890683122, 1.000000000000000000, 0.9659258262890683122, 1.000000000000000000, 0.9659258262890683122, 1.000000000000000000, 0.9659258262890683122, 1.000000000000000000, 0.9659258262890683122, 1.000000000000000000, 0.9659258262890683122, 1.000000000000000000, 0.9659258262890683122, 1.000000000000000000, 0.9659258262890683122, 1.000000000000000000, 0.9659258262890683122, 1.000000000000000000, 0.9659258262890683122, 1.000000000000000000, 0.9659258262890683122, 1.000000000000000000, 0.9659258262890683122, 1.000000000000000000, 0.9659258262890683122, 1.000000000000000000, 0.9659258262890683122, 1.000000000000000000, 0.9659258262890683122, 1.000000000000000000, 0.9659258262890683122, 1.000000000000000000, 0.9659258262890683122, 1.000000000000000000, 0.9659258262890683122, 1.000000000000000000, 0.9659258262890683122, 1.000000000000000000, 0.9659258262890683122, 1.000000000000000000, 0.9659258262890683122, 1.000000000000000000, 0.9659258262890683122, 1.000000000000000000, 0.9659258262890683122, 1.000000000000000000, 0.9659258262890683122, 1.000000000000000000, 0.9659258262890683122, 1.000000000000000000, 0.9659258262890683122, 1.000000000000000000, 0.9659258262890683122, 1.000000000000000000, 0.9659258262890683122, 1.000000000000000000, 0.9659258262890683122, 1.000000000000000000, 0.9659258262890683122, 1.000000000000000000, 0.9659258262890683122, 1.000000000000000000, 0.9659258262890683122, 1.000000000000000000, 0.9659258262890683122, 1.000000000000000000, 0.9659258262890683122, 1.000000000000000000, 0.9659258262890683122, 1.000000000000000000, 0.9659258262890683122, 1.000000000000000000, 0.9659258262890683122, 1.000000000000000000, 0.9659258262890683122, 1.000000000000000000, 0.9659258262890683122, 1.000000000000000000, 0.9659258262890683122, 1.000000000000000000, 0.9659258262890683122, 1.000000000000000000, 0.9659258262890683122, 1.000000000000000000, 0.9659258262890683122, 1.000000000000000000, 0.9659258262890683122, 1.000000000000000000, 0.9659258262890683122, 1.000000000000000000, 0.9659258262890683122, 1.000000000000000000, 0.9659258262890683122, 1.000000000000000000, 0.9659258262890683122, 1.000000000000000000, 0.9659258262890683122, 1.000000000000000000, 0.9659258262890683122, 1.000000000000000000, 0.9659258262890683122, 1.000000000000000000, 0.9659258262890683122, 1.000000000000000000, 0.9659258262890683122, 1.000000000000000000, 0.9659258262890683122, 1.000000000000000000, 0.9659258262890683122, 1.000000000000000000, 0.9659258262890683122, 1.000000000000000000, 0.9659258262890683122, 1.000000000000000000, 0.9659258262890683122, 1.000000000000000000, 0.9659258262890683122, 1.000000000000000000, 0.9659258262890683122, 1.000000000000000000, 0.9659258262890683122, 1.000000000000000000, 0.9659258262890683122, 1.000000000000000000, 0.9659258262890683122, 1.000000000000000000, 0.9659258262890683122, 1.000000000000000000, 0.9659258262890683122, 1.000000000000000000, 0.9659258262890683122, 1.000000000000000000, 0.9659258262890683122, 1.000000000000000000, 0.9659258262890683122, 1.000000000000000000, 0.9659258262890683122, 1.000000000000000000, 0.9659258262890683122, 1.000000000000000000, 0.9659258262890683122, 1.000000000000000000, 0.9659258262890683122, 1.000000000000000000, 0.9659258262890683122, 1.000000000000000000, 0.9659258262890683122, 1.000000000000000000, 0.9659258262890683122, 1.000000000000000000, 0.9659258262890683122, 1.000000000000000000, 0.9659258262890683122, 1.000000000000000000, 0.9659258262890683122, 1.000000000000000000, 0.9659258262890683122, 1.000000000000000000, 0.9659258262890683122, 1.000000000000000000, 0.9659258262890683122, 1.000000000000000000, 0.9659258262890683122, 1.000000000000000000, 0.9659258262890683122, 1.000000000000000000, 0.9659258262890683122, 1.000000000000000000, 0.9659258262890683122, 1.000000000000000000, 0.9659258262890683122, 1.000000000000000000, 0.9659258262890683122, 1.000000000000000000, 0.9659258262890683122, 1.000000000000000000, 0.9659258262890683122, 1.000000000000000000, 0.9659258262890683122, 1.000000000000000000, 0.9659258262890683122, 1.000000000000000000, 0.9659258262890683122, 1.000000000000000000, 0.9659258262890683122, 1.000000000000000000, 0.9659258262890683122, 1.000000000000000000, 0.9659258262890683122, 1.000000000000000000, 0.9659258262890683122, 1.000000000000000000, 0.9659258262890683122, 1.000000000000000000, 0.9659258262890683122, 1.000000000000000000, 0.9659258262890683122, 1.000000000000000000, 0.9659258262890683122, 1.000000000000000000, 0.9659258262890683122, 1.000000000000000000, 0.9659258262890683122, 1.000000000000000000, 0.9659258262890683122, 1.000000000000000000, 0.9659258262890683122, 1.000000000000000000, 0.9659258262890683122, 1.000000000000000000, 0.9659258262890683122, 1.000000000000000000, 0.9659258262890683122, 1.000000000000000000, 0.9659258262890683122, 1.000000000000000000, 0.9659258262890683122, 1.000000000000000000, 0.9659258262890683122, 1.000000000000000000, 0.9659258262890683122, 1.000000000000000000, 0.9659258262890683122, 1.000000000000000000, 0.9659258262890683122, 1.000000000000000000, 0.9659258262890683122, 1.000000000000000000, 0.9659258262890683122, 1.000000000000000000, 0.9659258262890683122, 1.000000000000000000, 0.9659258262890683122, 1.000000000000000000, 0.9659258262890683122, 1.000000000000000000, 0.9659258262890683122, 1.000000000000000000, 0.9659258262890683122, 1.000000000000000000, 0.9659258262890683122, 1.000000000000000000, 0.9659258262890683122, 1.000000000000000000, 0.9659258262890683122, 1.000000000000000000, 0.9659258262890683122, 1.000000000000000000, 0.9659258262890683122, 1.000000000000000000),
 ( 1.000000000000000000, 0.9659258262890683122, 1.000000000000000000, 0.9659258262890683122, 1.000000000000000000, 0.9659258262890683122, 1.000000000000000000, 0.9659258262890683122, 1.000000000000000000, 0.9659258262890683122, 1.000000000000000000, 0.9659258262890683122, 1.000000000000000000, 0.9659258262890683122, 1.000000000000000000, 0.9659258262890683122, 1.000000000000000000, 0.9659258262890683122, 1.000000000000000000, 0.9659258262890683122, 1.000000000000000000, 0.9659258262890683122, 1.000000000000000000, 0.9659258262890683122, 1.000000000000000000, 0.9659258262890683122, 1.000000000000000000, 0.9659258262890683122, 1.000000000000000000, 0.9659258262890683122, 1.000000000000000000, 0.9659258262890683122, 1.000000000000000000, 0.9659258262890683122, 1.000000000000000000, 0.9659258262890683122, 1.000000000000000000, 0.9659258262890683122, 1.000000000000000000, 0.9659258262890683122, 1.000000000000000000, 0.9659258262890683122, 1.000000000000000000, 0.9659258262890683122, 1.000000000000000000, 0.9659258262890683122, 1.000000000000000000, 0.9659258262890683122, 1.000000000000000000, 0.9659258262890683122, 1.000000000000000000, 0.9659258262890683122, 1.000000000000000000, 0.9659258262890683122, 1.000000000000000000, 0.9659258262890683122, 1.000000000000000000, 0.9659258262890683122, 1.000000000000000000, 0.9659258262890683122, 1.000000000000000000, 0.9659258262890683122, 1.000000000000000000, 0.9659258262890683122, 1.000000000000000000, 0.9659258262890683122, 1.000000000000000000, 0.9659258262890683122, 1.000000000000000000, 0.9659258262890683122, 1.000000000000000000, 0.9659258262890683122, 1.000000000000000000, 0.9659258262890683122, 1.000000000000000000, 0.9659258262890683122, 1.000000000000000000, 0.9659258262890683122, 1.000000000000000000, 0.9659258262890683122, 1.000000000000000000, 0.9659258262890683122, 1.000000000000000000, 0.9659258262890683122, 1.000000000000000000, 0.9659258262890683122, 1.000000000000000000, 0.9659258262890683122, 1.000000000000000000, 0.9659258262890683122, 1.000000000000000000, 0.9659258262890683122, 1.000000000000000000, 0.9659258262890683122, 1.000000000000000000, 0.9659258262890683122, 1.000000000000000000, 0.9659258262890683122, 1.000000000000000000, 0.9659258262890683122, 1.000000000000000000, 0.9659258262890683122, 1.000000000000000000, 0.9659258262890683122, 1.000000000000000000, 0.9659258262890683122, 1.000000000000000000, 0.9659258262890683122, 1.000000000000000000, 0.9659258262890683122, 1.000000000000000000, 0.9659258262890683122, 1.000000000000000000, 0.9659258262890683122, 1.000000000000000000, 0.9659258262890683122, 1.000000000000000000, 0.9659258262890683122, 1.000000000000000000, 0.9659258262890683122, 1.000000000000000000, 0.9659258262890683122, 1.000000000000000000, 0.9659258262890683122, 1.000000000000000000, 0.9659258262890683122, 1.000000000000000000, 0.9659258262890683122, 1.000000000000000000, 0.9659258262890683122, 1.000000000000000000, 0.9659258262890683122, 1.000000000000000000, 0.9659258262890683122, 1.000000000000000000, 0.9659258262890683122, 1.000000000000000000, 0.9659258262890683122, 1.000000000000000000, 0.9659258262890683122, 1.000000000000000000, 0.9659258262890683122, 1.000000000000000000, 0.9659258262890683122, 1.000000000000000000, 0.9659258262890683122, 1.000000000000000000, 0.9659258262890683122, 1.000000000000000000, 0.9659258262890683122, 1.000000000000000000, 0.9659258262890683122, 1.000000000000000000, 0.9659258262890683122, 1.000000000000000000, 0.9659258262890683122, 1.000000000000000000, 0.9659258262890683122, 1.000000000000000000, 0.9659258262890683122, 1.000000000000000000, 0.9659258262890683122, 1.000000000000000000, 0.9659258262890683122, 1.000000000000000000, 0.9659258262890683122, 1.000000000000000000, 0.9659258262890683122, 1.000000000000000000, 0.9659258262890683122, 1.000000000000000000, 0.9659258262890683122, 1.000000000000000000, 0.9659258262890683122, 1.000000000000000000, 0.9659258262890683122, 1.000000000000000000, 0.9659258262890683122, 1.000000000000000000, 0.9659258262890683122, 1.000000000000000000, 0.9659258262890683122, 1.000000000000000000, 0.9659258262890683122, 1.000000000000000000, 0.9659258262890683122, 1.000000000000000000, 0.9659258262890683122, 1.000000000000000000, 0.9659258262890683122, 1.000000000000000000, 0.9659258262890683122, 1.000000000000000000, 0.9659258262890683122, 1.000000000000000000, 0.9659258262890683122, 1.000000000000000000, 0.9659258262890683122, 1.000000000000000000, 0.9659258262890683122, 1.000000000000000000, 0.9659258262890683122, 1.000000000000000000, 0.9659258262890683122, 1.000000000000000000, 0.9659258262890683122, 1.000000000000000000, 0.9659258262890683122, 1.000000000000000000, 0.9659258262890683122, 1.000000000000000000, 0.9659258262890683122, 1.000000000000000000, 0.9659258262890683122, 1.000000000000000000, 0.9659258262890683122, 1.000000000000000000, 0.9659258262890683122, 1.000000000000000000, 0.9659258262890683122, 1.000000000000000000, 0.9659258262890683122, 1.000000000000000000, 0.9659258262890683122, 1.000000000000000000, 0.9659258262890683122, 1.000000000000000000, 0.9659258262890683122, 1.000000000000000000, 0.9659258262890683122, 1.000000000000000000, 0.9659258262890683122, 1.000000000000000000, 0.9659258262890683122, 1.000000000000000000, 0.9659258262890683122, 1.000000000000000000, 0.9659258262890683122, 1.000000000000000000, 0.9659258262890683122, 1.000000000000000000, 0.9659258262890683122, 1.000000000000000000, 0.9659258262890683122, 1.000000000000000000, 0.9659258262890683122, 1.000000000000000000, 0.9659258262890683122, 1.000000000000000000, 0.9659258262890683122, 1.000000000000000000, 0.9659258262890683122, 1.000000000000000000, 0.9659258262890683122, 1.000000000000000000, 0.9659258262890683122, 1.000000000000000000, 0.9659258262890683122, 1.000000000000000000, 0.9659258262890683122, 1.000000000000000000, 0.9659258262890683122, 1.000000000000000000, 0.9659258262890683122, 1.000000000000000000, 0.9659258262890683122, 1.000000000000000000, 0.9659258262890683122, 1.000000000000000000, 0.9659258262890683122, 1.000000000000000000, 0.9659258262890683122, 1.000000000000000000, 0.9659258262890683122, 1.000000000000000000, 0.9659258262890683122, 1.000000000000000000, 0.9659258262890683122, 1.000000000000000000, 0.9659258262890683122, 1.000000000000000000, 0.9659258262890683122, 1.000000000000000000, 0.9659258262890683122, 1.000000000000000000, 0.9659258262890683122, 1.000000000000000000, 0.9659258262890683122, 1.000000000000000000, 0.9659258262890683122, 1.000000000000000000, 0.9659258262890683122, 1.000000000000000000, 0.9659258262890683122, 1.000000000000000000, 0.9659258262890683122, 1.000000000000000000, 0.9659258262890683122, 1.000000000000000000, 0.9659258262890683122, 1.000000000000000000, 0.9659258262890683122, 1.000000000000000000, 0.9659258262890683122, 1.000000000000000000, 0.9659258262890683122, 1.000000000000000000, 0.9659258262890683122, 1.000000000000000000, 0.9659258262890683122, 1.000000000000000000, 0.9659258262890683122, 1.000000000000000000, 0.9659258262890683122, 1.000000000000000000, 0.9659258262890683122, 1.000000000000000000, 0.9659258262890683122, 1.000000000000000000, 0.9659258262890683122, 1.000000000000000000, 0.9659258262890683122, 1.000000000000000000, 0.9659258262890683122, 1.000000000000000000, 0.9659258262890683122, 1.000000000000000000, 0.9659258262890683122, 1.000000000000000000, 0.9659258262890683122, 1.000000000000000000, 0.9659258262890683122, 1.000000000000000000, 0.9659258262890683122, 1.000000000000000000, 0.9659258262890683122, 1.000000000000000000, 0.9659258262890683122, 1.000000000000000000, 0.9659258262890683122, 1.000000000000000000, 0.9659258262890683122, 1.000000000000000000, 0.9659258262890683122, 1.000000000000000000, 0.9659258262890683122, 1.000000000000000000, 0.9659258262890683122, 1.000000000000000000, 0.9659258262890683122, 1.000000000000000000, 0.9659258262890683122, 1.000000000000000000, 0.9659258262890683122, 1.000000000000000000, 0.9659258262890683122, 1.000000000000000000, 0.9659258262890683122, 1.000000000000000000, 0.9659258262890683122, 1.000000000000000000, 0.9659258262890683122, 1.000000000000000000, 0.9659258262890683122, 1.000000000000000000, 0.9659258262890683122, 1.000000000000000000, 0.9659258262890683122, 1.000000000000000000, 0.9659258262890683122, 1.000000000000000000, 0.9659258262890683122, 1.000000000000000000, 0.9659258262890683122, 1.000000000000000000, 0.9659258262890683122, 1.000000000000000000, 0.9659258262890683122, 1.000000000000000000, 0.9659258262890683122, 1.000000000000000000, 0.9659258262890683122, 1.000000000000000000, 0.9659258262890683122, 1.000000000000000000, 0.9659258262890683122, 1.000000000000000000, 0.9659258262890683122, 1.000000000000000000, 0.9659258262890683122, 1.000000000000000000, 0.9659258262890683122, 1.000000000000000000, 0.9659258262890683122, 1.000000000000000000, 0.9659258262890683122, 1.000000000000000000, 0.9659258262890683122, 1.000000000000000000, 0.9659258262890683122, 1.000000000000000000, 0.9659258262890683122, 1.000000000000000000, 0.9659258262890683122, 1.000000000000000000, 0.9659258262890683122, 1.000000000000000000, 0.9659258262890683122, 1.000000000000000000, 0.9659258262890683122, 1.000000000000000000, 0.9659258262890683122, 1.000000000000000000, 0.9659258262890683122, 1.000000000000000000, 0.9659258262890683122, 1.000000000000000000, 0.9659258262890683122, 1.000000000000000000, 0.9659258262890683122, 1.000000000000000000, 0.9659258262890683122, 1.000000000000000000, 0.9659258262890683122, 1.000000000000000000, 0.9659258262890683122, 1.000000000000000000, 0.9659258262890683122, 1.000000000000000000, 0.9659258262890683122, 1.000000000000000000, 0.9659258262890683122, 1.000000000000000000, 0.9659258262890683122, 1.000000000000000000, 0.9659258262890683122, 1.000000000000000000, 0.9659258262890683122, 1.000000000000000000, 0.9659258262890683122, 1.000000000000000000, 0.9659258262890683122, 1.000000000000000000, 0.9659258262890683122, 1.000000000000000000, 0.9659258262890683122, 1.000000000000000000, 0.9659258262890683122, 1.000000000000000000, 0.9659258262890683122, 1.000000000000000000, 0.9659258262890683122, 1.000000000000000000, 0.9659258262890683122, 1.000000000000000000, 0.9659258262890683122, 1.000000000000000000, 0.9659258262890683122, 1.000000000000000000, 0.9659258262890683122, 1.000000000000000000, 0.9659258262890683122, 1.000000000000000000, 0.9659258262890683122, 1.000000000000000000, 0.9659258262890683122, 1.000000000000000000, 0.9659258262890683122, 1.000000000000000000, 0.9659258262890683122, 1.000000000000000000, 0.9659258262890683122, 1.000000000000000000, 0.9659258262890683122, 1.000000000000000000, 0.9659258262890683122, 1.000000000000000000, 0.9659258262890683122, 1.000000000000000000, 0.9659258262890683122, 1.000000000000000000, 0.9659258262890683122, 1.000000000000000000, 0.9659258262890683122, 1.000000000000000000, 0.9659258262890683122, 1.000000000000000000, 0.9659258262890683122, 1.000000000000000000, 0.9659258262890683122, 1.000000000000000000, 0.9659258262890683122, 1.000000000000000000, 0.9659258262890683122, 1.000000000000000000, 0.9659258262890683122, 1.000000000000000000, 0.9659258262890683122, 1.000000000000000000, 0.9659258262890683122, 1.000000000000000000, 0.9659258262890683122, 1.000000000000000000, 0.9659258262890683122, 1.000000000000000000, 0.9659258262890683122, 1.000000000000000000, 0.9659258262890683122, 1.000000000000000000, 0.9659258262890683122, 1.000000000000000000) ) ) 
 REPRESENTATION_ITEM ( '' )  SURFACE ( )  );
#28883 = CARTESIAN_POINT ( 'NONE',  ( -0.2690288713910754526, -0.5511811023622046335, 0.09757992244046803654 ) ) ;
#28884 = ADVANCED_FACE ( 'NONE', ( #26803 ), #53837, .F. ) ;
#28885 = CARTESIAN_POINT ( 'NONE',  ( -0.6692913385826764205, -0.5511811023622047445, 6.969142054262312111E-17 ) ) ;
#28886 = PRODUCT_DEFINITION_FORMATION_WITH_SPECIFIED_SOURCE ( 'ANY', '', #8366, .NOT_KNOWN. ) ;
#28887 = CARTESIAN_POINT ( 'NONE',  ( -1.332020997375327642, -0.05778040916215522460, 0.4822834645669289988 ) ) ;
#28888 = CARTESIAN_POINT ( 'NONE',  ( 0.4527559055118117182, -0.5400638737290844871, 0.3530559997133364547 ) ) ;
#28889 = CARTESIAN_POINT ( 'NONE',  ( -1.043307086614172041, -0.5400638737290844871, 0.3530559997133364547 ) ) ;
#28890 = LINE ( 'NONE', #27643, #67585 ) ;
#28891 = EDGE_LOOP ( 'NONE', ( #3823, #2283, #73063, #25336 ) ) ;
#28892 = CARTESIAN_POINT ( 'NONE',  ( -1.601049868766403650, 0.2306618581243847221, -0.2411417322834647770 ) ) ;
#28893 = FACE_OUTER_BOUND ( 'NONE', #12411, .T. ) ;
#28894 = CARTESIAN_POINT ( 'NONE',  ( 0.1265901696524989462, 0.4724409448818897572, -1.883202099737532276 ) ) ;
#28895 = CARTESIAN_POINT ( 'NONE',  ( -1.646051170424378096, -0.1870078740157480046, 1.254653134982923898E-17 ) ) ;
#28896 = CARTESIAN_POINT ( 'NONE',  ( -0.1049643490035302024, -0.3917322834645671215, -0.8517060367454066805 ) ) ;
#28897 = CARTESIAN_POINT ( 'NONE',  ( -1.157146581871515012E-16, 0.4724409448818898682, -0.9448818897637796255 ) ) ;
#28898 = CARTESIAN_POINT ( 'NONE',  ( -0.8530183727034112984, 0.05413385826771666132, 0.4176697321401328100 ) ) ;
#28899 = CARTESIAN_POINT ( 'NONE',  ( 1.332020997375329197, -0.3162353388693405765, 0.4822834645669290543 ) ) ;
#28901 = CARTESIAN_POINT ( 'NONE',  ( 0.4724409448818898682, 2.892866454678787531E-17, -2.007874015748031482 ) ) ;
#28900 = CARTESIAN_POINT ( 'NONE',  ( -1.627296587926508442, -0.6046776061558809534, -0.2411417322834644161 ) ) ;
#28902 = CARTESIAN_POINT ( 'NONE',  ( -1.220472440944881054, 0.2952755905511811885, 0.000000000000000000 ) ) ;
#28903 = CARTESIAN_POINT ( 'NONE',  ( -0.9842519685039365918, -0.6692913385826771977, 8.415575281601705876E-17 ) ) ;
#28904 = AXIS2_PLACEMENT_3D ( 'NONE', #30841, #31250, #43869 ) ;
#28905 = CARTESIAN_POINT ( 'NONE',  ( 0.2867679344610365999, -0.2867679344610365999, 0.1365022554143850153 ) ) ;
#28906 = CARTESIAN_POINT ( 'NONE',  ( 0.4855643044619428750, -0.004921259842519576551, 0.3153832671262227771 ) ) ;
#28907 = CARTESIAN_POINT ( 'NONE',  ( 0.2867679344610366554, -0.2867679344610365444, -0.4980314960629921850 ) ) ;
#28908 = CARTESIAN_POINT ( 'NONE',  ( 0.07217847769028949700, -0.2845877964562159024, 0.3641732283464567677 ) ) ;
#28909 = CARTESIAN_POINT ( 'NONE',  ( 0.9383202099737536495, -0.2845877964562159024, 0.3641732283464567677 ) ) ;
#28910 = CARTESIAN_POINT ( 'NONE',  ( 0.8333333333333340365, 0.2952755905511810774, -0.1292274648535930714 ) ) ;
#28911 = CARTESIAN_POINT ( 'NONE',  ( -0.2821522309711278487, -0.5511811023622048555, -0.09757992244046775898 ) ) ;
#28912 = CARTESIAN_POINT ( 'NONE',  ( 4.797336870675656522E-17, -0.3917322834645670104, -2.433070866141732402 ) ) ;
#28913 = CARTESIAN_POINT ( 'NONE',  ( 1.574803149606299746, -0.1870078740157479769, 0.4822834645669291653 ) ) ;
#28914 = CARTESIAN_POINT ( 'NONE',  ( -1.417322834645668772, -0.1870078740157480601, -0.3641732283464567677 ) ) ;
#28915 = CARTESIAN_POINT ( 'NONE',  ( -0.4724409448818898682, -8.678599364036362592E-17, -0.4311023622047244208 ) ) ;
#28916 = CARTESIAN_POINT ( 'NONE',  ( 0.02624671916010564918, -0.6046776061558809534, -0.2411417322834644161 ) ) ;
#28917 = CARTESIAN_POINT ( 'NONE',  ( 1.489501312335958172, -0.2845877964562159024, 0.3641732283464567677 ) ) ;
#28918 = CARTESIAN_POINT ( 'NONE',  ( 0.6430446194225728496, -0.004921259842519576551, 0.3153832671262227771 ) ) ;
#28919 = CARTESIAN_POINT ( 'NONE',  ( -0.2493438320209966919, -0.004921259842519870586, -0.3153832671262229437 ) ) ;
#28920 = CARTESIAN_POINT ( 'NONE',  ( -0.6889763779527552368, 0.1660481256975885056, 0.3530559997133364547 ) ) ;
#28921 = LINE ( 'NONE', #16728, #6261 ) ;
#28922 = CARTESIAN_POINT ( 'NONE',  ( 0.4091458600556403535, 0.2362204724409449896, -1.940288713910761187 ) ) ;
#28923 = CARTESIAN_POINT ( 'NONE',  ( 0.2099737532808405305, -0.6046776061558807314, 0.2411417322834647770 ) ) ;
#28924 = CARTESIAN_POINT ( 'NONE',  ( 0.3460692066303959202, -0.1998031496062991630, -1.756561679790026309 ) ) ;
#28925 = DIRECTION ( 'NONE',  ( -0.000000000000000000, 1.000000000000000000, 0.000000000000000000 ) ) ;
#28926 = CARTESIAN_POINT ( 'NONE',  ( -0.2493438320209966919, -0.004921259842519870586, -0.3153832671262229437 ) ) ;
#28927 = CARTESIAN_POINT ( 'NONE',  ( 0.03280839895013198948, 0.2952755905511811885, 0.1292274648535926551 ) ) ;
#28928 = CARTESIAN_POINT ( 'NONE',  ( -1.614173228346455824, 0.2952755905511811885, 0.000000000000000000 ) ) ;
#28929 = CARTESIAN_POINT ( 'NONE',  ( -1.548556430446193399, -0.5023911411419708095, -0.1820866141732282451 ) ) ;
#28930 = CARTESIAN_POINT ( 'NONE',  ( 1.148293963254593875, -0.6692913385826771977, 0.1292274648535927661 ) ) ;
#28931 = CARTESIAN_POINT ( 'NONE',  ( -1.259842519685038686, -0.1870078740157480879, -0.4822834645669291653 ) ) ;
#28932 = CARTESIAN_POINT ( 'NONE',  ( -0.8005249343832013809, -0.3690944881889763329, 0.3153832671262228327 ) ) ;
#28933 = CARTESIAN_POINT ( 'NONE',  ( 0.1070741851644054637, -0.3996062992125984925, -0.3195538057742782212 ) ) ;
#28934 = CARTESIAN_POINT ( 'NONE',  ( -0.1998031496062994683, 0.3460692066303958092, -0.3280839895013123453 ) ) ;
#28935 = CARTESIAN_POINT ( 'NONE',  ( -0.3917322834645670659, -7.196005306013484475E-17, -2.870754223918321912 ) ) ;
#28936 = CARTESIAN_POINT ( 'NONE',  ( 0.6167979002624679463, 0.05413385826771626580, -0.4176697321401330321 ) ) ;
#28937 = CARTESIAN_POINT ( 'NONE',  ( -0.5314960629921346991, 2.755905511811024056, 2.503252890251014939 ) ) ;
#28938 = ADVANCED_FACE ( 'NONE', ( #42641 ), #75066, .F. ) ;
#28939 = CARTESIAN_POINT ( 'NONE',  ( 1.095800524934383846, -0.2845877964562159024, 0.3641732283464567677 ) ) ;
#28940 = LINE ( 'NONE', #47461, #33192 ) ;
#28941 = ADVANCED_FACE ( 'NONE', ( #68338 ), #56503, .F. ) ;
#28942 = CARTESIAN_POINT ( 'NONE',  ( 0.8202099737532813073, 0.2952755905511811885, 0.1292274648535926551 ) ) ;
#28943 = CARTESIAN_POINT ( 'NONE',  ( 0.3949938075777408852, 0.1058382717557500435, -0.9888451443569553634 ) ) ;
#28944 = CARTESIAN_POINT ( 'NONE',  ( 1.062992125984252745, 0.1771653543307087630, 0.000000000000000000 ) ) ;
#28945 = EDGE_CURVE ( 'NONE', #49366, #50786, #23959, .T. ) ;
#28946 = CARTESIAN_POINT ( 'NONE',  ( 0.2034120734908144990, -0.6692913385826771977, 0.1292274648535927661 ) ) ;
#28947 = CARTESIAN_POINT ( 'NONE',  ( -0.9055118110236215490, -0.6692913385826771977, 8.415575281601705876E-17 ) ) ;
#28948 = DIRECTION ( 'NONE',  ( 0.000000000000000000, 8.673617379884024625E-16, 1.000000000000000000 ) ) ;
#28949 = CARTESIAN_POINT ( 'NONE',  ( 0.4091458600556403535, 0.2362204724409449896, -1.391076115485564424 ) ) ;
#28950 = CARTESIAN_POINT ( 'NONE',  ( 0.1070741851644054915, -0.3996062992125985480, -2.290026246719159886 ) ) ;
#28951 = CARTESIAN_POINT ( 'NONE',  ( 0.4002624671916016896, -0.2845877964562161244, -0.3641732283464567121 ) ) ;
#28952 = ORIENTED_EDGE ( 'NONE', *, *, #58971, .F. ) ;
#28953 = CARTESIAN_POINT ( 'NONE',  ( -0.3392501089628017219, -0.1958661417322836995, -0.5216728590889256889 ) ) ;
#28954 = EDGE_LOOP ( 'NONE', ( #14606, #36619, #50375, #16544, #14397, #52794, #11910, #62392, #75531, #30623, #34804, #51278, #46315, #24975 ) ) ;
#28955 = CARTESIAN_POINT ( 'NONE',  ( -0.3412073490813641308, -0.6046776061558807314, 0.2411417322834647770 ) ) ;
#28956 = CARTESIAN_POINT ( 'NONE',  ( -0.3412073490813641308, 0.2306618581243847221, -0.2411417322834647770 ) ) ;
#28957 = CARTESIAN_POINT ( 'NONE',  ( -0.4002624671916004129, -0.2845877964562159024, 0.3641732283464567677 ) ) ;
#28958 = CARTESIAN_POINT ( 'NONE',  ( 0.6758530183727039509, -0.6692913385826771977, 0.1292274648535927661 ) ) ;
#28959 = CARTESIAN_POINT ( 'NONE',  ( -0.7939632545931750718, -0.05778040916215560624, -0.4822834645669293319 ) ) ;
#28960 = CARTESIAN_POINT ( 'NONE',  ( -0.3608923884514428360, -0.6692913385826773087, -0.1292274648535924053 ) ) ;
#28961 = CARTESIAN_POINT ( 'NONE',  ( 1.023622047244095112, -0.1870078740157480879, -0.4822834645669291653 ) ) ;
#28962 = CARTESIAN_POINT ( 'NONE',  ( 0.8923884514435701520, -0.6046776061558809534, -0.2411417322834644161 ) ) ;
#28963 = CARTESIAN_POINT ( 'NONE',  ( 0.8661417322834653598, -0.1870078740157479769, 0.4822834645669291653 ) ) ;
#28964 = EDGE_CURVE ( 'NONE', #42501, #49642, #82205, .T. ) ;
#28965 = CARTESIAN_POINT ( 'NONE',  ( 4.797336870675656522E-17, -0.3917322834645670104, -0.8582677165354329896 ) ) ;
#28966 = CARTESIAN_POINT ( 'NONE',  ( -0.1574803149606292529, -0.1870078740157480601, -0.3641732283464567677 ) ) ;
#28967 = ORIENTED_EDGE ( 'NONE', *, *, #33956, .T. ) ;
#28968 = CARTESIAN_POINT ( 'NONE',  ( -0.3949938075777409963, -7.255918531996591613E-17, -1.141732283464566899 ) ) ;
#28969 = ORIENTED_EDGE ( 'NONE', *, *, #60504, .F. ) ;
#28970 = CARTESIAN_POINT ( 'NONE',  ( -0.7677165354330699465, 0.07958543189024085140, 0.2665933059059887866 ) ) ;
#28971 = CARTESIAN_POINT ( 'NONE',  ( -0.6102362204724400829, -0.5400638737290845981, -0.3530559997133363437 ) ) ;
#28972 = CARTESIAN_POINT ( 'NONE',  ( 0.3460692066303959202, 0.1998031496062993295, 0.02624671916010497957 ) ) ;
#28973 = CARTESIAN_POINT ( 'NONE',  ( -0.2296587926509179312, -0.3162353388693409650, -0.4822834645669289433 ) ) ;
#28974 = CARTESIAN_POINT ( 'NONE',  ( -0.2821522309711278487, 0.2952755905511811885, 0.1292274648535926551 ) ) ;
#28975 = CARTESIAN_POINT ( 'NONE',  ( -1.233595800524933894, -0.6046776061558809534, -0.2411417322834644161 ) ) ;
#28976 = CARTESIAN_POINT ( 'NONE',  ( -1.410761154855642463, -0.05778040916215522460, 0.4822834645669289988 ) ) ;
#28977 = CARTESIAN_POINT ( 'NONE',  ( 0.9908136482939640111, -0.5511811023622046335, 0.09757992244046803654 ) ) ;
#28978 = CARTESIAN_POINT ( 'NONE',  ( -0.4744094488188934089, 1.537401574803149984, -1.016821367227985551 ) ) ;
#28979 = CARTESIAN_POINT ( 'NONE',  ( 0.2596871853482274894, 0.1407230452551245514, 5.593746434152945035 ) ) ;
#28980 = CARTESIAN_POINT ( 'NONE',  ( 0.6364829396325465405, -0.08942795157527998196, 0.3641732283464567121 ) ) ;
#28981 = CARTESIAN_POINT ( 'NONE',  ( 0.06561679790026316017, -0.4281496062992124485, 0.4176697321401328655 ) ) ;
#28982 = CARTESIAN_POINT ( 'NONE',  ( 0.4527559055118117182, 0.1660481256975883668, -0.3530559997133364547 ) ) ;
#28983 = ORIENTED_EDGE ( 'NONE', *, *, #59891, .T. ) ;
#28984 = CARTESIAN_POINT ( 'NONE',  ( -0.1070741851644051862, -0.3996062992125987146, -1.489501312335957950 ) ) ;
#28985 = DIRECTION ( 'NONE',  ( 0.000000000000000000, 1.000000000000000000, 0.000000000000000000 ) ) ;
#28986 = ORIENTED_EDGE ( 'NONE', *, *, #64378, .T. ) ;
#28987 = CARTESIAN_POINT ( 'NONE',  ( -0.2925321140481930149, -0.2925321140481933480, -1.080708661417322691 ) ) ;
#28988 = CARTESIAN_POINT ( 'NONE',  ( -0.2925321140481932369, 0.2925321140481931259, -0.4114173228346455491 ) ) ;
#28989 = CARTESIAN_POINT ( 'NONE',  ( -0.7808398950131225646, -0.08942795157527998196, 0.3641732283464567121 ) ) ;
#28990 = CARTESIAN_POINT ( 'NONE',  ( -1.115485564304461219, -0.4281496062992124485, 0.4176697321401328655 ) ) ;
#28991 = CARTESIAN_POINT ( 'NONE',  ( -0.2362204724409451284, 0.4091458600556402425, -0.01312335958005249326 ) ) ;
#28992 = CARTESIAN_POINT ( 'NONE',  ( 0.1958661417322836440, -0.3392501089628017219, -2.696194225721784576 ) ) ;
#28993 = CARTESIAN_POINT ( 'NONE',  ( 1.653543307086614789, -0.1870078740157479769, 0.4822834645669291653 ) ) ;
#28994 = CARTESIAN_POINT ( 'NONE',  ( 0.7283464566929140904, -0.5400638737290845981, -0.3530559997133363437 ) ) ;
#28995 = CARTESIAN_POINT ( 'NONE',  ( 0.6692913385826778638, -0.6692913385826771977, 8.415575281601705876E-17 ) ) ;
#28996 = CARTESIAN_POINT ( 'NONE',  ( -0.5183727034120726440, 0.1771653543307087630, 0.09757992244046791164 ) ) ;
#28997 = CARTESIAN_POINT ( 'NONE',  ( 0.06561679790026316017, 0.05413385826771626580, -0.4176697321401330321 ) ) ;
#28998 = CARTESIAN_POINT ( 'NONE',  ( -0.4091458600556402980, -0.2362204724409451284, -2.176509186351706315 ) ) ;
#28999 = CARTESIAN_POINT ( 'NONE',  ( -0.7020997375328074108, -0.08942795157527998196, 0.3641732283464567121 ) ) ;
#29000 = CARTESIAN_POINT ( 'NONE',  ( -0.3018372703412066094, 0.05413385826771666132, 0.4176697321401328100 ) ) ;
#29001 = CARTESIAN_POINT ( 'NONE',  ( -0.3949938075777411073, 0.1058382717557497660, -1.684383202099737575 ) ) ;
#29002 = CARTESIAN_POINT ( 'NONE',  ( -1.528871391076114250, 0.2952755905511810774, -0.1292274648535930714 ) ) ;
#29003 = CARTESIAN_POINT ( 'NONE',  ( -0.1049868766404193215, 0.1283753931104746893, -0.1820866141732285504 ) ) ;
#29004 = CARTESIAN_POINT ( 'NONE',  ( 1.614173228346457378, -0.5511811023622047445, 6.969142054262312111E-17 ) ) ;
#29005 = CARTESIAN_POINT ( 'NONE',  ( -1.089238845144356427, 0.05413385826771666132, 0.4176697321401328100 ) ) ;
#29006 = CARTESIAN_POINT ( 'NONE',  ( -0.8333333333333323711, 0.1771653543307087630, 0.09757992244046791164 ) ) ;
#29007 = CARTESIAN_POINT ( 'NONE',  ( 0.1265901696524989184, 0.4724409448818898127, -2.274934383202099397 ) ) ;
#29008 = CARTESIAN_POINT ( 'NONE',  ( -1.043307086614172707, 0.1660481256975883668, -0.3530559997133364547 ) ) ;
#29009 = CARTESIAN_POINT ( 'NONE',  ( -0.5183727034120726440, 0.2952755905511811885, 0.1292274648535926551 ) ) ;
#29010 =( BOUNDED_CURVE ( )  B_SPLINE_CURVE ( 3, ( #47203, #72893, #15243, #37782 ),
 .UNSPECIFIED., .F., .F. ) 
 B_SPLINE_CURVE_WITH_KNOTS ( ( 4, 4 ),
 ( 4.502511237001506572, 4.502773989760327389 ),
 .UNSPECIFIED. ) 
 CURVE ( )  GEOMETRIC_REPRESENTATION_ITEM ( )  RATIONAL_B_SPLINE_CURVE ( ( 1.000000000000000000, 0.9999999942467490133, 0.9999999942467490133, 1.000000000000000000 ) ) 
 REPRESENTATION_ITEM ( '' )  );
#29011 = CARTESIAN_POINT ( 'NONE',  ( 0.1771653543307093182, -0.5400638737290845981, -0.3530559997133363437 ) ) ;
#29012 = CARTESIAN_POINT ( 'NONE',  ( -0.1958661417322834497, -0.3392501089628018884, -2.507854699966192147 ) ) ;
#29013 = AXIS2_PLACEMENT_3D ( 'NONE', #31248, #45531, #26181 ) ;
#29014 = CARTESIAN_POINT ( 'NONE',  ( -1.895263394252401090, 1.111778211650215509, -0.2101609992702490048 ) ) ;
#29015 = CARTESIAN_POINT ( 'NONE',  ( 0.2624671916010504757, 0.1283753931104748280, 0.1820866141732283561 ) ) ;
#29016 = CARTESIAN_POINT ( 'NONE',  ( 0.9645669291338588858, 0.1660481256975885056, 0.3530559997133364547 ) ) ;
#29017 = CARTESIAN_POINT ( 'NONE',  ( -1.161417322834644716, -0.4536011799217368745, -0.2665933059059886201 ) ) ;
#29018 = CARTESIAN_POINT ( 'NONE',  ( 1.253280839895013710, -0.05778040916215560624, -0.4822834645669293319 ) ) ;
#29019 = CARTESIAN_POINT ( 'NONE',  ( -1.581364829396324945, -0.2845877964562159024, 0.3641732283464567677 ) ) ;
#29020 = CARTESIAN_POINT ( 'NONE',  ( -0.4002624671916004129, -0.05778040916215560624, -0.4822834645669293319 ) ) ;
#29021 = CARTESIAN_POINT ( 'NONE',  ( 0.2821522309711292364, 0.1771653543307087075, -0.09757992244046823083 ) ) ;
#29022 = DIRECTION ( 'NONE',  ( -0.4999999999999886202, 0.7071067811865615615, -0.4999999999999915068 ) ) ;
#29023 = CARTESIAN_POINT ( 'NONE',  ( 0.6430446194225728496, -0.004921259842519576551, 0.3153832671262227771 ) ) ;
#29024 = EDGE_CURVE ( 'NONE', #27310, #9114, #48486, .T. ) ;
#29025 = CARTESIAN_POINT ( 'NONE',  ( -0.2296587926509179312, -0.05778040916215522460, 0.4822834645669289988 ) ) ;
#29026 = CARTESIAN_POINT ( 'NONE',  ( -0.2925321140481930149, -0.2925321140481933480, -0.1358267716535432879 ) ) ;
#29027 = CARTESIAN_POINT ( 'NONE',  ( -0.9842519685039365918, -0.6692913385826771977, 8.415575281601705876E-17 ) ) ;
#29028 = CARTESIAN_POINT ( 'NONE',  ( 0.1049643490035304938, -0.3917322834645669549, -1.744750656167979308 ) ) ;
#29029 = CARTESIAN_POINT ( 'NONE',  ( 0.9908136482939640111, 0.1771653543307087075, -0.09757992244046823083 ) ) ;
#29030 = CARTESIAN_POINT ( 'NONE',  ( 8.195543980992789655E-16, -0.1870078740157480879, -0.4822834645669291653 ) ) ;
#29031 = CARTESIAN_POINT ( 'NONE',  ( -0.4396325459317577122, -0.6692913385826773087, -0.1292274648535924053 ) ) ;
#29032 = CARTESIAN_POINT ( 'NONE',  ( -0.3805774278215216522, -0.004921259842519576551, 0.3153832671262227771 ) ) ;
#29033 = DIRECTION ( 'NONE',  ( 0.000000000000000000, 0.000000000000000000, 1.000000000000000000 ) ) ;
#29034 = CARTESIAN_POINT ( 'NONE',  ( -0.3805774278215216522, -0.004921259842519576551, 0.3153832671262227771 ) ) ;
#29035 = CARTESIAN_POINT ( 'NONE',  ( 0.3674540682414705883, -0.6046776061558807314, 0.2411417322834647770 ) ) ;
#29036 = CARTESIAN_POINT ( 'NONE',  ( -1.338582677165353729, -0.1870078740157480601, -0.3641732283464567677 ) ) ;
#29037 = CARTESIAN_POINT ( 'NONE',  ( -0.3996062992125984925, -0.1070741851644056858, -1.067585301837270517 ) ) ;
#29038 = CARTESIAN_POINT ( 'NONE',  ( -1.259842519685038686, -0.1870078740157480879, -0.4822834645669291653 ) ) ;
#29039 = FACE_OUTER_BOUND ( 'NONE', #34449, .T. ) ;
#29040 = ORIENTED_EDGE ( 'NONE', *, *, #25308, .T. ) ;
#29041 = CARTESIAN_POINT ( 'NONE',  ( -1.450131233595799651, -0.5511811023622046335, 0.09757992244046803654 ) ) ;
#29042 = CARTESIAN_POINT ( 'NONE',  ( -0.5839895013123351797, 0.2952755905511810774, -0.1292274648535930714 ) ) ;
#29043 = CARTESIAN_POINT ( 'NONE',  ( 0.2661270878686344821, 1.144642331940836755, -1.467344394069625579 ) ) ;
#29044 = CARTESIAN_POINT ( 'NONE',  ( -1.391076115485563314, -0.6046776061558809534, -0.2411417322834644161 ) ) ;
#29045 = CARTESIAN_POINT ( 'NONE',  ( -0.1049643490035302024, -0.3917322834645671215, -1.731627296587926468 ) ) ;
#29046 = CARTESIAN_POINT ( 'NONE',  ( 0.2579773093944593976, 0.2955417804206795784, -1.220472440944881942 ) ) ;
#29047 = CARTESIAN_POINT ( 'NONE',  ( 1.351706036745407680, 0.05413385826771666132, 0.4176697321401328100 ) ) ;
#29048 = CARTESIAN_POINT ( 'NONE',  ( 0.7874015748031503170, -0.1870078740157480879, -0.4822834645669291653 ) ) ;
#29049 = CARTESIAN_POINT ( 'NONE',  ( 1.092353285368624860, -4.408777212815537393E-16, -0.4445507791589063395 ) ) ;
#29050 = AXIS2_PLACEMENT_3D ( 'NONE', #49495, #11623, #54563 ) ;
#29051 = AXIS2_PLACEMENT_3D ( 'NONE', #9162, #73131, #47438 ) ;
#29052 = CARTESIAN_POINT ( 'NONE',  ( -0.1070741851644051862, -0.3996062992125986035, -2.511154855643044748 ) ) ;
#29053 = CARTESIAN_POINT ( 'NONE',  ( 1.561679790026247350, -0.3690944881889763329, 0.3153832671262228327 ) ) ;
#29054 = CARTESIAN_POINT ( 'NONE',  ( -0.1070741851644056997, 0.3996062992125986035, -0.3215223097112860362 ) ) ;
#29055 = VERTEX_POINT ( 'NONE', #75479 ) ;
#29056 = CARTESIAN_POINT ( 'NONE',  ( -0.6824146981627288167, 0.1283753931104748280, 0.1820866141732283561 ) ) ;
#29057 = CARTESIAN_POINT ( 'NONE',  ( -0.3917322834645671215, 0.1049643490035301469, -2.229658792650918819 ) ) ;
#29058 = VERTEX_POINT ( 'NONE', #81383 ) ;
#29059 = CARTESIAN_POINT ( 'NONE',  ( 0.7020997375328090762, -0.05778040916215560624, -0.4822834645669293319 ) ) ;
#29060 = CARTESIAN_POINT ( 'NONE',  ( -0.2690288713910754526, 0.2952755905511810774, -0.1292274648535930714 ) ) ;
#29061 = CARTESIAN_POINT ( 'NONE',  ( -0.9711286089238838626, 0.2306618581243847221, -0.2411417322834647770 ) ) ;
#29062 = CARTESIAN_POINT ( 'NONE',  ( 1.410761154855643795, -0.05778040916215560624, -0.4822834645669293319 ) ) ;
#29063 = CARTESIAN_POINT ( 'NONE',  ( -1.391076115485563314, -0.5023911411419708095, -0.1820866141732282451 ) ) ;
#29064 = CARTESIAN_POINT ( 'NONE',  ( -0.4744094488188882464, 1.546091976385118194, -2.554262525012306551 ) ) ;
#29065 = CARTESIAN_POINT ( 'NONE',  ( 0.3543307086614181922, -0.6692913385826771977, 8.415575281601705876E-17 ) ) ;
#29066 = CARTESIAN_POINT ( 'NONE',  ( -0.9186351706036736120, -0.6046776061558809534, -0.2411417322834644161 ) ) ;
#29067 = CARTESIAN_POINT ( 'NONE',  ( -0.3917322834645670659, 0.1049643490035301607, -1.687644726212911506 ) ) ;
#29068 = CARTESIAN_POINT ( 'NONE',  ( -1.102362204724408601, -0.1870078740157480879, -0.4822834645669291653 ) ) ;
#29069 = CARTESIAN_POINT ( 'NONE',  ( 0.2886821576726813499, 1.160628398849492315, -2.785086082795377393 ) ) ;
#29070 = CARTESIAN_POINT ( 'NONE',  ( 0.8530183727034128527, -0.4281496062992124485, 0.4176697321401328655 ) ) ;
#29071 = CARTESIAN_POINT ( 'NONE',  ( 1.305774278215223960, -0.5511811023622046335, 0.09757992244046803654 ) ) ;
#29072 = VERTEX_POINT ( 'NONE', #80565 ) ;
#29073 = CARTESIAN_POINT ( 'NONE',  ( 0.3392501089628018329, 0.1958661417322835607, -2.805137426018059710 ) ) ;
#29074 = CARTESIAN_POINT ( 'NONE',  ( -0.5577427821522301654, -0.3162353388693405765, 0.4822834645669290543 ) ) ;
#29075 = ORIENTED_EDGE ( 'NONE', *, *, #4265, .T. ) ;
#29077 = AXIS2_PLACEMENT_3D ( 'NONE', #5690, #10789, #43159 ) ;
#29076 = CARTESIAN_POINT ( 'NONE',  ( 0.4002624671916016896, -0.2845877964562161244, -0.3641732283464567121 ) ) ;
#29078 = CARTESIAN_POINT ( 'NONE',  ( -1.157146581871515012E-16, 0.4724409448818898682, -0.1574803149606299191 ) ) ;
#29079 = CARTESIAN_POINT ( 'NONE',  ( 0.9383202099737536495, -0.3162353388693405765, 0.4822834645669290543 ) ) ;
#29080 = CARTESIAN_POINT ( 'NONE',  ( 0.8398950131233602345, 0.2306618581243847221, -0.2411417322834647770 ) ) ;
#29081 = CARTESIAN_POINT ( 'NONE',  ( -0.3477690288713905509, -0.6692913385826771977, 0.1292274648535927661 ) ) ;
#29082 = CARTESIAN_POINT ( 'NONE',  ( 0.3392501089628018884, -0.1958661417322833942, -1.204087557251655394 ) ) ;
#29083 = CARTESIAN_POINT ( 'NONE',  ( -0.7480314960629914633, -0.6692913385826771977, 8.415575281601705876E-17 ) ) ;
#29084 = CARTESIAN_POINT ( 'NONE',  ( -0.2867679344610364334, -0.2867679344610367109, -2.190944881889763440 ) ) ;
#29085 = CARTESIAN_POINT ( 'NONE',  ( -1.463254593175852492, -0.6692913385826773087, -0.1292274648535924053 ) ) ;
#29086 = CARTESIAN_POINT ( 'NONE',  ( -1.010498687664041384, 0.05413385826771666132, 0.4176697321401328100 ) ) ;
#29087 = CARTESIAN_POINT ( 'NONE',  ( 1.397637795275591177, 0.1660481256975883668, -0.3530559997133364547 ) ) ;
#29088 = CARTESIAN_POINT ( 'NONE',  ( -0.1938976377952756625, -0.1938976377952756625, 0.1574803149606299191 ) ) ;
#29089 = CARTESIAN_POINT ( 'NONE',  ( -0.9120734908136475250, 0.2952755905511811885, 0.1292274648535926551 ) ) ;
#29090 = CARTESIAN_POINT ( 'NONE',  ( -0.1070741851644051862, -0.3996062992125986590, 0.008530183727034111943 ) ) ;
#29091 = CARTESIAN_POINT ( 'NONE',  ( 0.1706036745406830368, 0.05413385826771666132, 0.4176697321401328100 ) ) ;
#29092 = CARTESIAN_POINT ( 'NONE',  ( 4.893765752498283924E-17, -0.3996062992125986035, -1.811023622047244208 ) ) ;
#29093 = CARTESIAN_POINT ( 'NONE',  ( -0.5577427821522301654, -0.3162353388693405765, 0.4822834645669290543 ) ) ;
#29094 = CARTESIAN_POINT ( 'NONE',  ( -1.450131233595799651, 0.1771653543307087075, -0.09757992244046823083 ) ) ;
#29095 = CARTESIAN_POINT ( 'NONE',  ( 0.5380577427821529035, -0.3690944881889763329, 0.3153832671262228327 ) ) ;
#29096 = CARTESIAN_POINT ( 'NONE',  ( 1.213910761154856299, -0.6692913385826773087, -0.1292274648535924053 ) ) ;
#29097 = CARTESIAN_POINT ( 'NONE',  ( 0.4091458600556404646, -0.2362204724409448231, -0.6541994750656167090 ) ) ;
#29098 = CARTESIAN_POINT ( 'NONE',  ( 1.154855643044620184, -0.5023911411419708095, 0.1820866141732285504 ) ) ;
#29099 = EDGE_CURVE ( 'NONE', #13017, #2386, #83295, .T. ) ;
#29100 = CARTESIAN_POINT ( 'NONE',  ( 0.7283464566929140904, -0.5400638737290845981, -0.3530559997133363437 ) ) ;
#29101 = CARTESIAN_POINT ( 'NONE',  ( -0.2891555358219911054, 0.2891555358219909388, -0.7263779527559056648 ) ) ;
#29102 = CARTESIAN_POINT ( 'NONE',  ( -0.5446194225721777693, -0.3162353388693409650, -0.4822834645669289433 ) ) ;
#29103 = CARTESIAN_POINT ( 'NONE',  ( 0.5314960629921373636, 2.729657712569141026, -3.237502114873378023 ) ) ;
#29104 = CARTESIAN_POINT ( 'NONE',  ( 1.496062992125984703, -0.1870078740157480601, -0.3641732283464567677 ) ) ;
#29105 = CARTESIAN_POINT ( 'NONE',  ( -0.4921259842519677963, -0.5400638737290844871, 0.3530559997133364547 ) ) ;
#29106 = ADVANCED_FACE ( 'NONE', ( #3943 ), #22876, .F. ) ;
#29107 = CARTESIAN_POINT ( 'NONE',  ( 0.1974969037888706092, -0.3420746716998660508, -0.6410761154855643129 ) ) ;
#29108 = CARTESIAN_POINT ( 'NONE',  ( 1.430446194225722500, -0.4281496062992127816, -0.4176697321401328100 ) ) ;
#29109 = CARTESIAN_POINT ( 'NONE',  ( 0.06561679790026316017, 0.05413385826771626580, -0.4176697321401330321 ) ) ;
#29110 = CARTESIAN_POINT ( 'NONE',  ( 0.5708661417322842269, 0.07958543189024085140, 0.2665933059059887866 ) ) ;
#29111 = CARTESIAN_POINT ( 'NONE',  ( -0.3726288332202236653, -0.1208384647423932784, -1.929133858267952473 ) ) ;
#29112 = CARTESIAN_POINT ( 'NONE',  ( -0.1181102362204717315, -0.5511811023622047445, 6.969142054262312111E-17 ) ) ;
#29113 = CARTESIAN_POINT ( 'NONE',  ( -1.528871391076114250, -0.6692913385826771977, 0.1292274648535927661 ) ) ;
#29114 = CARTESIAN_POINT ( 'NONE',  ( 0.3996062992125984925, 0.1070741851644054637, -1.461286089238845065 ) ) ;
#29115 = CARTESIAN_POINT ( 'NONE',  ( 0.8202099737532814183, -0.6692913385826773087, -0.1292274648535924053 ) ) ;
#29116 = AXIS2_PLACEMENT_3D ( 'NONE', #57955, #45747, #26402 ) ;
#29117 = CARTESIAN_POINT ( 'NONE',  ( -0.1049643490035302024, -0.3917322834645671215, -1.166666666666666519 ) ) ;
#29118 = AXIS2_PLACEMENT_3D ( 'NONE', #55820, #67654, #23848 ) ;
#29119 = VECTOR ( 'NONE', #39758, 39.37007874015748143 ) ;
#29120 = CARTESIAN_POINT ( 'NONE',  ( 1.614173228346457378, -0.5511811023622047445, 6.969142054262312111E-17 ) ) ;
#29121 = CARTESIAN_POINT ( 'NONE',  ( -0.2898214735618663274, -0.2643935821217201498, -4.446769521226820888E-17 ) ) ;
#29122 = CARTESIAN_POINT ( 'NONE',  ( -0.1706036745406816491, -0.3690944881889763329, 0.3153832671262228327 ) ) ;
#29123 = CARTESIAN_POINT ( 'NONE',  ( 0.02624671916010564918, -0.6046776061558809534, -0.2411417322834644161 ) ) ;
#29124 = CARTESIAN_POINT ( 'NONE',  ( 1.266404199475066328, -0.2845877964562161244, -0.3641732283464567121 ) ) ;
#29125 = CARTESIAN_POINT ( 'NONE',  ( -1.325459317585300889, -0.3690944881889765550, -0.3153832671262227771 ) ) ;
#29126 = CARTESIAN_POINT ( 'NONE',  ( -1.253280839895012377, -0.05778040916215522460, 0.4822834645669289988 ) ) ;
#29127 = CARTESIAN_POINT ( 'NONE',  ( 0.5183727034120741983, -0.6692913385826771977, 0.1292274648535927661 ) ) ;
#29128 = EDGE_CURVE ( 'NONE', #15186, #47884, #55213, .T. ) ;
#29129 = CARTESIAN_POINT ( 'NONE',  ( 1.299212598425197429, -0.6692913385826771977, 8.415575281601705876E-17 ) ) ;
#29130 = CARTESIAN_POINT ( 'NONE',  ( 0.1181102362204724532, 0.04921259842519689481, 0.08523872084492503665 ) ) ;
#29131 = CARTESIAN_POINT ( 'NONE',  ( -0.04593175853018302557, -0.6692913385826773087, -0.1292274648535924053 ) ) ;
#29132 = CARTESIAN_POINT ( 'NONE',  ( 1.187664041994751285, -0.05778040916215522460, 0.4822834645669289988 ) ) ;
#29133 = CARTESIAN_POINT ( 'NONE',  ( 0.9186351706036752773, 0.2306618581243847221, -0.2411417322834647770 ) ) ;
#29134 = CARTESIAN_POINT ( 'NONE',  ( 1.614173228346456712, 2.401574803149606474, 0.1372047244094478646 ) ) ;
#29135 = CARTESIAN_POINT ( 'NONE',  ( 0.9514435695538062676, -0.2845877964562161244, -0.3641732283464567121 ) ) ;
#29136 = CARTESIAN_POINT ( 'NONE',  ( -1.522309711286088607, -0.5023911411419708095, 0.1820866141732285504 ) ) ;
#29137 = ADVANCED_FACE ( 'NONE', ( #36333 ), #18929, .T. ) ;
#29138 = CARTESIAN_POINT ( 'NONE',  ( -0.03280839895013062252, -0.5511811023622046335, 0.09757992244046803654 ) ) ;
#29139 = CARTESIAN_POINT ( 'NONE',  ( 0.05905511811023709395, -0.5400638737290844871, 0.3530559997133364547 ) ) ;
#29140 = CARTESIAN_POINT ( 'NONE',  ( 0.8202099737532813073, 0.2952755905511811885, 0.1292274648535926551 ) ) ;
#29141 = CARTESIAN_POINT ( 'NONE',  ( -0.2230971128608915943, 0.05413385826771666132, 0.4176697321401328100 ) ) ;
#29142 = CARTESIAN_POINT ( 'NONE',  ( -0.2427821522309703550, -0.08942795157528024563, -0.3641732283464568787 ) ) ;
#29143 = CARTESIAN_POINT ( 'NONE',  ( 0.8070866141732288002, 0.1660481256975885056, 0.3530559997133364547 ) ) ;
#29144 = CARTESIAN_POINT ( 'NONE',  ( 0.7808398950131241190, -0.08942795157528024563, -0.3641732283464568787 ) ) ;
#29145 = DIRECTION ( 'NONE',  ( 0.000000000000000000, 0.000000000000000000, 1.000000000000000000 ) ) ;
#29147 = CARTESIAN_POINT ( 'NONE',  ( 0.3996062992125985480, 0.1070741851644054637, -1.069553805774278166 ) ) ;
#29146 = PLANE ( 'NONE',  #51346 ) ;
#29148 = CARTESIAN_POINT ( 'NONE',  ( -0.2589415859896363470, 1.118607810292596705, 0.1761306047597130386 ) ) ;
#29149 = CARTESIAN_POINT ( 'NONE',  ( -1.259842519685038686, -0.1870078740157480879, -0.4822834645669291653 ) ) ;
#29150 = CARTESIAN_POINT ( 'NONE',  ( -0.6758530183727028406, -0.6692913385826773087, -0.1292274648535924053 ) ) ;
#29151 = CARTESIAN_POINT ( 'NONE',  ( 0.3458507752293908943, -0.3458507752293908943, -0.09842519685039372024 ) ) ;
#29152 = CARTESIAN_POINT ( 'NONE',  ( -0.3420746716998661618, 0.1974969037888702206, -2.545931758530183497 ) ) ;
#29153 = ORIENTED_EDGE ( 'NONE', *, *, #74789, .F. ) ;
#29154 = CARTESIAN_POINT ( 'NONE',  ( 0.8595800524934390507, -0.2845877964562159024, 0.3641732283464567677 ) ) ;
#29155 = CARTESIAN_POINT ( 'NONE',  ( 0.2867679344610365999, -0.2867679344610365444, -0.8779527559055116948 ) ) ;
#29156 = CARTESIAN_POINT ( 'NONE',  ( 0.9842519685039375910, 0.2952755905511811885, 0.000000000000000000 ) ) ;
#29157 = CARTESIAN_POINT ( 'NONE',  ( -0.1265901696524993347, 0.4724409448818895907, -2.368766404199475151 ) ) ;
#29158 = CARTESIAN_POINT ( 'NONE',  ( -1.430446194225721390, -0.3690944881889763329, 0.3153832671262228327 ) ) ;
#29159 = CARTESIAN_POINT ( 'NONE',  ( 1.541994750656168645, 0.2952755905511810774, -0.1292274648535930714 ) ) ;
#29160 = CARTESIAN_POINT ( 'NONE',  ( 1.423884514435696191, -0.08942795157527998196, 0.3641732283464567121 ) ) ;
#29161 = CARTESIAN_POINT ( 'NONE',  ( 0.3280839895013130669, -0.4281496062992127816, -0.4176697321401328100 ) ) ;
#29162 = AXIS2_PLACEMENT_3D ( 'NONE', #60822, #67158, #9487 ) ;
#29163 = CARTESIAN_POINT ( 'NONE',  ( -0.1958661417322836440, 0.3392501089628016664, -0.2506368521971635843 ) ) ;
#29164 = CARTESIAN_POINT ( 'NONE',  ( 0.1049868766404206816, 0.2306618581243848609, 0.2411417322834645549 ) ) ;
#29165 = CARTESIAN_POINT ( 'NONE',  ( -0.7020997375328076329, -0.2845877964562161244, -0.3641732283464567121 ) ) ;
#29166 = CARTESIAN_POINT ( 'NONE',  ( 0.8333333333333340365, 0.2952755905511810774, -0.1292274648535930714 ) ) ;
#29167 = CARTESIAN_POINT ( 'NONE',  ( -0.1246719160104980823, 0.2952755905511811885, 0.1292274648535926551 ) ) ;
#29168 = CARTESIAN_POINT ( 'NONE',  ( -0.4724409448818898682, -8.678599364036362592E-17, -0.2736220472440945017 ) ) ;
#29169 = AXIS2_PLACEMENT_3D ( 'NONE', #61825, #81620, #17235 ) ;
#29170 = CARTESIAN_POINT ( 'NONE',  ( -0.1265901696524993347, 0.4724409448818896462, -1.108923884514435798 ) ) ;
#29171 = CARTESIAN_POINT ( 'NONE',  ( -0.1958661417322833942, -0.3392501089628018884, -1.794638738354017660 ) ) ;
#29172 = CARTESIAN_POINT ( 'NONE',  ( 0.8464566929133866546, -0.5400638737290844871, 0.3530559997133364547 ) ) ;
#29173 = AXIS2_PLACEMENT_3D ( 'NONE', #57732, #5985, #5167 ) ;
#29174 = CIRCLE ( 'NONE', #70809, 0.1978346456692914035 ) ;
#29175 = CARTESIAN_POINT ( 'NONE',  ( -0.03937007874015669567, -0.6692913385826771977, 8.415575281601705876E-17 ) ) ;
#29176 = CARTESIAN_POINT ( 'NONE',  ( -0.8595800524934373854, -0.05778040916215522460, 0.4822834645669289988 ) ) ;
#29177 = CARTESIAN_POINT ( 'NONE',  ( 1.233595800524935227, -0.6046776061558807314, 0.2411417322834647770 ) ) ;
#29178 = CARTESIAN_POINT ( 'NONE',  ( 0.6561679790026253567, -0.6046776061558809534, -0.2411417322834644161 ) ) ;
#29179 = CARTESIAN_POINT ( 'NONE',  ( -0.3917322834645671215, 0.1049643490035301469, -1.062335958005249603 ) ) ;
#29180 = CARTESIAN_POINT ( 'NONE',  ( -0.3805774278215216522, -0.4281496062992127816, -0.4176697321401328100 ) ) ;
#29181 = CARTESIAN_POINT ( 'NONE',  ( 0.5577427821522316087, -0.05778040916215522460, 0.4822834645669289988 ) ) ;
#29182 = CARTESIAN_POINT ( 'NONE',  ( -0.1443569553805765515, -0.4281496062992127816, -0.4176697321401328100 ) ) ;
#29183 = CARTESIAN_POINT ( 'NONE',  ( 0.5905511811023629321, 0.1771653543307087630, 0.000000000000000000 ) ) ;
#29184 = CARTESIAN_POINT ( 'NONE',  ( -1.568241469816272105, -0.05778040916215522460, 0.4822834645669289988 ) ) ;
#29185 = CARTESIAN_POINT ( 'NONE',  ( -0.4477123500621962293, 1.379796003448452435, -2.610391114557127690 ) ) ;
#29186 = CARTESIAN_POINT ( 'NONE',  ( 0.4002624671916016896, -0.3162353388693409650, -0.4822834645669289433 ) ) ;
#29187 = PRESENTATION_STYLE_ASSIGNMENT (( #55667 ) ) ;
#29188 = CARTESIAN_POINT ( 'NONE',  ( -0.1958661417322836718, 0.3392501089628017219, -2.524934383202099397 ) ) ;
#29189 = VERTEX_POINT ( 'NONE', #30429 ) ;
#29190 = VERTEX_POINT ( 'NONE', #81799 ) ;
#29191 = CARTESIAN_POINT ( 'NONE',  ( 0.6233595800524942554, -0.05778040916215560624, -0.4822834645669293319 ) ) ;
#29192 = CARTESIAN_POINT ( 'NONE',  ( 0.6430446194225728496, -0.004921259842519576551, 0.3153832671262227771 ) ) ;
#29194 = CARTESIAN_POINT ( 'NONE',  ( 4.773229650219999425E-16, 0.000000000000000000, -3.858267716535433323 ) ) ;
#29193 = DIRECTION ( 'NONE',  ( -8.673617379884022653E-16, 1.000000000000000000, -3.028377322213053966E-30 ) ) ;
#29195 = CARTESIAN_POINT ( 'NONE',  ( -0.3392501089628017219, -0.1958661417322836718, -0.9245406824146982228 ) ) ;
#29196 = CARTESIAN_POINT ( 'NONE',  ( -0.4359958488159856316, 1.724409448818897905, 3.912791665790197992 ) ) ;
#29197 = LINE ( 'NONE', #54443, #45891 ) ;
#29198 = CARTESIAN_POINT ( 'NONE',  ( -0.3917322834645671215, 0.1049643490035301469, -1.219816272965879023 ) ) ;
#29199 = EDGE_CURVE ( 'NONE', #64485, #18885, #67225, .T. ) ;
#29200 = CARTESIAN_POINT ( 'NONE',  ( 0.1070741851644053388, 0.3996062992125986035, -2.589895013123359568 ) ) ;
#29201 = CARTESIAN_POINT ( 'NONE',  ( 1.023622047244095112, -0.1870078740157480879, -0.4822834645669291653 ) ) ;
#29202 = CARTESIAN_POINT ( 'NONE',  ( -1.010498687664041384, 0.05413385826771666132, 0.4176697321401328100 ) ) ;
#29203 = CARTESIAN_POINT ( 'NONE',  ( -0.8202099737532801971, -0.6692913385826771977, 0.1292274648535927661 ) ) ;
#29204 = CARTESIAN_POINT ( 'NONE',  ( 0.7283464566929140904, -0.5400638737290845981, -0.3530559997133363437 ) ) ;
#29205 = CARTESIAN_POINT ( 'NONE',  ( 1.213910761154856299, -0.6692913385826773087, -0.1292274648535924053 ) ) ;
#29206 = CARTESIAN_POINT ( 'NONE',  ( -1.111516660996405559, 1.088445792224367326, 0.1541100987596267513 ) ) ;
#29207 = PRODUCT_CONTEXT ( 'NONE', #25567, 'mechanical' ) ;
#29208 = CARTESIAN_POINT ( 'NONE',  ( 1.286089238845145033, -0.5023911411419708095, -0.1820866141732282451 ) ) ;
#29209 = CARTESIAN_POINT ( 'NONE',  ( -0.2952755905511810774, 3.616083068348483797E-17, -1.220472440944881942 ) ) ;
#29210 = CARTESIAN_POINT ( 'NONE',  ( -1.437007874015747477, 0.07958543189024071263, -0.2665933059059888421 ) ) ;
#29211 = FACE_BOUND ( 'NONE', #72022, .T. ) ;
#29212 = CARTESIAN_POINT ( 'NONE',  ( 0.006561679790026889343, -0.3162353388693409650, -0.4822834645669289433 ) ) ;
#29214 = DIRECTION ( 'NONE',  ( -1.000000000000000000, 0.000000000000000000, 0.000000000000000000 ) ) ;
#29213 = CARTESIAN_POINT ( 'NONE',  ( 1.528871391076116026, 0.2952755905511811885, 0.1292274648535926551 ) ) ;
#29215 = CARTESIAN_POINT ( 'NONE',  ( -1.161417322834644716, -0.4536011799217368745, -0.2665933059059886201 ) ) ;
#29216 = CARTESIAN_POINT ( 'NONE',  ( 0.4199475065616805614, 0.2306618581243848609, 0.2411417322834645549 ) ) ;
#29217 = CARTESIAN_POINT ( 'NONE',  ( 1.259842519685040019, -0.1870078740157479769, 0.3641732283464567677 ) ) ;
#29218 = CARTESIAN_POINT ( 'NONE',  ( -0.3917322834645670659, 0.1049643490035301607, -1.057723466370391829 ) ) ;
#29219 = CARTESIAN_POINT ( 'NONE',  ( -1.148293963254592542, -0.5511811023622048555, -0.09757992244046775898 ) ) ;
#29220 = CARTESIAN_POINT ( 'NONE',  ( 1.522309711286089939, 0.2306618581243848609, 0.2411417322834645549 ) ) ;
#29221 = FACE_BOUND ( 'NONE', #40771, .T. ) ;
#29222 = CARTESIAN_POINT ( 'NONE',  ( -0.1115485564304456306, 0.2952755905511810774, -0.1292274648535930714 ) ) ;
#29223 = CARTESIAN_POINT ( 'NONE',  ( -1.279527559055116948, 0.07958543189024071263, -0.2665933059059888421 ) ) ;
#29224 = CARTESIAN_POINT ( 'NONE',  ( -0.5183727034120726440, -0.6692913385826773087, -0.1292274648535924053 ) ) ;
#29225 = CARTESIAN_POINT ( 'NONE',  ( -1.646981627296586703, -0.08942795157527998196, 0.3641732283464567121 ) ) ;
#29226 = CARTESIAN_POINT ( 'NONE',  ( -0.3392501089628017219, -0.1958661417322836995, -0.6791531740495557745 ) ) ;
#29227 = CARTESIAN_POINT ( 'NONE',  ( 0.1246719160104994284, -0.6692913385826771977, 0.1292274648535927661 ) ) ;
#29228 = CIRCLE ( 'NONE', #76276, 2.598425196850393970 ) ;
#29229 = CARTESIAN_POINT ( 'NONE',  ( 1.410761154855643795, -0.3162353388693405765, 0.4822834645669290543 ) ) ;
#29230 = AXIS2_PLACEMENT_3D ( 'NONE', #15073, #40731, #66415 ) ;
#29231 = CARTESIAN_POINT ( 'NONE',  ( 0.4724409448818898682, 2.892866454678787531E-17, -2.084645669291338432 ) ) ;
#29232 = CARTESIAN_POINT ( 'NONE',  ( -1.266404199475064773, -0.3162353388693405765, 0.4822834645669290543 ) ) ;
#29233 = CARTESIAN_POINT ( 'NONE',  ( -0.6692913385826764205, -0.5511811023622047445, 6.969142054262312111E-17 ) ) ;
#29234 = DIRECTION ( 'NONE',  ( 1.000000000000000000, -0.000000000000000000, -0.000000000000000000 ) ) ;
#29235 = CARTESIAN_POINT ( 'NONE',  ( -0.02624671916010428221, 0.2306618581243847221, -0.2411417322834647770 ) ) ;
#29236 = CARTESIAN_POINT ( 'NONE',  ( 0.5249343832021005074, -0.5023911411419708095, 0.1820866141732285504 ) ) ;
#29237 = CARTESIAN_POINT ( 'NONE',  ( -1.056430446194224881, 0.1771653543307087075, -0.09757992244046823083 ) ) ;
#29238 = CARTESIAN_POINT ( 'NONE',  ( -1.351706036745406347, 0.05413385826771626580, -0.4176697321401330321 ) ) ;
#29239 = CARTESIAN_POINT ( 'NONE',  ( -1.614173228346456268, -0.6692913385826771977, 8.415575281601705876E-17 ) ) ;
#29240 = CARTESIAN_POINT ( 'NONE',  ( 1.358267716535433323, 0.1660481256975885056, 0.3530559997133364547 ) ) ;
#29241 = CARTESIAN_POINT ( 'NONE',  ( -6.686372609646914991E-25, 1.062992125984252745, 1.850393700787401619 ) ) ;
#29242 = CARTESIAN_POINT ( 'NONE',  ( 0.4855643044619430415, -0.3690944881889765550, -0.3153832671262227771 ) ) ;
#29243 = CARTESIAN_POINT ( 'NONE',  ( 0.9448818897637802916, -0.1870078740157480879, -0.4822834645669291653 ) ) ;
#29244 = LINE ( 'NONE', #24465, #23248 ) ;
#29245 = CARTESIAN_POINT ( 'NONE',  ( 1.594488188976378673, 0.07958543189024085140, 0.2665933059059887866 ) ) ;
#29246 = ORIENTED_EDGE ( 'NONE', *, *, #67169, .T. ) ;
#29247 = CARTESIAN_POINT ( 'NONE',  ( -1.115485564304461219, 0.05413385826771626580, -0.4176697321401330321 ) ) ;
#29248 = CARTESIAN_POINT ( 'NONE',  ( -0.9186351706036736120, -0.6046776061558809534, -0.2411417322834644161 ) ) ;
#29249 = CARTESIAN_POINT ( 'NONE',  ( 0.3543307086614179147, 0.2952755905511811885, 0.000000000000000000 ) ) ;
#29250 = CARTESIAN_POINT ( 'NONE',  ( 0.5400834452262274210, 1.809133623825372073E-16, -0.3954985857520062487 ) ) ;
#29251 = CARTESIAN_POINT ( 'NONE',  ( -0.3996062992125984925, -0.1070741851644056858, -2.012467191601049699 ) ) ;
#29252 = CARTESIAN_POINT ( 'NONE',  ( 1.010498687664042716, 0.05413385826771626580, -0.4176697321401330321 ) ) ;
#29253 = CARTESIAN_POINT ( 'NONE',  ( 1.463254593175853824, 0.1771653543307087075, -0.09757992244046823083 ) ) ;
#29254 = CARTESIAN_POINT ( 'NONE',  ( 0.4724409448818904789, -0.1870078740157480879, -0.4822834645669291653 ) ) ;
#29255 = CARTESIAN_POINT ( 'NONE',  ( 0.6233595800524939223, -0.3162353388693405765, 0.4822834645669290543 ) ) ;
#29256 = CARTESIAN_POINT ( 'NONE',  ( -9.787531504996567848E-17, 0.3996062992125986035, -1.889763779527559251 ) ) ;
#29257 = CARTESIAN_POINT ( 'NONE',  ( -0.3949938075777409963, -7.255918531996591613E-17, -1.141732283464566899 ) ) ;
#29258 = CARTESIAN_POINT ( 'NONE',  ( -0.1998031496062994683, 0.3460692066303958092, -2.532808398950130879 ) ) ;
#29259 = CARTESIAN_POINT ( 'NONE',  ( -0.7426113562971995430, 1.972848275015057995, -0.5309055118110235227 ) ) ;
#29260 = CARTESIAN_POINT ( 'NONE',  ( -0.3392501089628019995, 0.1958661417322832277, -0.1758530183727033402 ) ) ;
#29261 = CARTESIAN_POINT ( 'NONE',  ( -0.05905511811023545637, -0.4536011799217368745, -0.2665933059059886201 ) ) ;
#29262 = CARTESIAN_POINT ( 'NONE',  ( -0.2099737532808391705, -0.6046776061558809534, -0.2411417322834644161 ) ) ;
#29263 = CARTESIAN_POINT ( 'NONE',  ( 0.8989501312335963501, -0.6692913385826773087, -0.1292274648535924053 ) ) ;
#29264 = CARTESIAN_POINT ( 'NONE',  ( -0.2891555358219911054, 0.2891555358219909388, -2.143700787401574548 ) ) ;
#29265 = CARTESIAN_POINT ( 'NONE',  ( 0.04593175853018440641, -0.5511811023622046335, 0.09757992244046803654 ) ) ;
#29266 = CARTESIAN_POINT ( 'NONE',  ( -1.102362204724408601, -0.1870078740157480879, -0.4822834645669291653 ) ) ;
#29267 = CARTESIAN_POINT ( 'NONE',  ( 1.102362204724410155, -0.1870078740157479769, 0.4822834645669291653 ) ) ;
#29268 = CARTESIAN_POINT ( 'NONE',  ( 0.4724409448818896462, 0.1265901696524990294, -2.644356955380577912 ) ) ;
#29269 = CARTESIAN_POINT ( 'NONE',  ( -0.3996062992125986035, -0.1070741851644056997, -1.935695538057742526 ) ) ;
#29270 = DIRECTION ( 'NONE',  ( 0.000000000000000000, 0.000000000000000000, 1.000000000000000000 ) ) ;
#29271 = B_SPLINE_CURVE_WITH_KNOTS ( 'NONE', 3,
 ( #55322, #42697, #67978, #17058, #17875, #43509, #50246, #80620, #68394, #10733, #23757, #75942 ),
 .UNSPECIFIED., .F., .F.,
 ( 4, 2, 2, 2, 2, 4 ),
 ( 0.007992874908874989665, 0.009303755029337034896, 0.01061463514979908013, 0.01192551527026112709, 0.01258095533049215925, 0.01323639539072319141 ),
 .UNSPECIFIED. ) ;
#29272 = ORIENTED_EDGE ( 'NONE', *, *, #31494, .T. ) ;
#29273 = CARTESIAN_POINT ( 'NONE',  ( 1.043307086614173818, -0.5400638737290845981, -0.3530559997133363437 ) ) ;
#29274 = CARTESIAN_POINT ( 'NONE',  ( 1.292650918635171564, 0.1771653543307087630, 0.09757992244046791164 ) ) ;
#29276 = CARTESIAN_POINT ( 'NONE',  ( -1.404199475065615932, -0.4281496062992127816, -0.4176697321401328100 ) ) ;
#29275 = CARTESIAN_POINT ( 'NONE',  ( -1.417322834645668772, -0.1870078740157480601, -0.3641732283464567677 ) ) ;
#29277 = CARTESIAN_POINT ( 'NONE',  ( -0.1958661417322834220, -0.3392501089628018884, 0.1646981627296586759 ) ) ;
#29278 = DIRECTION ( 'NONE',  ( 9.381338752702757898E-17, -0.6427876096865366984, 0.7660444431189802339 ) ) ;
#29279 = CARTESIAN_POINT ( 'NONE',  ( 1.338582677165355062, -0.1870078740157479769, 0.4822834645669291653 ) ) ;
#29280 = CARTESIAN_POINT ( 'NONE',  ( -1.522309711286088607, 0.2306618581243847221, -0.2411417322834647770 ) ) ;
#29281 = CARTESIAN_POINT ( 'NONE',  ( 0.1246719160104994284, -0.6692913385826771977, 0.1292274648535927661 ) ) ;
#29282 = CARTESIAN_POINT ( 'NONE',  ( -0.5577427821522301654, -0.05778040916215560624, -0.4822834645669293319 ) ) ;
#29283 = CARTESIAN_POINT ( 'NONE',  ( 1.430446194225722500, 0.05413385826771666132, 0.4176697321401328100 ) ) ;
#29284 = CARTESIAN_POINT ( 'NONE',  ( -0.1958661417322834220, -0.3392501089628018884, -0.1502624671916011345 ) ) ;
#29285 = ADVANCED_FACE ( 'NONE', ( #55263 ), #11320, .F. ) ;
#29286 = CARTESIAN_POINT ( 'NONE',  ( 0.3280839895013130669, 0.05413385826771666132, 0.4176697321401328100 ) ) ;
#29287 = CARTESIAN_POINT ( 'NONE',  ( -0.3392501089628017219, -0.1958661417322836718, -2.406824146981627166 ) ) ;
#29288 = CARTESIAN_POINT ( 'NONE',  ( 1.541994750656168645, 0.2952755905511810774, -0.1292274648535930714 ) ) ;
#29289 = ORIENTED_EDGE ( 'NONE', *, *, #65634, .T. ) ;
#29290 = CARTESIAN_POINT ( 'NONE',  ( -0.1974969037888706647, 0.3420746716998658843, -2.532808398950130879 ) ) ;
#29291 = VERTEX_POINT ( 'NONE', #40612 ) ;
#29292 = CARTESIAN_POINT ( 'NONE',  ( 0.4849061582275024929, 1.726086921369708538, -0.4921425059946356040 ) ) ;
#29293 = AXIS2_PLACEMENT_3D ( 'NONE', #35767, #36175, #61848 ) ;
#29294 = CARTESIAN_POINT ( 'NONE',  ( -1.725721784776902190, -0.05778040916215522460, 0.4822834645669289988 ) ) ;
#29295 = CARTESIAN_POINT ( 'NONE',  ( -0.1998031496062991907, -0.3460692066303959757, -0.8530183727034120755 ) ) ;
#29296 = CARTESIAN_POINT ( 'NONE',  ( -0.1450607720586916394, 0.000000000000000000, 0.3464511005275205946 ) ) ;
#29297 = DIRECTION ( 'NONE',  ( 0.000000000000000000, 1.000000000000000000, 0.000000000000000000 ) ) ;
#29298 = LINE ( 'NONE', #22156, #63851 ) ;
#29299 = CARTESIAN_POINT ( 'NONE',  ( 0.1208384647389237204, -0.3726288332213487653, -2.755905511811024056 ) ) ;
#29300 = CARTESIAN_POINT ( 'NONE',  ( -0.1049643490035307020, 0.3917322834645669549, 0.06627296587926499727 ) ) ;
#29301 = CARTESIAN_POINT ( 'NONE',  ( -0.4658792650918627265, -0.2845877964562161244, -0.3641732283464567121 ) ) ;
#29302 = CARTESIAN_POINT ( 'NONE',  ( -1.141732283464566011, -0.5511811023622047445, 6.969142054262312111E-17 ) ) ;
#29303 = CARTESIAN_POINT ( 'NONE',  ( -1.141732283464566011, 0.2952755905511811885, 0.000000000000000000 ) ) ;
#29304 = CARTESIAN_POINT ( 'NONE',  ( 0.3871391076115492380, -0.05778040916215560624, -0.4822834645669293319 ) ) ;
#29305 = CARTESIAN_POINT ( 'NONE',  ( -1.299212598425196097, 0.2952755905511811885, 0.000000000000000000 ) ) ;
#29306 = DIRECTION ( 'NONE',  ( 0.000000000000000000, -1.000000000000000000, 1.734723475976805615E-16 ) ) ;
#29307 = EDGE_LOOP ( 'NONE', ( #76060, #8054, #13747, #44381 ) ) ;
#29308 = CARTESIAN_POINT ( 'NONE',  ( -1.417322834645668772, -0.1870078740157480879, -0.4822834645669291653 ) ) ;
#29309 = DIRECTION ( 'NONE',  ( -0.000000000000000000, -1.000000000000000000, -0.000000000000000000 ) ) ;
#29310 =( CONVERSION_BASED_UNIT ( 'INCH', #17525 ) LENGTH_UNIT ( ) NAMED_UNIT ( #50239 ) );
#29311 = CARTESIAN_POINT ( 'NONE',  ( -0.4091458600556402980, -0.2362204724409451284, -1.627296587926509330 ) ) ;
#29312 = DIRECTION ( 'NONE',  ( -0.7119855458575274909, 0.7021941202331152265, 0.000000000000000000 ) ) ;
#29313 = CARTESIAN_POINT ( 'NONE',  ( 0.2867679344610365999, -0.2867679344610365444, -0.5629921259842519676 ) ) ;
#29314 = CARTESIAN_POINT ( 'NONE',  ( 0.4849061582275024929, 1.568468489416427580, -0.4921425059946356040 ) ) ;
#29315 = CARTESIAN_POINT ( 'NONE',  ( -0.9251968503937002541, -0.5400638737290845981, -0.3530559997133363437 ) ) ;
#29316 = CARTESIAN_POINT ( 'NONE',  ( 1.325459317585302665, -0.4281496062992124485, 0.4176697321401328655 ) ) ;
#29318 = CARTESIAN_POINT ( 'NONE',  ( -0.4603267246303611726, 1.653225543546885223, 2.586063147568501641 ) ) ;
#29317 = DIRECTION ( 'NONE',  ( 0.8660254037844363761, 0.000000000000000000, 0.5000000000000038858 ) ) ;
#29319 = CARTESIAN_POINT ( 'NONE',  ( 1.509186351706037543, 0.05413385826771666132, 0.4176697321401328100 ) ) ;
#29320 = CARTESIAN_POINT ( 'NONE',  ( -0.7939632545931754048, -0.3162353388693405765, 0.4822834645669290543 ) ) ;
#29321 = CARTESIAN_POINT ( 'NONE',  ( -0.1049643490035301746, -0.3917322834645670659, 0.005268659613860090553 ) ) ;
#29322 = CARTESIAN_POINT ( 'NONE',  ( 0.1246719160104994284, -0.5511811023622046335, 0.09757992244046803654 ) ) ;
#29323 = CARTESIAN_POINT ( 'NONE',  ( -0.3917322834645670104, -7.196005306013484475E-17, -0.4389763779527560139 ) ) ;
#29324 = CARTESIAN_POINT ( 'NONE',  ( -0.07217847769028787330, -0.08942795157527998196, 0.3641732283464567121 ) ) ;
#29325 = CARTESIAN_POINT ( 'NONE',  ( 0.8333333333333340365, 0.1771653543307087075, -0.09757992244046823083 ) ) ;
#29326 = CARTESIAN_POINT ( 'NONE',  ( 0.6233595800524939223, -0.3162353388693405765, 0.4822834645669290543 ) ) ;
#29327 = CARTESIAN_POINT ( 'NONE',  ( -0.3871391076115476282, -0.08942795157527998196, 0.3641732283464567121 ) ) ;
#29328 = CARTESIAN_POINT ( 'NONE',  ( 0.3917322834645670104, -0.1049643490035303411, -2.465879265091863282 ) ) ;
#29329 = CARTESIAN_POINT ( 'NONE',  ( -1.574803149606298192, -0.1870078740157480879, -0.4822834645669291653 ) ) ;
#29330 = CARTESIAN_POINT ( 'NONE',  ( -1.456692913385826182, 0.1771653543307087630, 0.000000000000000000 ) ) ;
#29331 = CARTESIAN_POINT ( 'NONE',  ( -0.3458507752293909498, 0.3458507752293907833, -0.7263779527559056648 ) ) ;
#29332 = CARTESIAN_POINT ( 'NONE',  ( 0.05905511811023681640, 0.1660481256975883668, -0.3530559997133364547 ) ) ;
#29333 = CARTESIAN_POINT ( 'NONE',  ( -0.5905511811023613777, -0.6692913385826771977, 8.415575281601705876E-17 ) ) ;
#29334 = CARTESIAN_POINT ( 'NONE',  ( 1.594488188976378673, -0.4536011799217368745, -0.2665933059059886201 ) ) ;
#29335 = CARTESIAN_POINT ( 'NONE',  ( 0.4461942257217855201, -0.5023911411419708095, 0.1820866141732285504 ) ) ;
#29336 = CARTESIAN_POINT ( 'NONE',  ( -0.4133858267716528645, 0.1660481256975883668, -0.3530559997133364547 ) ) ;
#29337 = CARTESIAN_POINT ( 'NONE',  ( -0.7808398950131222316, -0.3162353388693409650, -0.4822834645669289433 ) ) ;
#29338 = DIRECTION ( 'NONE',  ( 0.7071067811865489050, 2.189697074797801291E-16, -0.7071067811865460184 ) ) ;
#29339 = CARTESIAN_POINT ( 'NONE',  ( 1.535433070866142558, 0.1771653543307087630, 0.000000000000000000 ) ) ;
#29340 = CARTESIAN_POINT ( 'NONE',  ( -0.05249343832020911260, 0.2306618581243848609, 0.2411417322834645549 ) ) ;
#29341 = ORIENTED_EDGE ( 'NONE', *, *, #42486, .T. ) ;
#29342 = CARTESIAN_POINT ( 'NONE',  ( 0.3996062992125984925, 0.1070741851644054637, -1.618766404199474929 ) ) ;
#29343 = DIRECTION ( 'NONE',  ( 0.000000000000000000, 0.000000000000000000, 1.000000000000000000 ) ) ;
#29344 = CARTESIAN_POINT ( 'NONE',  ( -0.2165354330708654795, -0.4536011799217368745, -0.2665933059059886201 ) ) ;
#29345 = AXIS2_PLACEMENT_3D ( 'NONE', #58749, #1111, #38967 ) ;
#29346 = CARTESIAN_POINT ( 'NONE',  ( -0.4658792650918627265, -0.05778040916215522460, 0.4822834645669289988 ) ) ;
#29347 = CARTESIAN_POINT ( 'NONE',  ( -1.476377952755905110, 0.07958543189024085140, 0.2665933059059887866 ) ) ;
#29348 = CARTESIAN_POINT ( 'NONE',  ( 1.213910761154856299, 0.2952755905511811885, 0.1292274648535926551 ) ) ;
#29349 = CARTESIAN_POINT ( 'NONE',  ( -1.423884514435694859, -0.05778040916215560624, -0.4822834645669293319 ) ) ;
#29350 = CARTESIAN_POINT ( 'NONE',  ( -0.4921259842519677963, -0.4536011799217367080, 0.2665933059059888421 ) ) ;
#29351 = CARTESIAN_POINT ( 'NONE',  ( -0.3460692066303960313, 0.1998031496062989965, -0.1030183727034120894 ) ) ;
#29352 = CARTESIAN_POINT ( 'NONE',  ( -0.3996062992125986035, -0.1070741851644056997, -0.6758530183727035068 ) ) ;
#29353 = CARTESIAN_POINT ( 'NONE',  ( -0.1974969037888703871, -0.3420746716998661063, 0.09186351706036739728 ) ) ;
#29354 = CARTESIAN_POINT ( 'NONE',  ( 1.666666666666667185, -0.004921259842519576551, 0.3153832671262227771 ) ) ;
#29355 = CARTESIAN_POINT ( 'NONE',  ( 1.167979002624672580, -0.004921259842519870586, -0.3153832671262229437 ) ) ;
#29356 = CARTESIAN_POINT ( 'NONE',  ( 1.003937007874016185, 0.1660481256975883668, -0.3530559997133364547 ) ) ;
#29357 = DIRECTION ( 'NONE',  ( 0.000000000000000000, 0.000000000000000000, -1.000000000000000000 ) ) ;
#29358 = CARTESIAN_POINT ( 'NONE',  ( 1.017060367454068581, -0.05778040916215560624, -0.4822834645669293319 ) ) ;
#29359 = CARTESIAN_POINT ( 'NONE',  ( -0.3949938075777409963, -7.255918531996591613E-17, -0.7460629921259843700 ) ) ;
#29360 = CARTESIAN_POINT ( 'NONE',  ( 1.430446194225722500, -0.3690944881889765550, -0.3153832671262227771 ) ) ;
#29361 = CARTESIAN_POINT ( 'NONE',  ( 0.1574803149606306130, -0.1870078740157480879, -0.4822834645669291653 ) ) ;
#29362 = CARTESIAN_POINT ( 'NONE',  ( -0.6758530183727028406, 0.2952755905511811885, 0.1292274648535926551 ) ) ;
#29363 = DIRECTION ( 'NONE',  ( 1.000000000000000000, 0.000000000000000000, 0.000000000000000000 ) ) ;
#29364 = CARTESIAN_POINT ( 'NONE',  ( -0.1265901696524986964, -0.4724409448818899238, -1.017060367454067915 ) ) ;
#29365 = CARTESIAN_POINT ( 'NONE',  ( -0.3460692066303958092, -0.1998031496062994683, -2.414698162729658648 ) ) ;
#29366 = CARTESIAN_POINT ( 'NONE',  ( 0.2690288713910767848, -0.5511811023622048555, -0.09757992244046775898 ) ) ;
#29367 = VERTEX_POINT ( 'NONE', #53225 ) ;
#29368 = CARTESIAN_POINT ( 'NONE',  ( 0.3917322834645670659, 2.398668435337828261E-17, -0.5872896569891882246 ) ) ;
#29369 = ORIENTED_EDGE ( 'NONE', *, *, #49189, .T. ) ;
#29370 = CARTESIAN_POINT ( 'NONE',  ( -0.5905511811023615998, 0.2952755905511811885, 0.000000000000000000 ) ) ;
#29371 = CARTESIAN_POINT ( 'NONE',  ( -0.3740157480314953431, 0.1660481256975885056, 0.3530559997133364547 ) ) ;
#29372 = CARTESIAN_POINT ( 'NONE',  ( -0.2887139107611542133, -0.6046776061558809534, -0.2411417322834644161 ) ) ;
#29373 = CARTESIAN_POINT ( 'NONE',  ( 0.7939632545931766261, -0.3162353388693409650, -0.4822834645669289433 ) ) ;
#29374 = CARTESIAN_POINT ( 'NONE',  ( -0.8923884514435688198, -0.6046776061558807314, 0.2411417322834647770 ) ) ;
#29375 = CARTESIAN_POINT ( 'NONE',  ( -0.3018372703412066094, 0.05413385826771666132, 0.4176697321401328100 ) ) ;
#29376 = CARTESIAN_POINT ( 'NONE',  ( 1.305774278215223960, 0.2952755905511810774, -0.1292274648535930714 ) ) ;
#29377 = CARTESIAN_POINT ( 'NONE',  ( 0.2887139107611556010, -0.6046776061558807314, 0.2411417322834647770 ) ) ;
#29378 = CARTESIAN_POINT ( 'NONE',  ( 0.8727034120734913358, -0.05778040916215522460, 0.4822834645669289988 ) ) ;
#29379 = EDGE_CURVE ( 'NONE', #57515, #1754, #8038, .T. ) ;
#29380 = CARTESIAN_POINT ( 'NONE',  ( 0.3917322834645670104, 2.398668435337828261E-17, -1.212598425196850238 ) ) ;
#29381 = CARTESIAN_POINT ( 'NONE',  ( 0.2099737532808405305, -0.5023911411419708095, 0.1820866141732285504 ) ) ;
#29382 = ORIENTED_EDGE ( 'NONE', *, *, #45564, .T. ) ;
#29383 = CARTESIAN_POINT ( 'NONE',  ( -0.2891555358219908833, -0.2891555358219912164, -0.8464566929133858775 ) ) ;
#29384 = VERTEX_POINT ( 'NONE', #54475 ) ;
#29385 = CARTESIAN_POINT ( 'NONE',  ( -0.7349081364829390672, 0.1283753931104746893, -0.1820866141732285504 ) ) ;
#29386 = CARTESIAN_POINT ( 'NONE',  ( -0.4921259842519677963, 0.1660481256975883668, -0.3530559997133364547 ) ) ;
#29387 = CARTESIAN_POINT ( 'NONE',  ( -1.393803226718939747, 1.220767705744369547, 0.3535424564827598926 ) ) ;
#29388 = CARTESIAN_POINT ( 'NONE',  ( -0.5118110236220466680, -0.6692913385826771977, 8.415575281601705876E-17 ) ) ;
#29389 = CARTESIAN_POINT ( 'NONE',  ( -0.2165354330708654795, -0.5400638737290845981, -0.3530559997133363437 ) ) ;
#29390 = CARTESIAN_POINT ( 'NONE',  ( -1.128608923884513837, 0.2306618581243847221, -0.2411417322834647770 ) ) ;
#29391 = CARTESIAN_POINT ( 'NONE',  ( -1.568241469816272105, -0.05778040916215522460, 0.4822834645669289988 ) ) ;
#29392 = CARTESIAN_POINT ( 'NONE',  ( 0.9645669291338591078, -0.4536011799217368745, -0.2665933059059886201 ) ) ;
#29393 = CARTESIAN_POINT ( 'NONE',  ( -0.7874015748031497619, 1.968503937007873850, 0.000000000000000000 ) ) ;
#29394 = CARTESIAN_POINT ( 'NONE',  ( 0.4091458600556404646, -0.2362204724409448231, -0.6541994750656167090 ) ) ;
#29395 = CARTESIAN_POINT ( 'NONE',  ( 0.5052493438320215802, 0.1771653543307087630, 0.09757992244046791164 ) ) ;
#29396 = CARTESIAN_POINT ( 'NONE',  ( -0.1115485564304453947, -0.6692913385826771977, 0.1292274648535927661 ) ) ;
#29397 = CARTESIAN_POINT ( 'NONE',  ( 0.01968503937007957949, -0.5400638737290845981, -0.3530559997133363437 ) ) ;
#29398 = EDGE_LOOP ( 'NONE', ( #25434, #26055, #70171, #15332, #9097, #56692 ) ) ;
#29399 = CARTESIAN_POINT ( 'NONE',  ( -0.3996062992125987146, 0.1070741851644051862, -1.765091863517059823 ) ) ;
#29400 = DIRECTION ( 'NONE',  ( 1.000000000000000000, 0.000000000000000000, 3.455050906509825972E-15 ) ) ;
#29401 = VERTEX_POINT ( 'NONE', #78939 ) ;
#29402 = CARTESIAN_POINT ( 'NONE',  ( 0.3460692066303959202, -0.1998031496062991630, -1.284120734908136496 ) ) ;
#29403 = CARTESIAN_POINT ( 'NONE',  ( -0.03175677952935525988, 0.3980111619244049992, -2.755905511811024500 ) ) ;
#29404 = CARTESIAN_POINT ( 'NONE',  ( -0.7677165354330699465, 0.07958543189024085140, 0.2665933059059887866 ) ) ;
#29405 = CARTESIAN_POINT ( 'NONE',  ( -0.9580052493438311334, -0.4281496062992124485, 0.4176697321401328655 ) ) ;
#29406 = CARTESIAN_POINT ( 'NONE',  ( -0.4724409448818899238, 0.1265901696524986686, -0.3477690288713909950 ) ) ;
#29407 = CARTESIAN_POINT ( 'NONE',  ( -0.2867679344610364334, -0.2867679344610367109, -2.505905511811023612 ) ) ;
#29408 = CARTESIAN_POINT ( 'NONE',  ( 1.633858267716535639, -0.5400638737290844871, 0.3530559997133364547 ) ) ;
#29409 = CARTESIAN_POINT ( 'NONE',  ( 0.5314960629921264834, 0.1660481256975883668, -0.3530559997133364547 ) ) ;
#29410 = CARTESIAN_POINT ( 'NONE',  ( 0.5380577427821529035, -0.4281496062992124485, 0.4176697321401328655 ) ) ;
#29411 = CARTESIAN_POINT ( 'NONE',  ( -0.7611548556430438595, -0.5023911411419708095, -0.1820866141732282451 ) ) ;
#29412 = CARTESIAN_POINT ( 'NONE',  ( 0.05249343832021075018, 0.2306618581243847221, -0.2411417322834647770 ) ) ;
#29413 = CARTESIAN_POINT ( 'NONE',  ( 0.2362204724409451007, -0.4091458600556402980, -2.215879265091863726 ) ) ;
#29414 = CARTESIAN_POINT ( 'NONE',  ( -0.5183727034120726440, -0.6692913385826773087, -0.1292274648535924053 ) ) ;
#29415 = CARTESIAN_POINT ( 'NONE',  ( -0.2891555358219911054, 0.2891555358219909388, -1.671259842519685179 ) ) ;
#29416 = CARTESIAN_POINT ( 'NONE',  ( 1.089238845144357537, -0.3690944881889763329, 0.3153832671262228327 ) ) ;
#29417 = CARTESIAN_POINT ( 'NONE',  ( 0.01968503937007930540, 0.07958543189024085140, 0.2665933059059887866 ) ) ;
#29418 = CARTESIAN_POINT ( 'NONE',  ( 1.115485564304462551, -0.3690944881889765550, -0.3153832671262227771 ) ) ;
#29420 = EDGE_CURVE ( 'NONE', #46648, #32589, #74052, .T. ) ;
#29419 = CARTESIAN_POINT ( 'NONE',  ( -1.003937007874015297, -0.5400638737290845981, -0.3530559997133363437 ) ) ;
#29421 = CARTESIAN_POINT ( 'NONE',  ( -1.312335958005248715, 0.1283753931104748280, 0.1820866141732283561 ) ) ;
#29422 = CARTESIAN_POINT ( 'NONE',  ( -1.614173228346457378, 1.055049524192299693, 0.1372047244094476981 ) ) ;
#29423 = CARTESIAN_POINT ( 'NONE',  ( -1.246719160104986512, 0.05413385826771666132, 0.4176697321401328100 ) ) ;
#29424 = CARTESIAN_POINT ( 'NONE',  ( -0.6233595800524928121, -0.3162353388693409650, -0.4822834645669289433 ) ) ;
#29425 = CARTESIAN_POINT ( 'NONE',  ( 0.1706036745406830368, -0.4281496062992127816, -0.4176697321401328100 ) ) ;
#29426 = CARTESIAN_POINT ( 'NONE',  ( -0.3917322834645669549, -7.196005306013483243E-17, -2.324127665845457713 ) ) ;
#29427 = CARTESIAN_POINT ( 'NONE',  ( -1.851423525050897689, 1.064103292658516331, 0.03357545743410488698 ) ) ;
#29428 = CARTESIAN_POINT ( 'NONE',  ( 0.4593175853018380828, -0.004921259842519870586, -0.3153832671262229437 ) ) ;
#29429 = CARTESIAN_POINT ( 'NONE',  ( 0.9448818897637802916, -0.1870078740157479769, 0.4822834645669291653 ) ) ;
#29430 = CARTESIAN_POINT ( 'NONE',  ( -1.456692913385826182, -0.5511811023622047445, 6.969142054262312111E-17 ) ) ;
#29431 = CARTESIAN_POINT ( 'NONE',  ( 0.7808398950131241190, -0.05778040916215560624, -0.4822834645669293319 ) ) ;
#29432 = CARTESIAN_POINT ( 'NONE',  ( -1.574803149606298636, -0.1870078740157479769, 0.3641732283464567677 ) ) ;
#29433 = CARTESIAN_POINT ( 'NONE',  ( -1.410761154855642463, -0.05778040916215522460, 0.4822834645669289988 ) ) ;
#29434 = CARTESIAN_POINT ( 'NONE',  ( -0.7414698162729651543, 0.2952755905511810774, -0.1292274648535930714 ) ) ;
#29435 = CARTESIAN_POINT ( 'NONE',  ( -0.01968503937007793844, 0.07958543189024071263, -0.2665933059059888421 ) ) ;
#29436 = CARTESIAN_POINT ( 'NONE',  ( 1.606354222338493454, 0.2948481568435550315, 0.02349281142910526754 ) ) ;
#29437 = CARTESIAN_POINT ( 'NONE',  ( 0.8005249343832027131, -0.004921259842519576551, 0.3153832671262227771 ) ) ;
#29438 = CARTESIAN_POINT ( 'NONE',  ( -0.1115485564304453947, -0.6692913385826771977, 0.1292274648535927661 ) ) ;
#29439 = EDGE_CURVE ( 'NONE', #81026, #50981, #47744, .T. ) ;
#29440 = CARTESIAN_POINT ( 'NONE',  ( 0.3996062992125986035, -0.1070741851644052972, -0.3458005249343831244 ) ) ;
#29441 = CARTESIAN_POINT ( 'NONE',  ( -1.161417322834644716, -0.5400638737290845981, -0.3530559997133363437 ) ) ;
#29442 = CARTESIAN_POINT ( 'NONE',  ( -0.3917322834645670104, -7.196005306013484475E-17, -1.698818897637795367 ) ) ;
#29443 = CARTESIAN_POINT ( 'NONE',  ( 0.9842519685039375910, 0.1771653543307087630, 0.000000000000000000 ) ) ;
#29444 = CARTESIAN_POINT ( 'NONE',  ( 0.1574803149606306130, -0.1870078740157480879, -0.4822834645669291653 ) ) ;
#29445 = CARTESIAN_POINT ( 'NONE',  ( -0.3543307086614165824, 0.2952755905511811885, 0.000000000000000000 ) ) ;
#29446 = CARTESIAN_POINT ( 'NONE',  ( -0.5839895013123351797, -0.5511811023622046335, 0.09757992244046803654 ) ) ;
#29447 = DIRECTION ( 'NONE',  ( 1.000000000000000000, 2.238352872228138170E-16, 0.000000000000000000 ) ) ;
#29448 = CARTESIAN_POINT ( 'NONE',  ( -0.3937007874015740483, -0.1870078740157479769, 0.3641732283464567677 ) ) ;
#29449 = CARTESIAN_POINT ( 'NONE',  ( 0.3215223097112867578, -0.3162353388693409650, -0.4822834645669289433 ) ) ;
#29450 = AXIS2_PLACEMENT_3D ( 'NONE', #63033, #62203, #10867 ) ;
#29451 = CARTESIAN_POINT ( 'NONE',  ( -1.292650918635170010, -0.5511811023622046335, 0.09757992244046803654 ) ) ;
#29452 = CARTESIAN_POINT ( 'NONE',  ( 0.3996062992125986035, -0.1070741851644052972, -1.448162729658792669 ) ) ;
#29453 = CARTESIAN_POINT ( 'NONE',  ( -1.614173228346455824, 0.2952755905511811885, 0.000000000000000000 ) ) ;
#29454 = CARTESIAN_POINT ( 'NONE',  ( 0.3458507752293908943, 0.3458507752293908943, -2.576771653543307394 ) ) ;
#29455 = EDGE_LOOP ( 'NONE', ( #24297, #15531, #51625, #46973 ) ) ;
#29456 = CARTESIAN_POINT ( 'NONE',  ( -1.469816272965878357, -0.5023911411419708095, -0.1820866141732282451 ) ) ;
#29457 = CARTESIAN_POINT ( 'NONE',  ( -0.6496062992125976043, -0.5400638737290844871, 0.3530559997133364547 ) ) ;
#29458 = CARTESIAN_POINT ( 'NONE',  ( -1.161417322834644716, 0.1660481256975885056, 0.3530559997133364547 ) ) ;
#29459 = CARTESIAN_POINT ( 'NONE',  ( 0.3392501089628018329, 0.1958661417322835607, -1.475721784776902856 ) ) ;
#29460 = DIRECTION ( 'NONE',  ( 0.000000000000000000, 1.000000000000000000, -0.000000000000000000 ) ) ;
#29461 = CARTESIAN_POINT ( 'NONE',  ( 1.469816272965879911, -0.6046776061558807314, 0.2411417322834647770 ) ) ;
#29462 = CARTESIAN_POINT ( 'NONE',  ( 0.2624671916010504757, 0.2306618581243848609, 0.2411417322834645549 ) ) ;
#29463 = CARTESIAN_POINT ( 'NONE',  ( -0.2755905511811018171, 0.2066929133858268208, 0.000000000000000000 ) ) ;
#29464 = CARTESIAN_POINT ( 'NONE',  ( -0.3460692066303960313, 0.1998031496062989965, -2.307742782152231165 ) ) ;
#29465 = CARTESIAN_POINT ( 'NONE',  ( -1.535433070866141225, 0.2952755905511811885, 0.000000000000000000 ) ) ;
#29466 = CARTESIAN_POINT ( 'NONE',  ( 0.1070741851644054915, -0.3996062992125986035, -0.8727034120734907807 ) ) ;
#29467 = VERTEX_POINT ( 'NONE', #22504 ) ;
#29468 = CARTESIAN_POINT ( 'NONE',  ( -0.8202099737532799750, 0.1771653543307087075, -0.09757992244046823083 ) ) ;
#29469 = CARTESIAN_POINT ( 'NONE',  ( 0.3917322834645669549, 0.1049643490035304660, -2.321522309711285814 ) ) ;
#29470 = ORIENTED_EDGE ( 'NONE', *, *, #78723, .F. ) ;
#29471 = CARTESIAN_POINT ( 'NONE',  ( 0.9580052493438326877, 0.05413385826771666132, 0.4176697321401328100 ) ) ;
#29472 = CARTESIAN_POINT ( 'NONE',  ( -0.5314960629921254842, -0.5400638737290845981, -0.3530559997133363437 ) ) ;
#29473 = CARTESIAN_POINT ( 'NONE',  ( -1.312335958005248715, 0.2306618581243848609, 0.2411417322834645549 ) ) ;
#29474 = CARTESIAN_POINT ( 'NONE',  ( 1.148293963254593875, -0.6692913385826771977, 0.1292274648535927661 ) ) ;
#29475 = CARTESIAN_POINT ( 'NONE',  ( -1.246719160104985846, -0.3690944881889765550, -0.3153832671262227771 ) ) ;
#29476 = CARTESIAN_POINT ( 'NONE',  ( 0.1837270341207357105, -0.6046776061558809534, -0.2411417322834644161 ) ) ;
#29477 = CARTESIAN_POINT ( 'NONE',  ( -0.8595800524934373854, -0.05778040916215522460, 0.4822834645669289988 ) ) ;
#29478 = CARTESIAN_POINT ( 'NONE',  ( 4.797336870675655290E-17, -0.3917322834645669549, -1.418615854821835276 ) ) ;
#29479 = CARTESIAN_POINT ( 'NONE',  ( -1.410761154855641575, -0.3162353388693409650, -0.4822834645669289433 ) ) ;
#29480 = DIRECTION ( 'NONE',  ( 1.196716813021145407E-16, 0.7071067811865622277, 0.7071067811865328068 ) ) ;
#29481 = CARTESIAN_POINT ( 'NONE',  ( 0.8923884514435703741, 0.2306618581243848609, 0.2411417322834645549 ) ) ;
#29482 = CARTESIAN_POINT ( 'NONE',  ( 0.3392501089628018884, -0.1958661417322834220, 0.06036745406824151755 ) ) ;
#29483 = CARTESIAN_POINT ( 'NONE',  ( 1.240157480314961314, 0.07958543189024071263, -0.2665933059059888421 ) ) ;
#29484 = EDGE_LOOP ( 'NONE', ( #70803, #24315, #58137, #21710 ) ) ;
#29485 = CARTESIAN_POINT ( 'NONE',  ( -0.1058382717557497937, -0.3949938075777411628, 0.08530183727034117147 ) ) ;
#29486 = CARTESIAN_POINT ( 'NONE',  ( -0.5774278215223089816, -0.6046776061558807314, 0.2411417322834647770 ) ) ;
#29487 = VERTEX_POINT ( 'NONE', #27566 ) ;
#29488 = CARTESIAN_POINT ( 'NONE',  ( 0.4658792650918640033, -0.2845877964562159024, 0.3641732283464567677 ) ) ;
#29489 = CARTESIAN_POINT ( 'NONE',  ( -1.509186351706035767, 0.05413385826771626580, -0.4176697321401330321 ) ) ;
#29490 = CARTESIAN_POINT ( 'NONE',  ( 0.6692913385826777528, 0.2952755905511811885, 0.000000000000000000 ) ) ;
#29491 = CARTESIAN_POINT ( 'NONE',  ( 0.7939632545931766261, -0.05778040916215522460, 0.4822834645669289988 ) ) ;
#29492 = CARTESIAN_POINT ( 'NONE',  ( -0.09186351706036689768, 0.05413385826771626580, -0.4176697321401330321 ) ) ;
#29493 = CARTESIAN_POINT ( 'NONE',  ( -0.2867679344610367109, 0.2867679344610365444, -1.433746349902574213 ) ) ;
#29494 = CARTESIAN_POINT ( 'NONE',  ( -0.6824146981627288167, 0.2306618581243848609, 0.2411417322834645549 ) ) ;
#29495 = CARTESIAN_POINT ( 'NONE',  ( -0.1958661417322834220, -0.3392501089628018884, -2.354986876640420057 ) ) ;
#29496 = CARTESIAN_POINT ( 'NONE',  ( 1.594488188976378673, 0.07958543189024085140, 0.2665933059059887866 ) ) ;
#29497 = CARTESIAN_POINT ( 'NONE',  ( -0.9448818897637790704, -0.1870078740157480879, -0.4822834645669291653 ) ) ;
#29498 = CARTESIAN_POINT ( 'NONE',  ( 1.102362204724410155, -0.1870078740157480879, -0.4822834645669291653 ) ) ;
#29499 = CARTESIAN_POINT ( 'NONE',  ( 1.194225721784777594, 0.05413385826771666132, 0.4176697321401328100 ) ) ;
#29500 = CARTESIAN_POINT ( 'NONE',  ( 0.1998031496062992740, 0.3460692066303959757, -0.3018372703412073865 ) ) ;
#29501 = CARTESIAN_POINT ( 'NONE',  ( -1.102362204724408601, -0.1870078740157479769, 0.4822834645669291653 ) ) ;
#29502 = CARTESIAN_POINT ( 'NONE',  ( -0.3996062992125985480, -7.340648628747423112E-17, 0.1988188976377952832 ) ) ;
#29503 = CARTESIAN_POINT ( 'NONE',  ( 0.4330708661417329575, -0.6692913385826771977, 8.415575281601705876E-17 ) ) ;
#29504 = CARTESIAN_POINT ( 'NONE',  ( -0.3460692066303958092, -0.1998031496062994683, -2.099737532808398921 ) ) ;
#29505 = CARTESIAN_POINT ( 'NONE',  ( -0.3608923884514428360, 0.2952755905511811885, 0.1292274648535926551 ) ) ;
#29506 = CARTESIAN_POINT ( 'NONE',  ( -1.496062992125983815, -0.1870078740157479769, 0.3641732283464567677 ) ) ;
#29507 = CARTESIAN_POINT ( 'NONE',  ( 0.6496062992125991586, -0.4536011799217368745, -0.2665933059059886201 ) ) ;
#29508 = CARTESIAN_POINT ( 'NONE',  ( 1.397637795275591177, -0.5400638737290844871, 0.3530559997133364547 ) ) ;
#29509 = CARTESIAN_POINT ( 'NONE',  ( -0.4091458600556402980, -0.2362204724409451284, -0.9166666666666666297 ) ) ;
#29510 = CARTESIAN_POINT ( 'NONE',  ( 0.5839895013123367340, 0.1771653543307087630, 0.09757992244046791164 ) ) ;
#29511 = CARTESIAN_POINT ( 'NONE',  ( 0.9711286089238851948, 0.2306618581243848609, 0.2411417322834645549 ) ) ;
#29512 = CARTESIAN_POINT ( 'NONE',  ( -9.674558042662122972E-17, 0.3949938075777409963, -0.3917322834645669549 ) ) ;
#29513 = CARTESIAN_POINT ( 'NONE',  ( -0.1837270341207343505, -0.6046776061558807314, 0.2411417322834647770 ) ) ;
#29514 = CARTESIAN_POINT ( 'NONE',  ( 0.5314960629921373636, 2.755905511811024056, -3.264097702071371288 ) ) ;
#29515 = CARTESIAN_POINT ( 'NONE',  ( 1.286089238845145033, 0.1283753931104748280, 0.1820866141732283561 ) ) ;
#29516 = CARTESIAN_POINT ( 'NONE',  ( -0.7677165354330699465, 0.1660481256975885056, 0.3530559997133364547 ) ) ;
#29517 = CARTESIAN_POINT ( 'NONE',  ( 0.07217847769028949700, -0.05778040916215560624, -0.4822834645669293319 ) ) ;
#29518 = CARTESIAN_POINT ( 'NONE',  ( 0.000000000000000000, 0.000000000000000000, 0.000000000000000000 ) ) ;
#29519 = CARTESIAN_POINT ( 'NONE',  ( -0.05905511811023545637, -0.5400638737290845981, -0.3530559997133363437 ) ) ;
#29520 = CARTESIAN_POINT ( 'NONE',  ( 0.7414698162729663755, 0.1771653543307087630, 0.09757992244046791164 ) ) ;
#29521 = CARTESIAN_POINT ( 'NONE',  ( -0.4724409448818898682, -8.678599364036362592E-17, -0.1161417322834645827 ) ) ;
#29522 = CARTESIAN_POINT ( 'NONE',  ( -0.1443569553805765515, -0.3690944881889765550, -0.3153832671262227771 ) ) ;
#29523 = CARTESIAN_POINT ( 'NONE',  ( 0.6692913385826777528, 0.1771653543307087630, 0.000000000000000000 ) ) ;
#29524 = DIRECTION ( 'NONE',  ( 0.000000000000000000, 0.000000000000000000, -1.000000000000000000 ) ) ;
#29525 = CARTESIAN_POINT ( 'NONE',  ( -0.3996062992125984925, -0.1070741851644056858, -1.540026246719160108 ) ) ;
#29526 = CARTESIAN_POINT ( 'NONE',  ( 0.1443569553805781891, 0.05413385826771626580, -0.4176697321401330321 ) ) ;
#29527 = CARTESIAN_POINT ( 'NONE',  ( 0.1958661417322834775, 0.3392501089628018884, -0.9238845144356954142 ) ) ;
#29528 = CARTESIAN_POINT ( 'NONE',  ( 1.515748031496063408, 0.07958543189024085140, 0.2665933059059887866 ) ) ;
#29529 = CARTESIAN_POINT ( 'NONE',  ( -0.3330030935778838797, 0.2065800153021834507, 1.128668216881735203E-17 ) ) ;
#29530 = CARTESIAN_POINT ( 'NONE',  ( 0.1246719160104994284, -0.5511811023622046335, 0.09757992244046803654 ) ) ;
#29531 = CARTESIAN_POINT ( 'NONE',  ( 0.1574803149606306130, -0.1870078740157480879, -0.4822834645669291653 ) ) ;
#29532 = CARTESIAN_POINT ( 'NONE',  ( 1.391076115485564868, 0.1283753931104746893, -0.1820866141732285504 ) ) ;
#29533 = CARTESIAN_POINT ( 'NONE',  ( -1.266404199475064773, -0.2845877964562159024, 0.3641732283464567677 ) ) ;
#29534 = CARTESIAN_POINT ( 'NONE',  ( -1.463254593175852492, -0.6692913385826773087, -0.1292274648535924053 ) ) ;
#29535 = CARTESIAN_POINT ( 'NONE',  ( 0.1837270341207357105, -0.6046776061558809534, -0.2411417322834644161 ) ) ;
#29536 = CARTESIAN_POINT ( 'NONE',  ( 1.122047244094488860, -0.5400638737290845981, -0.3530559997133363437 ) ) ;
#29537 = DIRECTION ( 'NONE',  ( 1.000000000000000000, 8.462065736472229849E-17, -0.000000000000000000 ) ) ;
#29538 = CARTESIAN_POINT ( 'NONE',  ( 0.1902887139107617975, 0.2952755905511811885, 0.1292274648535926551 ) ) ;
#29539 = CARTESIAN_POINT ( 'NONE',  ( 1.148293963254593875, -0.6692913385826771977, 0.1292274648535927661 ) ) ;
#29540 = CARTESIAN_POINT ( 'NONE',  ( 0.8792650918635177559, 0.05413385826771666132, 0.4176697321401328100 ) ) ;
#29541 = EDGE_CURVE ( 'NONE', #24707, #30109, #33057, .T. ) ;
#29542 = DIRECTION ( 'NONE',  ( -3.491481338843132961E-15, -0.000000000000000000, 1.000000000000000000 ) ) ;
#29543 = CARTESIAN_POINT ( 'NONE',  ( 0.7349081364829403995, 0.1283753931104748280, 0.1820866141732283561 ) ) ;
#29544 = CARTESIAN_POINT ( 'NONE',  ( -1.627296587926508442, 0.1283753931104748280, 0.1820866141732283561 ) ) ;
#29545 = CARTESIAN_POINT ( 'NONE',  ( 0.1771653543307093182, 0.07958543189024085140, 0.2665933059059887866 ) ) ;
#29546 = CARTESIAN_POINT ( 'NONE',  ( 0.1049868766404206816, 0.2306618581243848609, 0.2411417322834645549 ) ) ;
#29547 = CARTESIAN_POINT ( 'NONE',  ( 0.5643044619422579178, -0.4281496062992127816, -0.4176697321401328100 ) ) ;
#29548 = CARTESIAN_POINT ( 'NONE',  ( -0.5314960629921250401, 0.1660481256975885056, 0.3530559997133364547 ) ) ;
#29549 = CARTESIAN_POINT ( 'NONE',  ( -9.594673741351313045E-17, 0.3917322834645670659, -2.201462885335645048 ) ) ;
#29550 = CARTESIAN_POINT ( 'NONE',  ( -0.09842519685039295696, 0.07958543189024071263, -0.2665933059059888421 ) ) ;
#29551 = CARTESIAN_POINT ( 'NONE',  ( 0.9186351706036751663, -0.6046776061558807314, 0.2411417322834647770 ) ) ;
#29552 = CARTESIAN_POINT ( 'NONE',  ( 1.062992125984252745, 0.1771653543307087630, 0.000000000000000000 ) ) ;
#29553 = LINE ( 'NONE', #22005, #46013 ) ;
#29555 = CARTESIAN_POINT ( 'NONE',  ( -0.7874015748031492068, 2.204724409448818978, 0.000000000000000000 ) ) ;
#29554 = CARTESIAN_POINT ( 'NONE',  ( -0.5314960629921171575, 2.716535433070866645, -2.543486866223390930 ) ) ;
#29556 = DIRECTION ( 'NONE',  ( 1.000000000000000000, 0.000000000000000000, 0.000000000000000000 ) ) ;
#29557 = CARTESIAN_POINT ( 'NONE',  ( -1.364829396325458521, -0.6046776061558807314, 0.2411417322834647770 ) ) ;
#29558 = CARTESIAN_POINT ( 'NONE',  ( -0.5052493438320203589, -0.6692913385826771977, 0.1292274648535927661 ) ) ;
#29559 = EDGE_CURVE ( 'NONE', #8463, #24368, #76671, .T. ) ;
#29560 = CARTESIAN_POINT ( 'NONE',  ( 0.4091458600556403535, 0.2362204724409449896, 0.02624671916010498651 ) ) ;
#29561 = CARTESIAN_POINT ( 'NONE',  ( 0.2891555358219910499, 0.2891555358219910499, -2.185039370078740273 ) ) ;
#29562 = ORIENTED_EDGE ( 'NONE', *, *, #10855, .T. ) ;
#29563 = CARTESIAN_POINT ( 'NONE',  ( 0.3608923884514443348, -0.5511811023622046335, 0.09757992244046803654 ) ) ;
#29564 = CARTESIAN_POINT ( 'NONE',  ( -0.3917322834645671215, 0.1049643490035301469, -0.8123359580052491591 ) ) ;
#29565 = CARTESIAN_POINT ( 'NONE',  ( 1.194225721784777594, -0.4281496062992127816, -0.4176697321401328100 ) ) ;
#29566 = CARTESIAN_POINT ( 'NONE',  ( 0.1265901696524990294, -0.4724409448818896462, -2.447506561679789527 ) ) ;
#29567 = CARTESIAN_POINT ( 'NONE',  ( 0.3458507752293908943, 0.3458507752293908943, -0.8444881889763780070 ) ) ;
#29568 = ADVANCED_FACE ( 'NONE', ( #1494 ), #28396, .F. ) ;
#29569 = CARTESIAN_POINT ( 'NONE',  ( -1.725721784776902190, -0.08942795157527998196, 0.3641732283464567121 ) ) ;
#29570 = FACE_OUTER_BOUND ( 'NONE', #7551, .T. ) ;
#29571 = CARTESIAN_POINT ( 'NONE',  ( 1.371391076115485719, -0.5511811023622048555, -0.09757992244046775898 ) ) ;
#29572 = CARTESIAN_POINT ( 'NONE',  ( 0.2296587926509192634, -0.3162353388693405765, 0.4822834645669290543 ) ) ;
#29573 = CARTESIAN_POINT ( 'NONE',  ( 0.3917322834645668994, -0.1049643490035303134, -0.3490620490475572768 ) ) ;
#29574 = CARTESIAN_POINT ( 'NONE',  ( 0.09842519685039434474, 0.1660481256975885056, 0.3530559997133364547 ) ) ;
#29575 = CARTESIAN_POINT ( 'NONE',  ( -0.9711286089238838626, -0.5023911411419708095, 0.1820866141732285504 ) ) ;
#29576 = CARTESIAN_POINT ( 'NONE',  ( 0.5971128608923890191, -0.6692913385826771977, 0.1292274648535927661 ) ) ;
#29577 = CARTESIAN_POINT ( 'NONE',  ( -0.07217847769028813698, -0.3162353388693409650, -0.4822834645669289433 ) ) ;
#29578 = CARTESIAN_POINT ( 'NONE',  ( 0.4744094488188841940, 1.569669905603892524, 3.908320185825794990 ) ) ;
#29579 = CARTESIAN_POINT ( 'NONE',  ( -0.3996062992125986035, -7.340648628747425578E-17, -2.874015748031495843 ) ) ;
#29580 = CARTESIAN_POINT ( 'NONE',  ( -0.3917322834645671770, 0.1049643490035302024, -1.446869709482626831 ) ) ;
#29581 = CARTESIAN_POINT ( 'NONE',  ( 0.9776902887139113929, -0.6692913385826773087, -0.1292274648535924053 ) ) ;
#29582 = CARTESIAN_POINT ( 'NONE',  ( -0.2034120734908131112, -0.6692913385826773087, -0.1292274648535924053 ) ) ;
#29583 = CARTESIAN_POINT ( 'NONE',  ( -0.9908136482939626788, 0.2952755905511811885, 0.1292274648535926551 ) ) ;
#29584 = CARTESIAN_POINT ( 'NONE',  ( 1.030183727034121421, -0.3162353388693409650, -0.4822834645669289433 ) ) ;
#29585 = CARTESIAN_POINT ( 'NONE',  ( 0.5380577427821529035, -0.4281496062992124485, 0.4176697321401328655 ) ) ;
#29586 = CARTESIAN_POINT ( 'NONE',  ( 0.1049643490035304938, -0.3917322834645669549, -1.114829396325459410 ) ) ;
#29587 = CARTESIAN_POINT ( 'NONE',  ( -0.4658792650918627265, -0.05778040916215522460, 0.4822834645669289988 ) ) ;
#29588 = CARTESIAN_POINT ( 'NONE',  ( 0.2559055118110243332, 0.1660481256975885056, 0.3530559997133364547 ) ) ;
#29589 = CARTESIAN_POINT ( 'NONE',  ( -0.4921259842519677963, 0.1660481256975883668, -0.3530559997133364547 ) ) ;
#29590 = CARTESIAN_POINT ( 'NONE',  ( 0.1706036745406830368, -0.3690944881889765550, -0.3153832671262227771 ) ) ;
#29591 = CARTESIAN_POINT ( 'NONE',  ( 1.673228346456693494, 0.07958543189024085140, 0.2665933059059887866 ) ) ;
#29592 = CARTESIAN_POINT ( 'NONE',  ( -0.3336463653987898903, 1.199832043049264163, -2.750549046294851419 ) ) ;
#29593 = CARTESIAN_POINT ( 'NONE',  ( 0.5118110236220478892, 0.2952755905511811885, 0.000000000000000000 ) ) ;
#29594 = DIRECTION ( 'NONE',  ( -0.000000000000000000, -1.000000000000000000, -0.000000000000000000 ) ) ;
#29595 = EDGE_CURVE ( 'NONE', #57099, #39221, #47330, .T. ) ;
#29596 = CARTESIAN_POINT ( 'NONE',  ( 1.364829396325459854, -0.6046776061558809534, -0.2411417322834644161 ) ) ;
#29597 = CARTESIAN_POINT ( 'NONE',  ( -0.3917322834645669549, -0.1049643490035306603, -2.557742782152230721 ) ) ;
#29598 = ORIENTED_EDGE ( 'NONE', *, *, #4428, .T. ) ;
#29599 = VERTEX_POINT ( 'NONE', #54054 ) ;
#29600 = CARTESIAN_POINT ( 'NONE',  ( 0.7217847769028878924, 0.05413385826771666132, 0.4176697321401328100 ) ) ;
#29601 = CARTESIAN_POINT ( 'NONE',  ( 0.4199475065616803948, -0.5023911411419708095, -0.1820866141732282451 ) ) ;
#29603 = CARTESIAN_POINT ( 'NONE',  ( 1.141392835773559211, 0.000000000000000000, 1.141392835773562764 ) ) ;
#29602 = DIRECTION ( 'NONE',  ( -1.000000000000000000, 1.445602896647338917E-16, -0.000000000000000000 ) ) ;
#29604 = CARTESIAN_POINT ( 'NONE',  ( 0.3392501089628018884, -0.1958661417322834220, -0.9770341207349081403 ) ) ;
#29605 = DIRECTION ( 'NONE',  ( 1.000000000000000000, 3.096699300667737957E-16, 0.000000000000000000 ) ) ;
#29606 = DIRECTION ( 'NONE',  ( 0.000000000000000000, 0.000000000000000000, -1.000000000000000000 ) ) ;
#29607 = EDGE_CURVE ( 'NONE', #10673, #21899, #37105, .T. ) ;
#29608 = CARTESIAN_POINT ( 'NONE',  ( -0.1998031496062991630, -0.3460692066303959202, -2.504593175853018661 ) ) ;
#29609 = CARTESIAN_POINT ( 'NONE',  ( 0.7939632545931766261, -0.05778040916215522460, 0.4822834645669289988 ) ) ;
#29610 = CARTESIAN_POINT ( 'NONE',  ( -0.7611548556430438595, -0.6046776061558809534, -0.2411417322834644161 ) ) ;
#29611 = CARTESIAN_POINT ( 'NONE',  ( -0.7283464566929126471, 0.1660481256975883668, -0.3530559997133364547 ) ) ;
#29612 = CARTESIAN_POINT ( 'NONE',  ( 0.5643044619422579178, -0.4281496062992127816, -0.4176697321401328100 ) ) ;
#29613 = CARTESIAN_POINT ( 'NONE',  ( 1.509186351706037543, -0.4281496062992127816, -0.4176697321401328100 ) ) ;
#29614 = DIRECTION ( 'NONE',  ( 0.000000000000000000, 0.000000000000000000, -1.000000000000000000 ) ) ;
#29615 = SHAPE_DEFINITION_REPRESENTATION ( #60807, #76132 ) ;
#29616 = CARTESIAN_POINT ( 'NONE',  ( 1.233595800524935227, 0.1283753931104746893, -0.1820866141732285504 ) ) ;
#29617 = CARTESIAN_POINT ( 'NONE',  ( 2.787279214012418738, 1.496062992125984481, 0.000000000000000000 ) ) ;
#29618 = CARTESIAN_POINT ( 'NONE',  ( -1.417322834645668772, -0.1870078740157480601, -0.3641732283464567677 ) ) ;
#29619 = ADVANCED_FACE ( 'NONE', ( #41031 ), #41444, .F. ) ;
#29620 = CARTESIAN_POINT ( 'NONE',  ( 1.827151662668104581, 2.742788190551038952, 0.5314960629921260393 ) ) ;
#29621 = CARTESIAN_POINT ( 'NONE',  ( 0.2427821522309719648, -0.05778040916215522460, 0.4822834645669289988 ) ) ;
#29623 = CARTESIAN_POINT ( 'NONE',  ( 0.4849061582275024929, 1.805669738366188382, -0.4921425059946357150 ) ) ;
#29622 = CARTESIAN_POINT ( 'NONE',  ( 1.122047244094488860, -0.5400638737290845981, -0.3530559997133363437 ) ) ;
#29624 = CARTESIAN_POINT ( 'NONE',  ( -1.233595800524933894, 0.1283753931104748280, 0.1820866141732283561 ) ) ;
#29625 = CARTESIAN_POINT ( 'NONE',  ( 0.5314960629921267055, -0.5400638737290844871, 0.3530559997133364547 ) ) ;
#29626 = CARTESIAN_POINT ( 'NONE',  ( 1.404199475065617264, -0.3690944881889763329, 0.3153832671262228327 ) ) ;
#29627 = CARTESIAN_POINT ( 'NONE',  ( -0.3392501089628019439, 0.1958661417322832554, -1.523602731462254889 ) ) ;
#29628 = CARTESIAN_POINT ( 'NONE',  ( -1.364829396325458521, 0.1283753931104746893, -0.1820866141732285504 ) ) ;
#29629 = CARTESIAN_POINT ( 'NONE',  ( 1.456692913385827515, -0.6692913385826771977, 8.415575281601705876E-17 ) ) ;
#29630 = CARTESIAN_POINT ( 'NONE',  ( 0.1083363854164813983, 1.946602136093918745, 0.2940643763633090102 ) ) ;
#29631 = CARTESIAN_POINT ( 'NONE',  ( -0.2887139107611542133, 0.1283753931104748280, 0.1820866141732283561 ) ) ;
#29632 = CARTESIAN_POINT ( 'NONE',  ( -0.3871391076115479057, -0.3162353388693409650, -0.4822834645669289433 ) ) ;
#29633 = CARTESIAN_POINT ( 'NONE',  ( -1.240157480314959759, -0.4536011799217368745, -0.2665933059059886201 ) ) ;
#29634 = CARTESIAN_POINT ( 'NONE',  ( -0.7874015748031489847, -0.1870078740157479769, 0.4822834645669291653 ) ) ;
#29635 = VECTOR ( 'NONE', #8634, 39.37007874015748143 ) ;
#29636 = CARTESIAN_POINT ( 'NONE',  ( 1.174540682414699111, -0.3162353388693405765, 0.4822834645669290543 ) ) ;
#29637 = CARTESIAN_POINT ( 'NONE',  ( -9.594673741351313045E-17, 0.3917322834645670659, -0.6266597357293457460 ) ) ;
#29638 = CARTESIAN_POINT ( 'NONE',  ( -0.4703312907311723579, 1.601535527459639896, -1.018715732779044592 ) ) ;
#29639 = CARTESIAN_POINT ( 'NONE',  ( 1.522309711286089939, -0.6046776061558809534, -0.2411417322834644161 ) ) ;
#29640 = CARTESIAN_POINT ( 'NONE',  ( -0.4724409448818898682, -8.678599364036362592E-17, -2.163385826771653697 ) ) ;
#29641 = CARTESIAN_POINT ( 'NONE',  ( -1.410761154855642463, -0.05778040916215522460, 0.4822834645669289988 ) ) ;
#29642 = CARTESIAN_POINT ( 'NONE',  ( -0.9580052493438311334, -0.004921259842519870586, -0.3153832671262229437 ) ) ;
#29643 = CARTESIAN_POINT ( 'NONE',  ( -0.7939632545931754048, -0.2845877964562159024, 0.3641732283464567677 ) ) ;
#29644 = CARTESIAN_POINT ( 'NONE',  ( 1.586052503253845281, 1.023622047244095556, -0.1653254495020587966 ) ) ;
#29645 = CARTESIAN_POINT ( 'NONE',  ( 0.1181102362204730916, 0.2952755905511811885, 0.000000000000000000 ) ) ;
#29646 = CARTESIAN_POINT ( 'NONE',  ( -0.1837270341207340729, 0.1283753931104746893, -0.1820866141732285504 ) ) ;
#29647 = CARTESIAN_POINT ( 'NONE',  ( -1.030183727034119867, -0.08942795157528024563, -0.3641732283464568787 ) ) ;
#29648 = CARTESIAN_POINT ( 'NONE',  ( -1.555118110236219930, 0.1660481256975885056, 0.3530559997133364547 ) ) ;
#29649 = CARTESIAN_POINT ( 'NONE',  ( 1.187664041994751285, -0.2845877964562161244, -0.3641732283464567121 ) ) ;
#29650 = CARTESIAN_POINT ( 'NONE',  ( 1.397637795275591177, 0.1660481256975883668, -0.3530559997133364547 ) ) ;
#29651 = CARTESIAN_POINT ( 'NONE',  ( -0.2362204724409451284, 0.4091458600556402425, -2.137139107611548905 ) ) ;
#29652 = CARTESIAN_POINT ( 'NONE',  ( 0.3477690288713918276, -0.5511811023622048555, -0.09757992244046775898 ) ) ;
#29653 = CARTESIAN_POINT ( 'NONE',  ( 0.8792650918635177559, 0.05413385826771666132, 0.4176697321401328100 ) ) ;
#29654 = CARTESIAN_POINT ( 'NONE',  ( 0.2362204724409449064, 0.1279527559055118335, 0.000000000000000000 ) ) ;
#29655 = CARTESIAN_POINT ( 'NONE',  ( 1.062992125984252745, -0.5511811023622047445, 6.969142054262312111E-17 ) ) ;
#29656 = ORIENTED_EDGE ( 'NONE', *, *, #53659, .F. ) ;
#29657 = CARTESIAN_POINT ( 'NONE',  ( -1.200787401574802349, -0.5400638737290844871, 0.3530559997133364547 ) ) ;
#29658 = CARTESIAN_POINT ( 'NONE',  ( -0.9973753280839886548, 0.2306618581243848609, 0.2411417322834645549 ) ) ;
#29659 = CARTESIAN_POINT ( 'NONE',  ( 0.02624671916010564918, 0.2306618581243848609, 0.2411417322834645549 ) ) ;
#29660 = CARTESIAN_POINT ( 'NONE',  ( -0.3996062992125986590, 0.1070741851644051862, -0.03280839895013124702 ) ) ;
#29661 = CARTESIAN_POINT ( 'NONE',  ( -0.1998031496062994405, 0.3460692066303957537, -2.137139107611548905 ) ) ;
#29662 = CARTESIAN_POINT ( 'NONE',  ( 0.8858267716535438430, -0.5400638737290845981, -0.3530559997133363437 ) ) ;
#29663 = CARTESIAN_POINT ( 'NONE',  ( 1.489501312335958172, -0.08942795157528024563, -0.3641732283464568787 ) ) ;
#29664 = CARTESIAN_POINT ( 'NONE',  ( 0.1706036745406830368, -0.4281496062992127816, -0.4176697321401328100 ) ) ;
#29665 = CARTESIAN_POINT ( 'NONE',  ( 0.6955380577427828781, 0.05413385826771626580, -0.4176697321401330321 ) ) ;
#29666 = EDGE_CURVE ( 'NONE', #22431, #6368, #59145, .T. ) ;
#29667 = CARTESIAN_POINT ( 'NONE',  ( 0.1070741851644054915, -0.3996062992125986035, -1.817585301837270517 ) ) ;
#29668 = CARTESIAN_POINT ( 'NONE',  ( 0.3949938075777409408, 0.1058382717557500574, -1.069553805774278388 ) ) ;
#29669 = CARTESIAN_POINT ( 'NONE',  ( 0.3996062992125986035, 2.446882876249141962E-17, -2.480314960629921295 ) ) ;
#29670 = CARTESIAN_POINT ( 'NONE',  ( 0.1049643490035304799, -0.3917322834645669549, -0.2349081364829395946 ) ) ;
#29671 = CARTESIAN_POINT ( 'NONE',  ( 0.09186351706036799403, -0.3690944881889765550, -0.3153832671262227771 ) ) ;
#29672 = CARTESIAN_POINT ( 'NONE',  ( -0.7086614173228339419, -0.1870078740157480879, -0.4822834645669291653 ) ) ;
#29673 = CARTESIAN_POINT ( 'NONE',  ( 0.9645669291338588858, 0.1660481256975885056, 0.3530559997133364547 ) ) ;
#29674 = CARTESIAN_POINT ( 'NONE',  ( 0.3420746716998660508, -0.1974969037888704149, -2.071522309711286258 ) ) ;
#29675 = CARTESIAN_POINT ( 'NONE',  ( -0.4921259842519677963, 0.07958543189024071263, -0.2665933059059888421 ) ) ;
#29676 = CARTESIAN_POINT ( 'NONE',  ( -1.535433070866141225, -0.6692913385826771977, 8.415575281601705876E-17 ) ) ;
#29677 = CARTESIAN_POINT ( 'NONE',  ( 1.174540682414699111, -0.05778040916215560624, -0.4822834645669293319 ) ) ;
#29678 = CARTESIAN_POINT ( 'NONE',  ( 0.4724409448818898682, 2.892866454678787531E-17, -2.322834645669291209 ) ) ;
#29679 = CARTESIAN_POINT ( 'NONE',  ( -0.3996062992125987146, 0.1070741851644051862, -1.607611548556430403 ) ) ;
#29680 = CARTESIAN_POINT ( 'NONE',  ( 1.112371124080195450, -4.927456884911482678E-16, 0.4445507791589062840 ) ) ;
#29681 = B_SPLINE_CURVE_WITH_KNOTS ( 'NONE', 3,
 ( #48387, #35773, #43709, #68994 ),
 .UNSPECIFIED., .F., .F.,
 ( 4, 4 ),
 ( 0.2189251788971746659, 0.2203393341987958387 ),
 .UNSPECIFIED. ) ;
#29682 = CARTESIAN_POINT ( 'NONE',  ( 0.9383202099737536495, -0.3162353388693405765, 0.4822834645669290543 ) ) ;
#29683 = CARTESIAN_POINT ( 'NONE',  ( 1.397637795275591177, -0.4536011799217367080, 0.2665933059059888421 ) ) ;
#29685 = CARTESIAN_POINT ( 'NONE',  ( -1.522309711286088607, -0.6046776061558807314, 0.2411417322834647770 ) ) ;
#29684 = CARTESIAN_POINT ( 'NONE',  ( 1.633858267716535639, -0.5400638737290844871, 0.3530559997133364547 ) ) ;
#29686 = CARTESIAN_POINT ( 'NONE',  ( -0.3917322834645670659, 0.1049643490035301607, -2.790006930937320995 ) ) ;
#29687 = DIRECTION ( 'NONE',  ( 0.000000000000000000, 0.000000000000000000, 1.000000000000000000 ) ) ;
#29688 = CARTESIAN_POINT ( 'NONE',  ( 0.8398950131233602345, -0.6046776061558807314, 0.2411417322834647770 ) ) ;
#29689 = CARTESIAN_POINT ( 'NONE',  ( -1.594488188976377563, -0.5400638737290844871, 0.3530559997133364547 ) ) ;
#29690 = CARTESIAN_POINT ( 'NONE',  ( -0.6496062992125976043, -0.5400638737290844871, 0.3530559997133364547 ) ) ;
#29691 = CARTESIAN_POINT ( 'NONE',  ( -0.3871391076115479057, -0.3162353388693409650, -0.4822834645669289433 ) ) ;
#29692 = AXIS2_PLACEMENT_3D ( 'NONE', #48538, #74238, #24523 ) ;
#29693 = CARTESIAN_POINT ( 'NONE',  ( -1.522309711286088607, -0.6046776061558807314, 0.2411417322834647770 ) ) ;
#29694 = CARTESIAN_POINT ( 'NONE',  ( -0.3917322834645670104, -7.196005306013484475E-17, -0.2814960629921260393 ) ) ;
#29695 = CARTESIAN_POINT ( 'NONE',  ( 0.2165354330708668673, 0.1660481256975883668, -0.3530559997133364547 ) ) ;
#29696 = CARTESIAN_POINT ( 'NONE',  ( 0.3917322834645670104, -0.1049643490035303411, -2.150918635170603554 ) ) ;
#29697 = CARTESIAN_POINT ( 'NONE',  ( -1.627296587926508442, 0.1283753931104748280, 0.1820866141732283561 ) ) ;
#29698 = ORIENTED_EDGE ( 'NONE', *, *, #34592, .F. ) ;
#29699 = CARTESIAN_POINT ( 'NONE',  ( 0.3420746716998660508, -0.1974969037888703871, -2.624671916010498318 ) ) ;
#29700 = EDGE_LOOP ( 'NONE', ( #62264, #12881, #10255, #80015 ) ) ;
#29701 = CARTESIAN_POINT ( 'NONE',  ( -0.7426113562972006532, 2.209901789876323797, -0.5309055118110235227 ) ) ;
#29702 = CARTESIAN_POINT ( 'NONE',  ( -1.364829396325458521, 0.2306618581243847221, -0.2411417322834647770 ) ) ;
#29703 = CARTESIAN_POINT ( 'NONE',  ( 0.1998031496062992740, 0.3460692066303959757, -1.089238845144356871 ) ) ;
#29704 = CARTESIAN_POINT ( 'NONE',  ( 1.594488188976378673, -0.4536011799217368745, -0.2665933059059886201 ) ) ;
#29705 = CARTESIAN_POINT ( 'NONE',  ( -0.1181102362204717315, 0.2066929133858268208, 0.000000000000000000 ) ) ;
#29706 = CARTESIAN_POINT ( 'NONE',  ( 0.5314960629921396951, 2.559055118110236560, -3.937007874015760578 ) ) ;
#29707 = CARTESIAN_POINT ( 'NONE',  ( -0.3674540682414689785, 0.2306618581243848609, 0.2411417322834645549 ) ) ;
#29708 = CARTESIAN_POINT ( 'NONE',  ( 0.3392501089628018329, 0.1958661417322835607, -0.5308398950131234528 ) ) ;
#29709 = CARTESIAN_POINT ( 'NONE',  ( -0.2296587926509179312, -0.08942795157527998196, 0.3641732283464567121 ) ) ;
#29710 = CARTESIAN_POINT ( 'NONE',  ( -1.253280839895012377, -0.08942795157527998196, 0.3641732283464567121 ) ) ;
#29711 = CARTESIAN_POINT ( 'NONE',  ( -1.607611548556429737, 0.2952755905511810774, -0.1292274648535930714 ) ) ;
#29712 = CARTESIAN_POINT ( 'NONE',  ( 0.5183727034120741983, 0.2952755905511810774, -0.1292274648535930714 ) ) ;
#29713 = CARTESIAN_POINT ( 'NONE',  ( -1.377952755905511140, -0.6692913385826771977, 8.415575281601705876E-17 ) ) ;
#29714 = AXIS2_PLACEMENT_3D ( 'NONE', #36188, #17271, #28637 ) ;
#29715 = CARTESIAN_POINT ( 'NONE',  ( 0.1958661417322836440, -0.3392501089628017219, -0.08398950131233591521 ) ) ;
#29716 = ORIENTED_EDGE ( 'NONE', *, *, #69619, .T. ) ;
#29717 = CARTESIAN_POINT ( 'NONE',  ( 1.430446194225722500, 0.05413385826771666132, 0.4176697321401328100 ) ) ;
#29718 = DIRECTION ( 'NONE',  ( -1.000000000000000000, -3.083952846180990774E-16, 0.000000000000000000 ) ) ;
#29719 = CARTESIAN_POINT ( 'NONE',  ( 0.4091458600556403535, 0.2362204724409449896, -1.548556430446194287 ) ) ;
#29720 = FACE_OUTER_BOUND ( 'NONE', #42022, .T. ) ;
#29721 = CARTESIAN_POINT ( 'NONE',  ( -0.3917322834645669549, -0.1049643490035306603, -2.650262467191601079 ) ) ;
#29722 = CARTESIAN_POINT ( 'NONE',  ( -0.8989501312335946848, -0.6692913385826771977, 0.1292274648535927661 ) ) ;
#29723 = CARTESIAN_POINT ( 'NONE',  ( 1.299212598425197429, -0.6692913385826771977, 8.415575281601705876E-17 ) ) ;
#29725 = CARTESIAN_POINT ( 'NONE',  ( 0.4724409448818898127, -0.1265901696524988629, -2.001312335958005395 ) ) ;
#29724 = CARTESIAN_POINT ( 'NONE',  ( 0.2362204724409451007, -0.4091458600556402980, -2.296587926509186417 ) ) ;
#29726 = CARTESIAN_POINT ( 'NONE',  ( -1.653543307086613234, -0.1870078740157480879, -0.4822834645669291653 ) ) ;
#29727 = CARTESIAN_POINT ( 'NONE',  ( -0.8070866141732276899, -0.5400638737290844871, 0.3530559997133364547 ) ) ;
#29728 = CARTESIAN_POINT ( 'NONE',  ( -0.3392501089628019439, 0.1958661417322832554, -0.5787208416984759296 ) ) ;
#29729 = CARTESIAN_POINT ( 'NONE',  ( 0.2230971128608929543, -0.004921259842519870586, -0.3153832671262229437 ) ) ;
#29730 = CARTESIAN_POINT ( 'NONE',  ( -9.594673741351313045E-17, 0.3917322834645670104, -0.2421259842519686289 ) ) ;
#29731 = CARTESIAN_POINT ( 'NONE',  ( 0.1049868766404206816, 0.1283753931104748280, 0.1820866141732283561 ) ) ;
#29732 = CARTESIAN_POINT ( 'NONE',  ( 0.5905511811023629321, -0.5511811023622047445, 6.969142054262312111E-17 ) ) ;
#29733 = CARTESIAN_POINT ( 'NONE',  ( 0.3543307086614179147, 0.2952755905511811885, 0.000000000000000000 ) ) ;
#29734 = CARTESIAN_POINT ( 'NONE',  ( -0.4199475065616791736, -0.5023911411419708095, 0.1820866141732285504 ) ) ;
#29735 = CARTESIAN_POINT ( 'NONE',  ( -0.2867679344610364334, -0.2867679344610367109, -2.413385826771653253 ) ) ;
#29736 = CARTESIAN_POINT ( 'NONE',  ( 1.528871391076116026, -0.6692913385826773087, -0.1292274648535924053 ) ) ;
#29737 = CARTESIAN_POINT ( 'NONE',  ( -0.8923884514435688198, -0.6046776061558807314, 0.2411417322834647770 ) ) ;
#29738 = CARTESIAN_POINT ( 'NONE',  ( 0.3458507752293908943, -0.3458507752293908943, -0.8051181102362205966 ) ) ;
#29739 = CARTESIAN_POINT ( 'NONE',  ( -0.07217847769028813698, -0.3162353388693409650, -0.4822834645669289433 ) ) ;
#29740 = CARTESIAN_POINT ( 'NONE',  ( -0.4724409448818890911, -0.1870078740157480879, -0.4822834645669291653 ) ) ;
#29741 = CARTESIAN_POINT ( 'NONE',  ( 1.528871391076116026, 0.1771653543307087630, 0.09757992244046791164 ) ) ;
#29742 = CARTESIAN_POINT ( 'NONE',  ( 0.03937007874015806264, 0.1771653543307087630, 0.000000000000000000 ) ) ;
#29743 = CARTESIAN_POINT ( 'NONE',  ( -0.2624671916010490880, 0.2306618581243847221, -0.2411417322834647770 ) ) ;
#29744 = CARTESIAN_POINT ( 'NONE',  ( -0.5774278215223089816, -0.6046776061558807314, 0.2411417322834647770 ) ) ;
#29745 = CARTESIAN_POINT ( 'NONE',  ( -3.898413161119330450, 2.697625129285034173, 0.5314960629921259283 ) ) ;
#29746 = CARTESIAN_POINT ( 'NONE',  ( -0.2362204724409451284, 0.4091458600556402425, -0.3280839895013123453 ) ) ;
#29747 = CARTESIAN_POINT ( 'NONE',  ( 0.3477690288713918276, -0.6692913385826773087, -0.1292274648535924053 ) ) ;
#29748 = AXIS2_PLACEMENT_3D ( 'NONE', #12580, #6671, #5434 ) ;
#29749 = ORIENTED_EDGE ( 'NONE', *, *, #75585, .T. ) ;
#29750 = CARTESIAN_POINT ( 'NONE',  ( -0.3460692066303960313, 0.1998031496062989965, -1.835301837270341352 ) ) ;
#29751 = CARTESIAN_POINT ( 'NONE',  ( 1.587926509186352142, 0.05413385826771666132, 0.4176697321401328100 ) ) ;
#29752 = CARTESIAN_POINT ( 'NONE',  ( -0.8202099737532801971, -0.5511811023622046335, 0.09757992244046803654 ) ) ;
#29753 = CARTESIAN_POINT ( 'NONE',  ( -0.7414698162729651543, 0.2952755905511810774, -0.1292274648535930714 ) ) ;
#29754 = CARTESIAN_POINT ( 'NONE',  ( 1.240157480314961314, 0.1660481256975883668, -0.3530559997133364547 ) ) ;
#29755 = CARTESIAN_POINT ( 'NONE',  ( 1.364829396325460076, 0.2306618581243848609, 0.2411417322834645549 ) ) ;
#29756 = CARTESIAN_POINT ( 'NONE',  ( -1.430446194225720724, 0.05413385826771626580, -0.4176697321401330321 ) ) ;
#29757 = CARTESIAN_POINT ( 'NONE',  ( -1.023622047244094002, -0.1870078740157480601, -0.3641732283464567677 ) ) ;
#29759 = ADVANCED_FACE ( 'NONE', ( #35545 ), #55298, .F. ) ;
#29758 = CARTESIAN_POINT ( 'NONE',  ( -9.787531504996566615E-17, 0.3996062992125985480, -0.07677165354330711677 ) ) ;
#29760 = CARTESIAN_POINT ( 'NONE',  ( 4.893765752498283924E-17, -0.3996062992125986035, -0.5511811023622047445 ) ) ;
#29761 = CARTESIAN_POINT ( 'NONE',  ( 0.1958661417322836718, -0.3392501089628017219, -2.765767347277902299 ) ) ;
#29762 = CARTESIAN_POINT ( 'NONE',  ( 1.535433070866142558, 0.1771653543307087630, 0.000000000000000000 ) ) ;
#29763 = CARTESIAN_POINT ( 'NONE',  ( 1.056430446194226436, -0.5511811023622048555, -0.09757992244046775898 ) ) ;
#29764 = CARTESIAN_POINT ( 'NONE',  ( 0.7152230971128614723, -0.3162353388693409650, -0.4822834645669289433 ) ) ;
#29765 = CARTESIAN_POINT ( 'NONE',  ( -1.699475065616797398, 0.2952755905511811885, 0.1292274648535926551 ) ) ;
#29766 = CARTESIAN_POINT ( 'NONE',  ( 0.9908136482939640111, 0.2952755905511810774, -0.1292274648535930714 ) ) ;
#29767 = CARTESIAN_POINT ( 'NONE',  ( -0.1974969037888706924, 0.3420746716998658843, -1.034776902887139194 ) ) ;
#29768 = CARTESIAN_POINT ( 'NONE',  ( 1.305774278215223960, -0.5511811023622046335, 0.09757992244046803654 ) ) ;
#29769 = CARTESIAN_POINT ( 'NONE',  ( 0.07874015748031558404, -0.1870078740157479769, 0.4822834645669291653 ) ) ;
#29770 = CARTESIAN_POINT ( 'NONE',  ( -0.9908136482939626788, 0.2952755905511811885, 0.1292274648535926551 ) ) ;
#29771 = CARTESIAN_POINT ( 'NONE',  ( 1.174540682414699111, -0.3162353388693405765, 0.4822834645669290543 ) ) ;
#29772 = CARTESIAN_POINT ( 'NONE',  ( 0.4724409448818898682, 2.892866454678787531E-17, -1.220472440944881942 ) ) ;
#29773 = CARTESIAN_POINT ( 'NONE',  ( 0.3996062992125985480, 0.1070741851644054637, -2.486876640419947382 ) ) ;
#29774 = CARTESIAN_POINT ( 'NONE',  ( 0.4133858267716541968, -0.4536011799217368745, -0.2665933059059886201 ) ) ;
#29775 = VERTEX_POINT ( 'NONE', #80418 ) ;
#29776 = CARTESIAN_POINT ( 'NONE',  ( 0.2867679344610366554, 0.2867679344610366554, -0.6069746963592669298 ) ) ;
#29777 = EDGE_LOOP ( 'NONE', ( #3410, #2554, #49127 ) ) ;
#29778 = CARTESIAN_POINT ( 'NONE',  ( -0.9383202099737524282, -0.05778040916215522460, 0.4822834645669289988 ) ) ;
#29779 = CARTESIAN_POINT ( 'NONE',  ( -0.1968503937007867743, 0.2952755905511811885, 0.000000000000000000 ) ) ;
#29780 = CARTESIAN_POINT ( 'NONE',  ( -0.1771653543307080136, 0.1660481256975883668, -0.3530559997133364547 ) ) ;
#29781 = CARTESIAN_POINT ( 'NONE',  ( 0.8989501312335964611, 0.2952755905511811885, 0.1292274648535926551 ) ) ;
#29782 = CARTESIAN_POINT ( 'NONE',  ( -1.207349081364828436, -0.6046776061558807314, 0.2411417322834647770 ) ) ;
#29783 = CARTESIAN_POINT ( 'NONE',  ( -0.3083989501312330295, -0.05778040916215522460, 0.4822834645669289988 ) ) ;
#29784 = CARTESIAN_POINT ( 'NONE',  ( 0.6299212598425204535, -0.1870078740157479769, 0.4822834645669291653 ) ) ;
#29785 = CARTESIAN_POINT ( 'NONE',  ( 0.2755905511811031494, -0.6692913385826771977, 8.415575281601705876E-17 ) ) ;
#29786 = B_SPLINE_CURVE_WITH_KNOTS ( 'NONE', 3,
 ( #43799, #69503, #30780, #57678, #11438, #11852, #64006, #18166, #5113, #76641, #38748, #24048, #77057, #5927, #70743, #70316, #69904, #51354, #25693, #6347, #75825, #50944, #63180, #18972, #37094, #37505 ),
 .UNSPECIFIED., .F., .F.,
 ( 4, 2, 2, 2, 2, 2, 2, 2, 2, 2, 2, 2, 4 ),
 ( 0.01885843700256156080, 0.02003653724487836768, 0.02121463748719517803, 0.02357083797182877444, 0.02474893821414556744, 0.02592703845646236738, 0.02828323894109595685, 0.03063943942572954632, 0.03181753966804633932, 0.03299563991036313232, 0.03535184039499672526, 0.03652994063731351826, 0.03770804087963031126 ),
 .UNSPECIFIED. ) ;
#29787 = CARTESIAN_POINT ( 'NONE',  ( 0.3917322834645670104, -0.1049643490035303411, -0.8910761154855640909 ) ) ;
#29788 = CARTESIAN_POINT ( 'NONE',  ( -0.3740157480314953431, 0.07958543189024085140, 0.2665933059059887866 ) ) ;
#29789 = ORIENTED_EDGE ( 'NONE', *, *, #55183, .T. ) ;
#29790 = CARTESIAN_POINT ( 'NONE',  ( 0.1974969037888704704, 0.3420746716998660508, -1.404199475065616820 ) ) ;
#29791 = VERTEX_POINT ( 'NONE', #58429 ) ;
#29792 = CARTESIAN_POINT ( 'NONE',  ( -1.181102362204723644, -0.1870078740157480601, -0.3641732283464567677 ) ) ;
#29793 = CARTESIAN_POINT ( 'NONE',  ( -0.5839895013123351797, -0.6692913385826771977, 0.1292274648535927661 ) ) ;
#29794 = CARTESIAN_POINT ( 'NONE',  ( -0.1070741851644051862, -0.3996062992125987146, 0.08530183727034119923 ) ) ;
#29795 = CARTESIAN_POINT ( 'NONE',  ( -0.8792650918635160906, 0.05413385826771626580, -0.4176697321401330321 ) ) ;
#29796 = CARTESIAN_POINT ( 'NONE',  ( -0.6430446194225716283, -0.4281496062992124485, 0.4176697321401328655 ) ) ;
#29797 = CARTESIAN_POINT ( 'NONE',  ( -1.430446194225720724, 0.05413385826771626580, -0.4176697321401330321 ) ) ;
#29798 = CARTESIAN_POINT ( 'NONE',  ( -1.535433070866141225, 0.2952755905511811885, 0.000000000000000000 ) ) ;
#29799 = CARTESIAN_POINT ( 'NONE',  ( 0.8333333333333340365, -0.5511811023622046335, 0.09757992244046803654 ) ) ;
#29800 = CARTESIAN_POINT ( 'NONE',  ( 0.4702942589932804229, 1.601810907557264851, 1.018732849840053634 ) ) ;
#29801 = CARTESIAN_POINT ( 'NONE',  ( 0.2867679344610365999, -0.2867679344610365444, -0.02559055118110245899 ) ) ;
#29802 = CARTESIAN_POINT ( 'NONE',  ( 0.2624671916010504757, -0.5023911411419708095, -0.1820866141732282451 ) ) ;
#29803 = CARTESIAN_POINT ( 'NONE',  ( -0.2952755905511803003, -0.5400638737290845981, -0.3530559997133363437 ) ) ;
#29804 = CARTESIAN_POINT ( 'NONE',  ( -0.2624671916010490880, -0.6046776061558807314, 0.2411417322834647770 ) ) ;
#29805 = EDGE_LOOP ( 'NONE', ( #82297, #7968, #78768, #81918 ) ) ;
#29806 = CARTESIAN_POINT ( 'NONE',  ( -0.2925321140481932924, 0.2925321140481931814, -2.224409448818897239 ) ) ;
#29807 = DIRECTION ( 'NONE',  ( 0.000000000000000000, 0.000000000000000000, 1.000000000000000000 ) ) ;
#29808 = VERTEX_POINT ( 'NONE', #71073 ) ;
#29809 = CARTESIAN_POINT ( 'NONE',  ( 0.1070741851644054776, -0.3996062992125984925, -1.421916010498687877 ) ) ;
#29810 = CARTESIAN_POINT ( 'NONE',  ( -0.03178304480585582292, 0.3983403474834776858, -2.755905511811024500 ) ) ;
#29811 = CARTESIAN_POINT ( 'NONE',  ( -0.5249343832020990641, -0.5023911411419708095, -0.1820866141732282451 ) ) ;
#29812 = CARTESIAN_POINT ( 'NONE',  ( -1.043307086614172707, 0.1660481256975883668, -0.3530559997133364547 ) ) ;
#29813 = CARTESIAN_POINT ( 'NONE',  ( 5.785732909357575061E-17, -0.4724409448818898682, -0.2362204724409449064 ) ) ;
#29814 = CARTESIAN_POINT ( 'NONE',  ( -0.1232739590129246776, 1.078238888412932583, 3.935195127778579938 ) ) ;
#29815 = CARTESIAN_POINT ( 'NONE',  ( 0.3392501089628018329, 0.1958661417322835607, -2.578083989501311901 ) ) ;
#29816 = CARTESIAN_POINT ( 'NONE',  ( 1.345144356955381593, -0.05778040916215522460, 0.4822834645669289988 ) ) ;
#29817 = CARTESIAN_POINT ( 'NONE',  ( 0.4265091863517067039, -0.6692913385826773087, -0.1292274648535924053 ) ) ;
#29818 = CARTESIAN_POINT ( 'NONE',  ( 0.4330708661417329575, 0.2952755905511811885, 0.000000000000000000 ) ) ;
#29819 = CARTESIAN_POINT ( 'NONE',  ( -0.5052493438320203589, 0.1771653543307087075, -0.09757992244046823083 ) ) ;
#29820 = CARTESIAN_POINT ( 'NONE',  ( -0.4330708661417315697, 0.2952755905511811885, 0.000000000000000000 ) ) ;
#29821 = CARTESIAN_POINT ( 'NONE',  ( 0.4724409448818897572, -0.1265901696524988906, -2.393044619422572072 ) ) ;
#29822 = CARTESIAN_POINT ( 'NONE',  ( -0.4724409448818890911, -0.1870078740157479769, 0.4822834645669291653 ) ) ;
#29823 = CARTESIAN_POINT ( 'NONE',  ( 0.3949938075777408852, 0.1058382717557500435, -1.618766404199474929 ) ) ;
#29824 = CARTESIAN_POINT ( 'NONE',  ( 1.338582677165355062, -0.1870078740157480601, -0.3641732283464567677 ) ) ;
#29825 = CARTESIAN_POINT ( 'NONE',  ( -0.3149606299212590610, -0.1870078740157479769, 0.3641732283464567677 ) ) ;
#29826 = CARTESIAN_POINT ( 'NONE',  ( 1.246719160104987623, -0.004921259842519870586, -0.3153832671262229437 ) ) ;
#29827 = CARTESIAN_POINT ( 'NONE',  ( -1.141732283464566011, -0.6692913385826771977, 8.415575281601705876E-17 ) ) ;
#29828 = CARTESIAN_POINT ( 'NONE',  ( -0.9580052493438311334, -0.004921259842519870586, -0.3153832671262229437 ) ) ;
#29829 = DIRECTION ( 'NONE',  ( -0.000000000000000000, -1.000000000000000000, 0.000000000000000000 ) ) ;
#29830 = CARTESIAN_POINT ( 'NONE',  ( -1.207349081364828880, 0.2306618581243847221, -0.2411417322834647770 ) ) ;
#29831 = CARTESIAN_POINT ( 'NONE',  ( -0.3674540682414689785, 0.2306618581243848609, 0.2411417322834645549 ) ) ;
#29832 = CARTESIAN_POINT ( 'NONE',  ( 0.2624671916010504757, 0.2306618581243848609, 0.2411417322834645549 ) ) ;
#29833 = CARTESIAN_POINT ( 'NONE',  ( 0.3392501089628018329, -0.1958661417322834497, -2.389744463745719916 ) ) ;
#29834 = CARTESIAN_POINT ( 'NONE',  ( -2.000606668791069076, 1.230840736495002030, 0.3632157284009445153 ) ) ;
#29835 = CARTESIAN_POINT ( 'NONE',  ( 0.5446194225721792126, -0.2845877964562159024, 0.3641732283464567677 ) ) ;
#29836 = CARTESIAN_POINT ( 'NONE',  ( -1.627296587926508442, -0.5023911411419708095, -0.1820866141732282451 ) ) ;
#29837 = CARTESIAN_POINT ( 'NONE',  ( 0.6692913385826778638, -0.6692913385826771977, 8.415575281601705876E-17 ) ) ;
#29838 = CARTESIAN_POINT ( 'NONE',  ( -1.496062992125983815, -0.1870078740157480601, -0.3641732283464567677 ) ) ;
#29839 = CARTESIAN_POINT ( 'NONE',  ( 1.561679790026247350, -0.3690944881889763329, 0.3153832671262228327 ) ) ;
#29840 = CARTESIAN_POINT ( 'NONE',  ( -1.030183727034119867, -0.05778040916215560624, -0.4822834645669293319 ) ) ;
#29841 = CARTESIAN_POINT ( 'NONE',  ( -0.4658792650918627265, -0.2845877964562161244, -0.3641732283464567121 ) ) ;
#29842 = CARTESIAN_POINT ( 'NONE',  ( 2.795275590551181466, 2.001539355558160871, 0.000000000000000000 ) ) ;
#29843 = CARTESIAN_POINT ( 'NONE',  ( 0.5577427821522314977, -0.2845877964562161244, -0.3641732283464567121 ) ) ;
#29844 = CARTESIAN_POINT ( 'NONE',  ( -0.2362204724409440182, -0.1870078740157479769, 0.4822834645669291653 ) ) ;
#29845 = CARTESIAN_POINT ( 'NONE',  ( -0.1070741851644056997, 0.3996062992125984925, -0.7132545931758530466 ) ) ;
#29846 = EDGE_CURVE ( 'NONE', #75163, #51509, #36052, .T. ) ;
#29847 = CARTESIAN_POINT ( 'NONE',  ( 0.1958661417322836440, -0.3392501089628017219, -1.908792650918635259 ) ) ;
#29848 = CARTESIAN_POINT ( 'NONE',  ( 0.4986876640419954376, 0.1283753931104748280, 0.1820866141732283561 ) ) ;
#29849 = CARTESIAN_POINT ( 'NONE',  ( 0.1968503937007881344, -0.6692913385826771977, 8.415575281601705876E-17 ) ) ;
#29850 = CARTESIAN_POINT ( 'NONE',  ( -0.5052493438320203589, 0.2952755905511810774, -0.1292274648535930714 ) ) ;
#29851 = CARTESIAN_POINT ( 'NONE',  ( -0.2362204724409440182, -0.1870078740157479769, 0.3641732283464567677 ) ) ;
#29852 = PLANE ( 'NONE',  #53498 ) ;
#29853 = CARTESIAN_POINT ( 'NONE',  ( -0.3477690288713902178, 0.1771653543307087075, -0.09757992244046823083 ) ) ;
#29854 = CARTESIAN_POINT ( 'NONE',  ( 0.1181102362204730916, 0.2952755905511811885, 0.000000000000000000 ) ) ;
#29855 = CARTESIAN_POINT ( 'NONE',  ( -1.010498687664041384, -0.3690944881889765550, -0.3153832671262227771 ) ) ;
#29856 = CARTESIAN_POINT ( 'NONE',  ( -0.1070741851644056997, 0.3996062992125984925, -1.500656167979002253 ) ) ;
#29857 = CARTESIAN_POINT ( 'NONE',  ( -1.456692913385826182, 0.2952755905511811885, 0.000000000000000000 ) ) ;
#29858 = CARTESIAN_POINT ( 'NONE',  ( 0.4600214019799526155, 2.784432375088962958E-17, -0.3464511005275205946 ) ) ;
#29859 = ORIENTED_EDGE ( 'NONE', *, *, #8199, .F. ) ;
#29860 = CARTESIAN_POINT ( 'NONE',  ( -1.509186351706035767, -0.004921259842519870586, -0.3153832671262229437 ) ) ;
#29861 = CIRCLE ( 'NONE', #28497, 2.362204724409449064 ) ;
#29862 = CARTESIAN_POINT ( 'NONE',  ( -0.5774278215223089816, 0.2306618581243847221, -0.2411417322834647770 ) ) ;
#29863 = CARTESIAN_POINT ( 'NONE',  ( -1.148293963254592542, 0.2952755905511811885, 0.1292274648535926551 ) ) ;
#29864 = CARTESIAN_POINT ( 'NONE',  ( 0.3392501089628018884, -0.1958661417322834220, -1.764435695538057791 ) ) ;
#29865 = DIRECTION ( 'NONE',  ( -3.096699300667737957E-16, 1.000000000000000000, -0.000000000000000000 ) ) ;
#29866 = CARTESIAN_POINT ( 'NONE',  ( 1.240157480314961314, 0.1660481256975883668, -0.3530559997133364547 ) ) ;
#29867 = CARTESIAN_POINT ( 'NONE',  ( 0.4330708661417329575, 0.2952755905511811885, 0.000000000000000000 ) ) ;
#29868 = DIRECTION ( 'NONE',  ( 0.000000000000000000, -1.000000000000000000, 0.000000000000000000 ) ) ;
#29869 = CARTESIAN_POINT ( 'NONE',  ( 0.3460692066303959202, -0.1998031496062991630, -2.229002624671916344 ) ) ;
#29870 = CARTESIAN_POINT ( 'NONE',  ( 1.581364829396326277, -0.08942795157527998196, 0.3641732283464567121 ) ) ;
#29871 = CARTESIAN_POINT ( 'NONE',  ( -0.2925321140481932924, 0.2925321140481931814, -0.9645669291338579976 ) ) ;
#29872 = ORIENTED_EDGE ( 'NONE', *, *, #69643, .T. ) ;
#29873 = CARTESIAN_POINT ( 'NONE',  ( -1.030183727034119867, -0.2845877964562159024, 0.3641732283464567677 ) ) ;
#29874 = CARTESIAN_POINT ( 'NONE',  ( 0.3917322834645669549, 0.1049643490035304660, -2.793963254593175183 ) ) ;
#29875 = VERTEX_POINT ( 'NONE', #369 ) ;
#29876 = CARTESIAN_POINT ( 'NONE',  ( 0.3412073490813655186, 0.2306618581243848609, 0.2411417322834645549 ) ) ;
#29877 = CARTESIAN_POINT ( 'NONE',  ( -0.2099737532808391705, -0.6046776061558809534, -0.2411417322834644161 ) ) ;
#29878 = CARTESIAN_POINT ( 'NONE',  ( -0.9973753280839886548, 0.2306618581243848609, 0.2411417322834645549 ) ) ;
#29879 = CARTESIAN_POINT ( 'NONE',  ( 1.115485564304462551, -0.4281496062992127816, -0.4176697321401328100 ) ) ;
#29880 = CARTESIAN_POINT ( 'NONE',  ( -1.351706036745406347, -0.3690944881889763329, 0.3153832671262228327 ) ) ;
#29881 = CARTESIAN_POINT ( 'NONE',  ( -0.7974104941589342799, -2.567464376874931580E-15, -0.4445507791589072832 ) ) ;
#29882 = CARTESIAN_POINT ( 'NONE',  ( 0.1049868766404206816, 0.2306618581243848609, 0.2411417322834645549 ) ) ;
#29883 = CARTESIAN_POINT ( 'NONE',  ( -0.9842519685039360366, 0.2952755905511811885, 0.000000000000000000 ) ) ;
#29884 = CARTESIAN_POINT ( 'NONE',  ( -0.2867679344610366554, 0.2867679344610365444, -1.832001681593488751 ) ) ;
#29885 = CARTESIAN_POINT ( 'NONE',  ( -1.548556430446193399, -0.6046776061558809534, -0.2411417322834644161 ) ) ;
#29886 = LINE ( 'NONE', #4222, #15682 ) ;
#29887 = CARTESIAN_POINT ( 'NONE',  ( -0.3392501089628019995, 0.1958661417322832277, 0.1391076115485564701 ) ) ;
#29888 = CARTESIAN_POINT ( 'NONE',  ( 1.062992125984252745, 0.1771653543307087630, 0.000000000000000000 ) ) ;
#29889 = ORIENTED_EDGE ( 'NONE', *, *, #50692, .T. ) ;
#29890 = CARTESIAN_POINT ( 'NONE',  ( -0.1058382717557503211, 0.3949938075777409408, -0.006561679790026304741 ) ) ;
#29891 = CARTESIAN_POINT ( 'NONE',  ( -0.9711286089238838626, 0.2306618581243847221, -0.2411417322834647770 ) ) ;
#29892 = ORIENTED_EDGE ( 'NONE', *, *, #57258, .F. ) ;
#29893 = CARTESIAN_POINT ( 'NONE',  ( 0.3740157480314966754, 0.07958543189024071263, -0.2665933059059888421 ) ) ;
#29894 = CARTESIAN_POINT ( 'NONE',  ( -1.561679790026246017, 0.05413385826771666132, 0.4176697321401328100 ) ) ;
#29895 = CARTESIAN_POINT ( 'NONE',  ( 0.4921259842519691285, 0.1660481256975885056, 0.3530559997133364547 ) ) ;
#29896 = CARTESIAN_POINT ( 'NONE',  ( 0.5971128608923890191, -0.6692913385826771977, 0.1292274648535927661 ) ) ;
#29897 = CARTESIAN_POINT ( 'NONE',  ( -0.09842519685039295696, 0.1660481256975883668, -0.3530559997133364547 ) ) ;
#29898 = CARTESIAN_POINT ( 'NONE',  ( 0.1049643490035304799, -0.3917322834645670104, -1.184402517881576911 ) ) ;
#29899 = CARTESIAN_POINT ( 'NONE',  ( -0.9711286089238838626, 0.2306618581243847221, -0.2411417322834647770 ) ) ;
#29900 = CARTESIAN_POINT ( 'NONE',  ( 0.2867679344610365999, -0.2867679344610365444, -2.230314960629921295 ) ) ;
#29901 = CARTESIAN_POINT ( 'NONE',  ( 1.437007874015748810, 0.07958543189024085140, 0.2665933059059887866 ) ) ;
#29902 = CARTESIAN_POINT ( 'NONE',  ( -1.023622047244093558, -0.1870078740157479769, 0.4822834645669291653 ) ) ;
#29903 = CARTESIAN_POINT ( 'NONE',  ( 1.207349081364829990, 0.2306618581243848609, 0.2411417322834645549 ) ) ;
#29904 = CARTESIAN_POINT ( 'NONE',  ( 1.338582677165355062, -0.1870078740157479769, 0.4822834645669291653 ) ) ;
#29905 = CARTESIAN_POINT ( 'NONE',  ( -0.1070741851644056997, 0.3996062992125986035, -0.3215223097112860362 ) ) ;
#29906 = CARTESIAN_POINT ( 'NONE',  ( -0.9711286089238838626, -0.6046776061558807314, 0.2411417322834647770 ) ) ;
#29907 = CARTESIAN_POINT ( 'NONE',  ( 0.3996062992125984925, 0.1070741851644054637, 0.1135170603674540563 ) ) ;
#29908 = CARTESIAN_POINT ( 'NONE',  ( 0.2493438320209980519, -0.4281496062992127816, -0.4176697321401328100 ) ) ;
#29909 = CARTESIAN_POINT ( 'NONE',  ( 0.3460692066303959757, -0.1998031496062991907, -2.152230971128608950 ) ) ;
#29910 = CARTESIAN_POINT ( 'NONE',  ( -0.6889763779527552368, 0.1660481256975885056, 0.3530559997133364547 ) ) ;
#29911 = CARTESIAN_POINT ( 'NONE',  ( -1.423884514435694859, -0.08942795157528024563, -0.3641732283464568787 ) ) ;
#29912 = CARTESIAN_POINT ( 'NONE',  ( 0.5774278215223104249, 0.1283753931104748280, 0.1820866141732283561 ) ) ;
#29913 = CARTESIAN_POINT ( 'NONE',  ( 1.351706036745407458, -0.4281496062992127816, -0.4176697321401328100 ) ) ;
#29914 = CARTESIAN_POINT ( 'NONE',  ( -0.3458507752293906723, -0.3458507752293910609, -1.238188976377952999 ) ) ;
#29915 = CARTESIAN_POINT ( 'NONE',  ( 0.7152230971128616943, -0.08942795157527998196, 0.3641732283464567121 ) ) ;
#29916 = CARTESIAN_POINT ( 'NONE',  ( 0.9317585301837276734, -0.4281496062992124485, 0.4176697321401328655 ) ) ;
#29917 = VECTOR ( 'NONE', #77654, 39.37007874015748143 ) ;
#29918 = CARTESIAN_POINT ( 'NONE',  ( 0.1974969037888704704, 0.3420746716998660508, -0.6935695538057742304 ) ) ;
#29919 = CARTESIAN_POINT ( 'NONE',  ( -0.7545931758530177724, 0.2952755905511811885, 0.1292274648535926551 ) ) ;
#29920 = CARTESIAN_POINT ( 'NONE',  ( 1.614173228346456712, 0.8346805926620878280, 0.1372047244094478646 ) ) ;
#29921 = CARTESIAN_POINT ( 'NONE',  ( 1.417322834645670104, -0.1870078740157479769, 0.3641732283464567677 ) ) ;
#29922 = CARTESIAN_POINT ( 'NONE',  ( -0.4527559055118102749, 0.1660481256975885056, 0.3530559997133364547 ) ) ;
#29923 = CARTESIAN_POINT ( 'NONE',  ( 5.463695987328526437E-16, -0.1870078740157479769, 0.4822834645669291653 ) ) ;
#29924 = CARTESIAN_POINT ( 'NONE',  ( -1.586052503253849499, 0.4724409448818907564, 0.1653254495020552439 ) ) ;
#29925 = CARTESIAN_POINT ( 'NONE',  ( 0.1902887139107617975, 0.2952755905511811885, 0.1292274648535926551 ) ) ;
#29926 = CARTESIAN_POINT ( 'NONE',  ( 0.2821522309711292364, 0.1771653543307087075, -0.09757992244046823083 ) ) ;
#29927 = CARTESIAN_POINT ( 'NONE',  ( -2.841478809456101207, 1.098283573398291413, -0.1802708669123563034 ) ) ;
#29928 = CARTESIAN_POINT ( 'NONE',  ( 0.1968503937007881344, -0.5511811023622047445, 6.969142054262312111E-17 ) ) ;
#29929 = CARTESIAN_POINT ( 'NONE',  ( 0.7020997375328090762, -0.08942795157528024563, -0.3641732283464568787 ) ) ;
#29930 = CARTESIAN_POINT ( 'NONE',  ( -0.1023049608108107106, 1.074140789190347389, -1.493476385750995394 ) ) ;
#29931 = CARTESIAN_POINT ( 'NONE',  ( 0.2925321140481932369, -0.2925321140481931814, -1.592519685039370358 ) ) ;
#29932 = CARTESIAN_POINT ( 'NONE',  ( 0.2624671916010504757, 0.2306618581243848609, 0.2411417322834645549 ) ) ;
#29933 = CARTESIAN_POINT ( 'NONE',  ( 0.3917322834645670104, -0.1049643490035303411, -1.678477690288713964 ) ) ;
#29934 = CARTESIAN_POINT ( 'NONE',  ( 1.601049868766404982, -0.5023911411419708095, -0.1820866141732282451 ) ) ;
#29935 = CARTESIAN_POINT ( 'NONE',  ( 0.1312335958005257930, 0.2306618581243847221, -0.2411417322834647770 ) ) ;
#29936 = CARTESIAN_POINT ( 'NONE',  ( -0.4068241469816267775, -0.004921259842519870586, -0.3153832671262229437 ) ) ;
#29937 = CARTESIAN_POINT ( 'NONE',  ( -0.05905511811023545637, 0.1660481256975885056, 0.3530559997133364547 ) ) ;
#29938 = CARTESIAN_POINT ( 'NONE',  ( 1.141732283464567788, -0.5511811023622047445, 6.969142054262312111E-17 ) ) ;
#29939 = CARTESIAN_POINT ( 'NONE',  ( 0.4744094488189011249, 1.505635681685443039, -1.016821367227981776 ) ) ;
#29940 = CARTESIAN_POINT ( 'NONE',  ( -1.377952755905511140, 0.2952755905511811885, 0.000000000000000000 ) ) ;
#29941 = CARTESIAN_POINT ( 'NONE',  ( 0.01968503937007957949, -0.5400638737290845981, -0.3530559997133363437 ) ) ;
#29942 = B_SPLINE_CURVE_WITH_KNOTS ( 'NONE', 3,
 ( #24103, #4746, #19446, #43445, #44676, #81792, #30831, #50996 ),
 .UNSPECIFIED., .F., .F.,
 ( 4, 2, 2, 4 ),
 ( 0.03284617093396371978, 0.03527709790192264105, 0.03649256138590211557, 0.03770802486988159008 ),
 .UNSPECIFIED. ) ;
#29943 = CARTESIAN_POINT ( 'NONE',  ( 1.141732283464567788, -0.6692913385826771977, 8.415575281601705876E-17 ) ) ;
#29944 = CARTESIAN_POINT ( 'NONE',  ( -1.614173228346457378, 1.881821177735609085, -0.1372047244094477536 ) ) ;
#29945 = CARTESIAN_POINT ( 'NONE',  ( 0.006561679790026889343, -0.05778040916215522460, 0.4822834645669289988 ) ) ;
#29946 = CARTESIAN_POINT ( 'NONE',  ( 1.371391076115485941, 0.2952755905511811885, 0.1292274648535926551 ) ) ;
#29947 = CARTESIAN_POINT ( 'NONE',  ( 0.7808398950131241190, -0.05778040916215560624, -0.4822834645669293319 ) ) ;
#29948 = CARTESIAN_POINT ( 'NONE',  ( -1.712598425196849572, 0.07958543189024085140, 0.2665933059059887866 ) ) ;
#29949 = CARTESIAN_POINT ( 'NONE',  ( 0.8595800524934390507, -0.2845877964562159024, 0.3641732283464567677 ) ) ;
#29950 = CARTESIAN_POINT ( 'NONE',  ( -1.528871391076114250, -0.5511811023622046335, 0.09757992244046803654 ) ) ;
#29951 = CARTESIAN_POINT ( 'NONE',  ( 0.2755905511811031494, -0.5511811023622047445, 6.969142054262312111E-17 ) ) ;
#29952 = CARTESIAN_POINT ( 'NONE',  ( -0.2952755905511803003, -0.5400638737290845981, -0.3530559997133363437 ) ) ;
#29953 = CARTESIAN_POINT ( 'NONE',  ( 0.5052493438320215802, 0.2952755905511811885, 0.1292274648535926551 ) ) ;
#29954 = CARTESIAN_POINT ( 'NONE',  ( -0.2624671916010490880, -0.6046776061558807314, 0.2411417322834647770 ) ) ;
#29955 = AXIS2_PLACEMENT_3D ( 'NONE', #76632, #31173, #18563 ) ;
#29956 = CARTESIAN_POINT ( 'NONE',  ( -0.3392501089628019995, 0.1958661417322831999, -2.227709604495750284 ) ) ;
#29957 = CARTESIAN_POINT ( 'NONE',  ( -0.3083989501312330295, -0.08942795157527998196, 0.3641732283464567121 ) ) ;
#29958 = CARTESIAN_POINT ( 'NONE',  ( 0.9711286089238851948, 0.2306618581243848609, 0.2411417322834645549 ) ) ;
#29959 = CARTESIAN_POINT ( 'NONE',  ( 1.082677165354331228, 0.07958543189024071263, -0.2665933059059888421 ) ) ;
#29960 = CARTESIAN_POINT ( 'NONE',  ( 0.1312335958005257930, 0.2306618581243847221, -0.2411417322834647770 ) ) ;
#29961 = CARTESIAN_POINT ( 'NONE',  ( -1.681781318038497730, 1.161248049485916312, 0.2892642709497436071 ) ) ;
#29963 = CARTESIAN_POINT ( 'NONE',  ( 1.581364829396326277, -0.05778040916215522460, 0.4822834645669289988 ) ) ;
#29962 = CARTESIAN_POINT ( 'NONE',  ( 3.937007874015748143, 2.755905511811024056, -0.5314960629921260393 ) ) ;
#29964 = CARTESIAN_POINT ( 'NONE',  ( -0.3917322834645671215, 0.1049643490035301469, -2.229658792650918819 ) ) ;
#29965 = CARTESIAN_POINT ( 'NONE',  ( -1.312335958005248715, 0.2306618581243848609, 0.2411417322834645549 ) ) ;
#29966 = CARTESIAN_POINT ( 'NONE',  ( -0.3805774278215216522, -0.4281496062992127816, -0.4176697321401328100 ) ) ;
#29967 = CARTESIAN_POINT ( 'NONE',  ( -0.3458507752293906723, -0.3458507752293910609, -0.05905511811023620578 ) ) ;
#29968 = CARTESIAN_POINT ( 'NONE',  ( -0.1974969037888703871, -0.3420746716998661063, -2.742782152230970993 ) ) ;
#29969 = ORIENTED_EDGE ( 'NONE', *, *, #66020, .F. ) ;
#29970 = CARTESIAN_POINT ( 'NONE',  ( 0.4396325459317593221, 0.1771653543307087075, -0.09757992244046823083 ) ) ;
#29972 = CARTESIAN_POINT ( 'NONE',  ( -0.2867679344610365999, 0.2867679344610364889, -1.429133858267716661 ) ) ;
#29971 = AXIS2_PLACEMENT_3D ( 'NONE', #11344, #74502, #16850 ) ;
#29973 = CARTESIAN_POINT ( 'NONE',  ( 0.9317585301837276734, -0.4281496062992124485, 0.4176697321401328655 ) ) ;
#29974 = CARTESIAN_POINT ( 'NONE',  ( 0.4091458600556404646, -0.2362204724409448231, -2.624671916010498762 ) ) ;
#29975 = CARTESIAN_POINT ( 'NONE',  ( 1.010498687664042716, 0.05413385826771626580, -0.4176697321401330321 ) ) ;
#29976 = CARTESIAN_POINT ( 'NONE',  ( -1.699475065616797398, 0.1771653543307087630, 0.09757992244046791164 ) ) ;
#29977 = CARTESIAN_POINT ( 'NONE',  ( 1.437007874015748810, -0.5400638737290845981, -0.3530559997133363437 ) ) ;
#29978 = EDGE_CURVE ( 'NONE', #39084, #74503, #49152, .T. ) ;
#29979 = CARTESIAN_POINT ( 'NONE',  ( 1.194225721784777594, -0.3690944881889765550, -0.3153832671262227771 ) ) ;
#29980 = CARTESIAN_POINT ( 'NONE',  ( 0.4724409448818904789, -0.1870078740157480879, -0.4822834645669291653 ) ) ;
#29981 = CARTESIAN_POINT ( 'NONE',  ( 0.1958661417322834497, 0.3392501089628018329, -0.2243901330370585701 ) ) ;
#29982 = CARTESIAN_POINT ( 'NONE',  ( -0.2690288713910754526, -0.6692913385826771977, 0.1292274648535927661 ) ) ;
#29983 = CARTESIAN_POINT ( 'NONE',  ( -1.023622047244094002, -0.1870078740157480601, -0.3641732283464567677 ) ) ;
#29984 = CARTESIAN_POINT ( 'NONE',  ( 0.3937007874015754361, -0.1870078740157480879, -0.4822834645669291653 ) ) ;
#29986 = ADVANCED_FACE ( 'NONE', ( #69822 ), #39072, .F. ) ;
#29985 = CARTESIAN_POINT ( 'NONE',  ( -0.1574803149606292529, -0.1870078740157479769, 0.4822834645669291653 ) ) ;
#29987 = CARTESIAN_POINT ( 'NONE',  ( 0.5118110236220478892, 0.2952755905511811885, 0.000000000000000000 ) ) ;
#29988 = CARTESIAN_POINT ( 'NONE',  ( 2.795275590551181910, 1.535433070866142335, 0.000000000000000000 ) ) ;
#29989 = CARTESIAN_POINT ( 'NONE',  ( -0.2867679344610367109, 0.2867679344610365444, -1.591226664863204077 ) ) ;
#29990 = CARTESIAN_POINT ( 'NONE',  ( 1.023622047244095334, -0.1870078740157479769, 0.4822834645669291653 ) ) ;
#29991 = CARTESIAN_POINT ( 'NONE',  ( -0.4133858267716528645, 0.1660481256975883668, -0.3530559997133364547 ) ) ;
#29992 = CARTESIAN_POINT ( 'NONE',  ( -1.371391076115484609, -0.6692913385826771977, 0.1292274648535927661 ) ) ;
#29993 = CARTESIAN_POINT ( 'NONE',  ( 0.9317585301837276734, -0.4281496062992124485, 0.4176697321401328655 ) ) ;
#29994 = CARTESIAN_POINT ( 'NONE',  ( 0.5314960629921267055, -0.5400638737290844871, 0.3530559997133364547 ) ) ;
#29995 = CARTESIAN_POINT ( 'NONE',  ( 0.1049643490035303689, 0.3917322834645670104, -1.022965879265091749 ) ) ;
#29996 = CARTESIAN_POINT ( 'NONE',  ( -0.2034120734908131112, -0.6692913385826773087, -0.1292274648535924053 ) ) ;
#29997 = CARTESIAN_POINT ( 'NONE',  ( 0.07874015748031558404, -0.1870078740157479769, 0.4822834645669291653 ) ) ;
#29998 = CARTESIAN_POINT ( 'NONE',  ( -0.3740157480314953431, 0.1660481256975885056, 0.3530559997133364547 ) ) ;
#29999 = CARTESIAN_POINT ( 'NONE',  ( 0.4199475065616805614, 0.1283753931104748280, 0.1820866141732283561 ) ) ;
#30000 = CARTESIAN_POINT ( 'NONE',  ( 1.620734908136483465, -0.5511811023622046335, 0.09757992244046803654 ) ) ;
#30001 = CARTESIAN_POINT ( 'NONE',  ( -0.6299212598425332210, 2.165354330708661568, 3.886287458032460229 ) ) ;
#30002 = CARTESIAN_POINT ( 'NONE',  ( 0.3674540682414705883, 0.2306618581243847221, -0.2411417322834647770 ) ) ;
#30003 = FACE_OUTER_BOUND ( 'NONE', #61870, .T. ) ;
#30004 = CARTESIAN_POINT ( 'NONE',  ( -1.620734908136482577, 0.2952755905511811885, 0.1292274648535926551 ) ) ;
#30005 = CARTESIAN_POINT ( 'NONE',  ( 0.4921259842519691841, 0.1012011053420777407, 0.2882089793578257453 ) ) ;
#30006 = ORIENTED_EDGE ( 'NONE', *, *, #58860, .T. ) ;
#30007 = EDGE_CURVE ( 'NONE', #2585, #46748, #19717, .T. ) ;
#30008 = ORIENTED_EDGE ( 'NONE', *, *, #55359, .F. ) ;
#30009 = CARTESIAN_POINT ( 'NONE',  ( 0.5511811023622055217, -0.1870078740157479769, 0.4822834645669291653 ) ) ;
#30010 = CARTESIAN_POINT ( 'NONE',  ( 0.1377952755905518800, -0.4536011799217367080, 0.2665933059059888421 ) ) ;
#30012 = CARTESIAN_POINT ( 'NONE',  ( -3.224202737261815166, 2.716535433070866645, -0.5314960629921260393 ) ) ;
#30011 = CARTESIAN_POINT ( 'NONE',  ( -1.016821367227983997, 1.537401574803149984, 0.4744094488188970171 ) ) ;
#30013 = CARTESIAN_POINT ( 'NONE',  ( -0.3917322834645671215, 0.1049643490035301469, -0.7473753280839893209 ) ) ;
#30014 = CARTESIAN_POINT ( 'NONE',  ( -0.9568149321855660139, 1.315108829465093930E-15, -0.3627985898453513491 ) ) ;
#30015 = CARTESIAN_POINT ( 'NONE',  ( 0.4563452811745912219, 0.01305114060239447385, -2.130073781772667374 ) ) ;
#30016 = CARTESIAN_POINT ( 'NONE',  ( -0.2925321140481932369, 0.2925321140481931259, -2.458661417322834719 ) ) ;
#30017 = CARTESIAN_POINT ( 'NONE',  ( 0.5511811023622054106, -0.1870078740157480879, -0.4822834645669291653 ) ) ;
#30018 = CARTESIAN_POINT ( 'NONE',  ( -0.8136482939632537770, 0.2306618581243847221, -0.2411417322834647770 ) ) ;
#30019 = CIRCLE ( 'NONE', #25989, 3.228346456692913424 ) ;
#30020 = CARTESIAN_POINT ( 'NONE',  ( -0.8858267716535425107, 0.1660481256975883668, -0.3530559997133364547 ) ) ;
#30021 = CARTESIAN_POINT ( 'NONE',  ( 0.5905511811023629321, -0.6692913385826771977, 8.415575281601705876E-17 ) ) ;
#30022 = CARTESIAN_POINT ( 'NONE',  ( 1.574803149606299746, -0.1870078740157479769, 0.4822834645669291653 ) ) ;
#30023 = CARTESIAN_POINT ( 'NONE',  ( 1.240157480314961314, 0.07958543189024071263, -0.2665933059059888421 ) ) ;
#30024 = PRODUCT_CONTEXT ( 'NONE', #61604, 'mechanical' ) ;
#30025 = CARTESIAN_POINT ( 'NONE',  ( 1.115485564304462551, -0.3690944881889765550, -0.3153832671262227771 ) ) ;
#30026 = CARTESIAN_POINT ( 'NONE',  ( -0.7742782152230962556, -0.4281496062992127816, -0.4176697321401328100 ) ) ;
#30027 = CARTESIAN_POINT ( 'NONE',  ( 0.1998031496062992463, 0.3460692066303959202, -0.6935695538057742304 ) ) ;
#30028 = CARTESIAN_POINT ( 'NONE',  ( 1.541994750656168645, 0.2952755905511810774, -0.1292274648535930714 ) ) ;
#30029 = CARTESIAN_POINT ( 'NONE',  ( 0.4724409448818898682, 2.892866454678787531E-17, -2.084645669291338432 ) ) ;
#30030 = CARTESIAN_POINT ( 'NONE',  ( -0.3805774278215216522, 0.05413385826771666132, 0.4176697321401328100 ) ) ;
#30032 = CARTESIAN_POINT ( 'NONE',  ( 0.000000000000000000, 2.401574803149606474, 0.000000000000000000 ) ) ;
#30031 = CARTESIAN_POINT ( 'NONE',  ( 1.036745406824147731, 0.05413385826771666132, 0.4176697321401328100 ) ) ;
#30033 = CARTESIAN_POINT ( 'NONE',  ( -1.056430446194224881, 0.1771653543307087075, -0.09757992244046823083 ) ) ;
#30034 = CARTESIAN_POINT ( 'NONE',  ( 0.5839895013123367340, 0.2952755905511811885, 0.1292274648535926551 ) ) ;
#30035 = CARTESIAN_POINT ( 'NONE',  ( 0.9580052493438326877, -0.004921259842519576551, 0.3153832671262227771 ) ) ;
#30036 = CARTESIAN_POINT ( 'NONE',  ( -0.1049643490035306742, 0.3917322834645668994, -1.818878322013436355 ) ) ;
#30037 = VECTOR ( 'NONE', #37862, 39.37007874015748143 ) ;
#30038 = CARTESIAN_POINT ( 'NONE',  ( -1.181102362204723644, -0.1870078740157480601, -0.3641732283464567677 ) ) ;
#30039 = CARTESIAN_POINT ( 'NONE',  ( 1.253280839895013710, -0.05778040916215560624, -0.4822834645669293319 ) ) ;
#30040 = CARTESIAN_POINT ( 'NONE',  ( 1.080276388343102000E-18, 2.169649841009090648E-17, 0.1771653543307086798 ) ) ;
#30041 = CARTESIAN_POINT ( 'NONE',  ( -0.1837270341207343505, -0.5023911411419708095, 0.1820866141732285504 ) ) ;
#30042 = CARTESIAN_POINT ( 'NONE',  ( -0.3018372703412066094, 0.05413385826771666132, 0.4176697321401328100 ) ) ;
#30043 = CARTESIAN_POINT ( 'NONE',  ( -1.161417322834644716, 0.07958543189024085140, 0.2665933059059887866 ) ) ;
#30044 = CARTESIAN_POINT ( 'NONE',  ( -0.5971128608923877978, 0.2952755905511811885, 0.1292274648535926551 ) ) ;
#30045 = CARTESIAN_POINT ( 'NONE',  ( 1.338582677165355062, -0.1870078740157479769, 0.4822834645669291653 ) ) ;
#30046 = CARTESIAN_POINT ( 'NONE',  ( 0.3917322834645670659, -0.1049643490035303273, -0.4232476622385321074 ) ) ;
#30047 = CARTESIAN_POINT ( 'NONE',  ( -0.9055118110236215490, -0.5511811023622047445, 6.969142054262312111E-17 ) ) ;
#30048 = CARTESIAN_POINT ( 'NONE',  ( 0.000000000000000000, 2.677165354330708791, 0.000000000000000000 ) ) ;
#30049 = CARTESIAN_POINT ( 'NONE',  ( 1.325459317585302665, 0.05413385826771626580, -0.4176697321401330321 ) ) ;
#30050 = CARTESIAN_POINT ( 'NONE',  ( 0.3458507752293908943, 0.3458507752293908943, -2.104330708661417138 ) ) ;
#30051 = CARTESIAN_POINT ( 'NONE',  ( -1.246719160104986512, 0.05413385826771666132, 0.4176697321401328100 ) ) ;
#30053 = EDGE_CURVE ( 'NONE', #30109, #58566, #18077, .T. ) ;
#30052 = CARTESIAN_POINT ( 'NONE',  ( -1.227034120734907141, -0.5511811023622048555, -0.09757992244046775898 ) ) ;
#30054 = CARTESIAN_POINT ( 'NONE',  ( -0.5511811023622041894, -0.1870078740157480601, -0.3641732283464567677 ) ) ;
#30055 = CARTESIAN_POINT ( 'NONE',  ( -0.5314960629921250401, 0.1012011053420777407, 0.2882089793578256898 ) ) ;
#30056 = CARTESIAN_POINT ( 'NONE',  ( 0.1771653543307093182, -0.5400638737290845981, -0.3530559997133363437 ) ) ;
#30057 = CARTESIAN_POINT ( 'NONE',  ( 0.1443569553805781891, -0.004921259842519870586, -0.3153832671262229437 ) ) ;
#30058 = CARTESIAN_POINT ( 'NONE',  ( -1.312335958005248715, -0.5023911411419708095, -0.1820866141732282451 ) ) ;
#30059 = CARTESIAN_POINT ( 'NONE',  ( -1.384514435695537005, 0.2952755905511811885, 0.1292274648535926551 ) ) ;
#30060 = CARTESIAN_POINT ( 'NONE',  ( 1.364829396325459854, -0.5023911411419708095, -0.1820866141732282451 ) ) ;
#30061 = CARTESIAN_POINT ( 'NONE',  ( 1.167979002624672580, -0.4281496062992124485, 0.4176697321401328655 ) ) ;
#30062 = CARTESIAN_POINT ( 'NONE',  ( -0.4724409448818898682, -8.678599364036362592E-17, -2.163385826771653697 ) ) ;
#30063 = CARTESIAN_POINT ( 'NONE',  ( 0.2493438320209980519, -0.004921259842519576551, 0.3153832671262227771 ) ) ;
#30064 = CARTESIAN_POINT ( 'NONE',  ( 0.7808398950131241190, -0.05778040916215560624, -0.4822834645669293319 ) ) ;
#30065 = CARTESIAN_POINT ( 'NONE',  ( 0.9186351706036751663, -0.5023911411419708095, 0.1820866141732285504 ) ) ;
#30066 = ORIENTED_EDGE ( 'NONE', *, *, #82328, .F. ) ;
#30067 = CARTESIAN_POINT ( 'NONE',  ( -1.181102362204723644, -0.1870078740157479769, 0.4822834645669291653 ) ) ;
#30068 = EDGE_CURVE ( 'NONE', #49008, #3939, #66058, .T. ) ;
#30069 = CARTESIAN_POINT ( 'NONE',  ( -1.095800524934382292, -0.3162353388693409650, -0.4822834645669289433 ) ) ;
#30070 = CARTESIAN_POINT ( 'NONE',  ( -0.2362204724409442680, -0.1870078740157480879, -0.4822834645669291653 ) ) ;
#30071 = CARTESIAN_POINT ( 'NONE',  ( -1.712598425196849572, 0.07958543189024085140, 0.2665933059059887866 ) ) ;
#30072 = CARTESIAN_POINT ( 'NONE',  ( 0.1070741851644053388, 0.3996062992125986035, -2.117454068241469756 ) ) ;
#30073 = CARTESIAN_POINT ( 'NONE',  ( 0.7020997375328090762, -0.05778040916215560624, -0.4822834645669293319 ) ) ;
#30074 = CARTESIAN_POINT ( 'NONE',  ( -1.692913385826770645, 0.2952755905511811885, 0.000000000000000000 ) ) ;
#30075 = CARTESIAN_POINT ( 'NONE',  ( 8.195543980992789655E-16, -0.1870078740157480879, -0.4822834645669291653 ) ) ;
#30076 = CARTESIAN_POINT ( 'NONE',  ( 0.9120734908136489683, -0.6692913385826771977, 0.1292274648535927661 ) ) ;
#30077 = CARTESIAN_POINT ( 'NONE',  ( -0.3460692066303958092, -0.1998031496062994683, -1.784776902887138972 ) ) ;
#30078 = CARTESIAN_POINT ( 'NONE',  ( 0.2891555358219910499, -0.2891555358219909944, -1.515748031496063186 ) ) ;
#30079 = CARTESIAN_POINT ( 'NONE',  ( -0.3996062992125986035, -0.1070741851644056997, -2.408136482939632561 ) ) ;
#30080 = CARTESIAN_POINT ( 'NONE',  ( 0.000000000000000000, 0.000000000000000000, 0.000000000000000000 ) ) ;
#30081 = VECTOR ( 'NONE', #54120, 39.37007874015748143 ) ;
#30082 = CARTESIAN_POINT ( 'NONE',  ( 0.3917322834645669549, 0.1049643490035304660, -0.5892388451443569819 ) ) ;
#30083 = CARTESIAN_POINT ( 'NONE',  ( -0.4658792650918627265, -0.08942795157527998196, 0.3641732283464567121 ) ) ;
#30084 = CARTESIAN_POINT ( 'NONE',  ( -0.6430446194225716283, -0.4281496062992124485, 0.4176697321401328655 ) ) ;
#30085 = CARTESIAN_POINT ( 'NONE',  ( 0.3280839895013130669, 0.05413385826771666132, 0.4176697321401328100 ) ) ;
#30086 = CARTESIAN_POINT ( 'NONE',  ( -0.1974969037888706924, 0.3420746716998658843, -2.137139107611548905 ) ) ;
#30087 = CARTESIAN_POINT ( 'NONE',  ( -1.640419947506561060, 0.05413385826771666132, 0.4176697321401328100 ) ) ;
#30088 = CARTESIAN_POINT ( 'NONE',  ( 1.364829396325459854, -0.6046776061558809534, -0.2411417322834644161 ) ) ;
#30089 = CARTESIAN_POINT ( 'NONE',  ( -0.1265901696524986964, -0.4724409448818899238, -2.591863517060367439 ) ) ;
#30090 = CARTESIAN_POINT ( 'NONE',  ( -9.787531504996567848E-17, 0.3996062992125986035, -1.574803149606299302 ) ) ;
#30091 = CARTESIAN_POINT ( 'NONE',  ( 1.968503937007874072, 0.000000000000000000, 5.701968306260621233 ) ) ;
#30092 = CARTESIAN_POINT ( 'NONE',  ( 0.8070866141732288002, 0.1660481256975885056, 0.3530559997133364547 ) ) ;
#30093 = CARTESIAN_POINT ( 'NONE',  ( 0.6364829396325465405, -0.05778040916215522460, 0.4822834645669289988 ) ) ;
#30094 = CIRCLE ( 'NONE', #62356, 0.09842519685039351207 ) ;
#30095 = CARTESIAN_POINT ( 'NONE',  ( 1.115485564304462551, -0.004921259842519576551, 0.3153832671262227771 ) ) ;
#30097 = CARTESIAN_POINT ( 'NONE',  ( -1.528871391076114250, -0.6692913385826771977, 0.1292274648535927661 ) ) ;
#30096 = CARTESIAN_POINT ( 'NONE',  ( -1.437007874015747477, 0.07958543189024071263, -0.2665933059059888421 ) ) ;
#30098 = CARTESIAN_POINT ( 'NONE',  ( -0.3917322834645670104, -7.196005306013484475E-17, 0.1909448818897636901 ) ) ;
#30099 =( LENGTH_UNIT ( ) NAMED_UNIT ( * ) SI_UNIT ( $, .METRE. ) );
#30100 = CARTESIAN_POINT ( 'NONE',  ( 0.8923884514435703741, 0.2306618581243848609, 0.2411417322834645549 ) ) ;
#30101 = CARTESIAN_POINT ( 'NONE',  ( -2.795275590551181466, 2.165354330708661568, 0.000000000000000000 ) ) ;
#30102 = CARTESIAN_POINT ( 'NONE',  ( -0.4527559055118102749, 0.1660481256975885056, 0.3530559997133364547 ) ) ;
#30103 = CARTESIAN_POINT ( 'NONE',  ( -0.7086614173228339419, -0.1870078740157480879, -0.4822834645669291653 ) ) ;
#30104 = CARTESIAN_POINT ( 'NONE',  ( -1.620734908136482577, 0.2952755905511811885, 0.1292274648535926551 ) ) ;
#30105 = CARTESIAN_POINT ( 'NONE',  ( 0.3917322834645669549, 0.1049643490035304660, -0.2093175853018373611 ) ) ;
#30106 = CARTESIAN_POINT ( 'NONE',  ( 0.3740157480314966754, 0.1660481256975883668, -0.3530559997133364547 ) ) ;
#30107 = CARTESIAN_POINT ( 'NONE',  ( 0.3392501089628018329, 0.1958661417322835607, -2.485564304461941987 ) ) ;
#30108 = CARTESIAN_POINT ( 'NONE',  ( 1.496062992125985147, -0.1870078740157479769, 0.4822834645669291653 ) ) ;
#30109 = VERTEX_POINT ( 'NONE', #38657 ) ;
#30110 = CARTESIAN_POINT ( 'NONE',  ( -0.1974969037888703871, -0.3420746716998661063, -2.900262467191600635 ) ) ;
#30111 = VERTEX_POINT ( 'NONE', #63915 ) ;
#30112 = DIRECTION ( 'NONE',  ( -0.000000000000000000, -1.000000000000000000, -0.000000000000000000 ) ) ;
#30113 = CARTESIAN_POINT ( 'NONE',  ( 1.187664041994751285, -0.2845877964562161244, -0.3641732283464567121 ) ) ;
#30114 = CARTESIAN_POINT ( 'NONE',  ( -9.787531504996567848E-17, 0.3996062992125986035, -1.102362204724409489 ) ) ;
#30115 = CARTESIAN_POINT ( 'NONE',  ( 1.548556430446194954, 0.1283753931104746893, -0.1820866141732285504 ) ) ;
#30116 = DIRECTION ( 'NONE',  ( -0.5773502691896305050, -0.5773502691896320593, 0.5773502691896145178 ) ) ;
#30117 = LINE ( 'NONE', #17921, #51697 ) ;
#30118 = CARTESIAN_POINT ( 'NONE',  ( -0.06257671775081299903, 1.952079521258549777, 0.3070762858441002940 ) ) ;
#30119 = CARTESIAN_POINT ( 'NONE',  ( 0.2867679344610365999, 0.2867679344610365999, -0.2224409448818898127 ) ) ;
#30120 = CARTESIAN_POINT ( 'NONE',  ( -0.2230971128608915943, -0.004921259842519576551, 0.3153832671262227771 ) ) ;
#30121 = CARTESIAN_POINT ( 'NONE',  ( -1.240157480314959759, 0.07958543189024085140, 0.2665933059059887866 ) ) ;
#30122 = CARTESIAN_POINT ( 'NONE',  ( 1.450131233595801428, 0.2952755905511811885, 0.1292274648535926551 ) ) ;
#30123 = CARTESIAN_POINT ( 'NONE',  ( 0.5314960629921264834, 0.1660481256975883668, -0.3530559997133364547 ) ) ;
#30124 = CARTESIAN_POINT ( 'NONE',  ( -1.272965879265091305, 0.05413385826771626580, -0.4176697321401330321 ) ) ;
#30125 = CARTESIAN_POINT ( 'NONE',  ( 0.3917322834645669549, 0.1049643490035304660, -0.1167979002624671692 ) ) ;
#30126 = VERTEX_POINT ( 'NONE', #76968 ) ;
#30127 = CARTESIAN_POINT ( 'NONE',  ( 1.417322834645670104, -0.1870078740157479769, 0.4822834645669291653 ) ) ;
#30128 = CARTESIAN_POINT ( 'NONE',  ( -1.614173228346457378, 0.2753471884572478157, -0.1372047244094478091 ) ) ;
#30129 = CARTESIAN_POINT ( 'NONE',  ( -0.4724409448818898682, -8.678599364036362592E-17, -1.614173228346456712 ) ) ;
#30130 = CARTESIAN_POINT ( 'NONE',  ( 1.604771003085129433, 1.044625174762918496, -0.1466069496707749775 ) ) ;
#30131 = CARTESIAN_POINT ( 'NONE',  ( 4.797336870675656522E-17, -0.3917322834645670104, -2.683070866141731958 ) ) ;
#30132 = CARTESIAN_POINT ( 'NONE',  ( -0.6102362204724400829, -0.5400638737290845981, -0.3530559997133363437 ) ) ;
#30133 = CARTESIAN_POINT ( 'NONE',  ( 1.279527559055118724, -0.5400638737290845981, -0.3530559997133363437 ) ) ;
#30135 = CARTESIAN_POINT ( 'NONE',  ( 5.785732909357575061E-17, -0.4724409448818898682, -1.968503937007873850 ) ) ;
#30134 = CARTESIAN_POINT ( 'NONE',  ( 0.5314960629921064994, 2.716535433070866645, 1.854472803289057836 ) ) ;
#30136 = EDGE_CURVE ( 'NONE', #11377, #36098, #75263, .T. ) ;
#30137 = CARTESIAN_POINT ( 'NONE',  ( 1.443569553805774897, -0.6046776061558809534, -0.2411417322834644161 ) ) ;
#30138 = CARTESIAN_POINT ( 'NONE',  ( -0.8595800524934373854, -0.3162353388693409650, -0.4822834645669289433 ) ) ;
#30139 = CARTESIAN_POINT ( 'NONE',  ( 0.1049643490035303689, 0.3917322834645668994, -0.3884321277877147427 ) ) ;
#30140 = CARTESIAN_POINT ( 'NONE',  ( -0.1312335958005241554, 0.1283753931104748280, 0.1820866141732283561 ) ) ;
#30141 = CARTESIAN_POINT ( 'NONE',  ( 0.1049643490035303689, 0.3917322834645670104, -0.3930446194225722945 ) ) ;
#30142 = AXIS2_PLACEMENT_3D ( 'NONE', #18747, #43575, #82323 ) ;
#30143 = EDGE_CURVE ( 'NONE', #53475, #77295, #50445, .T. ) ;
#30144 = CARTESIAN_POINT ( 'NONE',  ( -0.2362204724409440182, -0.1870078740157479769, 0.3641732283464567677 ) ) ;
#30145 = CARTESIAN_POINT ( 'NONE',  ( 0.4658792650918640033, -0.2845877964562159024, 0.3641732283464567677 ) ) ;
#30146 = CARTESIAN_POINT ( 'NONE',  ( 0.6627296587926515548, 0.2952755905511811885, 0.1292274648535926551 ) ) ;
#30147 = CARTESIAN_POINT ( 'NONE',  ( -0.8923884514435688198, -0.5023911411419708095, 0.1820866141732285504 ) ) ;
#30148 = CARTESIAN_POINT ( 'NONE',  ( -0.3917322834645671215, 0.1049643490035301469, -2.544619422572177658 ) ) ;
#30149 = CARTESIAN_POINT ( 'NONE',  ( -1.633858267716534529, 0.1660481256975885056, 0.3530559997133364547 ) ) ;
#30150 = CARTESIAN_POINT ( 'NONE',  ( -1.062992125984250968, -0.6692913385826771977, 8.415575281601705876E-17 ) ) ;
#30151 = CARTESIAN_POINT ( 'NONE',  ( 0.1265901696524989462, 0.4724409448818897572, -0.8576115485564304031 ) ) ;
#30152 = CARTESIAN_POINT ( 'NONE',  ( -0.08530183727034056085, -0.05778040916215560624, -0.4822834645669293319 ) ) ;
#30153 = CARTESIAN_POINT ( 'NONE',  ( -0.3412073490813641308, 0.2306618581243847221, -0.2411417322834647770 ) ) ;
#30154 = CARTESIAN_POINT ( 'NONE',  ( 1.292650918635171564, -0.5511811023622048555, -0.09757992244046775898 ) ) ;
#30155 = CARTESIAN_POINT ( 'NONE',  ( 0.2887139107611556010, -0.5023911411419708095, 0.1820866141732285504 ) ) ;
#30156 = CARTESIAN_POINT ( 'NONE',  ( -0.05249343832020938322, -0.6046776061558809534, -0.2411417322834644161 ) ) ;
#30157 = CARTESIAN_POINT ( 'NONE',  ( -0.8005249343832011588, 0.05413385826771626580, -0.4176697321401330321 ) ) ;
#30158 = CARTESIAN_POINT ( 'NONE',  ( -0.6365311798326280801, 1.942272084518505082, -0.5177672855602343249 ) ) ;
#30159 = CARTESIAN_POINT ( 'NONE',  ( 1.502624671916010790, -0.08942795157527998196, 0.3641732283464567121 ) ) ;
#30160 = CARTESIAN_POINT ( 'NONE',  ( 0.1181102362204730916, 0.2952755905511811885, 0.000000000000000000 ) ) ;
#30161 = VERTEX_POINT ( 'NONE', #44535 ) ;
#30162 = CARTESIAN_POINT ( 'NONE',  ( -0.1998031496062994405, 0.3460692066303957537, -1.822178477690288512 ) ) ;
#30163 = CARTESIAN_POINT ( 'NONE',  ( 1.056430446194226436, -0.6692913385826773087, -0.1292274648535924053 ) ) ;
#30164 = CARTESIAN_POINT ( 'NONE',  ( -0.5380577427821514602, -0.3690944881889765550, -0.3153832671262227771 ) ) ;
#30165 = CARTESIAN_POINT ( 'NONE',  ( -0.7808398950131225646, -0.05778040916215522460, 0.4822834645669289988 ) ) ;
#30166 = CARTESIAN_POINT ( 'NONE',  ( 1.108923884514436686, -0.3162353388693409650, -0.4822834645669289433 ) ) ;
#30167 = CARTESIAN_POINT ( 'NONE',  ( 0.7874015748031503170, -0.1870078740157480879, -0.4822834645669291653 ) ) ;
#30168 = CARTESIAN_POINT ( 'NONE',  ( -1.561679790026246017, -0.4281496062992127816, -0.4176697321401328100 ) ) ;
#30169 = CARTESIAN_POINT ( 'NONE',  ( -1.200787401574802349, 0.07958543189024071263, -0.2665933059059888421 ) ) ;
#30170 = CARTESIAN_POINT ( 'NONE',  ( 0.3996062992125985480, -0.1070741851644052972, -0.1883202099737532609 ) ) ;
#30171 = CARTESIAN_POINT ( 'NONE',  ( 0.3996062992125986035, 2.446882876249141962E-17, -0.5905511811023621549 ) ) ;
#30172 = CARTESIAN_POINT ( 'NONE',  ( 0.3949938075777409408, 0.1058382717557500574, 0.03280839895013118457 ) ) ;
#30173 = CARTESIAN_POINT ( 'NONE',  ( 1.646981627296588035, -0.2845877964562159024, 0.3641732283464567677 ) ) ;
#30174 = CARTESIAN_POINT ( 'NONE',  ( 0.8661417322834652488, -0.1870078740157480601, -0.3641732283464567677 ) ) ;
#30175 = CARTESIAN_POINT ( 'NONE',  ( 0.6036745406824153282, -0.6046776061558807314, 0.2411417322834647770 ) ) ;
#30176 = CARTESIAN_POINT ( 'NONE',  ( 1.541994750656168645, -0.6692913385826771977, 0.1292274648535927661 ) ) ;
#30177 = B_SPLINE_CURVE_WITH_KNOTS ( 'NONE', 3,
 ( #13161, #39227, #63654, #7249 ),
 .UNSPECIFIED., .F., .F.,
 ( 4, 4 ),
 ( 1.999999999910059834E-07, 0.006970199999999934261 ),
 .UNSPECIFIED. ) ;
#30178 = CARTESIAN_POINT ( 'NONE',  ( 0.2891555358219910499, 0.2891555358219910499, -1.001968503937007871 ) ) ;
#30179 = CARTESIAN_POINT ( 'NONE',  ( 0.7349081364829403995, 0.1283753931104748280, 0.1820866141732283561 ) ) ;
#30180 = CARTESIAN_POINT ( 'NONE',  ( -0.1443569553805765515, -0.4281496062992127816, -0.4176697321401328100 ) ) ;
#30181 = CARTESIAN_POINT ( 'NONE',  ( -0.9842519685039360366, 0.2952755905511811885, 0.000000000000000000 ) ) ;
#30182 = CARTESIAN_POINT ( 'NONE',  ( 1.437007874015748810, -0.5400638737290845981, -0.3530559997133363437 ) ) ;
#30183 = CARTESIAN_POINT ( 'NONE',  ( 5.785732909357575061E-17, -0.4724409448818898682, -1.181102362204724310 ) ) ;
#30184 = CARTESIAN_POINT ( 'NONE',  ( 0.2925321140481932369, -0.2925321140481931814, -2.303149606299212060 ) ) ;
#30185 = CARTESIAN_POINT ( 'NONE',  ( -0.1181102362204717315, 0.1771653543307087630, 0.000000000000000000 ) ) ;
#30186 = ORIENTED_EDGE ( 'NONE', *, *, #19084, .F. ) ;
#30187 = CARTESIAN_POINT ( 'NONE',  ( -0.3917322834645670659, -7.196005306013484475E-17, -0.8235101294301331309 ) ) ;
#30188 = ORIENTED_EDGE ( 'NONE', *, *, #79291, .F. ) ;
#30189 = CARTESIAN_POINT ( 'NONE',  ( -0.7545931758530177724, 0.2952755905511811885, 0.1292274648535926551 ) ) ;
#30190 = CARTESIAN_POINT ( 'NONE',  ( -0.01968503937007793844, 0.1660481256975883668, -0.3530559997133364547 ) ) ;
#30191 = CARTESIAN_POINT ( 'NONE',  ( -0.4330708661417315697, -0.6692913385826771977, 8.415575281601705876E-17 ) ) ;
#30192 = AXIS2_PLACEMENT_3D ( 'NONE', #50711, #38506, #70490 ) ;
#30193 = CARTESIAN_POINT ( 'NONE',  ( 0.5577427821522316087, -0.05778040916215522460, 0.4822834645669289988 ) ) ;
#30194 = CARTESIAN_POINT ( 'NONE',  ( -0.6299212598425188991, -0.1870078740157480879, -0.4822834645669291653 ) ) ;
#30195 = CARTESIAN_POINT ( 'NONE',  ( -1.443569553805773564, 0.2306618581243847221, -0.2411417322834647770 ) ) ;
#30196 = CARTESIAN_POINT ( 'NONE',  ( -0.6692913385826764205, -0.6692913385826771977, 8.415575281601705876E-17 ) ) ;
#30197 = CARTESIAN_POINT ( 'NONE',  ( 0.7349081364829402885, -0.6046776061558809534, -0.2411417322834644161 ) ) ;
#30198 = CARTESIAN_POINT ( 'NONE',  ( 0.3543307086614179147, 0.2952755905511811885, 0.000000000000000000 ) ) ;
#30199 = CARTESIAN_POINT ( 'NONE',  ( -0.3917322834645669549, -0.1049643490035306603, -1.140419947506561282 ) ) ;
#30200 = CARTESIAN_POINT ( 'NONE',  ( -0.3477690288713902178, 0.1771653543307087075, -0.09757992244046823083 ) ) ;
#30201 = ORIENTED_EDGE ( 'NONE', *, *, #7741, .F. ) ;
#30202 = CARTESIAN_POINT ( 'NONE',  ( -0.1058382717557503211, 0.3949938075777409408, -1.423884514435695969 ) ) ;
#30203 = EDGE_LOOP ( 'NONE', ( #3108, #76570, #40755, #13359 ) ) ;
#30204 = CARTESIAN_POINT ( 'NONE',  ( -1.148293963254592542, -0.5511811023622048555, -0.09757992244046775898 ) ) ;
#30205 = CARTESIAN_POINT ( 'NONE',  ( -0.4199475065616791736, -0.6046776061558807314, 0.2411417322834647770 ) ) ;
#30206 = CARTESIAN_POINT ( 'NONE',  ( 0.000000000000000000, 1.062992125984252745, 1.122047244094488194 ) ) ;
#30207 = CARTESIAN_POINT ( 'NONE',  ( -0.7152230971128602510, -0.05778040916215560624, -0.4822834645669293319 ) ) ;
#30208 = CARTESIAN_POINT ( 'NONE',  ( -0.7677165354330699465, 0.1660481256975885056, 0.3530559997133364547 ) ) ;
#30209 = CARTESIAN_POINT ( 'NONE',  ( -0.7137454485294948414, 2.793565526369265584, -0.4917280318828583519 ) ) ;
#30210 = CARTESIAN_POINT ( 'NONE',  ( 0.1181102362204724532, 0.09842519685039372024, 0.000000000000000000 ) ) ;
#30211 = AXIS2_PLACEMENT_3D ( 'NONE', #55779, #17514, #63343 ) ;
#30212 = CARTESIAN_POINT ( 'NONE',  ( 1.089238845144357759, -0.004921259842519870586, -0.3153832671262229437 ) ) ;
#30213 = CARTESIAN_POINT ( 'NONE',  ( 1.614173228346457378, 0.4410134679336836783, -0.1372047244094476148 ) ) ;
#30214 = CARTESIAN_POINT ( 'NONE',  ( 0.1049643490035303689, 0.3917322834645670104, -0.07808398950131241467 ) ) ;
#30215 = CARTESIAN_POINT ( 'NONE',  ( -0.09186351706036689768, -0.004921259842519870586, -0.3153832671262229437 ) ) ;
#30216 = CARTESIAN_POINT ( 'NONE',  ( -0.1968503937007867743, 0.2952755905511811885, 0.000000000000000000 ) ) ;
#30217 = CARTESIAN_POINT ( 'NONE',  ( 3.916359054710398357, 1.286266870969481779, 0.4027888758938074076 ) ) ;
#30218 = CARTESIAN_POINT ( 'NONE',  ( -0.2821522309711278487, -0.6692913385826773087, -0.1292274648535924053 ) ) ;
#30219 = VERTEX_POINT ( 'NONE', #12171 ) ;
#30220 = CARTESIAN_POINT ( 'NONE',  ( -0.1998031496062991907, -0.3460692066303959757, -1.955380577427821454 ) ) ;
#30221 = CARTESIAN_POINT ( 'NONE',  ( -2.118110236220467790, 0.000000000000000000, -0.4498537592783120598 ) ) ;
#30222 = ORIENTED_EDGE ( 'NONE', *, *, #73238, .T. ) ;
#30223 = CARTESIAN_POINT ( 'NONE',  ( 0.2925321140481932369, 0.2925321140481932369, -1.474409448818897683 ) ) ;
#30224 = CARTESIAN_POINT ( 'NONE',  ( 1.595398199321655275, 0.4619154201552251315, -0.1559797534342493852 ) ) ;
#30225 = CARTESIAN_POINT ( 'NONE',  ( -0.8661417322834640276, -0.1870078740157480601, -0.3641732283464567677 ) ) ;
#30226 = CARTESIAN_POINT ( 'NONE',  ( -0.8464566929133852113, -0.5400638737290845981, -0.3530559997133363437 ) ) ;
#30227 = CARTESIAN_POINT ( 'NONE',  ( 5.785732909357575061E-17, -0.4724409448818898682, -0.5511811023622047445 ) ) ;
#30228 = CARTESIAN_POINT ( 'NONE',  ( -2.795275590551181910, 1.889763779527559251, -6.635626899597537341E-17 ) ) ;
#30229 =( BOUNDED_CURVE ( )  B_SPLINE_CURVE ( 3, ( #37276, #51116, #4872, #62951 ),
 .UNSPECIFIED., .F., .F. ) 
 B_SPLINE_CURVE_WITH_KNOTS ( ( 4, 4 ),
 ( 4.773032204416207236, 4.776949949702167686 ),
 .UNSPECIFIED. ) 
 CURVE ( )  GEOMETRIC_REPRESENTATION_ITEM ( )  RATIONAL_B_SPLINE_CURVE ( ( 1.000000000000000000, 0.9999987209397318555, 0.9999987209397318555, 1.000000000000000000 ) ) 
 REPRESENTATION_ITEM ( '' )  );
#30230 = CARTESIAN_POINT ( 'NONE',  ( -9.594673741351313045E-17, 0.3917322834645670104, -2.761811023622046779 ) ) ;
#30231 = CARTESIAN_POINT ( 'NONE',  ( 1.489501312335958172, -0.3162353388693405765, 0.4822834645669290543 ) ) ;
#30232 = CARTESIAN_POINT ( 'NONE',  ( 0.6102362204724416372, -0.5400638737290844871, 0.3530559997133364547 ) ) ;
#30233 = CARTESIAN_POINT ( 'NONE',  ( 0.4724409448818904789, -0.1870078740157480879, -0.4822834645669291653 ) ) ;
#30234 = CARTESIAN_POINT ( 'NONE',  ( -0.7414698162729651543, -0.5511811023622046335, 0.09757992244046803654 ) ) ;
#30235 = CARTESIAN_POINT ( 'NONE',  ( -0.4658792650918627265, -0.05778040916215522460, 0.4822834645669289988 ) ) ;
#30236 = CARTESIAN_POINT ( 'NONE',  ( 0.4091458600556404646, -0.2362204724409448231, -2.229002624671915900 ) ) ;
#30237 = CARTESIAN_POINT ( 'NONE',  ( -1.017060367454067249, -0.3162353388693409650, -0.4822834645669289433 ) ) ;
#30238 = EDGE_CURVE ( 'NONE', #73035, #80330, #5837, .T. ) ;
#30239 = CARTESIAN_POINT ( 'NONE',  ( 0.1974969037888706092, -0.3420746716998660508, -2.058398950131233640 ) ) ;
#30240 = CARTESIAN_POINT ( 'NONE',  ( 1.148293963254593653, 0.1771653543307087075, -0.09757992244046823083 ) ) ;
#30241 = CARTESIAN_POINT ( 'NONE',  ( -0.4790026246719154557, -0.2845877964562159024, 0.3641732283464567677 ) ) ;
#30242 = CARTESIAN_POINT ( 'NONE',  ( 1.220472440944882608, 0.1771653543307087630, 0.000000000000000000 ) ) ;
#30243 = CARTESIAN_POINT ( 'NONE',  ( -1.692913385826770645, 0.2952755905511811885, 0.000000000000000000 ) ) ;
#30244 = CARTESIAN_POINT ( 'NONE',  ( -1.056430446194224881, -0.5511811023622046335, 0.09757992244046803654 ) ) ;
#30245 = DIRECTION ( 'NONE',  ( 1.000000000000000000, 1.601283208593975810E-15, 0.000000000000000000 ) ) ;
#30246 = CARTESIAN_POINT ( 'NONE',  ( 0.3346456692913393205, -0.4536011799217368745, -0.2665933059059886201 ) ) ;
#30247 = CARTESIAN_POINT ( 'NONE',  ( -0.3149606299212590610, -0.1870078740157480879, -0.4822834645669291653 ) ) ;
#30248 = CARTESIAN_POINT ( 'NONE',  ( 0.3018372703412079971, 0.05413385826771626580, -0.4176697321401330321 ) ) ;
#30249 = CARTESIAN_POINT ( 'NONE',  ( -0.06561679790026180015, -0.004921259842519576551, 0.3153832671262227771 ) ) ;
#30250 = CARTESIAN_POINT ( 'NONE',  ( -1.725721784776902190, -0.08942795157527998196, 0.3641732283464567121 ) ) ;
#30251 = CARTESIAN_POINT ( 'NONE',  ( 0.8005249343832028242, -0.4281496062992127816, -0.4176697321401328100 ) ) ;
#30252 = CYLINDRICAL_SURFACE ( 'NONE', #31741, 0.3937007874015748254 ) ;
#30253 = CARTESIAN_POINT ( 'NONE',  ( 1.338582677165355062, -0.1870078740157480601, -0.3641732283464567677 ) ) ;
#30254 = CARTESIAN_POINT ( 'NONE',  ( -0.9186351706036736120, 0.2306618581243848609, 0.2411417322834645549 ) ) ;
#30255 = CARTESIAN_POINT ( 'NONE',  ( -0.2624671916010490880, -0.5023911411419708095, 0.1820866141732285504 ) ) ;
#30256 = DIRECTION ( 'NONE',  ( -3.491481338843132961E-15, -0.000000000000000000, 1.000000000000000000 ) ) ;
#30257 = CARTESIAN_POINT ( 'NONE',  ( 0.4002624671916016896, -0.2845877964562161244, -0.3641732283464567121 ) ) ;
#30258 = CARTESIAN_POINT ( 'NONE',  ( 0.04593175853018440641, -0.6692913385826771977, 0.1292274648535927661 ) ) ;
#30259 = CARTESIAN_POINT ( 'NONE',  ( -0.3996062992125985480, -7.340648628747423112E-17, -0.9035433070866141225 ) ) ;
#30260 = CARTESIAN_POINT ( 'NONE',  ( -0.2867679344610364334, -0.2867679344610367109, -2.190944881889763440 ) ) ;
#30261 = CARTESIAN_POINT ( 'NONE',  ( 0.6496062992125991586, 0.07958543189024085140, 0.2665933059059887866 ) ) ;
#30262 = CARTESIAN_POINT ( 'NONE',  ( -0.2559055118110227234, -0.5400638737290844871, 0.3530559997133364547 ) ) ;
#30263 = CARTESIAN_POINT ( 'NONE',  ( -0.8070866141732276899, 0.1660481256975883668, -0.3530559997133364547 ) ) ;
#30264 = CARTESIAN_POINT ( 'NONE',  ( -0.8595800524934373854, -0.08942795157527998196, 0.3641732283464567121 ) ) ;
#30265 = DIRECTION ( 'NONE',  ( -0.000000000000000000, 1.000000000000000000, -1.408710688920637755E-15 ) ) ;
#30266 = CARTESIAN_POINT ( 'NONE',  ( -0.7020997375328074108, -0.08942795157527998196, 0.3641732283464567121 ) ) ;
#30267 = CARTESIAN_POINT ( 'NONE',  ( -0.006561679790025524116, -0.05778040916215560624, -0.4822834645669293319 ) ) ;
#30268 = CARTESIAN_POINT ( 'NONE',  ( -1.128608923884513837, -0.5023911411419708095, 0.1820866141732285504 ) ) ;
#30269 = AXIS2_PLACEMENT_3D ( 'NONE', #68418, #17496, #29687 ) ;
#30270 = CARTESIAN_POINT ( 'NONE',  ( -1.410761154855641575, -0.3162353388693409650, -0.4822834645669289433 ) ) ;
#30271 = CARTESIAN_POINT ( 'NONE',  ( 0.4724409448818914781, 0.1265901696524960318, -2.171916010498687655 ) ) ;
#30272 = VERTEX_POINT ( 'NONE', #26024 ) ;
#30273 = CARTESIAN_POINT ( 'NONE',  ( -1.325459317585300889, -0.3690944881889765550, -0.3153832671262227771 ) ) ;
#30274 = CARTESIAN_POINT ( 'NONE',  ( -1.095800524934382292, -0.05778040916215522460, 0.4822834645669289988 ) ) ;
#30275 = CARTESIAN_POINT ( 'NONE',  ( -0.4265091863517051496, 0.2952755905511810774, -0.1292274648535930714 ) ) ;
#30276 = CARTESIAN_POINT ( 'NONE',  ( -1.082677165354329896, -0.5400638737290845981, -0.3530559997133363437 ) ) ;
#30277 = CARTESIAN_POINT ( 'NONE',  ( 0.2867679344610365999, -0.2867679344610365444, -1.600393700787401619 ) ) ;
#30278 = DIRECTION ( 'NONE',  ( 0.000000000000000000, 0.000000000000000000, -1.000000000000000000 ) ) ;
#30279 = CARTESIAN_POINT ( 'NONE',  ( 0.8136482939632553313, -0.6046776061558809534, -0.2411417322834644161 ) ) ;
#30280 = CARTESIAN_POINT ( 'NONE',  ( 0.4199475065616805614, 0.2306618581243848609, 0.2411417322834645549 ) ) ;
#30281 = DIRECTION ( 'NONE',  ( -0.000000000000000000, -1.000000000000000000, -0.000000000000000000 ) ) ;
#30282 = CARTESIAN_POINT ( 'NONE',  ( 0.3996062992125984925, 0.1070741851644054499, -2.406167979002624246 ) ) ;
#30283 = CARTESIAN_POINT ( 'NONE',  ( 1.227034120734908917, -0.5511811023622046335, 0.09757992244046803654 ) ) ;
#30284 = CARTESIAN_POINT ( 'NONE',  ( 0.2925321140481932369, -0.2925321140481932369, -0.7283464566929134243 ) ) ;
#30285 = EDGE_LOOP ( 'NONE', ( #24106, #48011, #67603, #82055 ) ) ;
#30286 = CARTESIAN_POINT ( 'NONE',  ( -0.8989501312335946848, -0.5511811023622046335, 0.09757992244046803654 ) ) ;
#30287 = CARTESIAN_POINT ( 'NONE',  ( -0.1049643490035307020, 0.3917322834645669549, -2.675853018372703396 ) ) ;
#30288 = ORIENTED_EDGE ( 'NONE', *, *, #68572, .T. ) ;
#30289 = CARTESIAN_POINT ( 'NONE',  ( 0.3215223097112867578, -0.05778040916215522460, 0.4822834645669289988 ) ) ;
#30290 = CARTESIAN_POINT ( 'NONE',  ( -0.3477690288713905509, -0.6692913385826771977, 0.1292274648535927661 ) ) ;
#30291 = CARTESIAN_POINT ( 'NONE',  ( -0.9908136482939626788, 0.2952755905511811885, 0.1292274648535926551 ) ) ;
#30292 = CARTESIAN_POINT ( 'NONE',  ( 1.141732283464567788, -0.6692913385826771977, 8.415575281601705876E-17 ) ) ;
#30293 = CARTESIAN_POINT ( 'NONE',  ( -1.128608923884513837, 0.1283753931104746893, -0.1820866141732285504 ) ) ;
#30294 = CYLINDRICAL_SURFACE ( 'NONE', #17173, 0.1771653543307085410 ) ;
#30295 = CARTESIAN_POINT ( 'NONE',  ( 0.1181102362204730916, 0.2952755905511811885, 0.000000000000000000 ) ) ;
#30296 = CARTESIAN_POINT ( 'NONE',  ( -1.272965879265091305, 0.05413385826771626580, -0.4176697321401330321 ) ) ;
#30297 = CARTESIAN_POINT ( 'NONE',  ( -0.1958661417322836440, 0.3392501089628016664, -1.982920316764092306 ) ) ;
#30298 = CARTESIAN_POINT ( 'NONE',  ( -1.476377952755905110, 0.1660481256975885056, 0.3530559997133364547 ) ) ;
#30299 = DIRECTION ( 'NONE',  ( 8.673617379884022653E-16, -1.000000000000000000, 3.028377322213053966E-30 ) ) ;
#30300 = CARTESIAN_POINT ( 'NONE',  ( 0.2867679344610365999, 0.2867679344610365999, 0.02755905511811028441 ) ) ;
#30301 = CARTESIAN_POINT ( 'NONE',  ( 0.7742782152230979209, -0.004921259842519870586, -0.3153832671262229437 ) ) ;
#30302 = ORIENTED_EDGE ( 'NONE', *, *, #60079, .T. ) ;
#30303 = CARTESIAN_POINT ( 'NONE',  ( -0.1974969037888706647, 0.3420746716998658843, -0.3280839895013124563 ) ) ;
#30304 = CARTESIAN_POINT ( 'NONE',  ( -1.036745406824146176, -0.4281496062992124485, 0.4176697321401328655 ) ) ;
#30305 = ORIENTED_EDGE ( 'NONE', *, *, #22777, .F. ) ;
#30306 = CARTESIAN_POINT ( 'NONE',  ( 0.03280839895013198948, 0.1771653543307087630, 0.09757992244046791164 ) ) ;
#30307 = CARTESIAN_POINT ( 'NONE',  ( -1.437007874015747477, -0.5400638737290844871, 0.3530559997133364547 ) ) ;
#30308 = CARTESIAN_POINT ( 'NONE',  ( 0.3608923884514443348, 0.2952755905511810774, -0.1292274648535930714 ) ) ;
#30309 = CARTESIAN_POINT ( 'NONE',  ( 0.3674540682414705883, 0.2306618581243847221, -0.2411417322834647770 ) ) ;
#30310 = CARTESIAN_POINT ( 'NONE',  ( -0.7217847769028863381, 0.05413385826771626580, -0.4176697321401330321 ) ) ;
#30311 = CARTESIAN_POINT ( 'NONE',  ( 0.3917322834645670659, 2.398668435337828261E-17, -1.059730601871078148 ) ) ;
#30312 = CARTESIAN_POINT ( 'NONE',  ( -0.7611548556430438595, -0.6046776061558809534, -0.2411417322834644161 ) ) ;
#30313 = CARTESIAN_POINT ( 'NONE',  ( -0.3917322834645669549, -0.1049643490035306603, -2.807742782152229832 ) ) ;
#30314 = CARTESIAN_POINT ( 'NONE',  ( 1.292650918635171564, 0.1771653543307087630, 0.09757992244046791164 ) ) ;
#30315 = CARTESIAN_POINT ( 'NONE',  ( -0.9251968503937002541, -0.5400638737290845981, -0.3530559997133363437 ) ) ;
#30316 = CARTESIAN_POINT ( 'NONE',  ( 0.9514435695538062676, -0.3162353388693409650, -0.4822834645669289433 ) ) ;
#30317 = CARTESIAN_POINT ( 'NONE',  ( 1.286089238845145033, -0.6046776061558809534, -0.2411417322834644161 ) ) ;
#30318 = CARTESIAN_POINT ( 'NONE',  ( 0.2925321140481932369, 0.2925321140481932369, -0.7677165354330709457 ) ) ;
#30319 = CARTESIAN_POINT ( 'NONE',  ( -1.509186351706035767, 0.05413385826771626580, -0.4176697321401330321 ) ) ;
#30320 = CARTESIAN_POINT ( 'NONE',  ( 0.1070741851644054776, -0.3996062992125984925, -0.1620734908136483021 ) ) ;
#30321 = CARTESIAN_POINT ( 'NONE',  ( 0.2690288713910767848, -0.6692913385826773087, -0.1292274648535924053 ) ) ;
#30322 = CARTESIAN_POINT ( 'NONE',  ( -0.3996062992125986035, -7.340648628747425578E-17, -2.244094488188976388 ) ) ;
#30323 = EDGE_CURVE ( 'NONE', #15098, #11783, #25647, .T. ) ;
#30324 = AXIS2_PLACEMENT_3D ( 'NONE', #34793, #34372, #41513 ) ;
#30325 = CARTESIAN_POINT ( 'NONE',  ( -1.391076115485563314, -0.5023911411419708095, -0.1820866141732282451 ) ) ;
#30326 = CARTESIAN_POINT ( 'NONE',  ( 0.4396325459317593221, 0.1771653543307087075, -0.09757992244046823083 ) ) ;
#30327 = CARTESIAN_POINT ( 'NONE',  ( 0.8661417322834652488, -0.1870078740157480879, -0.4822834645669291653 ) ) ;
#30328 = CARTESIAN_POINT ( 'NONE',  ( -0.4091458600556402980, -0.2362204724409451284, -1.074146981627296604 ) ) ;
#30329 = CARTESIAN_POINT ( 'NONE',  ( 0.8464566929133866546, -0.4536011799217367080, 0.2665933059059888421 ) ) ;
#30330 = CARTESIAN_POINT ( 'NONE',  ( 0.2690288713910767848, -0.6692913385826773087, -0.1292274648535924053 ) ) ;
#30331 = ADVANCED_FACE ( 'NONE', ( #38238, #37422, #63095 ), #6251, .F. ) ;
#30332 = CARTESIAN_POINT ( 'NONE',  ( 4.837279021331061486E-17, -0.3949938075777409963, -0.7854330708661416693 ) ) ;
#30333 = CARTESIAN_POINT ( 'NONE',  ( -0.9055118110236215490, 0.2952755905511811885, 0.000000000000000000 ) ) ;
#30334 = LINE ( 'NONE', #24429, #2863 ) ;
#30335 = CARTESIAN_POINT ( 'NONE',  ( 0.8595800524934390507, -0.08942795157528024563, -0.3641732283464568787 ) ) ;
#30336 = CARTESIAN_POINT ( 'NONE',  ( 0.1115485564304467270, -0.6692913385826773087, -0.1292274648535924053 ) ) ;
#30337 = CARTESIAN_POINT ( 'NONE',  ( 0.4486317206264793800, 1.694949792723955850, -1.028546380722449527 ) ) ;
#30338 = CARTESIAN_POINT ( 'NONE',  ( -0.3937007874015740483, -0.1870078740157480879, -0.4822834645669291653 ) ) ;
#30339 = CARTESIAN_POINT ( 'NONE',  ( 0.07217847769028949700, -0.2845877964562159024, 0.3641732283464567677 ) ) ;
#30340 = CARTESIAN_POINT ( 'NONE',  ( -2.829146054566457291, 1.111778211650234605, 0.2101609992702869745 ) ) ;
#30341 = CARTESIAN_POINT ( 'NONE',  ( 0.08530183727034192087, -0.08942795157527998196, 0.3641732283464567121 ) ) ;
#30342 = CARTESIAN_POINT ( 'NONE',  ( 0.7217847769028878924, -0.3690944881889765550, -0.3153832671262227771 ) ) ;
#30343 = CARTESIAN_POINT ( 'NONE',  ( -0.1109781590376841404, 1.076155248315993074, -1.526021004911278567 ) ) ;
#30344 = CARTESIAN_POINT ( 'NONE',  ( 0.3996062992125986035, -0.1070741851644052972, -1.763123359580052174 ) ) ;
#30345 = CARTESIAN_POINT ( 'NONE',  ( 0.3215223097112867578, -0.3162353388693409650, -0.4822834645669289433 ) ) ;
#30346 = CARTESIAN_POINT ( 'NONE',  ( -0.3392501089628017219, -0.1958661417322836718, -1.461942257217847763 ) ) ;
#30347 = CARTESIAN_POINT ( 'NONE',  ( 1.305774278215223960, -0.5511811023622046335, 0.09757992244046803654 ) ) ;
#30348 = CARTESIAN_POINT ( 'NONE',  ( 0.1674892343164159914, -2.191421614605370878E-15, 0.4445507791589071167 ) ) ;
#30349 = CARTESIAN_POINT ( 'NONE',  ( -0.4593175853018366950, -0.004921259842519576551, 0.3153832671262227771 ) ) ;
#30350 = CARTESIAN_POINT ( 'NONE',  ( -0.2624671916010490880, 0.1283753931104746893, -0.1820866141732285504 ) ) ;
#30351 = CARTESIAN_POINT ( 'NONE',  ( -0.2887139107611542133, -0.6046776061558809534, -0.2411417322834644161 ) ) ;
#30352 = CARTESIAN_POINT ( 'NONE',  ( 0.8136482939632553313, -0.5023911411419708095, -0.1820866141732282451 ) ) ;
#30353 = CARTESIAN_POINT ( 'NONE',  ( 0.4582086034426817722, 1.413485598871839555, -1.024236350951628571 ) ) ;
#30354 = CARTESIAN_POINT ( 'NONE',  ( 1.292650918635171564, 0.1771653543307087630, 0.09757992244046791164 ) ) ;
#30355 = CARTESIAN_POINT ( 'NONE',  ( 0.006561679790026889343, -0.3162353388693409650, -0.4822834645669289433 ) ) ;
#30356 = CARTESIAN_POINT ( 'NONE',  ( 1.115485564304462551, -0.4281496062992127816, -0.4176697321401328100 ) ) ;
#30357 = CARTESIAN_POINT ( 'NONE',  ( -0.03443470937339728616, 0.2755905511811023723, -1.537015892239756099 ) ) ;
#30358 = CARTESIAN_POINT ( 'NONE',  ( 0.2690288713910767848, -0.6692913385826773087, -0.1292274648535924053 ) ) ;
#30359 = CARTESIAN_POINT ( 'NONE',  ( 0.3392501089628018329, 0.1958661417322835607, -0.8458005249343831800 ) ) ;
#30361 = CARTESIAN_POINT ( 'NONE',  ( 1.364829396325460076, 0.2306618581243848609, 0.2411417322834645549 ) ) ;
#30360 = CIRCLE ( 'NONE', #70681, 0.01968503937007875723 ) ;
#30362 = AXIS2_PLACEMENT_3D ( 'NONE', #37592, #11527, #37184 ) ;
#30363 = CARTESIAN_POINT ( 'NONE',  ( 0.6627296587926517768, -0.6692913385826773087, -0.1292274648535924053 ) ) ;
#30364 = CARTESIAN_POINT ( 'NONE',  ( 0.000000000000000000, 2.716535433070866645, 0.000000000000000000 ) ) ;
#30365 = CARTESIAN_POINT ( 'NONE',  ( 0.8661417322834653598, -0.1870078740157479769, 0.3641732283464567677 ) ) ;
#30366 = CARTESIAN_POINT ( 'NONE',  ( 1.148293963254593875, -0.6692913385826771977, 0.1292274648535927661 ) ) ;
#30367 = CARTESIAN_POINT ( 'NONE',  ( -0.01968503937007793844, -0.4536011799217367080, 0.2665933059059888421 ) ) ;
#30368 = CARTESIAN_POINT ( 'NONE',  ( -0.3477690288713902178, 0.2952755905511810774, -0.1292274648535930714 ) ) ;
#30369 = CARTESIAN_POINT ( 'NONE',  ( 0.2099737532808405305, 0.2306618581243847221, -0.2411417322834647770 ) ) ;
#30370 = CARTESIAN_POINT ( 'NONE',  ( -0.6889763779527552368, 0.1660481256975885056, 0.3530559997133364547 ) ) ;
#30371 = CARTESIAN_POINT ( 'NONE',  ( -0.1771653543307080136, -0.4536011799217367080, 0.2665933059059888421 ) ) ;
#30372 = CARTESIAN_POINT ( 'NONE',  ( 0.7545931758530188826, -0.6692913385826771977, 0.1292274648535927661 ) ) ;
#30373 = CARTESIAN_POINT ( 'NONE',  ( 0.9317585301837276734, -0.004921259842519870586, -0.3153832671262229437 ) ) ;
#30374 = CARTESIAN_POINT ( 'NONE',  ( 0.1902887139107617975, -0.6692913385826773087, -0.1292274648535924053 ) ) ;
#30375 = CARTESIAN_POINT ( 'NONE',  ( 0.3149606299212479033, -5.463695987328517809E-17, 1.076935383196061080 ) ) ;
#30377 = CARTESIAN_POINT ( 'NONE',  ( 0.3996062992125986035, 2.446882876249141962E-17, -1.220472440944881942 ) ) ;
#30376 = DIRECTION ( 'NONE',  ( 0.000000000000000000, 1.000000000000000000, 0.000000000000000000 ) ) ;
#30378 = CARTESIAN_POINT ( 'NONE',  ( 1.220472440944879722, 0.4405861044731111953, 0.5309055118110233007 ) ) ;
#30379 = CARTESIAN_POINT ( 'NONE',  ( 0.3392501089628018884, -0.1958661417322834220, -1.986876640419947604 ) ) ;
#30381 = AXIS2_PLACEMENT_3D ( 'NONE', #53607, #72571, #1456 ) ;
#30380 = CARTESIAN_POINT ( 'NONE',  ( -1.207349081364828436, -0.6046776061558807314, 0.2411417322834647770 ) ) ;
#30382 = CARTESIAN_POINT ( 'NONE',  ( -0.4724409448818890911, -0.1870078740157479769, 0.4822834645669291653 ) ) ;
#30383 = CARTESIAN_POINT ( 'NONE',  ( 0.2362204724409451007, -0.4091458600556402980, -0.4068241469816273326 ) ) ;
#30384 = CARTESIAN_POINT ( 'NONE',  ( 4.837279021331060870E-17, -0.3949938075777409963, -2.913385826771653253 ) ) ;
#30385 = ORIENTED_EDGE ( 'NONE', *, *, #55825, .T. ) ;
#30386 = CARTESIAN_POINT ( 'NONE',  ( 0.1509186351706045259, -0.08942795157528024563, -0.3641732283464568787 ) ) ;
#30387 = CARTESIAN_POINT ( 'NONE',  ( -0.1958661417322836718, 0.3392501089628017219, -1.265091863517060489 ) ) ;
#30388 = CARTESIAN_POINT ( 'NONE',  ( 0.6036745406824153282, -0.6046776061558807314, 0.2411417322834647770 ) ) ;
#30389 = CARTESIAN_POINT ( 'NONE',  ( 0.3458507752293908943, 0.3458507752293908943, -2.657480314960630530 ) ) ;
#30390 = CARTESIAN_POINT ( 'NONE',  ( 2.118110236220470899, 0.000000000000000000, 0.4498537592782972383 ) ) ;
#30391 = CARTESIAN_POINT ( 'NONE',  ( 0.5314960629921371416, 2.755905511811024056, -3.184294706754629001 ) ) ;
#30392 = CARTESIAN_POINT ( 'NONE',  ( 1.122047244094488860, -0.5400638737290845981, -0.3530559997133363437 ) ) ;
#30393 = CARTESIAN_POINT ( 'NONE',  ( 1.325459317585302665, -0.004921259842519870586, -0.3153832671262229437 ) ) ;
#30394 = CARTESIAN_POINT ( 'NONE',  ( 0.1509186351706045259, -0.05778040916215560624, -0.4822834645669293319 ) ) ;
#30395 = CARTESIAN_POINT ( 'NONE',  ( -0.2867679344610364334, -0.2867679344610368219, -0.6115292406486071419 ) ) ;
#30396 = CARTESIAN_POINT ( 'NONE',  ( -0.2099737532808391705, 0.2306618581243848609, 0.2411417322834645549 ) ) ;
#30398 = CARTESIAN_POINT ( 'NONE',  ( -1.115485564304461219, -0.3690944881889763329, 0.3153832671262228327 ) ) ;
#30397 =( BOUNDED_CURVE ( )  B_SPLINE_CURVE ( 3, ( #41651, #66932, #53853, #55095 ),
 .UNSPECIFIED., .F., .F. ) 
 B_SPLINE_CURVE_WITH_KNOTS ( ( 4, 4 ),
 ( 3.539787554096436306, 4.423914789137159964 ),
 .UNSPECIFIED. ) 
 CURVE ( )  GEOMETRIC_REPRESENTATION_ITEM ( )  RATIONAL_B_SPLINE_CURVE ( ( 1.000000000000000000, 0.9359138408343250504, 0.9359138408343250504, 1.000000000000000000 ) ) 
 REPRESENTATION_ITEM ( '' )  );
#30399 = CARTESIAN_POINT ( 'NONE',  ( 0.5446194225721792126, -0.05778040916215560624, -0.4822834645669293319 ) ) ;
#30400 = CARTESIAN_POINT ( 'NONE',  ( -0.6758530183727028406, -0.6692913385826773087, -0.1292274648535924053 ) ) ;
#30401 = CARTESIAN_POINT ( 'NONE',  ( 1.633858267716535639, -0.5400638737290844871, 0.3530559997133364547 ) ) ;
#30402 = DIRECTION ( 'NONE',  ( 1.224646799147349509E-16, 0.000000000000000000, -1.000000000000000000 ) ) ;
#30403 = ORIENTED_EDGE ( 'NONE', *, *, #17120, .T. ) ;
#30404 = CARTESIAN_POINT ( 'NONE',  ( 0.2867679344610366554, -0.2867679344610365999, -2.142407767225408932 ) ) ;
#30405 = CARTESIAN_POINT ( 'NONE',  ( 0.2230971128608932319, -0.4281496062992124485, 0.4176697321401328655 ) ) ;
#30406 = CARTESIAN_POINT ( 'NONE',  ( -0.4921259842519677963, -0.5400638737290844871, 0.3530559997133364547 ) ) ;
#30407 = CARTESIAN_POINT ( 'NONE',  ( -1.509186351706035767, -0.4281496062992124485, 0.4176697321401328655 ) ) ;
#30408 = B_SPLINE_CURVE_WITH_KNOTS ( 'NONE', 3,
 ( #45801, #64761, #377, #58437, #33611, #78241, #7100, #26460, #52113, #77821, #20151, #71498, #27289, #1630, #39504, #20573, #65192, #7528, #33198, #14270, #58866, #1224, #26873, #71920, #46224 ),
 .UNSPECIFIED., .F., .F.,
 ( 4, 2, 2, 1, 2, 2, 2, 2, 2, 2, 2, 2, 4 ),
 ( 0.03770804087963031126, 0.04006530914106495866, 0.04124394327178228237, 0.04242257740249960607, 0.04360121153321692977, 0.04477984566393425347, 0.04713711392536890782, 0.04831574805608623846, 0.04949438218680355522, 0.05185165044823820957, 0.05303028457895553327, 0.05420891870967285697, 0.05656618697110752519 ),
 .UNSPECIFIED. ) ;
#30409 = CARTESIAN_POINT ( 'NONE',  ( 0.5118110236220478892, 0.2952755905511811885, 0.000000000000000000 ) ) ;
#30410 = CARTESIAN_POINT ( 'NONE',  ( 0.5839895013123367340, 0.2952755905511811885, 0.1292274648535926551 ) ) ;
#30411 = CARTESIAN_POINT ( 'NONE',  ( 0.3392501089628018884, -0.1958661417322834220, -1.449475065616798064 ) ) ;
#30412 = CARTESIAN_POINT ( 'NONE',  ( -0.5971128608923877978, 0.2952755905511811885, 0.1292274648535926551 ) ) ;
#30413 = CARTESIAN_POINT ( 'NONE',  ( 0.02624671916010564918, -0.6046776061558809534, -0.2411417322834644161 ) ) ;
#30414 = CARTESIAN_POINT ( 'NONE',  ( -0.2427821522309703550, -0.3162353388693405765, 0.4822834645669290543 ) ) ;
#30415 = CARTESIAN_POINT ( 'NONE',  ( 0.1181102362204730916, 0.1771653543307087630, 0.000000000000000000 ) ) ;
#30416 = CARTESIAN_POINT ( 'NONE',  ( -1.673228346456691717, 0.1660481256975883668, -0.3530559997133364547 ) ) ;
#30417 = CARTESIAN_POINT ( 'NONE',  ( -0.01707598052245469858, 1.062992125984253411, -2.874015748031497175 ) ) ;
#30418 = CARTESIAN_POINT ( 'NONE',  ( 0.3346456692913390985, 0.1660481256975885056, 0.3530559997133364547 ) ) ;
#30419 = DIRECTION ( 'NONE',  ( 0.000000000000000000, 0.000000000000000000, -1.000000000000000000 ) ) ;
#30420 = CARTESIAN_POINT ( 'NONE',  ( -1.614173228346455824, 0.2952755905511811885, 0.000000000000000000 ) ) ;
#30421 = CARTESIAN_POINT ( 'NONE',  ( 4.797336870675656522E-17, -0.3917322834645670104, -2.590551181102362044 ) ) ;
#30422 = ORIENTED_EDGE ( 'NONE', *, *, #14203, .F. ) ;
#30423 = ORIENTED_EDGE ( 'NONE', *, *, #32224, .F. ) ;
#30424 = CONICAL_SURFACE ( 'NONE', #77475, 0.09842519685039351207, 1.029744258676652091 ) ;
#30425 = CARTESIAN_POINT ( 'NONE',  ( 0.7349081364829403995, 0.2306618581243848609, 0.2411417322834645549 ) ) ;
#30426 = CARTESIAN_POINT ( 'NONE',  ( 0.1640419947506569498, -0.08942795157527998196, 0.3641732283464567121 ) ) ;
#30427 = AXIS2_PLACEMENT_3D ( 'NONE', #74947, #68615, #67386 ) ;
#30428 = VECTOR ( 'NONE', #72239, 39.37007874015748854 ) ;
#30430 = LINE ( 'NONE', #35510, #49190 ) ;
#30429 = CARTESIAN_POINT ( 'NONE',  ( 1.374111566022513293E-16, 1.062992125984252745, -1.122047244094488194 ) ) ;
#30431 = CARTESIAN_POINT ( 'NONE',  ( -9.594673741351313045E-17, 0.3917322834645670104, -0.7145669291338584417 ) ) ;
#30432 = CARTESIAN_POINT ( 'NONE',  ( -0.2362204724409447953, -0.4091458600556404646, 0.1725721784776902690 ) ) ;
#30433 = CARTESIAN_POINT ( 'NONE',  ( 0.7193605937323486188, 1.521610601467410833E-15, 0.4118484887281966822 ) ) ;
#30434 = CARTESIAN_POINT ( 'NONE',  ( -0.3460692066303960313, 0.1998031496062989965, -2.307742782152230721 ) ) ;
#30435 = CARTESIAN_POINT ( 'NONE',  ( 0.6233595800524939223, -0.3162353388693405765, 0.4822834645669290543 ) ) ;
#30436 = CARTESIAN_POINT ( 'NONE',  ( -1.187664041994749731, -0.3162353388693405765, 0.4822834645669290543 ) ) ;
#30437 = CARTESIAN_POINT ( 'NONE',  ( -1.200787401574802349, 0.1660481256975883668, -0.3530559997133364547 ) ) ;
#30438 = CARTESIAN_POINT ( 'NONE',  ( 0.8595800524934390507, -0.05778040916215560624, -0.4822834645669293319 ) ) ;
#30439 = CARTESIAN_POINT ( 'NONE',  ( 1.272965879265092637, 0.05413385826771666132, 0.4176697321401328100 ) ) ;
#30440 = CARTESIAN_POINT ( 'NONE',  ( 1.581364829396326277, -0.2845877964562161244, -0.3641732283464567121 ) ) ;
#30441 = CARTESIAN_POINT ( 'NONE',  ( 1.423884514435696413, -0.2845877964562161244, -0.3641732283464567121 ) ) ;
#30442 = CARTESIAN_POINT ( 'NONE',  ( -0.7480314960629914633, -0.6692913385826771977, 8.415575281601705876E-17 ) ) ;
#30443 = CARTESIAN_POINT ( 'NONE',  ( -0.3460692066303957537, -0.1998031496062994405, -0.6017060367454067915 ) ) ;
#30444 = CARTESIAN_POINT ( 'NONE',  ( 1.397637795275591177, 0.1660481256975883668, -0.3530559997133364547 ) ) ;
#30445 = CARTESIAN_POINT ( 'NONE',  ( -0.3917322834645669549, -0.1049643490035306603, -0.03805774278215218187 ) ) ;
#30446 = CARTESIAN_POINT ( 'NONE',  ( -0.03937007874015669567, 0.2952755905511811885, 0.000000000000000000 ) ) ;
#30447 = CIRCLE ( 'NONE', #55973, 0.5118110236220472231 ) ;
#30449 = CARTESIAN_POINT ( 'NONE',  ( -1.603475055217291612, 1.543447618314657932, -0.04573490813648263542 ) ) ;
#30448 = CARTESIAN_POINT ( 'NONE',  ( 1.279527559055118724, -0.5400638737290845981, -0.3530559997133363437 ) ) ;
#30450 = CARTESIAN_POINT ( 'NONE',  ( -0.9908136482939626788, -0.5511811023622048555, -0.09757992244046775898 ) ) ;
#30451 = CARTESIAN_POINT ( 'NONE',  ( 0.5249343832021005074, -0.6046776061558807314, 0.2411417322834647770 ) ) ;
#30452 = CARTESIAN_POINT ( 'NONE',  ( 0.8727034120734912248, -0.2845877964562161244, -0.3641732283464567121 ) ) ;
#30453 = CARTESIAN_POINT ( 'NONE',  ( -9.594673741351310580E-17, 0.3917322834645669549, -1.497356012302150763 ) ) ;
#30454 = CARTESIAN_POINT ( 'NONE',  ( -1.049868766404198794, 0.1283753931104746893, -0.1820866141732285504 ) ) ;
#30455 = CARTESIAN_POINT ( 'NONE',  ( 0.9186351706036752773, 0.2306618581243847221, -0.2411417322834647770 ) ) ;
#30456 = CARTESIAN_POINT ( 'NONE',  ( -0.4986876640419939388, 0.2306618581243847221, -0.2411417322834647770 ) ) ;
#30457 = CARTESIAN_POINT ( 'NONE',  ( -0.5183727034120726440, -0.5511811023622048555, -0.09757992244046775898 ) ) ;
#30458 = CARTESIAN_POINT ( 'NONE',  ( -0.4330708661417315697, 0.2952755905511811885, 0.000000000000000000 ) ) ;
#30459 = CARTESIAN_POINT ( 'NONE',  ( -1.509186351706035767, -0.3690944881889763329, 0.3153832671262228327 ) ) ;
#30460 = EDGE_CURVE ( 'NONE', #55363, #50475, #31094, .T. ) ;
#30461 = CARTESIAN_POINT ( 'NONE',  ( -0.8727034120734901146, -0.05778040916215560624, -0.4822834645669293319 ) ) ;
#30462 = CARTESIAN_POINT ( 'NONE',  ( 1.279527559055118724, -0.5400638737290845981, -0.3530559997133363437 ) ) ;
#30463 = CARTESIAN_POINT ( 'NONE',  ( 0.1958661417322836718, -0.3392501089628017219, -0.8760035677503431595 ) ) ;
#30464 = CARTESIAN_POINT ( 'NONE',  ( -1.089238845144356427, -0.3690944881889765550, -0.3153832671262227771 ) ) ;
#30465 = CARTESIAN_POINT ( 'NONE',  ( 1.111517297590296494, 1.088444344143271847, 0.1541001657482228560 ) ) ;
#30466 = CARTESIAN_POINT ( 'NONE',  ( 1.515748031496063186, -0.5400638737290845981, -0.3530559997133363437 ) ) ;
#30467 = CARTESIAN_POINT ( 'NONE',  ( 0.4724409448818896462, 0.1265901696524990294, -2.248687664041994605 ) ) ;
#30468 = CARTESIAN_POINT ( 'NONE',  ( -1.187664041994750175, -0.05778040916215560624, -0.4822834645669293319 ) ) ;
#30469 = CARTESIAN_POINT ( 'NONE',  ( -1.456692913385826182, 0.1771653543307087630, 0.000000000000000000 ) ) ;
#30470 = CARTESIAN_POINT ( 'NONE',  ( -0.8070866141732276899, -0.4536011799217367080, 0.2665933059059888421 ) ) ;
#30471 = CARTESIAN_POINT ( 'NONE',  ( -0.5249343832020990641, 0.1539470093639523085, 0.1968503937007873850 ) ) ;
#30472 = CARTESIAN_POINT ( 'NONE',  ( -0.5183727034120726440, 0.2952755905511811885, 0.1292274648535926551 ) ) ;
#30473 = CARTESIAN_POINT ( 'NONE',  ( -0.03280839895013062252, 0.1771653543307087075, -0.09757992244046823083 ) ) ;
#30474 = CARTESIAN_POINT ( 'NONE',  ( -1.259842519685038686, -0.1870078740157479769, 0.3641732283464567677 ) ) ;
#30475 = CARTESIAN_POINT ( 'NONE',  ( -1.653543307086613234, -0.1870078740157480879, -0.4822834645669291653 ) ) ;
#30476 = CARTESIAN_POINT ( 'NONE',  ( 1.148293963254593653, 0.1771653543307087075, -0.09757992244046823083 ) ) ;
#30477 = CARTESIAN_POINT ( 'NONE',  ( 1.089238845144357759, 0.05413385826771626580, -0.4176697321401330321 ) ) ;
#30478 = DIRECTION ( 'NONE',  ( 0.000000000000000000, 0.000000000000000000, 1.000000000000000000 ) ) ;
#30479 = CARTESIAN_POINT ( 'NONE',  ( 0.4461942257217856311, 0.1283753931104746893, -0.1820866141732285504 ) ) ;
#30480 = CARTESIAN_POINT ( 'NONE',  ( 0.3149606299212606708, -0.1870078740157480879, -0.4822834645669291653 ) ) ;
#30481 = CARTESIAN_POINT ( 'NONE',  ( 1.043307086614173818, -0.4536011799217368745, -0.2665933059059886201 ) ) ;
#30482 = ORIENTED_EDGE ( 'NONE', *, *, #64825, .F. ) ;
#30483 = CARTESIAN_POINT ( 'NONE',  ( -1.089238845144356427, -0.4281496062992127816, -0.4176697321401328100 ) ) ;
#30484 = EDGE_CURVE ( 'NONE', #22014, #52853, #41823, .T. ) ;
#30485 = CARTESIAN_POINT ( 'NONE',  ( -0.8595800524934373854, -0.05778040916215522460, 0.4822834645669289988 ) ) ;
#30486 = CARTESIAN_POINT ( 'NONE',  ( 0.03280839895013198948, 0.2952755905511811885, 0.1292274648535926551 ) ) ;
#30487 = CARTESIAN_POINT ( 'NONE',  ( 0.3996062992125986035, -0.1070741851644053111, -0.1115485564304461857 ) ) ;
#30488 = CARTESIAN_POINT ( 'NONE',  ( 0.2925321140481932369, 0.2925321140481932369, -2.734251968503936148 ) ) ;
#30489 = CARTESIAN_POINT ( 'NONE',  ( 0.5643044619422579178, -0.4281496062992127816, -0.4176697321401328100 ) ) ;
#30490 = CARTESIAN_POINT ( 'NONE',  ( -1.732283464566928277, -0.1870078740157479769, 0.4822834645669291653 ) ) ;
#30491 = AXIS2_PLACEMENT_3D ( 'NONE', #12726, #68733, #30419 ) ;
#30492 = CIRCLE ( 'NONE', #4956, 3.937007874015748143 ) ;
#30493 = CARTESIAN_POINT ( 'NONE',  ( 0.09842519685039434474, 0.1660481256975885056, 0.3530559997133364547 ) ) ;
#30494 = CARTESIAN_POINT ( 'NONE',  ( 0.6561679790026253567, 0.2306618581243848609, 0.2411417322834645549 ) ) ;
#30495 = CARTESIAN_POINT ( 'NONE',  ( 0.3996062992125986590, -0.1070741851644053111, -2.001312335958005395 ) ) ;
#30496 = CARTESIAN_POINT ( 'NONE',  ( -0.1974969037888703871, -0.3420746716998661063, -1.482939632545931863 ) ) ;
#30497 = CARTESIAN_POINT ( 'NONE',  ( -0.4318705504292276176, 1.340445554703190378, 1.035625287865071353 ) ) ;
#30498 = CARTESIAN_POINT ( 'NONE',  ( -0.5314960629921196000, 2.742788220949579081, -1.827151630990901054 ) ) ;
#30499 = CARTESIAN_POINT ( 'NONE',  ( -0.2867679344610366554, 0.2867679344610365444, -0.7992125984251967630 ) ) ;
#30500 = CARTESIAN_POINT ( 'NONE',  ( -0.5511811023622041894, -0.1870078740157480601, -0.3641732283464567677 ) ) ;
#30501 = CARTESIAN_POINT ( 'NONE',  ( -0.9120734908136475250, 0.2952755905511811885, 0.1292274648535926551 ) ) ;
#30502 = CARTESIAN_POINT ( 'NONE',  ( 0.5249343832021003964, 0.2306618581243847221, -0.2411417322834647770 ) ) ;
#30503 = EDGE_CURVE ( 'NONE', #54019, #11621, #37829, .T. ) ;
#30504 = CARTESIAN_POINT ( 'NONE',  ( -0.3949938075777411073, 0.1058382717557497660, -2.629265091863516979 ) ) ;
#30505 = CARTESIAN_POINT ( 'NONE',  ( 1.036745406824147731, 0.05413385826771666132, 0.4176697321401328100 ) ) ;
#30506 = CARTESIAN_POINT ( 'NONE',  ( -1.430446194225720724, 0.05413385826771626580, -0.4176697321401330321 ) ) ;
#30507 = CARTESIAN_POINT ( 'NONE',  ( 1.279527559055118724, 0.1660481256975885056, 0.3530559997133364547 ) ) ;
#30508 = CARTESIAN_POINT ( 'NONE',  ( -0.4091458600556402980, -0.2362204724409451284, -2.572178477690288734 ) ) ;
#30509 = CARTESIAN_POINT ( 'NONE',  ( -0.1070741851644051862, -0.3996062992125987146, -2.276902887139107268 ) ) ;
#30510 = CARTESIAN_POINT ( 'NONE',  ( 0.4177787735907000366, 0.3937007874015747699, -1.559171609364239375 ) ) ;
#30511 = CARTESIAN_POINT ( 'NONE',  ( 0.8398950131233602345, 0.2306618581243847221, -0.2411417322834647770 ) ) ;
#30512 = CARTESIAN_POINT ( 'NONE',  ( 0.4461942257217855201, -0.6046776061558807314, 0.2411417322834647770 ) ) ;
#30513 = CARTESIAN_POINT ( 'NONE',  ( 1.148293963254593653, 0.1771653543307087075, -0.09757992244046823083 ) ) ;
#30515 = CARTESIAN_POINT ( 'NONE',  ( -1.476377952755905110, 0.1660481256975885056, 0.3530559997133364547 ) ) ;
#30514 = CARTESIAN_POINT ( 'NONE',  ( 1.679790026246720025, 0.2306618581243848609, 0.2411417322834645549 ) ) ;
#30516 = CARTESIAN_POINT ( 'NONE',  ( 0.3917322834645669549, 2.398668435337827645E-17, -2.875308768207662347 ) ) ;
#30517 =( NAMED_UNIT ( * ) PLANE_ANGLE_UNIT ( ) SI_UNIT ( $, .RADIAN. ) );
#30518 = CARTESIAN_POINT ( 'NONE',  ( 0.6758530183727039509, -0.6692913385826771977, 0.1292274648535927661 ) ) ;
#30519 = CARTESIAN_POINT ( 'NONE',  ( 1.443569553805774897, -0.5023911411419708095, -0.1820866141732282451 ) ) ;
#30520 = CARTESIAN_POINT ( 'NONE',  ( -0.3937007874015740483, -0.1870078740157480879, -0.4822834645669291653 ) ) ;
#30521 = CARTESIAN_POINT ( 'NONE',  ( -0.4855643044619415427, -0.4281496062992124485, 0.4176697321401328655 ) ) ;
#30522 = CARTESIAN_POINT ( 'NONE',  ( -1.476377952755905110, 0.1660481256975885056, 0.3530559997133364547 ) ) ;
#30523 = CARTESIAN_POINT ( 'NONE',  ( 0.1049643490035304938, -0.3917322834645669549, -0.3274278215223098143 ) ) ;
#30524 = CARTESIAN_POINT ( 'NONE',  ( -0.1049643490035302024, -0.3917322834645671215, -1.324146981627296826 ) ) ;
#30525 = CARTESIAN_POINT ( 'NONE',  ( -0.1958661417322836718, 0.3392501089628017219, -2.367454068241469756 ) ) ;
#30526 = CARTESIAN_POINT ( 'NONE',  ( -1.515748031496062076, -0.4536011799217367080, 0.2665933059059888421 ) ) ;
#30527 = ORIENTED_EDGE ( 'NONE', *, *, #2876, .T. ) ;
#30528 = CARTESIAN_POINT ( 'NONE',  ( 0.3949938075777411073, -0.1058382717557499464, -2.788713910761155379 ) ) ;
#30529 = EDGE_LOOP ( 'NONE', ( #68699, #5151, #42400, #66563 ) ) ;
#30530 = CARTESIAN_POINT ( 'NONE',  ( -0.01312335958005186529, 0.009842519685039147898, -0.3409548833797004797 ) ) ;
#30531 = CARTESIAN_POINT ( 'NONE',  ( 1.489501312335958172, -0.08942795157528024563, -0.3641732283464568787 ) ) ;
#30532 = CARTESIAN_POINT ( 'NONE',  ( 0.1998031496062994405, -0.3460692066303958092, -1.509186351706036655 ) ) ;
#30533 = CARTESIAN_POINT ( 'NONE',  ( 1.627296587926509996, -0.5023911411419708095, 0.1820866141732285504 ) ) ;
#30534 = CARTESIAN_POINT ( 'NONE',  ( -0.5314960629921225976, 2.559055118110236560, -0.9881811337016657149 ) ) ;
#30535 = CYLINDRICAL_SURFACE ( 'NONE', #70517, 0.4724409448818898682 ) ;
#30536 = CARTESIAN_POINT ( 'NONE',  ( 0.5314960629921323676, 2.729664702882089511, -1.840814949217402186 ) ) ;
#30537 = CARTESIAN_POINT ( 'NONE',  ( -0.1049643490035307020, 0.3917322834645669549, -0.2486876640419948270 ) ) ;
#30538 = CARTESIAN_POINT ( 'NONE',  ( -0.7742782152230962556, -0.3690944881889765550, -0.3153832671262227771 ) ) ;
#30539 = CARTESIAN_POINT ( 'NONE',  ( -0.9973753280839886548, -0.5023911411419708095, -0.1820866141732282451 ) ) ;
#30540 = CARTESIAN_POINT ( 'NONE',  ( 0.5643044619422579178, -0.4281496062992127816, -0.4176697321401328100 ) ) ;
#30541 = CARTESIAN_POINT ( 'NONE',  ( -1.292650918635170010, 0.2952755905511810774, -0.1292274648535930714 ) ) ;
#30542 = CARTESIAN_POINT ( 'NONE',  ( -9.594673741351313045E-17, 0.3917322834645670104, -0.1496062992125983815 ) ) ;
#30543 = ORIENTED_EDGE ( 'NONE', *, *, #73157, .F. ) ;
#30544 = CARTESIAN_POINT ( 'NONE',  ( 1.345144356955381593, -0.3162353388693409650, -0.4822834645669289433 ) ) ;
#30545 = CARTESIAN_POINT ( 'NONE',  ( 0.000000000000000000, 2.755905511811024056, 0.000000000000000000 ) ) ;
#30546 = VECTOR ( 'NONE', #55229, 39.37007874015748143 ) ;
#30547 = CARTESIAN_POINT ( 'NONE',  ( -0.4724409448818895907, -0.1265901696524993070, -1.778215223097112663 ) ) ;
#30548 = DIRECTION ( 'NONE',  ( 0.000000000000000000, 0.000000000000000000, 1.000000000000000000 ) ) ;
#30549 = CARTESIAN_POINT ( 'NONE',  ( -0.5971128608923877978, -0.5511811023622048555, -0.09757992244046775898 ) ) ;
#30550 = AXIS2_PLACEMENT_3D ( 'NONE', #7495, #64310, #57979 ) ;
#30551 = DIRECTION ( 'NONE',  ( -3.491481338843132961E-15, -0.000000000000000000, 1.000000000000000000 ) ) ;
#30552 = CARTESIAN_POINT ( 'NONE',  ( -1.069553805774277722, -0.6692913385826773087, -0.1292274648535924053 ) ) ;
#30553 = CARTESIAN_POINT ( 'NONE',  ( 1.069553805774278832, 0.2952755905511810774, -0.1292274648535930714 ) ) ;
#30554 = STYLED_ITEM ( 'NONE', ( #36299 ), #61376 ) ;
#30555 = EDGE_LOOP ( 'NONE', ( #23169, #17914, #39523, #35275 ) ) ;
#30556 = CARTESIAN_POINT ( 'NONE',  ( 0.6824146981627303710, 0.1539470093639521697, -0.1968503937007875793 ) ) ;
#30557 = CARTESIAN_POINT ( 'NONE',  ( 1.660104986876641320, -0.05778040916215522460, 0.4822834645669289988 ) ) ;
#30558 = CARTESIAN_POINT ( 'NONE',  ( -1.351706036745406347, 0.05413385826771626580, -0.4176697321401330321 ) ) ;
#30559 = CARTESIAN_POINT ( 'NONE',  ( -0.2867679344610364334, -0.2867679344610368219, -0.4540489256879772784 ) ) ;
#30560 = CARTESIAN_POINT ( 'NONE',  ( 0.1640419947506569498, -0.08942795157527998196, 0.3641732283464567121 ) ) ;
#30561 = CARTESIAN_POINT ( 'NONE',  ( 0.3917322834645669549, 0.1049643490035304660, -0.9967191601049869565 ) ) ;
#30562 = CARTESIAN_POINT ( 'NONE',  ( -0.1968503937007867743, 0.1771653543307087630, 0.000000000000000000 ) ) ;
#30564 = EDGE_CURVE ( 'NONE', #39863, #57436, #81138, .T. ) ;
#30563 = CARTESIAN_POINT ( 'NONE',  ( 0.4133858267716541968, -0.4536011799217368745, -0.2665933059059886201 ) ) ;
#30565 = CARTESIAN_POINT ( 'NONE',  ( 0.5708661417322841158, -0.5400638737290845981, -0.3530559997133363437 ) ) ;
#30566 = CARTESIAN_POINT ( 'NONE',  ( -0.9186351706036736120, -0.5023911411419708095, -0.1820866141732282451 ) ) ;
#30567 = CARTESIAN_POINT ( 'NONE',  ( 0.1049643490035303689, 0.3917322834645670104, -2.190288713910760521 ) ) ;
#30568 = CARTESIAN_POINT ( 'NONE',  ( 1.489501312335958172, -0.05778040916215560624, -0.4822834645669293319 ) ) ;
#30569 = CARTESIAN_POINT ( 'NONE',  ( -1.089238845144356427, -0.4281496062992127816, -0.4176697321401328100 ) ) ;
#30570 = CARTESIAN_POINT ( 'NONE',  ( -0.4724409448818898682, -8.678599364036362592E-17, -0.5885826771653542844 ) ) ;
#30571 = CARTESIAN_POINT ( 'NONE',  ( 0.04593175853018440641, 0.2952755905511810774, -0.1292274648535930714 ) ) ;
#30572 = CARTESIAN_POINT ( 'NONE',  ( -0.7152230971128602510, -0.3162353388693405765, 0.4822834645669290543 ) ) ;
#30573 = CARTESIAN_POINT ( 'NONE',  ( 1.240157480314961314, 0.07958543189024071263, -0.2665933059059888421 ) ) ;
#30574 = CARTESIAN_POINT ( 'NONE',  ( -0.05905511811023545637, -0.4536011799217368745, -0.2665933059059886201 ) ) ;
#30575 = CARTESIAN_POINT ( 'NONE',  ( -0.3215223097112853146, -0.3162353388693405765, 0.4822834645669290543 ) ) ;
#30576 = CARTESIAN_POINT ( 'NONE',  ( -1.089238845144356427, -0.4281496062992127816, -0.4176697321401328100 ) ) ;
#30577 = CARTESIAN_POINT ( 'NONE',  ( -1.614173228346457378, 2.157411728916712068, 0.1372047244094476981 ) ) ;
#30578 = CARTESIAN_POINT ( 'NONE',  ( -1.012125901091927904, 5.991678263669262536E-15, 0.3791483426435162674 ) ) ;
#30579 = CARTESIAN_POINT ( 'NONE',  ( -0.1640419947506553400, -0.05778040916215560624, -0.4822834645669293319 ) ) ;
#30580 = VERTEX_POINT ( 'NONE', #47045 ) ;
#30581 = CARTESIAN_POINT ( 'NONE',  ( 0.3996062992125984925, 0.1070741851644054637, -1.933727034120735100 ) ) ;
#30582 = CARTESIAN_POINT ( 'NONE',  ( 1.305774278215223960, 0.2952755905511810774, -0.1292274648535930714 ) ) ;
#30583 = CARTESIAN_POINT ( 'NONE',  ( -0.6299212598425188991, -0.1870078740157479769, 0.3641732283464567677 ) ) ;
#30584 = CARTESIAN_POINT ( 'NONE',  ( -0.6889763779527552368, -0.5400638737290845981, -0.3530559997133363437 ) ) ;
#30585 = CARTESIAN_POINT ( 'NONE',  ( 1.430446194225722500, -0.4281496062992127816, -0.4176697321401328100 ) ) ;
#30586 = CARTESIAN_POINT ( 'NONE',  ( 1.036745406824147731, 0.05413385826771666132, 0.4176697321401328100 ) ) ;
#30587 = CARTESIAN_POINT ( 'NONE',  ( 0.000000000000000000, 0.000000000000000000, 0.000000000000000000 ) ) ;
#30588 = CARTESIAN_POINT ( 'NONE',  ( -0.9514435695538050464, -0.2845877964562159024, 0.3641732283464567677 ) ) ;
#30589 = CARTESIAN_POINT ( 'NONE',  ( -0.2925321140481930149, -0.2925321140481933480, -0.6082677165354329896 ) ) ;
#30590 = CARTESIAN_POINT ( 'NONE',  ( -9.787531504996567848E-17, 0.3996062992125986035, -0.3149606299212598381 ) ) ;
#30591 = CARTESIAN_POINT ( 'NONE',  ( -9.674558042662121740E-17, 0.3949938075777409963, -0.3149606299212598937 ) ) ;
#30592 = CARTESIAN_POINT ( 'NONE',  ( 0.1345703391920829439, 1.081211091791629109, 2.857167579953707737 ) ) ;
#30593 = CARTESIAN_POINT ( 'NONE',  ( 0.9842519685039378130, -0.5511811023622047445, 6.969142054262312111E-17 ) ) ;
#30594 = CARTESIAN_POINT ( 'NONE',  ( 0.6299212598425204535, -0.1870078740157479769, 0.3641732283464567677 ) ) ;
#30595 = CARTESIAN_POINT ( 'NONE',  ( 0.3280839895013130669, 0.05413385826771666132, 0.4176697321401328100 ) ) ;
#30596 = CARTESIAN_POINT ( 'NONE',  ( 0.2642592750917004407, -0.1321325610835860920, 0.1571896754257856577 ) ) ;
#30597 = CARTESIAN_POINT ( 'NONE',  ( -0.1058382717557497660, -0.3949938075777411073, -0.9363517060367456679 ) ) ;
#30598 = CARTESIAN_POINT ( 'NONE',  ( 0.9711286089238851948, -0.5023911411419708095, -0.1820866141732282451 ) ) ;
#30599 = CARTESIAN_POINT ( 'NONE',  ( -0.2230971128608915943, 0.05413385826771666132, 0.4176697321401328100 ) ) ;
#30600 = CARTESIAN_POINT ( 'NONE',  ( -0.8595800524934373854, -0.05778040916215522460, 0.4822834645669289988 ) ) ;
#30601 = CARTESIAN_POINT ( 'NONE',  ( 1.095800524934383846, -0.05778040916215560624, -0.4822834645669293319 ) ) ;
#30602 = CARTESIAN_POINT ( 'NONE',  ( 0.4724409448818897572, -0.1265901696524988906, -1.371391076115485053 ) ) ;
#30603 = AXIS2_PLACEMENT_3D ( 'NONE', #78744, #66105, #59772 ) ;
#30604 = CARTESIAN_POINT ( 'NONE',  ( 0.1998031496062994405, -0.3460692066303958092, -2.296587926509186417 ) ) ;
#30605 = CARTESIAN_POINT ( 'NONE',  ( -0.07217847769028813698, -0.2845877964562161244, -0.3641732283464567121 ) ) ;
#30606 = EDGE_CURVE ( 'NONE', #3377, #30219, #52939, .T. ) ;
#30607 = ORIENTED_EDGE ( 'NONE', *, *, #69950, .F. ) ;
#30608 = CARTESIAN_POINT ( 'NONE',  ( -0.3917322834645671770, 0.1049643490035302024, -0.8169484496401069329 ) ) ;
#30609 = VERTEX_POINT ( 'NONE', #34436 ) ;
#30610 = CARTESIAN_POINT ( 'NONE',  ( -0.7086614173228339419, -0.1870078740157480879, -0.4822834645669291653 ) ) ;
#30611 = CARTESIAN_POINT ( 'NONE',  ( -0.2230971128608915943, 0.05413385826771666132, 0.4176697321401328100 ) ) ;
#30612 = CARTESIAN_POINT ( 'NONE',  ( -0.5314960629921250401, 0.1660481256975885056, 0.3530559997133364547 ) ) ;
#30613 = CARTESIAN_POINT ( 'NONE',  ( 0.5511811023622055217, -0.1870078740157479769, 0.4822834645669291653 ) ) ;
#30614 = EDGE_CURVE ( 'NONE', #712, #60855, #12935, .T. ) ;
#30615 = CARTESIAN_POINT ( 'NONE',  ( -0.5118110236220466680, 0.2952755905511811885, 0.000000000000000000 ) ) ;
#30616 = CARTESIAN_POINT ( 'NONE',  ( -1.476377952755905110, 0.1660481256975885056, 0.3530559997133364547 ) ) ;
#30617 = CARTESIAN_POINT ( 'NONE',  ( -0.7217847769028863381, 0.05413385826771626580, -0.4176697321401330321 ) ) ;
#30618 = CARTESIAN_POINT ( 'NONE',  ( 0.6758530183727039509, 0.2952755905511810774, -0.1292274648535930714 ) ) ;
#30619 = CARTESIAN_POINT ( 'NONE',  ( 0.3917322834645670104, -0.1049643490035303411, -1.206036745406823707 ) ) ;
#30620 = CARTESIAN_POINT ( 'NONE',  ( -0.5052493438320203589, 0.1771653543307087075, -0.09757992244046823083 ) ) ;
#30621 = ORIENTED_EDGE ( 'NONE', *, *, #78936, .T. ) ;
#30622 = CARTESIAN_POINT ( 'NONE',  ( -0.1974969037888703871, -0.3420746716998661063, -1.325459317585301777 ) ) ;
#30623 = ORIENTED_EDGE ( 'NONE', *, *, #16700, .F. ) ;
#30624 = CARTESIAN_POINT ( 'NONE',  ( -1.482939632545930975, -0.3690944881889765550, -0.3153832671262227771 ) ) ;
#30625 = CARTESIAN_POINT ( 'NONE',  ( -1.082677165354329896, -0.5400638737290845981, -0.3530559997133363437 ) ) ;
#30626 = CARTESIAN_POINT ( 'NONE',  ( -0.9645669291338575535, 0.1660481256975883668, -0.3530559997133364547 ) ) ;
#30627 = CARTESIAN_POINT ( 'NONE',  ( 1.948818897637795367, 0.000000000000000000, 5.701968306260621233 ) ) ;
#30628 = CARTESIAN_POINT ( 'NONE',  ( -0.5971128608923877978, 0.2952755905511811885, 0.1292274648535926551 ) ) ;
#30629 = CARTESIAN_POINT ( 'NONE',  ( -0.7414698162729651543, 0.2952755905511810774, -0.1292274648535930714 ) ) ;
#30630 = DIRECTION ( 'NONE',  ( 1.000000000000000000, 0.000000000000000000, 0.000000000000000000 ) ) ;
#30631 = CARTESIAN_POINT ( 'NONE',  ( -0.4574207045264588878, 1.664236311372951471, -3.910347889586886172 ) ) ;
#30632 = CARTESIAN_POINT ( 'NONE',  ( 0.7152230971128616943, -0.08942795157527998196, 0.3641732283464567121 ) ) ;
#30633 = CARTESIAN_POINT ( 'NONE',  ( 1.603475055217291612, 0.4410854135902469442, 0.04573490813648272563 ) ) ;
#30634 = CARTESIAN_POINT ( 'NONE',  ( 0.1958661417322834775, 0.3392501089628018884, -0.07152230971128617498 ) ) ;
#30635 = CARTESIAN_POINT ( 'NONE',  ( 0.03937007874015806264, 0.1771653543307087630, 0.000000000000000000 ) ) ;
#30636 = CARTESIAN_POINT ( 'NONE',  ( -0.2821522309711278487, -0.6692913385826773087, -0.1292274648535924053 ) ) ;
#30637 = CARTESIAN_POINT ( 'NONE',  ( 3.935572654129527503, 1.075044193959341809, 0.1073736613157593028 ) ) ;
#30638 = CARTESIAN_POINT ( 'NONE',  ( -0.1049868766404193215, -0.6046776061558807314, 0.2411417322834647770 ) ) ;
#30639 = ORIENTED_EDGE ( 'NONE', *, *, #27779, .F. ) ;
#30640 = CARTESIAN_POINT ( 'NONE',  ( -0.1998031496062994683, 0.3460692066303958092, -2.217847769028871596 ) ) ;
#30641 = FACE_OUTER_BOUND ( 'NONE', #10361, .T. ) ;
#30642 = ORIENTED_EDGE ( 'NONE', *, *, #70994, .F. ) ;
#30643 = CARTESIAN_POINT ( 'NONE',  ( -0.3460692066303957537, -0.1998031496062994405, -1.389107611548556553 ) ) ;
#30644 = CARTESIAN_POINT ( 'NONE',  ( -0.02963302784744966181, 0.3970677821444046907, -2.755905511811023612 ) ) ;
#30645 = CARTESIAN_POINT ( 'NONE',  ( -1.227034120734907585, 0.1771653543307087630, 0.09757992244046791164 ) ) ;
#30646 = CARTESIAN_POINT ( 'NONE',  ( -1.036745406824146176, 0.05413385826771626580, -0.4176697321401330321 ) ) ;
#30647 = CARTESIAN_POINT ( 'NONE',  ( -0.1265901696524993347, 0.4724409448818895907, -0.3215223097112860362 ) ) ;
#30648 = ADVANCED_FACE ( 'NONE', ( #58857 ), #10899, .F. ) ;
#30649 = LINE ( 'NONE', #36961, #58621 ) ;
#30650 = CARTESIAN_POINT ( 'NONE',  ( -0.2867679344610365999, 0.2867679344610364889, 0.1456692913385827237 ) ) ;
#30651 = CARTESIAN_POINT ( 'NONE',  ( 1.430446194225722500, -0.4281496062992127816, -0.4176697321401328100 ) ) ;
#30652 = CARTESIAN_POINT ( 'NONE',  ( 0.5708661417322841158, -0.5400638737290845981, -0.3530559997133363437 ) ) ;
#30653 = CARTESIAN_POINT ( 'NONE',  ( 0.3674540682414705883, -0.6046776061558807314, 0.2411417322834647770 ) ) ;
#30654 = CARTESIAN_POINT ( 'NONE',  ( -1.253280839895012377, -0.2845877964562161244, -0.3641732283464567121 ) ) ;
#30655 = CARTESIAN_POINT ( 'NONE',  ( -0.4855643044619415427, -0.4281496062992124485, 0.4176697321401328655 ) ) ;
#30656 = CARTESIAN_POINT ( 'NONE',  ( 0.3458507752293908943, -0.3458507752293908943, -2.537401574803149984 ) ) ;
#30657 = CARTESIAN_POINT ( 'NONE',  ( -0.7874015748031489847, -0.1870078740157479769, 0.4822834645669291653 ) ) ;
#30658 = EDGE_CURVE ( 'NONE', #51820, #33736, #79481, .T. ) ;
#30659 = CARTESIAN_POINT ( 'NONE',  ( 0.1058382717557499880, 0.3949938075777409408, -2.274934383202099841 ) ) ;
#30660 = CARTESIAN_POINT ( 'NONE',  ( 1.391076115485564868, -0.5023911411419708095, 0.1820866141732285504 ) ) ;
#30661 = CARTESIAN_POINT ( 'NONE',  ( -0.3412073490813641308, -0.5023911411419708095, 0.1820866141732285504 ) ) ;
#30662 = CARTESIAN_POINT ( 'NONE',  ( 1.043307086614173818, 0.07958543189024085140, 0.2665933059059887866 ) ) ;
#30663 = CARTESIAN_POINT ( 'NONE',  ( -1.463254593175852492, -0.6692913385826773087, -0.1292274648535924053 ) ) ;
#30664 = CARTESIAN_POINT ( 'NONE',  ( -0.9383202099737524282, -0.2845877964562161244, -0.3641732283464567121 ) ) ;
#30665 = CARTESIAN_POINT ( 'NONE',  ( 0.1463826306659141430, 2.110655687203366066E-15, -0.3954974714151459625 ) ) ;
#30666 = CARTESIAN_POINT ( 'NONE',  ( 0.4068241469816281097, -0.004921259842519576551, 0.3153832671262227771 ) ) ;
#30667 = CARTESIAN_POINT ( 'NONE',  ( -0.2624671916010490880, -0.6046776061558807314, 0.2411417322834647770 ) ) ;
#30668 = ADVANCED_FACE ( 'NONE', ( #66426, #46633, #1214, #9181, #33601 ), #15083, .F. ) ;
#30669 = B_SPLINE_CURVE_WITH_KNOTS ( 'NONE', 3,
 ( #67836, #61089, #29103, #10175 ),
 .UNSPECIFIED., .F., .F.,
 ( 4, 4 ),
 ( 0.1000642744325471178, 0.1014879310549284402 ),
 .UNSPECIFIED. ) ;
#30670 = CARTESIAN_POINT ( 'NONE',  ( -0.2238009295390064879, -2.294479370626195693E-15, 0.3464511005275217603 ) ) ;
#30671 = CARTESIAN_POINT ( 'NONE',  ( 0.1246719160104994284, 0.1771653543307087075, -0.09757992244046823083 ) ) ;
#30672 = LINE ( 'NONE', #37803, #22446 ) ;
#30673 = CARTESIAN_POINT ( 'NONE',  ( 0.9251968503937015864, 0.1660481256975883668, -0.3530559997133364547 ) ) ;
#30674 = LINE ( 'NONE', #43278, #23633 ) ;
#30675 = CARTESIAN_POINT ( 'NONE',  ( 1.496062992125984703, -0.1870078740157480601, -0.3641732283464567677 ) ) ;
#30676 = CARTESIAN_POINT ( 'NONE',  ( -1.128608923884513837, -0.6046776061558807314, 0.2411417322834647770 ) ) ;
#30677 = CARTESIAN_POINT ( 'NONE',  ( -0.1049868766404193215, -0.5023911411419708095, 0.1820866141732285504 ) ) ;
#30678 = CARTESIAN_POINT ( 'NONE',  ( -0.7233796917120556280, 1.992010844874188447, 0.5048038503170210189 ) ) ;
#30679 = CARTESIAN_POINT ( 'NONE',  ( 0.2427821522309716595, -0.2845877964562161244, -0.3641732283464567121 ) ) ;
#30680 = CARTESIAN_POINT ( 'NONE',  ( -1.338582677165353729, -0.1870078740157480879, -0.4822834645669291653 ) ) ;
#30681 = CARTESIAN_POINT ( 'NONE',  ( -0.4396325459317577122, -0.6692913385826773087, -0.1292274648535924053 ) ) ;
#30682 = CARTESIAN_POINT ( 'NONE',  ( -0.1070741851644051862, -0.3996062992125986590, -0.6213910761154856077 ) ) ;
#30683 = CARTESIAN_POINT ( 'NONE',  ( 0.2867679344610365999, -0.2867679344610365444, -2.387795275590551380 ) ) ;
#30684 = CARTESIAN_POINT ( 'NONE',  ( 0.5052493438320215802, 0.1771653543307087630, 0.09757992244046791164 ) ) ;
#30685 = CARTESIAN_POINT ( 'NONE',  ( -0.3805774278215216522, 0.05413385826771666132, 0.4176697321401328100 ) ) ;
#30686 = CARTESIAN_POINT ( 'NONE',  ( -0.7283464566929126471, -0.5400638737290844871, 0.3530559997133364547 ) ) ;
#30687 = CARTESIAN_POINT ( 'NONE',  ( -0.9514435695538050464, -0.08942795157528024563, -0.3641732283464568787 ) ) ;
#30688 = CARTESIAN_POINT ( 'NONE',  ( -3.929901827426621530, 1.125753869628013160, -0.2378376118093886160 ) ) ;
#30689 = CARTESIAN_POINT ( 'NONE',  ( 0.05905511811023709395, -0.5400638737290844871, 0.3530559997133364547 ) ) ;
#30690 = CARTESIAN_POINT ( 'NONE',  ( -1.259842519685038686, -0.1870078740157479769, 0.3641732283464567677 ) ) ;
#30691 = CARTESIAN_POINT ( 'NONE',  ( -1.594488188976377119, 0.1660481256975883668, -0.3530559997133364547 ) ) ;
#30692 = CARTESIAN_POINT ( 'NONE',  ( 0.4091458600556403535, 0.2362204724409449896, -2.178477690288713742 ) ) ;
#30693 = ORIENTED_EDGE ( 'NONE', *, *, #41957, .F. ) ;
#30694 = CARTESIAN_POINT ( 'NONE',  ( -1.601049868766403650, -0.5023911411419708095, 0.1820866141732285504 ) ) ;
#30695 = CARTESIAN_POINT ( 'NONE',  ( -1.181102362204723644, -0.1870078740157480879, -0.4822834645669291653 ) ) ;
#30696 = CARTESIAN_POINT ( 'NONE',  ( -0.9186351706036736120, 0.2306618581243848609, 0.2411417322834645549 ) ) ;
#30697 = CARTESIAN_POINT ( 'NONE',  ( -1.535433070866141225, -0.6692913385826771977, 8.415575281601705876E-17 ) ) ;
#30698 = CARTESIAN_POINT ( 'NONE',  ( 4.797336870675656522E-17, -0.3917322834645670104, -1.580708661417322913 ) ) ;
#30699 = CARTESIAN_POINT ( 'NONE',  ( -0.2643935821217223148, 0.2898214735618642734, -1.220472440944881498 ) ) ;
#30700 = CARTESIAN_POINT ( 'NONE',  ( 1.043307086614173818, 0.1660481256975885056, 0.3530559997133364547 ) ) ;
#30701 = CARTESIAN_POINT ( 'NONE',  ( 0.5380577427821529035, -0.4281496062992124485, 0.4176697321401328655 ) ) ;
#30702 = CARTESIAN_POINT ( 'NONE',  ( 0.4359958488159500489, 1.724409448818897905, 2.094141031014936871 ) ) ;
#30703 = CARTESIAN_POINT ( 'NONE',  ( 4.893765752498283308E-17, -0.3996062992125985480, -2.517716535433071279 ) ) ;
#30704 = CARTESIAN_POINT ( 'NONE',  ( 1.122047244094488860, 0.07958543189024085140, 0.2665933059059887866 ) ) ;
#30705 = EDGE_CURVE ( 'NONE', #21301, #75845, #44069, .T. ) ;
#30706 = CARTESIAN_POINT ( 'NONE',  ( 0.3996062992125986035, 2.446882876249141962E-17, -1.062992125984252079 ) ) ;
#30707 = VERTEX_POINT ( 'NONE', #73152 ) ;
#30708 = CARTESIAN_POINT ( 'NONE',  ( -0.9580052493438311334, -0.004921259842519870586, -0.3153832671262229437 ) ) ;
#30709 = CARTESIAN_POINT ( 'NONE',  ( -0.3917322834645670104, -7.196005306013484475E-17, -2.708661417322834275 ) ) ;
#30710 = ORIENTED_EDGE ( 'NONE', *, *, #63585, .T. ) ;
#30711 = CARTESIAN_POINT ( 'NONE',  ( 0.4593175853018379162, -0.4281496062992124485, 0.4176697321401328655 ) ) ;
#30712 = CARTESIAN_POINT ( 'NONE',  ( -0.7677165354330699465, 0.1660481256975885056, 0.3530559997133364547 ) ) ;
#30713 = CARTESIAN_POINT ( 'NONE',  ( -0.9120734908136475250, -0.6692913385826773087, -0.1292274648535924053 ) ) ;
#30714 = CARTESIAN_POINT ( 'NONE',  ( 0.9383202099737538715, -0.05778040916215560624, -0.4822834645669293319 ) ) ;
#30715 = CARTESIAN_POINT ( 'NONE',  ( 1.581364829396326277, -0.3162353388693409650, -0.4822834645669289433 ) ) ;
#30716 = DIRECTION ( 'NONE',  ( 0.000000000000000000, 0.000000000000000000, -1.000000000000000000 ) ) ;
#30717 = CARTESIAN_POINT ( 'NONE',  ( 0.01312335958005323398, -0.4281496062992127816, -0.4176697321401328100 ) ) ;
#30718 = CARTESIAN_POINT ( 'NONE',  ( -1.187664041994749731, -0.3162353388693405765, 0.4822834645669290543 ) ) ;
#30719 = CARTESIAN_POINT ( 'NONE',  ( -1.614173228346457378, 1.606230626554505658, -0.1372047244094477536 ) ) ;
#30720 = CARTESIAN_POINT ( 'NONE',  ( 1.535433070866142558, 0.2952755905511811885, 0.000000000000000000 ) ) ;
#30721 =( BOUNDED_CURVE ( )  B_SPLINE_CURVE ( 2, ( #28537, #40751, #34445, #65619, #65193, #46225, #1631, #21806, #47470, #54194, #78242, #27290, #14686, #66435, #2465, #71921, #28123, #20983, #53778, #59275, #79910, #47882, #14271, #79491, #52948, #39505, #78662, #40343, #67269, #23047, #55434, #60935, #68907, #80326, #56269, #41987, #36096, #48300, #23874, #4936, #81965, #74829, #9602, #68501, #49123, #61767, #74412, #54615, #16344, #4515, #10440, #15932, #81143, #10017, #3285, #28950, #30604, #30184, #62177, #16756, #22640, #35270, #73997, #67681, #49540, #23458, #10841, #35682, #41579, #61348, #3702, #81555, #75235, #62593, #29365, #55025, #42395, #17174, #42807, #80733, #4107, #17578, #48714, #68094, #36501, #29773, #55846, #43211, #24280, #11259, #49951, #36917, #11677, #12487, #37738, #64247, #12907, #50360, #63412, #12080, #25512, #24692, #277, #64661, #32667, #50772, #19623, #38978, #82777, #25932, #31837, #76472, #76057, #5346, #77292, #5747, #6162, #63007, #25099, #75649, #18799, #6581, #38566, #44443, #31005, #45285, #17989 ),
 .UNSPECIFIED., .F., .F. ) 
 B_SPLINE_CURVE_WITH_KNOTS ( ( 3, 2, 2, 2, 2, 2, 2, 2, 2, 2, 2, 2, 2, 2, 2, 2, 2, 2, 2, 2, 2, 2, 2, 2, 2, 2, 2, 2, 2, 2, 2, 2, 2, 2, 2, 2, 2, 2, 2, 2, 2, 2, 2, 2, 2, 2, 2, 2, 2, 2, 2, 2, 2, 2, 2, 2, 2, 2, 2, 2, 2, 2, 2, 3 ),
 ( 0.6625000000000256239, 0.6666666666666918317, 0.6708333333333581505, 0.6750000000000244693, 0.6791666666666906771, 0.6833333333333569959, 0.6875000000000232037, 0.6916666666666894114, 0.6958333333333557302, 0.7000000000000219380, 0.7041666666666882568, 0.7083333333333545756, 0.7125000000000207834, 0.7166666666666869911, 0.7208333333333533099, 0.7250000000000195177, 0.7291666666666857255, 0.7333333333333520443, 0.7375000000000183631, 0.7416666666666845709, 0.7458333333333508897, 0.7500000000000170974, 0.7541666666666833052, 0.7583333333333496240, 0.7625000000000158318, 0.7666666666666821506, 0.7708333333333484694, 0.7750000000000146771, 0.7791666666666808849, 0.7833333333333472037, 0.7875000000000134115, 0.7916666666666796193, 0.7958333333333459381, 0.8000000000000122569, 0.8041666666666784646, 0.8083333333333446724, 0.8125000000000109912, 0.8166666666666771990, 0.8208333333333435178, 0.8250000000000097256, 0.8291666666666761554, 0.8333333333333423631, 0.8375000000000085709, 0.8416666666666747787, 0.8458333333333410975, 0.8500000000000073053, 0.8541666666666735130, 0.8583333333333398318, 0.8625000000000061506, 0.8666666666666723584, 0.8708333333333386772, 0.8750000000000048850, 0.8791666666666710928, 0.8833333333333374116, 0.8875000000000036193, 0.8916666666666699381, 0.8958333333333361459, 0.9000000000000024647, 0.9041666666666687835, 0.9083333333333349913, 0.9125000000000011990, 0.9166666666666674068, 0.9208333333333336146, 0.9250000000000000444 ),
 .UNSPECIFIED. ) 
 CURVE ( )  GEOMETRIC_REPRESENTATION_ITEM ( )  RATIONAL_B_SPLINE_CURVE ( ( 0.9999999999997902789, 0.9659258262892780333, 1.000000000000000000, 0.9659258262890683122, 1.000000000000000000, 0.9659258262890683122, 1.000000000000000000, 0.9659258262890683122, 1.000000000000000000, 0.9659258262890683122, 1.000000000000000000, 0.9659258262890683122, 1.000000000000000000, 0.9659258262890683122, 1.000000000000000000, 0.9659258262890683122, 1.000000000000000000, 0.9659258262890683122, 1.000000000000000000, 0.9659258262890683122, 1.000000000000000000, 0.9659258262890683122, 1.000000000000000000, 0.9659258262890683122, 1.000000000000000000, 0.9659258262890683122, 1.000000000000000000, 0.9659258262890683122, 1.000000000000000000, 0.9659258262890683122, 1.000000000000000000, 0.9659258262890683122, 1.000000000000000000, 0.9659258262890683122, 1.000000000000000000, 0.9659258262890683122, 1.000000000000000000, 0.9659258262890683122, 1.000000000000000000, 0.9659258262890683122, 1.000000000000000000, 0.9659258262890683122, 1.000000000000000000, 0.9659258262890683122, 1.000000000000000000, 0.9659258262890683122, 1.000000000000000000, 0.9659258262890683122, 1.000000000000000000, 0.9659258262890683122, 1.000000000000000000, 0.9659258262890683122, 1.000000000000000000, 0.9659258262890683122, 1.000000000000000000, 0.9659258262890683122, 1.000000000000000000, 0.9659258262890683122, 1.000000000000000000, 0.9659258262890683122, 1.000000000000000000, 0.9659258262890683122, 1.000000000000000000, 0.9659258262890683122, 1.000000000000000000, 0.9659258262890683122, 1.000000000000000000, 0.9659258262890683122, 1.000000000000000000, 0.9659258262890683122, 1.000000000000000000, 0.9659258262890683122, 1.000000000000000000, 0.9659258262890683122, 1.000000000000000000, 0.9659258262890683122, 1.000000000000000000, 0.9659258262890683122, 1.000000000000000000, 0.9659258262890683122, 1.000000000000000000, 0.9659258262890683122, 1.000000000000000000, 0.9659258262890683122, 1.000000000000000000, 0.9659258262890683122, 1.000000000000000000, 0.9659258262890683122, 1.000000000000000000, 0.9659258262890683122, 1.000000000000000000, 0.9659258262890683122, 1.000000000000000000, 0.9659258262890683122, 1.000000000000000000, 0.9659258262890683122, 1.000000000000000000, 0.9659258262890683122, 1.000000000000000000, 0.9659258262890683122, 1.000000000000000000, 0.9659258262890683122, 1.000000000000000000, 0.9659258262890683122, 1.000000000000000000, 0.9659258262890683122, 1.000000000000000000, 0.9659258262890683122, 1.000000000000000000, 0.9659258262890683122, 1.000000000000000000, 0.9659258262890683122, 1.000000000000000000, 0.9659258262890683122, 1.000000000000000000, 0.9659258262890683122, 1.000000000000000000, 0.9659258262890683122, 1.000000000000000000, 0.9659258262890683122, 1.000000000000000000, 0.9659258262890683122, 1.000000000000000000, 0.9659258262890683122, 1.000000000000000000, 0.9659258262890683122, 1.000000000000000000 ) ) 
 REPRESENTATION_ITEM ( '' )  );
#30722 = CARTESIAN_POINT ( 'NONE',  ( -0.3917322834645669549, -0.1049643490035306603, -2.807742782152229832 ) ) ;
#30723 = CARTESIAN_POINT ( 'NONE',  ( 0.6824146981627303710, -0.5023911411419708095, 0.1820866141732285504 ) ) ;
#30724 = ORIENTED_EDGE ( 'NONE', *, *, #46607, .F. ) ;
#30725 = CARTESIAN_POINT ( 'NONE',  ( -0.3949938075777409408, -0.1058382717557502933, -0.3608923884514436686 ) ) ;
#30726 = ORIENTED_EDGE ( 'NONE', *, *, #15919, .T. ) ;
#30727 = CARTESIAN_POINT ( 'NONE',  ( 0.1312335958005255154, -0.5023911411419708095, 0.1820866141732285504 ) ) ;
#30728 = CARTESIAN_POINT ( 'NONE',  ( -1.076935383196057749, 2.165354330708661568, 0.3149606299212595606 ) ) ;
#30729 = CARTESIAN_POINT ( 'NONE',  ( 0.4658792650918640033, -0.3162353388693405765, 0.4822834645669290543 ) ) ;
#30730 = CARTESIAN_POINT ( 'NONE',  ( 0.3083989501312343062, -0.3162353388693405765, 0.4822834645669290543 ) ) ;
#30731 = CARTESIAN_POINT ( 'NONE',  ( -0.5839895013123351797, 0.2952755905511810774, -0.1292274648535930714 ) ) ;
#30732 = CARTESIAN_POINT ( 'NONE',  ( 0.1958661417322836718, -0.3392501089628017219, -1.505924827592862503 ) ) ;
#30733 = CARTESIAN_POINT ( 'NONE',  ( -1.410761154855641575, -0.3162353388693409650, -0.4822834645669289433 ) ) ;
#30734 = CARTESIAN_POINT ( 'NONE',  ( 4.797336870675656522E-17, -0.3917322834645670104, -2.525590551181102317 ) ) ;
#30735 = CARTESIAN_POINT ( 'NONE',  ( 1.469816272965879911, 0.1283753931104746893, -0.1820866141732285504 ) ) ;
#30736 = CARTESIAN_POINT ( 'NONE',  ( -1.056430446194224881, -0.6692913385826771977, 0.1292274648535927661 ) ) ;
#30737 = CARTESIAN_POINT ( 'NONE',  ( 0.9908136482939640111, -0.6692913385826771977, 0.1292274648535927661 ) ) ;
#30738 = CARTESIAN_POINT ( 'NONE',  ( 1.377952755905512472, 0.2952755905511811885, 0.000000000000000000 ) ) ;
#30739 = CARTESIAN_POINT ( 'NONE',  ( -0.2925321140481930704, -0.2925321140481933480, -0.6889763779527556808 ) ) ;
#30740 = CARTESIAN_POINT ( 'NONE',  ( -1.548556430446193399, 0.2306618581243848609, 0.2411417322834645549 ) ) ;
#30741 = CARTESIAN_POINT ( 'NONE',  ( -0.3460692066303960313, 0.1998031496062989965, -0.4179790026246719137 ) ) ;
#30742 = CARTESIAN_POINT ( 'NONE',  ( 0.4265091863517067039, -0.6692913385826773087, -0.1292274648535924053 ) ) ;
#30743 = CARTESIAN_POINT ( 'NONE',  ( 0.1070741851644054915, -0.3996062992125986035, -2.290026246719159442 ) ) ;
#30744 = CARTESIAN_POINT ( 'NONE',  ( 0.3917322834645670104, 2.398668435337828261E-17, -1.777559055118110409 ) ) ;
#30745 = CARTESIAN_POINT ( 'NONE',  ( 1.692913385826772421, 0.2952755905511811885, 0.000000000000000000 ) ) ;
#30746 = CARTESIAN_POINT ( 'NONE',  ( 0.8136482939632553313, -0.5023911411419708095, -0.1820866141732282451 ) ) ;
#30747 = CARTESIAN_POINT ( 'NONE',  ( 0.7677165354330716118, -0.5400638737290844871, 0.3530559997133364547 ) ) ;
#30748 = CARTESIAN_POINT ( 'NONE',  ( 0.4091458600556403535, 0.2362204724409449896, -0.9954068241469815614 ) ) ;
#30749 = CARTESIAN_POINT ( 'NONE',  ( 0.6561679790026253567, -0.5023911411419708095, -0.1820866141732282451 ) ) ;
#30750 = CARTESIAN_POINT ( 'NONE',  ( 0.3608923884514443348, 0.2952755905511810774, -0.1292274648535930714 ) ) ;
#30751 = CARTESIAN_POINT ( 'NONE',  ( -0.3949938075777409963, -7.255918531996591613E-17, -1.061023622047243986 ) ) ;
#30752 = CARTESIAN_POINT ( 'NONE',  ( -0.6036745406824141069, 0.2306618581243848609, 0.2411417322834645549 ) ) ;
#30753 = CARTESIAN_POINT ( 'NONE',  ( 0.2462293917967310342, -2.191421614605370878E-15, 0.4445507791589071167 ) ) ;
#30754 = CARTESIAN_POINT ( 'NONE',  ( 0.8398950131233602345, 0.1283753931104746893, -0.1820866141732285504 ) ) ;
#30755 = CARTESIAN_POINT ( 'NONE',  ( 0.1837270341207354329, 0.2306618581243848609, 0.2411417322834645549 ) ) ;
#30756 = CARTESIAN_POINT ( 'NONE',  ( 0.1685779992553469442, -2.839693391405754848E-15, 0.3954974714151476278 ) ) ;
#30757 = CARTESIAN_POINT ( 'NONE',  ( -0.1443569553805768291, 0.05413385826771666132, 0.4176697321401328100 ) ) ;
#30758 = CARTESIAN_POINT ( 'NONE',  ( 0.09842519685039434474, 0.07958543189024085140, 0.2665933059059887866 ) ) ;
#30759 = CARTESIAN_POINT ( 'NONE',  ( -2.872985923768006877, 1.064103292658512556, -0.03357545743405447591 ) ) ;
#30760 = CARTESIAN_POINT ( 'NONE',  ( -0.1706036745406816491, -0.4281496062992124485, 0.4176697321401328655 ) ) ;
#30761 = CARTESIAN_POINT ( 'NONE',  ( 0.5708661417322841158, -0.4536011799217368745, -0.2665933059059886201 ) ) ;
#30762 = DIRECTION ( 'NONE',  ( 1.000000000000000000, 0.000000000000000000, -1.224646799147353207E-16 ) ) ;
#30763 = CARTESIAN_POINT ( 'NONE',  ( 0.1070741851644053388, 0.3996062992125986035, -1.645013123359579943 ) ) ;
#30764 = CARTESIAN_POINT ( 'NONE',  ( 0.2821522309711292364, 0.2952755905511810774, -0.1292274648535930714 ) ) ;
#30765 = CARTESIAN_POINT ( 'NONE',  ( 1.312335958005250269, -0.5023911411419708095, 0.1820866141732285504 ) ) ;
#30766 = CARTESIAN_POINT ( 'NONE',  ( 1.220472440944882386, 1.277248692536265747E-15, -0.4445507791589058955 ) ) ;
#30767 = CARTESIAN_POINT ( 'NONE',  ( -0.4002624671916004129, -0.08942795157528024563, -0.3641732283464568787 ) ) ;
#30768 = CARTESIAN_POINT ( 'NONE',  ( -0.9448818897637790704, -0.1870078740157479769, 0.3641732283464567677 ) ) ;
#30769 = CARTESIAN_POINT ( 'NONE',  ( -0.2099737532808391705, 0.2306618581243848609, 0.2411417322834645549 ) ) ;
#30770 = CARTESIAN_POINT ( 'NONE',  ( 0.1902887139107617975, 0.2952755905511811885, 0.1292274648535926551 ) ) ;
#30771 = CARTESIAN_POINT ( 'NONE',  ( 0.9711286089238851948, -0.5023911411419708095, -0.1820866141732282451 ) ) ;
#30772 = CARTESIAN_POINT ( 'NONE',  ( -1.719160104986876103, -0.004921259842519576551, 0.3153832671262227771 ) ) ;
#30773 = CARTESIAN_POINT ( 'NONE',  ( 1.541994750656168645, -0.5511811023622046335, 0.09757992244046803654 ) ) ;
#30774 = CARTESIAN_POINT ( 'NONE',  ( 0.7874015748031503170, -0.1870078740157480879, -0.4822834645669291653 ) ) ;
#30775 = DIRECTION ( 'NONE',  ( -0.000000000000000000, -1.000000000000000000, -0.000000000000000000 ) ) ;
#30776 = CARTESIAN_POINT ( 'NONE',  ( 0.03280839895013198948, 0.2952755905511811885, 0.1292274648535926551 ) ) ;
#30777 = CARTESIAN_POINT ( 'NONE',  ( 0.3917322834645670104, -0.1049643490035303411, -0.9835958005249345604 ) ) ;
#30778 = CARTESIAN_POINT ( 'NONE',  ( 1.030183727034121421, -0.05778040916215522460, 0.4822834645669289988 ) ) ;
#30779 = CARTESIAN_POINT ( 'NONE',  ( 0.7349081364829403995, 0.2306618581243848609, 0.2411417322834645549 ) ) ;
#30780 = CARTESIAN_POINT ( 'NONE',  ( -0.4736533538817698230, 1.506391317405408214, -3.908412196150712781 ) ) ;
#30781 = CARTESIAN_POINT ( 'NONE',  ( 0.3608923884514443348, -0.5511811023622046335, 0.09757992244046803654 ) ) ;
#30782 = CARTESIAN_POINT ( 'NONE',  ( 1.397637795275591177, 0.1660481256975883668, -0.3530559997133364547 ) ) ;
#30783 = CARTESIAN_POINT ( 'NONE',  ( 0.1968503937007881344, 0.1771653543307087630, 0.000000000000000000 ) ) ;
#30784 = CARTESIAN_POINT ( 'NONE',  ( -0.4593175853018364174, -0.4281496062992127816, -0.4176697321401328100 ) ) ;
#30785 = CARTESIAN_POINT ( 'NONE',  ( 0.1968503937007881344, 0.2952755905511811885, 0.000000000000000000 ) ) ;
#30786 = CARTESIAN_POINT ( 'NONE',  ( -0.8333333333333323711, 0.2952755905511811885, 0.1292274648535926551 ) ) ;
#30787 = CARTESIAN_POINT ( 'NONE',  ( -0.3937007874015740483, -0.1870078740157480601, -0.3641732283464567677 ) ) ;
#30788 = CARTESIAN_POINT ( 'NONE',  ( 0.5577427821522314977, -0.3162353388693409650, -0.4822834645669289433 ) ) ;
#30789 = CARTESIAN_POINT ( 'NONE',  ( 0.9120734908136490793, 0.1771653543307087075, -0.09757992244046823083 ) ) ;
#30790 = CARTESIAN_POINT ( 'NONE',  ( -0.2559055118110227234, -0.5400638737290844871, 0.3530559997133364547 ) ) ;
#30791 = CARTESIAN_POINT ( 'NONE',  ( 4.893765752498283924E-17, -0.3996062992125986035, -1.023622047244094446 ) ) ;
#30792 = CARTESIAN_POINT ( 'NONE',  ( 1.515748031496063408, 0.1660481256975885056, 0.3530559997133364547 ) ) ;
#30793 = DIRECTION ( 'NONE',  ( 0.000000000000000000, 0.000000000000000000, 1.000000000000000000 ) ) ;
#30794 = CARTESIAN_POINT ( 'NONE',  ( -1.069553805774277722, -0.6692913385826773087, -0.1292274648535924053 ) ) ;
#30795 = CARTESIAN_POINT ( 'NONE',  ( -0.9514435695538050464, -0.3162353388693405765, 0.4822834645669290543 ) ) ;
#30796 = CARTESIAN_POINT ( 'NONE',  ( 0.4724409448818896462, 0.1265901696524990294, -0.2821522309711286258 ) ) ;
#30797 = EDGE_CURVE ( 'NONE', #49144, #45904, #22034, .T. ) ;
#30798 = CARTESIAN_POINT ( 'NONE',  ( -0.2891555358219908833, -0.2891555358219912164, -2.736220472440944462 ) ) ;
#30799 = ORIENTED_EDGE ( 'NONE', *, *, #22798, .F. ) ;
#30800 = CARTESIAN_POINT ( 'NONE',  ( 0.2165354330708668673, -0.4536011799217367080, 0.2665933059059888421 ) ) ;
#30801 = CARTESIAN_POINT ( 'NONE',  ( 0.3392501089628018329, 0.1958661417322835607, -1.383202099737532942 ) ) ;
#30802 = CARTESIAN_POINT ( 'NONE',  ( 0.6692913385826777528, 0.2952755905511811885, 0.000000000000000000 ) ) ;
#30803 = CARTESIAN_POINT ( 'NONE',  ( 0.2362204724409451007, -0.4091458600556402980, -2.296587926509186417 ) ) ;
#30804 = CARTESIAN_POINT ( 'NONE',  ( -0.4724409448818898682, -8.678599364036362592E-17, -0.9035433070866141225 ) ) ;
#30805 = CARTESIAN_POINT ( 'NONE',  ( -1.686351706036744558, 0.1771653543307087075, -0.09757992244046823083 ) ) ;
#30806 = CARTESIAN_POINT ( 'NONE',  ( 1.358267716535433323, 0.1660481256975885056, 0.3530559997133364547 ) ) ;
#30807 = CARTESIAN_POINT ( 'NONE',  ( 1.312335958005249825, 0.1283753931104746893, -0.1820866141732285504 ) ) ;
#30808 = CARTESIAN_POINT ( 'NONE',  ( 0.03937007874015833325, -0.6692913385826771977, 8.415575281601705876E-17 ) ) ;
#30809 = CARTESIAN_POINT ( 'NONE',  ( 0.3392501089628018329, 0.1958661417322835052, -0.5262274033782657900 ) ) ;
#30810 = CARTESIAN_POINT ( 'NONE',  ( -0.3477690288713902178, 0.2952755905511810774, -0.1292274648535930714 ) ) ;
#30811 = CARTESIAN_POINT ( 'NONE',  ( -1.410761154855642463, -0.08942795157527998196, 0.3641732283464567121 ) ) ;
#30812 = CARTESIAN_POINT ( 'NONE',  ( -0.2952755905511804668, 0.1660481256975885056, 0.3530559997133364547 ) ) ;
#30813 = CARTESIAN_POINT ( 'NONE',  ( 1.614173228346457378, 0.4410134679336836783, -0.1372047244094476148 ) ) ;
#30814 = CARTESIAN_POINT ( 'NONE',  ( -0.1654368116759051266, 1.092466590690397199, -1.877592342312344842 ) ) ;
#30815 = VERTEX_POINT ( 'NONE', #4925 ) ;
#30816 = CARTESIAN_POINT ( 'NONE',  ( -0.1958661417322833942, -0.3392501089628018884, -1.952119053314647523 ) ) ;
#30817 = CARTESIAN_POINT ( 'NONE',  ( 0.4527559055118117182, 0.1660481256975883668, -0.3530559997133364547 ) ) ;
#30818 = EDGE_LOOP ( 'NONE', ( #5972, #72766, #80360, #56148 ) ) ;
#30819 = CARTESIAN_POINT ( 'NONE',  ( -0.3740157480314953431, -0.5400638737290845981, -0.3530559997133363437 ) ) ;
#30820 = CARTESIAN_POINT ( 'NONE',  ( -1.574803149606298192, -0.1870078740157480879, -0.4822834645669291653 ) ) ;
#30821 = VECTOR ( 'NONE', #15239, 39.37007874015748143 ) ;
#30822 = CARTESIAN_POINT ( 'NONE',  ( 0.6627296587926515548, 0.2952755905511811885, 0.1292274648535926551 ) ) ;
#30823 = CARTESIAN_POINT ( 'NONE',  ( 8.195543980992789655E-16, -0.1870078740157480879, -0.4822834645669291653 ) ) ;
#30824 = CARTESIAN_POINT ( 'NONE',  ( -0.2867679344610364334, -0.2867679344610367109, -1.403543307086614123 ) ) ;
#30825 = CARTESIAN_POINT ( 'NONE',  ( -0.6758530183727028406, -0.6692913385826773087, -0.1292274648535924053 ) ) ;
#30826 = CARTESIAN_POINT ( 'NONE',  ( 0.3740157480314966754, -0.5400638737290844871, 0.3530559997133364547 ) ) ;
#30827 = CARTESIAN_POINT ( 'NONE',  ( -0.4986876640419939388, 0.2306618581243847221, -0.2411417322834647770 ) ) ;
#30828 = CARTESIAN_POINT ( 'NONE',  ( 0.5118110236220480003, -0.5511811023622047445, 6.969142054262312111E-17 ) ) ;
#30829 = CARTESIAN_POINT ( 'NONE',  ( -0.2896775404227472372, -0.05826908593210169962, 5.534257978450463966 ) ) ;
#30830 = CARTESIAN_POINT ( 'NONE',  ( -0.2952755905511804668, 0.1660481256975885056, 0.3530559997133364547 ) ) ;
#30831 = CARTESIAN_POINT ( 'NONE',  ( 3.908320185825792326, 1.553377289108603732, -0.4744094488188970171 ) ) ;
#30832 = CARTESIAN_POINT ( 'NONE',  ( 1.607611548556431069, 0.2952755905511811885, 0.1292274648535926551 ) ) ;
#30833 = CARTESIAN_POINT ( 'NONE',  ( -0.3392501089628019995, 0.1958661417322832277, -2.853018372703412187 ) ) ;
#30834 = VERTEX_POINT ( 'NONE', #28937 ) ;
#30835 = ORIENTED_EDGE ( 'NONE', *, *, #68572, .F. ) ;
#30836 = CARTESIAN_POINT ( 'NONE',  ( 0.7677165354330716118, 0.1660481256975883668, -0.3530559997133364547 ) ) ;
#30837 = CARTESIAN_POINT ( 'NONE',  ( 0.1049868766404206816, -0.5023911411419708095, -0.1820866141732282451 ) ) ;
#30839 = DIRECTION ( 'NONE',  ( 1.000000000000000000, 0.000000000000000000, -0.000000000000000000 ) ) ;
#30838 = CARTESIAN_POINT ( 'NONE',  ( 3.937007874015748143, 2.165354330708661568, -0.6299212598425196763 ) ) ;
#30840 = CARTESIAN_POINT ( 'NONE',  ( -0.3392501089628017219, -0.1958661417322836718, -1.082020997375328086 ) ) ;
#30841 = CARTESIAN_POINT ( 'NONE',  ( 0.000000000000000000, 2.755905511811024056, 0.000000000000000000 ) ) ;
#30842 = CARTESIAN_POINT ( 'NONE',  ( 0.6889763779527560139, 0.000000000000000000, 0.000000000000000000 ) ) ;
#30843 = CARTESIAN_POINT ( 'NONE',  ( -0.1974969037888706924, 0.3420746716998658843, 0.2250656167979003253 ) ) ;
#30844 = CARTESIAN_POINT ( 'NONE',  ( 0.4199475065616803948, -0.6046776061558809534, -0.2411417322834644161 ) ) ;
#30845 = CARTESIAN_POINT ( 'NONE',  ( -1.076115485564303809, -0.6046776061558809534, -0.2411417322834644161 ) ) ;
#30846 = CARTESIAN_POINT ( 'NONE',  ( -1.128608923884513837, -0.6046776061558807314, 0.2411417322834647770 ) ) ;
#30847 = CARTESIAN_POINT ( 'NONE',  ( 0.4068241469816279987, -0.4281496062992127816, -0.4176697321401328100 ) ) ;
#30848 = CARTESIAN_POINT ( 'NONE',  ( 1.076115485564305141, -0.6046776061558807314, 0.2411417322834647770 ) ) ;
#30849 = CARTESIAN_POINT ( 'NONE',  ( 1.213910761154856299, 0.1771653543307087630, 0.09757992244046791164 ) ) ;
#30850 = ITEM_DEFINED_TRANSFORMATION ( 'NONE', 'NONE', #10093,  #22098 ) ;
#30851 = CARTESIAN_POINT ( 'NONE',  ( 1.456692913385827515, -0.5511811023622047445, 6.969142054262312111E-17 ) ) ;
#30852 = CARTESIAN_POINT ( 'NONE',  ( -0.7808398950131222316, -0.3162353388693409650, -0.4822834645669289433 ) ) ;
#30853 = CARTESIAN_POINT ( 'NONE',  ( 0.2925321140481932369, -0.2925321140481931814, -0.4901574803149606474 ) ) ;
#30854 = CARTESIAN_POINT ( 'NONE',  ( 1.633858267716535639, -0.5400638737290844871, 0.3530559997133364547 ) ) ;
#30855 = CARTESIAN_POINT ( 'NONE',  ( -0.1958661417322836718, 0.3392501089628017219, -0.1627296587926508609 ) ) ;
#30856 = CARTESIAN_POINT ( 'NONE',  ( -0.3937007874015740483, -0.1870078740157479769, 0.4822834645669291653 ) ) ;
#30858 = CARTESIAN_POINT ( 'NONE',  ( 0.5314960629920997270, 2.755905511811024056, 2.503252890251021601 ) ) ;
#30857 = CARTESIAN_POINT ( 'NONE',  ( 0.9645669291338591078, -0.5400638737290845981, -0.3530559997133363437 ) ) ;
#30859 = CARTESIAN_POINT ( 'NONE',  ( -1.555118110236219930, 0.07958543189024085140, 0.2665933059059887866 ) ) ;
#30860 = CARTESIAN_POINT ( 'NONE',  ( 0.2427821522309719648, -0.05778040916215522460, 0.4822834645669289988 ) ) ;
#30861 = CARTESIAN_POINT ( 'NONE',  ( 0.7874015748031503170, -0.1870078740157479769, 0.3641732283464567677 ) ) ;
#30862 = CARTESIAN_POINT ( 'NONE',  ( -0.5314960629921124946, 2.716724272663528783, -3.890406373195416379 ) ) ;
#30863 = CARTESIAN_POINT ( 'NONE',  ( 1.036745406824147731, 0.05413385826771666132, 0.4176697321401328100 ) ) ;
#30864 = DIRECTION ( 'NONE',  ( 0.000000000000000000, 0.000000000000000000, -1.000000000000000000 ) ) ;
#30865 = CARTESIAN_POINT ( 'NONE',  ( -0.4068241469816267775, -0.004921259842519870586, -0.3153832671262229437 ) ) ;
#30866 = CARTESIAN_POINT ( 'NONE',  ( -0.4855643044619415427, -0.4281496062992124485, 0.4176697321401328655 ) ) ;
#30867 = CARTESIAN_POINT ( 'NONE',  ( -1.581364829396324945, -0.08942795157528024563, -0.3641732283464568787 ) ) ;
#30868 = CARTESIAN_POINT ( 'NONE',  ( -1.259842519685038686, -0.1870078740157479769, 0.4822834645669291653 ) ) ;
#30869 = CARTESIAN_POINT ( 'NONE',  ( 1.371391076115485941, 0.2952755905511811885, 0.1292274648535926551 ) ) ;
#30870 = CARTESIAN_POINT ( 'NONE',  ( -0.3917322834645671770, 0.1049643490035302024, -0.9744287646007369075 ) ) ;
#30871 = CARTESIAN_POINT ( 'NONE',  ( -1.502624671916009680, -0.2845877964562159024, 0.3641732283464567677 ) ) ;
#30872 = CARTESIAN_POINT ( 'NONE',  ( 1.109386689909465318, 1.093731576984011689, 0.1687003897380535689 ) ) ;
#30873 = CARTESIAN_POINT ( 'NONE',  ( 1.541994750656168645, -0.6692913385826771977, 0.1292274648535927661 ) ) ;
#30874 = CARTESIAN_POINT ( 'NONE',  ( -0.4091458600556405756, 0.2362204724409446288, -1.835301837270341352 ) ) ;
#30875 = CARTESIAN_POINT ( 'NONE',  ( 0.4713260495230639502, 1.475165172288837923, 3.908697958268506856 ) ) ;
#30876 = CARTESIAN_POINT ( 'NONE',  ( 1.692913385826772421, 0.2952755905511811885, 0.000000000000000000 ) ) ;
#30877 = CARTESIAN_POINT ( 'NONE',  ( -0.9186351706036736120, 0.1283753931104748280, 0.1820866141732283561 ) ) ;
#30878 = FACE_OUTER_BOUND ( 'NONE', #81230, .T. ) ;
#30879 = CARTESIAN_POINT ( 'NONE',  ( -0.2493438320209966919, -0.4281496062992124485, 0.4176697321401328655 ) ) ;
#30880 = CARTESIAN_POINT ( 'NONE',  ( 0.1312335958005257930, 0.1283753931104746893, -0.1820866141732285504 ) ) ;
#30881 = CARTESIAN_POINT ( 'NONE',  ( -1.049868766404198794, 0.1283753931104746893, -0.1820866141732285504 ) ) ;
#30882 = CARTESIAN_POINT ( 'NONE',  ( 1.469816272965879911, 0.1283753931104746893, -0.1820866141732285504 ) ) ;
#30883 = CARTESIAN_POINT ( 'NONE',  ( 0.9120734908136490793, 0.2952755905511810774, -0.1292274648535930714 ) ) ;
#30884 = CARTESIAN_POINT ( 'NONE',  ( -0.5314960629921372526, 2.716535433070866645, 3.224202737261813834 ) ) ;
#30885 = CARTESIAN_POINT ( 'NONE',  ( 0.3346456692913393205, -0.4536011799217368745, -0.2665933059059886201 ) ) ;
#30886 = CARTESIAN_POINT ( 'NONE',  ( 0.5905511811023629321, 0.2952755905511811885, 0.000000000000000000 ) ) ;
#30887 = CARTESIAN_POINT ( 'NONE',  ( 0.7939632545931766261, -0.08942795157527998196, 0.3641732283464567121 ) ) ;
#30888 = ORIENTED_EDGE ( 'NONE', *, *, #69043, .T. ) ;
#30889 = CARTESIAN_POINT ( 'NONE',  ( -1.017060367454067249, -0.05778040916215522460, 0.4822834645669289988 ) ) ;
#30890 = ADVANCED_FACE ( 'NONE', ( #43201 ), #42384, .F. ) ;
#30891 = CARTESIAN_POINT ( 'NONE',  ( -1.522309711286088607, -0.6046776061558807314, 0.2411417322834647770 ) ) ;
#30892 = CARTESIAN_POINT ( 'NONE',  ( -0.1443569553805768291, 0.05413385826771666132, 0.4176697321401328100 ) ) ;
#30893 = CARTESIAN_POINT ( 'NONE',  ( -1.725721784776902190, -0.08942795157527998196, 0.3641732283464567121 ) ) ;
#30894 = CARTESIAN_POINT ( 'NONE',  ( -0.1998031496062991630, -0.3460692066303959202, -2.504593175853018661 ) ) ;
#30895 = CARTESIAN_POINT ( 'NONE',  ( 0.4265091863517067039, -0.6692913385826773087, -0.1292274648535924053 ) ) ;
#30896 = CARTESIAN_POINT ( 'NONE',  ( 1.213910761154856299, -0.5511811023622048555, -0.09757992244046775898 ) ) ;
#30897 = CARTESIAN_POINT ( 'NONE',  ( 0.1509186351706045259, -0.05778040916215560624, -0.4822834645669293319 ) ) ;
#30898 = CARTESIAN_POINT ( 'NONE',  ( 0.4921259842519691285, 0.1660481256975885056, 0.3530559997133364547 ) ) ;
#30899 = CARTESIAN_POINT ( 'NONE',  ( 0.2925321140481932369, -0.2925321140481932369, -2.145669291338581974 ) ) ;
#30900 = CARTESIAN_POINT ( 'NONE',  ( 0.2891555358219910499, -0.2891555358219909944, -1.673228346456693272 ) ) ;
#30901 = CARTESIAN_POINT ( 'NONE',  ( -0.2925321140481932924, 0.2925321140481931814, -2.696850393700787052 ) ) ;
#30902 = CARTESIAN_POINT ( 'NONE',  ( 0.000000000000000000, 2.165354330708661568, 0.000000000000000000 ) ) ;
#30903 = CARTESIAN_POINT ( 'NONE',  ( 0.3392501089628018329, 0.1958661417322835607, -0.4383202099737532609 ) ) ;
#30904 = CARTESIAN_POINT ( 'NONE',  ( -0.5314960629921254842, -0.4536011799217368745, -0.2665933059059886201 ) ) ;
#30905 = CARTESIAN_POINT ( 'NONE',  ( -0.7611548556430438595, 0.2306618581243848609, 0.2411417322834645549 ) ) ;
#30906 = CARTESIAN_POINT ( 'NONE',  ( 0.6364829396325465405, -0.05778040916215522460, 0.4822834645669289988 ) ) ;
#30907 = CARTESIAN_POINT ( 'NONE',  ( -0.1974969037888706924, 0.3420746716998658843, -2.767060367454068803 ) ) ;
#30908 = CARTESIAN_POINT ( 'NONE',  ( 0.8333333333333340365, -0.6692913385826771977, 0.1292274648535927661 ) ) ;
#30909 = CARTESIAN_POINT ( 'NONE',  ( -1.633858267716534529, 0.1660481256975885056, 0.3530559997133364547 ) ) ;
#30910 = CARTESIAN_POINT ( 'NONE',  ( 0.8464566929133865436, 0.1660481256975883668, -0.3530559997133364547 ) ) ;
#30911 = DIRECTION ( 'NONE',  ( -0.000000000000000000, 1.000000000000000000, -0.000000000000000000 ) ) ;
#30912 = CARTESIAN_POINT ( 'NONE',  ( -0.1998031496062991907, -0.3460692066303959757, -2.270341207349081181 ) ) ;
#30913 = CARTESIAN_POINT ( 'NONE',  ( -2.583694225513480713, 2.755905511811024056, 0.5314960629921260393 ) ) ;
#30914 = CARTESIAN_POINT ( 'NONE',  ( 1.023622047244095112, -0.1870078740157480879, -0.4822834645669291653 ) ) ;
#30915 = CARTESIAN_POINT ( 'NONE',  ( 0.4068241469816279987, -0.4281496062992127816, -0.4176697321401328100 ) ) ;
#30916 = CARTESIAN_POINT ( 'NONE',  ( 1.325459317585302665, -0.004921259842519870586, -0.3153832671262229437 ) ) ;
#30918 = CARTESIAN_POINT ( 'NONE',  ( 1.299212598425197429, 0.2952755905511811885, 0.000000000000000000 ) ) ;
#30917 = CARTESIAN_POINT ( 'NONE',  ( 1.568241469816273659, -0.05778040916215560624, -0.4822834645669293319 ) ) ;
#30919 = CARTESIAN_POINT ( 'NONE',  ( 0.3917322834645669549, 0.1049643490035304660, -0.05183727034120744204 ) ) ;
#30920 = CARTESIAN_POINT ( 'NONE',  ( -0.4724409448818898682, -8.678599364036362592E-17, -0.9842519685039369248 ) ) ;
#30921 = CARTESIAN_POINT ( 'NONE',  ( 0.6561679790026253567, -0.6046776061558809534, -0.2411417322834644161 ) ) ;
#30922 = CARTESIAN_POINT ( 'NONE',  ( 1.528871391076116026, 0.1771653543307087630, 0.09757992244046791164 ) ) ;
#30923 = CARTESIAN_POINT ( 'NONE',  ( -0.3608923884514428360, -0.6692913385826773087, -0.1292274648535924053 ) ) ;
#30924 = CARTESIAN_POINT ( 'NONE',  ( -1.030183727034119867, -0.05778040916215560624, -0.4822834645669293319 ) ) ;
#30925 = CARTESIAN_POINT ( 'NONE',  ( 1.043307086614173818, -0.5400638737290845981, -0.3530559997133363437 ) ) ;
#30926 = CARTESIAN_POINT ( 'NONE',  ( 0.1958661417322834775, 0.3392501089628018884, -0.5439632545931759600 ) ) ;
#30927 = CARTESIAN_POINT ( 'NONE',  ( -9.594673741351313045E-17, 0.3917322834645670104, -1.566929133858267820 ) ) ;
#30928 = CARTESIAN_POINT ( 'NONE',  ( -0.3917322834645671215, 0.1049643490035301469, -2.544619422572177658 ) ) ;
#30929 = CARTESIAN_POINT ( 'NONE',  ( 1.581364829396326277, -0.3162353388693409650, -0.4822834645669289433 ) ) ;
#30930 = EDGE_LOOP ( 'NONE', ( #41583, #77964, #34652, #74847 ) ) ;
#30931 = CARTESIAN_POINT ( 'NONE',  ( 0.1058382717557500713, -0.3949938075777409408, -2.919947506561680228 ) ) ;
#30932 = EDGE_LOOP ( 'NONE', ( #44679, #8073, #77909, #71399 ) ) ;
#30933 = CARTESIAN_POINT ( 'NONE',  ( -1.595398199321656385, 1.585328674332965315, -0.1559797534342482472 ) ) ;
#30934 = CARTESIAN_POINT ( 'NONE',  ( 1.292650918635171564, 0.1771653543307087630, 0.09757992244046791164 ) ) ;
#30935 = CARTESIAN_POINT ( 'NONE',  ( -0.2925321140481932924, 0.2925321140481931814, -1.279527559055118058 ) ) ;
#30936 = CARTESIAN_POINT ( 'NONE',  ( 1.515748031496063408, 0.07958543189024085140, 0.2665933059059887866 ) ) ;
#30937 = CARTESIAN_POINT ( 'NONE',  ( -0.2362204724409447953, -0.4091458600556404646, -0.7723097112860892732 ) ) ;
#30938 = CARTESIAN_POINT ( 'NONE',  ( -0.5314960629921146040, 2.729657713787763118, -3.237502116108450956 ) ) ;
#30939 = CARTESIAN_POINT ( 'NONE',  ( -0.1637150164629772586, 1.933882213591592736, 0.2671902889294776595 ) ) ;
#30940 = CARTESIAN_POINT ( 'NONE',  ( -0.3917322834645669549, -0.1049643490035306603, -0.2880577427821523484 ) ) ;
#30941 = CARTESIAN_POINT ( 'NONE',  ( -0.8530183727034112984, -0.004921259842519576551, 0.3153832671262227771 ) ) ;
#30942 = CARTESIAN_POINT ( 'NONE',  ( -1.338582677165353729, -0.1870078740157480601, -0.3641732283464567677 ) ) ;
#30943 = CARTESIAN_POINT ( 'NONE',  ( -1.095800524934382292, -0.3162353388693409650, -0.4822834645669289433 ) ) ;
#30944 = CARTESIAN_POINT ( 'NONE',  ( -0.03280839895013062252, -0.6692913385826771977, 0.1292274648535927661 ) ) ;
#30945 = CARTESIAN_POINT ( 'NONE',  ( 1.561679790026247350, -0.4281496062992124485, 0.4176697321401328655 ) ) ;
#30946 = VERTEX_POINT ( 'NONE', #68083 ) ;
#30947 = CARTESIAN_POINT ( 'NONE',  ( 1.437007874015748810, 0.1660481256975885056, 0.3530559997133364547 ) ) ;
#30948 = DIRECTION ( 'NONE',  ( 0.000000000000000000, -0.000000000000000000, 1.000000000000000000 ) ) ;
#30949 = DIRECTION ( 'NONE',  ( 0.000000000000000000, 1.000000000000000000, 5.551115123125781470E-17 ) ) ;
#30950 = CARTESIAN_POINT ( 'NONE',  ( 0.3458507752293908943, 0.3458507752293908943, -2.185039370078739829 ) ) ;
#30951 = CARTESIAN_POINT ( 'NONE',  ( 1.614173228346457378, 1.055049524192302579, -0.1372047244094476148 ) ) ;
#30952 = CARTESIAN_POINT ( 'NONE',  ( -0.4461942257217840213, -0.5023911411419708095, -0.1820866141732282451 ) ) ;
#30953 = CARTESIAN_POINT ( 'NONE',  ( -1.115485564304461219, 0.05413385826771626580, -0.4176697321401330321 ) ) ;
#30954 = CARTESIAN_POINT ( 'NONE',  ( 0.9251968503937015864, 0.1660481256975883668, -0.3530559997133364547 ) ) ;
#30955 = ORIENTED_EDGE ( 'NONE', *, *, #69950, .T. ) ;
#30957 = CARTESIAN_POINT ( 'NONE',  ( -0.2726377952755906220, 0.000000000000000000, 0.07874015748031495954 ) ) ;
#30956 = CARTESIAN_POINT ( 'NONE',  ( -0.1265901696524986964, -0.4724409448818899238, -2.276902887139107268 ) ) ;
#30958 = FACE_OUTER_BOUND ( 'NONE', #17099, .T. ) ;
#30959 = CARTESIAN_POINT ( 'NONE',  ( -1.148293963254592542, -0.6692913385826773087, -0.1292274648535924053 ) ) ;
#30960 = CARTESIAN_POINT ( 'NONE',  ( -9.594673741351310580E-17, 0.3917322834645669549, -0.5524741225383709153 ) ) ;
#30961 = CARTESIAN_POINT ( 'NONE',  ( 0.01312335958005323398, -0.004921259842519576551, 0.3153832671262227771 ) ) ;
#30962 = CARTESIAN_POINT ( 'NONE',  ( 0.1958661417322834775, 0.3392501089628018884, -0.7014435695538058235 ) ) ;
#30963 = CARTESIAN_POINT ( 'NONE',  ( -0.6496062992125976043, 0.07958543189024071263, -0.2665933059059888421 ) ) ;
#30964 = CARTESIAN_POINT ( 'NONE',  ( 0.4855643044619428750, -0.004921259842519576551, 0.3153832671262227771 ) ) ;
#30965 = CARTESIAN_POINT ( 'NONE',  ( 0.6299212598425204535, -0.1870078740157479769, 0.4822834645669291653 ) ) ;
#30966 = CARTESIAN_POINT ( 'NONE',  ( -0.5708661417322825615, -0.4536011799217367080, 0.2665933059059888421 ) ) ;
#30967 = CARTESIAN_POINT ( 'NONE',  ( -0.3392501089628019995, 0.1958661417322832277, -2.695538057742782101 ) ) ;
#30968 = CARTESIAN_POINT ( 'NONE',  ( 1.213910761154856299, -0.6692913385826773087, -0.1292274648535924053 ) ) ;
#30969 = CARTESIAN_POINT ( 'NONE',  ( -0.8989501312335946848, -0.6692913385826771977, 0.1292274648535927661 ) ) ;
#30970 = CARTESIAN_POINT ( 'NONE',  ( -0.1265901696524993347, 0.4724409448818895907, -0.8707349081364830212 ) ) ;
#30971 = CARTESIAN_POINT ( 'NONE',  ( -0.1837270341207343505, -0.6046776061558807314, 0.2411417322834647770 ) ) ;
#30972 = CARTESIAN_POINT ( 'NONE',  ( -0.5446194225721777693, -0.05778040916215522460, 0.4822834645669289988 ) ) ;
#30973 = CARTESIAN_POINT ( 'NONE',  ( 1.443569553805774897, -0.5023911411419708095, -0.1820866141732282451 ) ) ;
#30974 = CARTESIAN_POINT ( 'NONE',  ( 0.01312335958005323398, -0.004921259842519576551, 0.3153832671262227771 ) ) ;
#30975 = CARTESIAN_POINT ( 'NONE',  ( -0.01312335958005186876, -0.4281496062992124485, 0.4176697321401328655 ) ) ;
#30976 = CARTESIAN_POINT ( 'NONE',  ( -1.246719160104985846, -0.4281496062992127816, -0.4176697321401328100 ) ) ;
#30977 = CARTESIAN_POINT ( 'NONE',  ( 1.614173228346457378, 1.055049524192302579, -0.1372047244094476148 ) ) ;
#30978 = CARTESIAN_POINT ( 'NONE',  ( 0.3458507752293908943, 0.3458507752293908943, -0.2952755905511810774 ) ) ;
#30979 = CARTESIAN_POINT ( 'NONE',  ( -0.2362204724409440182, -0.1870078740157479769, 0.4822834645669291653 ) ) ;
#30980 = CARTESIAN_POINT ( 'NONE',  ( -0.9711286089238838626, -0.6046776061558807314, 0.2411417322834647770 ) ) ;
#30981 = ORIENTED_EDGE ( 'NONE', *, *, #40285, .F. ) ;
#30982 = CARTESIAN_POINT ( 'NONE',  ( -0.1998031496062994405, 0.3460692066303957537, -2.137139107611548905 ) ) ;
#30983 = CARTESIAN_POINT ( 'NONE',  ( 0.9514435695538062676, -0.05778040916215522460, 0.4822834645669289988 ) ) ;
#30984 = CARTESIAN_POINT ( 'NONE',  ( -0.7939632545931754048, -0.2845877964562159024, 0.3641732283464567677 ) ) ;
#30985 = CARTESIAN_POINT ( 'NONE',  ( -0.7020997375328076329, -0.3162353388693409650, -0.4822834645669289433 ) ) ;
#30986 = CARTESIAN_POINT ( 'NONE',  ( 1.154855643044620184, -0.6046776061558807314, 0.2411417322834647770 ) ) ;
#30987 = CARTESIAN_POINT ( 'NONE',  ( 0.8136482939632553313, -0.6046776061558809534, -0.2411417322834644161 ) ) ;
#30988 = CARTESIAN_POINT ( 'NONE',  ( 1.594488188976378673, 0.1660481256975885056, 0.3530559997133364547 ) ) ;
#30989 = CARTESIAN_POINT ( 'NONE',  ( -0.9055118110236215490, 0.1771653543307087630, 0.000000000000000000 ) ) ;
#30990 = CARTESIAN_POINT ( 'NONE',  ( 0.3996062992125985480, -0.1070741851644052972, -0.6607611548556431291 ) ) ;
#30991 = CARTESIAN_POINT ( 'NONE',  ( -0.3996062992125987146, 0.1070741851644051862, -0.9776902887139107268 ) ) ;
#30992 = CARTESIAN_POINT ( 'NONE',  ( -0.1974969037888703871, -0.3420746716998661063, -0.2230971128608924547 ) ) ;
#30993 = CARTESIAN_POINT ( 'NONE',  ( 0.3443067643236821795, 1.210770866460127770, -1.397620821078814579 ) ) ;
#30994 = CARTESIAN_POINT ( 'NONE',  ( 0.9973753280839902091, -0.5023911411419708095, 0.1820866141732285504 ) ) ;
#30995 = CARTESIAN_POINT ( 'NONE',  ( 0.9055118110236227702, -0.5511811023622047445, 6.969142054262312111E-17 ) ) ;
#30996 = CIRCLE ( 'NONE', #80787, 0.1574803149606299746 ) ;
#30997 = CARTESIAN_POINT ( 'NONE',  ( 0.5774278215223103139, -0.6046776061558809534, -0.2411417322834644161 ) ) ;
#30998 = CARTESIAN_POINT ( 'NONE',  ( 0.2362204724409451007, -0.4091458600556402980, -2.373359580052493367 ) ) ;
#30999 = CARTESIAN_POINT ( 'NONE',  ( 0.2891555358219910499, 0.2891555358219910499, -1.159448818897637956 ) ) ;
#31000 = CARTESIAN_POINT ( 'NONE',  ( 0.7677165354330716118, 0.07958543189024071263, -0.2665933059059888421 ) ) ;
#31001 = CARTESIAN_POINT ( 'NONE',  ( -0.2952755905511803003, -0.5400638737290845981, -0.3530559997133363437 ) ) ;
#31002 = CARTESIAN_POINT ( 'NONE',  ( -1.200787401574802349, -0.5400638737290844871, 0.3530559997133364547 ) ) ;
#31003 = CARTESIAN_POINT ( 'NONE',  ( 1.410761154855643795, -0.05778040916215560624, -0.4822834645669293319 ) ) ;
#31004 = CARTESIAN_POINT ( 'NONE',  ( -0.4091458600556402980, -0.2362204724409451284, -1.784776902887138972 ) ) ;
#31005 = CARTESIAN_POINT ( 'NONE',  ( -0.1998031496062991907, -0.3460692066303959757, -2.742782152230971437 ) ) ;
#31006 = CARTESIAN_POINT ( 'NONE',  ( 0.006561679790026889343, -0.08942795157527998196, 0.3641732283464567121 ) ) ;
#31007 = ORIENTED_EDGE ( 'NONE', *, *, #3924, .F. ) ;
#31008 = ORIENTED_EDGE ( 'NONE', *, *, #29024, .T. ) ;
#31009 = CARTESIAN_POINT ( 'NONE',  ( -0.9514435695538050464, -0.3162353388693405765, 0.4822834645669290543 ) ) ;
#31010 = CARTESIAN_POINT ( 'NONE',  ( -0.4527559055118102749, -0.5400638737290845981, -0.3530559997133363437 ) ) ;
#31011 = CARTESIAN_POINT ( 'NONE',  ( -0.2296587926509179312, -0.05778040916215522460, 0.4822834645669289988 ) ) ;
#31012 = CARTESIAN_POINT ( 'NONE',  ( 0.5249343832021005074, -0.6046776061558807314, 0.2411417322834647770 ) ) ;
#31013 = CARTESIAN_POINT ( 'NONE',  ( -0.2952755905511803003, -0.5400638737290845981, -0.3530559997133363437 ) ) ;
#31014 = CARTESIAN_POINT ( 'NONE',  ( -1.332020997375327642, -0.05778040916215522460, 0.4822834645669289988 ) ) ;
#31015 = CIRCLE ( 'NONE', #68653, 1.122047244094488194 ) ;
#31016 = CARTESIAN_POINT ( 'NONE',  ( -0.9973753280839886548, -0.6046776061558809534, -0.2411417322834644161 ) ) ;
#31017 = CARTESIAN_POINT ( 'NONE',  ( 0.8923884514435701520, -0.6046776061558809534, -0.2411417322834644161 ) ) ;
#31018 = ADVANCED_FACE ( 'NONE', ( #73987 ), #45198, .F. ) ;
#31019 = EDGE_CURVE ( 'NONE', #73693, #81247, #16319, .T. ) ;
#31020 = CARTESIAN_POINT ( 'NONE',  ( -0.3917322834645671215, 0.1049643490035301469, -1.599737532808399143 ) ) ;
#31021 = CARTESIAN_POINT ( 'NONE',  ( -0.4593175853018364174, -0.3690944881889765550, -0.3153832671262227771 ) ) ;
#31022 = ORIENTED_EDGE ( 'NONE', *, *, #41175, .F. ) ;
#31023 = CARTESIAN_POINT ( 'NONE',  ( -0.2891555358219911054, 0.2891555358219909388, -1.279527559055118280 ) ) ;
#31024 = EDGE_LOOP ( 'NONE', ( #61366, #74352, #80749, #14533 ) ) ;
#31025 = CARTESIAN_POINT ( 'NONE',  ( -1.246719160104986512, -0.004921259842519576551, 0.3153832671262227771 ) ) ;
#31026 = CARTESIAN_POINT ( 'NONE',  ( -1.167979002624671470, 0.05413385826771666132, 0.4176697321401328100 ) ) ;
#31027 = CARTESIAN_POINT ( 'NONE',  ( -0.7152230971128602510, -0.3162353388693405765, 0.4822834645669290543 ) ) ;
#31028 = CARTESIAN_POINT ( 'NONE',  ( -0.1998031496062994683, 0.3460692066303958092, -0.01312335958005250193 ) ) ;
#31029 = CARTESIAN_POINT ( 'NONE',  ( -0.8398950131233589023, -0.6046776061558809534, -0.2411417322834644161 ) ) ;
#31030 = CARTESIAN_POINT ( 'NONE',  ( -0.8923884514435688198, 0.2306618581243847221, -0.2411417322834647770 ) ) ;
#31031 = CARTESIAN_POINT ( 'NONE',  ( -0.9881811337016640495, 0.000000000000000000, 0.5314960629921260393 ) ) ;
#31032 = CARTESIAN_POINT ( 'NONE',  ( -1.673228346456691717, 0.1660481256975883668, -0.3530559997133364547 ) ) ;
#31033 = CARTESIAN_POINT ( 'NONE',  ( 0.5118110236220480003, -0.5511811023622047445, 6.969142054262312111E-17 ) ) ;
#31034 = CARTESIAN_POINT ( 'NONE',  ( 1.614173228346457378, 0.9921945702958886448, -0.1372047244094476148 ) ) ;
#31035 = CARTESIAN_POINT ( 'NONE',  ( -0.3392501089628017219, -0.1958661417322836718, 0.02034120734908127781 ) ) ;
#31036 = CARTESIAN_POINT ( 'NONE',  ( -0.04593175853018302557, -0.5511811023622048555, -0.09757992244046775898 ) ) ;
#31037 = CARTESIAN_POINT ( 'NONE',  ( -0.3215223097112853146, -0.05778040916215560624, -0.4822834645669293319 ) ) ;
#31038 = CARTESIAN_POINT ( 'NONE',  ( 1.299212598425197429, 0.2952755905511811885, 0.000000000000000000 ) ) ;
#31039 = CARTESIAN_POINT ( 'NONE',  ( -0.1312335958005241554, -0.6046776061558809534, -0.2411417322834644161 ) ) ;
#31040 = VERTEX_POINT ( 'NONE', #44470 ) ;
#31041 = CARTESIAN_POINT ( 'NONE',  ( -0.2925321140481932924, 0.2925321140481931814, -2.066929133858267154 ) ) ;
#31042 = CARTESIAN_POINT ( 'NONE',  ( -0.8005249343832011588, 0.009842519685039147898, -0.3409548833797004797 ) ) ;
#31043 = ORIENTED_EDGE ( 'NONE', *, *, #34523, .F. ) ;
#31044 = CARTESIAN_POINT ( 'NONE',  ( -0.1998031496062994405, 0.3460692066303957537, -1.507217847769029007 ) ) ;
#31045 = CARTESIAN_POINT ( 'NONE',  ( 1.135170603674541256, 0.2952755905511811885, 0.1292274648535926551 ) ) ;
#31046 = CARTESIAN_POINT ( 'NONE',  ( -0.9908136482939626788, -0.5511811023622048555, -0.09757992244046775898 ) ) ;
#31047 = CARTESIAN_POINT ( 'NONE',  ( -1.227034120734907585, 0.2952755905511811885, 0.1292274648535926551 ) ) ;
#31048 = CARTESIAN_POINT ( 'NONE',  ( 0.2362204724409449064, 0.4091458600556404646, -0.9317585301837270073 ) ) ;
#31049 = CARTESIAN_POINT ( 'NONE',  ( -0.3133562546434896512, 1.179838254429707023, 3.924580492031178647 ) ) ;
#31050 = EDGE_CURVE ( 'NONE', #24575, #12831, #81992, .T. ) ;
#31051 = CARTESIAN_POINT ( 'NONE',  ( -0.3917322834645670104, -7.196005306013484475E-17, -2.801181102362204633 ) ) ;
#31052 = CARTESIAN_POINT ( 'NONE',  ( 1.148293963254593875, -0.6692913385826771977, 0.1292274648535927661 ) ) ;
#31053 = CARTESIAN_POINT ( 'NONE',  ( 0.6364829396325465405, -0.05778040916215522460, 0.4822834645669289988 ) ) ;
#31054 = CARTESIAN_POINT ( 'NONE',  ( 0.1443569553805781891, 0.05413385826771626580, -0.4176697321401330321 ) ) ;
#31055 = CARTESIAN_POINT ( 'NONE',  ( -1.102362204724408601, -0.1870078740157480601, -0.3641732283464567677 ) ) ;
#31056 = CARTESIAN_POINT ( 'NONE',  ( -0.1837270341207343505, -0.6046776061558807314, 0.2411417322834647770 ) ) ;
#31057 = CARTESIAN_POINT ( 'NONE',  ( -0.1998031496062991630, -0.3460692066303959202, 0.1725721784776902690 ) ) ;
#31058 = EDGE_CURVE ( 'NONE', #19641, #28871, #76790, .T. ) ;
#31059 = CARTESIAN_POINT ( 'NONE',  ( -0.7283464566929126471, 0.1660481256975883668, -0.3530559997133364547 ) ) ;
#31060 = CARTESIAN_POINT ( 'NONE',  ( 0.1058382717557500852, -0.3949938075777408852, -2.209317585301837639 ) ) ;
#31061 = CARTESIAN_POINT ( 'NONE',  ( 1.207349081364829990, -0.5023911411419708095, -0.1820866141732282451 ) ) ;
#31062 = CARTESIAN_POINT ( 'NONE',  ( -0.3280839895013117347, -0.3690944881889763329, 0.3153832671262228327 ) ) ;
#31063 = CARTESIAN_POINT ( 'NONE',  ( 1.076115485564305141, 0.1283753931104746893, -0.1820866141732285504 ) ) ;
#31064 = CARTESIAN_POINT ( 'NONE',  ( -1.601049868766403650, -0.6046776061558807314, 0.2411417322834647770 ) ) ;
#31065 = CARTESIAN_POINT ( 'NONE',  ( -1.135170603674539924, 0.1771653543307087075, -0.09757992244046823083 ) ) ;
#31066 = CARTESIAN_POINT ( 'NONE',  ( 0.6824146981627303710, -0.5023911411419708095, 0.1820866141732285504 ) ) ;
#31067 = CARTESIAN_POINT ( 'NONE',  ( -0.7020997375328074108, -0.05778040916215522460, 0.4822834645669289988 ) ) ;
#31068 = CARTESIAN_POINT ( 'NONE',  ( -1.894990545102987367, 1.111478976311921274, 0.2095522481616672039 ) ) ;
#31069 = CARTESIAN_POINT ( 'NONE',  ( 0.08530183727034192087, -0.08942795157527998196, 0.3641732283464567121 ) ) ;
#31070 = CARTESIAN_POINT ( 'NONE',  ( -1.594488188976377563, -0.4536011799217367080, 0.2665933059059888421 ) ) ;
#31071 =( BOUNDED_CURVE ( )  B_SPLINE_CURVE ( 2, ( #72961, #47689, #48108, #15312, #67071, #73806, #9403, #29170, #35487, #35073, #61151, #61575, #76277 ),
 .UNSPECIFIED., .F., .F. ) 
 B_SPLINE_CURVE_WITH_KNOTS ( ( 3, 2, 2, 2, 2, 2, 3 ),
 ( 0.3875000000000000111, 0.3916666666666666630, 0.3958333333333333148, 0.4000000000000000222, 0.4041666666666667296, 0.4083333333333333814, 0.4125000000000000333 ),
 .UNSPECIFIED. ) 
 CURVE ( )  GEOMETRIC_REPRESENTATION_ITEM ( )  RATIONAL_B_SPLINE_CURVE ( ( 1.000000000000000000, 0.9659258262890683122, 1.000000000000000000, 0.9659258262890683122, 1.000000000000000000, 0.9659258262890683122, 1.000000000000000000, 0.9659258262890683122, 1.000000000000000000, 0.9659258262890683122, 1.000000000000000000, 0.9659258262890678681, 1.000000000000000444 ) ) 
 REPRESENTATION_ITEM ( '' )  );
#31072 = CARTESIAN_POINT ( 'NONE',  ( 0.5971128608923891301, 0.2952755905511810774, -0.1292274648535930714 ) ) ;
#31073 = CARTESIAN_POINT ( 'NONE',  ( 0.6627296587926515548, 0.2952755905511811885, 0.1292274648535926551 ) ) ;
#31074 = CARTESIAN_POINT ( 'NONE',  ( 1.463254593175853824, 0.1771653543307087075, -0.09757992244046823083 ) ) ;
#31075 = CARTESIAN_POINT ( 'NONE',  ( -0.9711286089238838626, -0.6046776061558807314, 0.2411417322834647770 ) ) ;
#31076 = CARTESIAN_POINT ( 'NONE',  ( -0.1312335958005241554, -0.5023911411419708095, -0.1820866141732282451 ) ) ;
#31077 = CARTESIAN_POINT ( 'NONE',  ( 0.3307086614173228023, 0.3647102339900947787, 0.000000000000000000 ) ) ;
#31078 = CARTESIAN_POINT ( 'NONE',  ( 0.4199475065616803948, -0.5023911411419708095, -0.1820866141732282451 ) ) ;
#31079 = AXIS2_PLACEMENT_3D ( 'NONE', #67009, #42141, #9342 ) ;
#31080 = CARTESIAN_POINT ( 'NONE',  ( -1.233595800524933894, 0.2306618581243848609, 0.2411417322834645549 ) ) ;
#31081 = CARTESIAN_POINT ( 'NONE',  ( -0.3805774278215216522, 0.05413385826771666132, 0.4176697321401328100 ) ) ;
#31082 = CARTESIAN_POINT ( 'NONE',  ( -0.2925321140481932369, 0.2925321140481931259, -0.8838582677165351953 ) ) ;
#31083 = CARTESIAN_POINT ( 'NONE',  ( 0.3392501089628018329, 0.1958661417322835607, -2.105643044619422533 ) ) ;
#31084 = CARTESIAN_POINT ( 'NONE',  ( 0.5183727034120741983, 0.1771653543307087075, -0.09757992244046823083 ) ) ;
#31085 = CARTESIAN_POINT ( 'NONE',  ( -0.3018372703412066094, -0.4281496062992127816, -0.4176697321401328100 ) ) ;
#31086 = CARTESIAN_POINT ( 'NONE',  ( -0.8464566929133852113, 0.1660481256975885056, 0.3530559997133364547 ) ) ;
#31087 = CARTESIAN_POINT ( 'NONE',  ( -0.7480314960629914633, -0.5511811023622047445, 6.969142054262312111E-17 ) ) ;
#31088 = CARTESIAN_POINT ( 'NONE',  ( -3.918976913854863575, 1.248341192856212034, 0.3764949346671048747 ) ) ;
#31089 = CARTESIAN_POINT ( 'NONE',  ( -0.2230971128608915943, 0.05413385826771666132, 0.4176697321401328100 ) ) ;
#31090 = CARTESIAN_POINT ( 'NONE',  ( -1.666666666666665853, -0.004921259842519870586, -0.3153832671262229437 ) ) ;
#31091 = CARTESIAN_POINT ( 'NONE',  ( 1.581364829396326277, -0.05778040916215522460, 0.4822834645669289988 ) ) ;
#31092 = CARTESIAN_POINT ( 'NONE',  ( 0.01033912696139590269, 2.459406111854941508E-15, 0.4281989832122450323 ) ) ;
#31093 = ORIENTED_EDGE ( 'NONE', *, *, #75321, .T. ) ;
#31094 = LINE ( 'NONE', #56761, #18981 ) ;
#31095 = CARTESIAN_POINT ( 'NONE',  ( -1.482939632545930975, -0.4281496062992127816, -0.4176697321401328100 ) ) ;
#31096 = CARTESIAN_POINT ( 'NONE',  ( -0.7545931758530177724, 0.2952755905511811885, 0.1292274648535926551 ) ) ;
#31097 = EDGE_CURVE ( 'NONE', #949, #13300, #31865, .T. ) ;
#31098 = CARTESIAN_POINT ( 'NONE',  ( -1.404199475065615932, -0.4281496062992127816, -0.4176697321401328100 ) ) ;
#31099 = CARTESIAN_POINT ( 'NONE',  ( 0.1958661417322836440, -0.3392501089628017219, -1.908792650918635259 ) ) ;
#31100 = CYLINDRICAL_SURFACE ( 'NONE', #61975, 0.1771653543307085410 ) ;
#31101 = CARTESIAN_POINT ( 'NONE',  ( 0.8923884514435703741, 0.2306618581243848609, 0.2411417322834645549 ) ) ;
#31102 = CARTESIAN_POINT ( 'NONE',  ( 0.4855643044619430415, -0.4281496062992127816, -0.4176697321401328100 ) ) ;
#31103 = LINE ( 'NONE', #56770, #31526 ) ;
#31104 = LINE ( 'NONE', #76567, #3588 ) ;
#31105 = CARTESIAN_POINT ( 'NONE',  ( 1.076115485564305141, -0.5023911411419708095, 0.1820866141732285504 ) ) ;
#31106 = CARTESIAN_POINT ( 'NONE',  ( 0.1998031496062992740, 0.3460692066303959757, -0.9317585301837270073 ) ) ;
#31107 = ORIENTED_EDGE ( 'NONE', *, *, #15715, .F. ) ;
#31108 = CARTESIAN_POINT ( 'NONE',  ( -0.1958661417322834220, -0.3392501089628018884, -2.577427821522309426 ) ) ;
#31109 = ORIENTED_EDGE ( 'NONE', *, *, #68162, .F. ) ;
#31110 = CARTESIAN_POINT ( 'NONE',  ( 0.3149606299212603933, -0.1870078740157479769, 0.4822834645669291653 ) ) ;
#31111 = CARTESIAN_POINT ( 'NONE',  ( -0.8333333333333323711, -0.6692913385826773087, -0.1292274648535924053 ) ) ;
#31112 = CARTESIAN_POINT ( 'NONE',  ( -1.437007874015747477, 0.1660481256975883668, -0.3530559997133364547 ) ) ;
#31113 = CARTESIAN_POINT ( 'NONE',  ( 1.069553805774278832, 0.2952755905511810774, -0.1292274648535930714 ) ) ;
#31114 = CARTESIAN_POINT ( 'NONE',  ( 1.515748031496063408, 0.1660481256975885056, 0.3530559997133364547 ) ) ;
#31115 = CARTESIAN_POINT ( 'NONE',  ( 1.080276388343102000E-18, 2.290185943287373359E-17, 0.1771653543307086798 ) ) ;
#31116 = CARTESIAN_POINT ( 'NONE',  ( -0.2624671916010490880, -0.6046776061558807314, 0.2411417322834647770 ) ) ;
#31117 = CIRCLE ( 'NONE', #20383, 1.122047244094488194 ) ;
#31118 = CARTESIAN_POINT ( 'NONE',  ( -1.332020997375327642, -0.05778040916215522460, 0.4822834645669289988 ) ) ;
#31119 = CARTESIAN_POINT ( 'NONE',  ( -1.482939632545930975, 0.05413385826771666132, 0.4176697321401328100 ) ) ;
#31120 = CARTESIAN_POINT ( 'NONE',  ( 1.515748031496063408, 0.1660481256975885056, 0.3530559997133364547 ) ) ;
#31121 = CARTESIAN_POINT ( 'NONE',  ( -0.1049643490035307020, 0.3917322834645669549, 0.1587926509186352031 ) ) ;
#31122 = CARTESIAN_POINT ( 'NONE',  ( 0.8202099737532814183, -0.5511811023622048555, -0.09757992244046775898 ) ) ;
#31123 = ORIENTED_EDGE ( 'NONE', *, *, #1221, .F. ) ;
#31124 = CARTESIAN_POINT ( 'NONE',  ( -0.1974969037888706647, 0.3420746716998658843, -0.1706036745406825095 ) ) ;
#31125 = ORIENTED_EDGE ( 'NONE', *, *, #4265, .F. ) ;
#31126 = CARTESIAN_POINT ( 'NONE',  ( 0.02624671916010564918, 0.1283753931104748280, 0.1820866141732283561 ) ) ;
#31127 = CARTESIAN_POINT ( 'NONE',  ( 2.869680830158524820, 1.067671560069316294, -0.06860298820096749628 ) ) ;
#31128 = CARTESIAN_POINT ( 'NONE',  ( 0.4986876640419954376, 0.2306618581243848609, 0.2411417322834645549 ) ) ;
#31129 = CARTESIAN_POINT ( 'NONE',  ( 0.2559055118110243332, -0.5400638737290845981, -0.3530559997133363437 ) ) ;
#31130 = B_SPLINE_CURVE_WITH_KNOTS ( 'NONE', 3,
 ( #79325, #48968, #2710, #21644, #73420, #9436, #67932 ),
 .UNSPECIFIED., .F., .F.,
 ( 4, 3, 4 ),
 ( 1.734723475976806902E-18, 0.001246232571205225376, 0.002492492258783241162 ),
 .UNSPECIFIED. ) ;
#31131 = CARTESIAN_POINT ( 'NONE',  ( -0.7480314960629914633, 0.2952755905511811885, 0.000000000000000000 ) ) ;
#31132 = CARTESIAN_POINT ( 'NONE',  ( 0.1049643490035303967, 0.3917322834645670659, -1.722460260663728926 ) ) ;
#31133 = CARTESIAN_POINT ( 'NONE',  ( -1.253280839895012377, -0.3162353388693409650, -0.4822834645669289433 ) ) ;
#31134 = CARTESIAN_POINT ( 'NONE',  ( -0.2867679344610365999, 0.2867679344610364889, -2.624015748031495399 ) ) ;
#31135 = CARTESIAN_POINT ( 'NONE',  ( 1.174540682414699111, -0.08942795157528024563, -0.3641732283464568787 ) ) ;
#31136 = CARTESIAN_POINT ( 'NONE',  ( -1.318897637795274802, 0.1660481256975885056, 0.3530559997133364547 ) ) ;
#31137 = CARTESIAN_POINT ( 'NONE',  ( 0.8136482939632553313, -0.6046776061558809534, -0.2411417322834644161 ) ) ;
#31138 = CARTESIAN_POINT ( 'NONE',  ( 1.062992125984252745, 0.2952755905511811885, 0.000000000000000000 ) ) ;
#31139 = CARTESIAN_POINT ( 'NONE',  ( 0.3996062992125986035, 2.446882876249141962E-17, -0.9055118110236221041 ) ) ;
#31140 = CARTESIAN_POINT ( 'NONE',  ( -1.200787401574802349, 0.1660481256975883668, -0.3530559997133364547 ) ) ;
#31141 = CARTESIAN_POINT ( 'NONE',  ( 0.1998031496062992463, 0.3460692066303959202, -0.2211286089238845010 ) ) ;
#31142 = CARTESIAN_POINT ( 'NONE',  ( -0.2296587926509179312, -0.3162353388693409650, -0.4822834645669289433 ) ) ;
#31143 = CARTESIAN_POINT ( 'NONE',  ( 0.1998031496062992740, 0.3460692066303959757, -2.191601049868766360 ) ) ;
#31144 = ADVANCED_FACE ( 'NONE', ( #50795 ), #4539, .F. ) ;
#31145 = CARTESIAN_POINT ( 'NONE',  ( -0.1958661417322836718, 0.3392501089628017219, -1.830052493438320216 ) ) ;
#31146 = CARTESIAN_POINT ( 'NONE',  ( 1.437007874015748810, -0.5400638737290845981, -0.3530559997133363437 ) ) ;
#31147 = CARTESIAN_POINT ( 'NONE',  ( 0.3608923884514443348, -0.5511811023622046335, 0.09757992244046803654 ) ) ;
#31148 = CARTESIAN_POINT ( 'NONE',  ( 1.023622047244095112, -0.1870078740157480879, -0.4822834645669291653 ) ) ;
#31149 = CARTESIAN_POINT ( 'NONE',  ( -0.4091458600556405756, 0.2362204724409446288, -1.205380577427821454 ) ) ;
#31150 = CARTESIAN_POINT ( 'NONE',  ( 0.7480314960629927956, 0.1771653543307087630, 0.000000000000000000 ) ) ;
#31151 = CARTESIAN_POINT ( 'NONE',  ( 0.4921259842519691285, 0.1660481256975885056, 0.3530559997133364547 ) ) ;
#31152 = CARTESIAN_POINT ( 'NONE',  ( -0.1058382717557503072, 0.3949938075777408852, -1.185695538057742748 ) ) ;
#31153 = CARTESIAN_POINT ( 'NONE',  ( -0.9317585301837263412, 0.05413385826771666132, 0.4176697321401328100 ) ) ;
#31154 = B_SPLINE_CURVE_WITH_KNOTS ( 'NONE', 3,
 ( #46154, #77323, #39431, #6608 ),
 .UNSPECIFIED., .F., .F.,
 ( 4, 4 ),
 ( 3.593986969215047557E-07, 0.001287825409103288176 ),
 .UNSPECIFIED. ) ;
#31155 = PLANE ( 'NONE',  #78824 ) ;
#31156 = CARTESIAN_POINT ( 'NONE',  ( 0.8792650918635177559, -0.3690944881889765550, -0.3153832671262227771 ) ) ;
#31157 = CARTESIAN_POINT ( 'NONE',  ( 0.1681795077207355327, -2.839693391405754848E-15, 0.4118477457932995245 ) ) ;
#31158 = CARTESIAN_POINT ( 'NONE',  ( -0.2296587926509179312, -0.3162353388693409650, -0.4822834645669289433 ) ) ;
#31159 = CARTESIAN_POINT ( 'NONE',  ( -0.09186351706036663400, -0.3690944881889763329, 0.3153832671262228327 ) ) ;
#31160 = CARTESIAN_POINT ( 'NONE',  ( -2.610350574616450814, 1.379859446982315330, 0.4477348144951694420 ) ) ;
#31161 = CARTESIAN_POINT ( 'NONE',  ( -0.1246719160104980823, 0.2952755905511811885, 0.1292274648535926551 ) ) ;
#31162 = CARTESIAN_POINT ( 'NONE',  ( 0.9251968503937015864, -0.4536011799217367080, 0.2665933059059888421 ) ) ;
#31163 = CARTESIAN_POINT ( 'NONE',  ( -0.1070741851644056997, 0.3996062992125984925, -1.815616797900262425 ) ) ;
#31164 = CARTESIAN_POINT ( 'NONE',  ( 0.2887139107611556010, 0.2306618581243847221, -0.2411417322834647770 ) ) ;
#31165 = CARTESIAN_POINT ( 'NONE',  ( 1.358267716535433323, 0.07958543189024085140, 0.2665933059059887866 ) ) ;
#31166 = CARTESIAN_POINT ( 'NONE',  ( 1.614173228346456712, 1.267785121476991517, 0.1372047244094478646 ) ) ;
#31167 = CARTESIAN_POINT ( 'NONE',  ( -0.5118110236220466680, -0.5511811023622047445, 6.969142054262312111E-17 ) ) ;
#31168 = ADVANCED_FACE ( 'NONE', ( #44067 ), #44880, .F. ) ;
#31169 = CARTESIAN_POINT ( 'NONE',  ( -0.8070866141732276899, -0.4536011799217367080, 0.2665933059059888421 ) ) ;
#31170 = CARTESIAN_POINT ( 'NONE',  ( -0.1509186351706028884, -0.3162353388693409650, -0.4822834645669289433 ) ) ;
#31171 = CARTESIAN_POINT ( 'NONE',  ( 0.1706036745406830368, 0.05413385826771666132, 0.4176697321401328100 ) ) ;
#31172 = CARTESIAN_POINT ( 'NONE',  ( 0.8398950131233602345, -0.5023911411419708095, 0.1820866141732285504 ) ) ;
#31173 = DIRECTION ( 'NONE',  ( -0.000000000000000000, -1.000000000000000000, -0.000000000000000000 ) ) ;
#31174 = CARTESIAN_POINT ( 'NONE',  ( 1.528871391076116026, -0.5511811023622048555, -0.09757992244046775898 ) ) ;
#31175 = ADVANCED_FACE ( 'NONE', ( #76496 ), #43237, .F. ) ;
#31176 = AXIS2_PLACEMENT_3D ( 'NONE', #49731, #57273, #25290 ) ;
#31177 = CARTESIAN_POINT ( 'NONE',  ( 0.7808398950131241190, -0.05778040916215560624, -0.4822834645669293319 ) ) ;
#31178 = DIRECTION ( 'NONE',  ( 0.000000000000000000, 1.000000000000000000, 0.000000000000000000 ) ) ;
#31179 = CARTESIAN_POINT ( 'NONE',  ( -0.1049868766404193215, 0.2306618581243847221, -0.2411417322834647770 ) ) ;
#31180 = CARTESIAN_POINT ( 'NONE',  ( 0.1958661417322834775, 0.3392501089628018884, -1.173884514435695525 ) ) ;
#31181 = CARTESIAN_POINT ( 'NONE',  ( 1.023622047244095334, -0.1870078740157479769, 0.4822834645669291653 ) ) ;
#31182 = CARTESIAN_POINT ( 'NONE',  ( 0.4396325459317593221, 0.2952755905511810774, -0.1292274648535930714 ) ) ;
#31183 = B_SPLINE_CURVE_WITH_KNOTS ( 'NONE', 3,
 ( #901, #32444, #27384, #47151, #26967, #46321, #6772, #71175, #72014, #58106, #72432, #77493 ),
 .UNSPECIFIED., .F., .F.,
 ( 4, 2, 2, 2, 2, 4 ),
 ( 0.000000000000000000, 0.001328432419540427623, 0.002656864839080855245, 0.003985297258621282868, 0.004649513468391494944, 0.005313729678161706153 ),
 .UNSPECIFIED. ) ;
#31184 = FACE_OUTER_BOUND ( 'NONE', #45644, .T. ) ;
#31185 = CARTESIAN_POINT ( 'NONE',  ( 0.1968503937007881344, -0.5511811023622047445, 6.969142054262312111E-17 ) ) ;
#31186 = CARTESIAN_POINT ( 'NONE',  ( 1.161417322834646493, -0.5400638737290844871, 0.3530559997133364547 ) ) ;
#31187 = CARTESIAN_POINT ( 'NONE',  ( -0.2296587926509179312, -0.2845877964562161244, -0.3641732283464567121 ) ) ;
#31188 = CARTESIAN_POINT ( 'NONE',  ( -0.3018372703412066094, -0.4281496062992127816, -0.4176697321401328100 ) ) ;
#31189 = CARTESIAN_POINT ( 'NONE',  ( -1.220472440944881054, 2.401574803149606474, 0.5309055118110237448 ) ) ;
#31190 = CARTESIAN_POINT ( 'NONE',  ( 0.3740157480314966754, 0.1660481256975883668, -0.3530559997133364547 ) ) ;
#31191 = CARTESIAN_POINT ( 'NONE',  ( -0.9645669291338575535, 0.1660481256975883668, -0.3530559997133364547 ) ) ;
#31192 = CARTESIAN_POINT ( 'NONE',  ( -0.6627296587926503335, -0.5511811023622046335, 0.09757992244046803654 ) ) ;
#31193 = CARTESIAN_POINT ( 'NONE',  ( 0.2559055118110243332, -0.5400638737290845981, -0.3530559997133363437 ) ) ;
#31194 = CARTESIAN_POINT ( 'NONE',  ( -1.384514435695537005, 0.2952755905511811885, 0.1292274648535926551 ) ) ;
#31195 = CARTESIAN_POINT ( 'NONE',  ( -0.4724409448818890911, -0.1870078740157480879, -0.4822834645669291653 ) ) ;
#31196 =( BOUNDED_CURVE ( )  B_SPLINE_CURVE ( 2, ( #19364, #51748, #82931, #65248, #76617, #52587, #38304, #32404, #44595, #20203, #1278, #32826, #37891 ),
 .UNSPECIFIED., .F., .F. ) 
 B_SPLINE_CURVE_WITH_KNOTS ( ( 3, 2, 2, 2, 2, 2, 3 ),
 ( 0.5944878114796872115, 0.5946969696969697239, 0.5984848484848485084, 0.6022727272727272929, 0.6060606060606060774, 0.6098484848484848619, 0.6100576430657673743 ),
 .UNSPECIFIED. ) 
 CURVE ( )  GEOMETRIC_REPRESENTATION_ITEM ( )  RATIONAL_B_SPLINE_CURVE ( ( 0.9964447847208419695, 0.9981185001348091834, 1.000000000000000000, 0.9659258262890683122, 1.000000000000000000, 0.9659258262890683122, 1.000000000000000000, 0.9659258262890683122, 1.000000000000000000, 0.9659258262890683122, 1.000000000000000000, 0.9981185001348091834, 0.9964447847208420805 ) ) 
 REPRESENTATION_ITEM ( '' )  );
#31197 = CARTESIAN_POINT ( 'NONE',  ( -0.4724409448818898682, -8.678599364036362592E-17, -1.218503937007874072 ) ) ;
#31199 = CARTESIAN_POINT ( 'NONE',  ( 1.292650918635171564, 0.2952755905511811885, 0.1292274648535926551 ) ) ;
#31198 = CARTESIAN_POINT ( 'NONE',  ( 0.000000000000000000, 2.755905511811024056, 0.000000000000000000 ) ) ;
#31200 = CARTESIAN_POINT ( 'NONE',  ( 1.587926509186352586, -0.4281496062992127816, -0.4176697321401328100 ) ) ;
#31201 = CARTESIAN_POINT ( 'NONE',  ( -0.2867679344610364334, -0.2867679344610367109, -2.255905511811023612 ) ) ;
#31202 = DIRECTION ( 'NONE',  ( 0.000000000000000000, 0.000000000000000000, -1.000000000000000000 ) ) ;
#31203 = CARTESIAN_POINT ( 'NONE',  ( -0.7349081364829390672, 0.2306618581243847221, -0.2411417322834647770 ) ) ;
#31204 = CARTESIAN_POINT ( 'NONE',  ( -0.4091458600556405756, 0.2362204724409446288, -0.3412073490813647969 ) ) ;
#31205 = CARTESIAN_POINT ( 'NONE',  ( 0.1974969037888706369, -0.3420746716998659953, -2.926509186351706315 ) ) ;
#31206 = ORIENTED_EDGE ( 'NONE', *, *, #28480, .F. ) ;
#31207 = CARTESIAN_POINT ( 'NONE',  ( 0.3674540682414705883, -0.5023911411419708095, 0.1820866141732285504 ) ) ;
#31208 = CARTESIAN_POINT ( 'NONE',  ( 0.1049643490035303689, 0.3917322834645670104, -1.245406824146981561 ) ) ;
#31209 = CARTESIAN_POINT ( 'NONE',  ( 0.5971128608923890191, -0.6692913385826771977, 0.1292274648535927661 ) ) ;
#31210 = CARTESIAN_POINT ( 'NONE',  ( -0.4724409448818899238, 0.1265901696524986686, -2.709973753280840114 ) ) ;
#31211 = CARTESIAN_POINT ( 'NONE',  ( -0.5626772485143695102, -5.582469467804009507E-15, -0.3791483426435192650 ) ) ;
#31212 = CARTESIAN_POINT ( 'NONE',  ( -0.4002624671916004129, -0.2845877964562159024, 0.3641732283464567677 ) ) ;
#31213 = CARTESIAN_POINT ( 'NONE',  ( -0.2559055118110230564, 0.1660481256975883391, -0.3530559997133364547 ) ) ;
#31214 = CARTESIAN_POINT ( 'NONE',  ( 1.135170603674541256, -0.6692913385826773087, -0.1292274648535924053 ) ) ;
#31215 = CARTESIAN_POINT ( 'NONE',  ( 0.8136482939632553313, 0.1283753931104748280, 0.1820866141732283561 ) ) ;
#31216 = CARTESIAN_POINT ( 'NONE',  ( -0.09842519685039295696, -0.5400638737290844871, 0.3530559997133364547 ) ) ;
#31217 = CARTESIAN_POINT ( 'NONE',  ( 4.797336870675655290E-17, -0.3917322834645669549, -0.7886945949793155997 ) ) ;
#31218 = CARTESIAN_POINT ( 'NONE',  ( -0.3740157480314953431, 0.1660481256975885056, 0.3530559997133364547 ) ) ;
#31219 = CARTESIAN_POINT ( 'NONE',  ( -1.509186351706035767, -0.004921259842519870586, -0.3153832671262229437 ) ) ;
#31220 = CARTESIAN_POINT ( 'NONE',  ( -0.4658792650918627265, -0.05778040916215522460, 0.4822834645669289988 ) ) ;
#31221 = CARTESIAN_POINT ( 'NONE',  ( -1.595398199321656829, 1.034147571970760238, 0.1559797534342477754 ) ) ;
#31222 = FACE_OUTER_BOUND ( 'NONE', #15936, .T. ) ;
#31223 = ORIENTED_EDGE ( 'NONE', *, *, #16008, .T. ) ;
#31224 = CARTESIAN_POINT ( 'NONE',  ( -9.594673741351313045E-17, 0.3917322834645670659, -1.886502255414385099 ) ) ;
#31225 = CARTESIAN_POINT ( 'NONE',  ( 0.3740157480314966754, -0.5400638737290844871, 0.3530559997133364547 ) ) ;
#31226 = ORIENTED_EDGE ( 'NONE', *, *, #37675, .T. ) ;
#31227 = CARTESIAN_POINT ( 'NONE',  ( -0.4068241469816267775, 0.05413385826771626580, -0.4176697321401330321 ) ) ;
#31228 = CARTESIAN_POINT ( 'NONE',  ( -1.548556430446193399, -0.6046776061558809534, -0.2411417322834644161 ) ) ;
#31229 = CARTESIAN_POINT ( 'NONE',  ( 0.8202099737532813073, 0.2952755905511811885, 0.1292274648535926551 ) ) ;
#31230 = AXIS2_PLACEMENT_3D ( 'NONE', #45148, #69606, #70851 ) ;
#31231 = CARTESIAN_POINT ( 'NONE',  ( 0.1443569553805781891, 0.05413385826771626580, -0.4176697321401330321 ) ) ;
#31232 = CARTESIAN_POINT ( 'NONE',  ( -0.3917322834645671215, 0.1049643490035301469, -1.534776902887139194 ) ) ;
#31233 = CARTESIAN_POINT ( 'NONE',  ( -0.7283464566929126471, 0.1660481256975883668, -0.3530559997133364547 ) ) ;
#31234 = CARTESIAN_POINT ( 'NONE',  ( 0.2362204724409456558, -0.1870078740157479769, 0.4822834645669291653 ) ) ;
#31235 = CARTESIAN_POINT ( 'NONE',  ( -0.6430446194225712953, 0.05413385826771626580, -0.4176697321401330321 ) ) ;
#31236 = CARTESIAN_POINT ( 'NONE',  ( 0.2165354330708668673, -0.4536011799217367080, 0.2665933059059888421 ) ) ;
#31237 = CARTESIAN_POINT ( 'NONE',  ( -9.787531504996567848E-17, 0.3996062992125986035, -1.920830620545185230E-17 ) ) ;
#31238 = CARTESIAN_POINT ( 'NONE',  ( 0.04593175853018440641, 0.2952755905511810774, -0.1292274648535930714 ) ) ;
#31239 = CONICAL_SURFACE ( 'NONE', #37970, 2.401574803149606918, 0.6981317007977250189 ) ;
#31240 = DIRECTION ( 'NONE',  ( 0.000000000000000000, 0.000000000000000000, 1.000000000000000000 ) ) ;
#31241 = CARTESIAN_POINT ( 'NONE',  ( -1.653543307086613234, -0.1870078740157479769, 0.4822834645669291653 ) ) ;
#31242 = CARTESIAN_POINT ( 'NONE',  ( 0.2867679344610365999, 0.2867679344610365999, -2.649606299212598604 ) ) ;
#31243 = ORIENTED_EDGE ( 'NONE', *, *, #17348, .F. ) ;
#31244 = ORIENTED_EDGE ( 'NONE', *, *, #13149, .T. ) ;
#31245 = CARTESIAN_POINT ( 'NONE',  ( 0.4068241469816281097, 0.05413385826771666132, 0.4176697321401328100 ) ) ;
#31246 = CARTESIAN_POINT ( 'NONE',  ( -0.03280839895013062252, -0.5511811023622046335, 0.09757992244046803654 ) ) ;
#31248 = CARTESIAN_POINT ( 'NONE',  ( 0.000000000000000000, 0.000000000000000000, -0.01968503937007903132 ) ) ;
#31247 = CARTESIAN_POINT ( 'NONE',  ( 1.640419947506562393, -0.3690944881889763329, 0.3153832671262228327 ) ) ;
#31249 = CARTESIAN_POINT ( 'NONE',  ( 0.3392501089628018884, -0.1958661417322834220, -1.134514435695538115 ) ) ;
#31250 = DIRECTION ( 'NONE',  ( 0.000000000000000000, 1.000000000000000000, -0.000000000000000000 ) ) ;
#31251 = DIRECTION ( 'NONE',  ( -0.8660254037844432595, 0.000000000000000000, 0.4999999999999918954 ) ) ;
#31252 = CARTESIAN_POINT ( 'NONE',  ( -0.3996062992125985480, -7.340648628747423112E-17, -2.635826771653543066 ) ) ;
#31253 = CARTESIAN_POINT ( 'NONE',  ( 0.3543307086614179147, 0.2952755905511811885, 0.000000000000000000 ) ) ;
#31254 = CARTESIAN_POINT ( 'NONE',  ( -1.437007874015747477, 0.1660481256975883668, -0.3530559997133364547 ) ) ;
#31255 = CARTESIAN_POINT ( 'NONE',  ( -1.036745406824146176, 0.05413385826771626580, -0.4176697321401330321 ) ) ;
#31256 = CARTESIAN_POINT ( 'NONE',  ( 0.09186351706036799403, -0.4281496062992127816, -0.4176697321401328100 ) ) ;
#31257 = CARTESIAN_POINT ( 'NONE',  ( 0.8727034120734912248, -0.3162353388693409650, -0.4822834645669289433 ) ) ;
#31258 = CARTESIAN_POINT ( 'NONE',  ( 1.384514435695538559, 0.1771653543307087075, -0.09757992244046823083 ) ) ;
#31259 = ITEM_DEFINED_TRANSFORMATION ( 'NONE', 'NONE', #63832,  #22098 ) ;
#31260 = CARTESIAN_POINT ( 'NONE',  ( 0.7217847769028878924, -0.004921259842519576551, 0.3153832671262227771 ) ) ;
#31261 = CARTESIAN_POINT ( 'NONE',  ( -1.056430446194224881, -0.6692913385826771977, 0.1292274648535927661 ) ) ;
#31262 = CARTESIAN_POINT ( 'NONE',  ( 0.1998031496062994128, -0.3460692066303957537, -0.6410761154855643129 ) ) ;
#31263 = CARTESIAN_POINT ( 'NONE',  ( 1.476377952755906442, -0.5400638737290844871, 0.3530559997133364547 ) ) ;
#31264 = CARTESIAN_POINT ( 'NONE',  ( -0.3917322834645669549, -0.1049643490035306603, -0.1955380577427821009 ) ) ;
#31265 = VECTOR ( 'NONE', #82673, 39.37007874015748143 ) ;
#31267 = CARTESIAN_POINT ( 'NONE',  ( -0.2096960158929757345, 1.111548270248047476, 1.895053761512689894 ) ) ;
#31266 = CARTESIAN_POINT ( 'NONE',  ( 1.181102362204725198, -0.1870078740157479769, 0.4822834645669291653 ) ) ;
#31268 = CARTESIAN_POINT ( 'NONE',  ( -1.679790026246718693, 0.1283753931104746893, -0.1820866141732285504 ) ) ;
#31269 = CARTESIAN_POINT ( 'NONE',  ( 0.02624671916010564918, -0.6046776061558809534, -0.2411417322834644161 ) ) ;
#31270 = CARTESIAN_POINT ( 'NONE',  ( 0.6627296587926515548, 0.1771653543307087630, 0.09757992244046791164 ) ) ;
#31271 = EDGE_CURVE ( 'NONE', #59707, #23851, #20989, .T. ) ;
#31272 = CARTESIAN_POINT ( 'NONE',  ( -1.443569553805773564, -0.5023911411419708095, 0.1820866141732285504 ) ) ;
#31273 = CARTESIAN_POINT ( 'NONE',  ( 0.8923884514435703741, 0.2306618581243848609, 0.2411417322834645549 ) ) ;
#31274 = DIRECTION ( 'NONE',  ( -0.000000000000000000, -1.000000000000000000, -0.000000000000000000 ) ) ;
#31275 = CARTESIAN_POINT ( 'NONE',  ( -0.4330708661417315697, 0.1771653543307087630, 0.000000000000000000 ) ) ;
#31276 = CARTESIAN_POINT ( 'NONE',  ( -0.6889763779527552368, -0.5400638737290845981, -0.3530559997133363437 ) ) ;
#31277 = CARTESIAN_POINT ( 'NONE',  ( 1.410761154855643795, -0.05778040916215560624, -0.4822834645669293319 ) ) ;
#31278 = CARTESIAN_POINT ( 'NONE',  ( -1.181102362204723644, -0.1870078740157480879, -0.4822834645669291653 ) ) ;
#31279 = CARTESIAN_POINT ( 'NONE',  ( 1.555118110236221041, 0.1660481256975883668, -0.3530559997133364547 ) ) ;
#31280 = CARTESIAN_POINT ( 'NONE',  ( -0.3917322834645671770, 0.1049643490035302024, -0.8169484496401069329 ) ) ;
#31281 = CARTESIAN_POINT ( 'NONE',  ( -1.279527559055116948, 0.07958543189024071263, -0.2665933059059888421 ) ) ;
#31282 = CARTESIAN_POINT ( 'NONE',  ( 0.000000000000000000, 2.716535433070866645, 0.000000000000000000 ) ) ;
#31283 = CARTESIAN_POINT ( 'NONE',  ( 0.7939632545931766261, -0.05778040916215522460, 0.4822834645669289988 ) ) ;
#31284 = CARTESIAN_POINT ( 'NONE',  ( -0.4724409448818898682, -8.678599364036362592E-17, -2.478346456692913868 ) ) ;
#31285 = CARTESIAN_POINT ( 'NONE',  ( -1.587926509186350810, -0.4281496062992124485, 0.4176697321401328655 ) ) ;
#31286 = CARTESIAN_POINT ( 'NONE',  ( -1.535433070866141225, -0.5511811023622047445, 6.969142054262312111E-17 ) ) ;
#31287 = CARTESIAN_POINT ( 'NONE',  ( -1.023622047244094002, -0.1870078740157480601, -0.3641732283464567677 ) ) ;
#31288 = CARTESIAN_POINT ( 'NONE',  ( 1.528871391076116026, 0.1771653543307087630, 0.09757992244046791164 ) ) ;
#31289 = CARTESIAN_POINT ( 'NONE',  ( -0.5643044619422565855, -0.4281496062992124485, 0.4176697321401328655 ) ) ;
#31290 = CARTESIAN_POINT ( 'NONE',  ( -0.06561679790026180015, -0.004921259842519576551, 0.3153832671262227771 ) ) ;
#31291 = CARTESIAN_POINT ( 'NONE',  ( -1.555118110236219930, 0.07958543189024085140, 0.2665933059059887866 ) ) ;
#31292 = CARTESIAN_POINT ( 'NONE',  ( 1.286089238845145033, 0.1283753931104748280, 0.1820866141732283561 ) ) ;
#31293 = CIRCLE ( 'NONE', #71628, 0.3149606299212597826 ) ;
#31294 = CARTESIAN_POINT ( 'NONE',  ( 0.8464566929133866546, -0.5400638737290844871, 0.3530559997133364547 ) ) ;
#31295 = CARTESIAN_POINT ( 'NONE',  ( 1.574803149606299746, -0.1870078740157479769, 0.4822834645669291653 ) ) ;
#31296 = CARTESIAN_POINT ( 'NONE',  ( 0.01968503937007957949, -0.4536011799217368745, -0.2665933059059886201 ) ) ;
#31297 = CARTESIAN_POINT ( 'NONE',  ( 0.4527559055118117182, 0.1660481256975883668, -0.3530559997133364547 ) ) ;
#31298 = CARTESIAN_POINT ( 'NONE',  ( 1.102362204724410155, -0.1870078740157479769, 0.3641732283464567677 ) ) ;
#31299 = ORIENTED_EDGE ( 'NONE', *, *, #50451, .T. ) ;
#31300 = CARTESIAN_POINT ( 'NONE',  ( -1.515748031496062076, -0.5400638737290844871, 0.3530559997133364547 ) ) ;
#31301 = CARTESIAN_POINT ( 'NONE',  ( -1.207349081364828436, -0.6046776061558807314, 0.2411417322834647770 ) ) ;
#31302 = CARTESIAN_POINT ( 'NONE',  ( -0.09186351706036689768, 0.05413385826771626580, -0.4176697321401330321 ) ) ;
#31303 = CARTESIAN_POINT ( 'NONE',  ( -0.3460692066303958092, -0.1998031496062994683, -0.3674540682414698112 ) ) ;
#31304 = CARTESIAN_POINT ( 'NONE',  ( -0.3460692066303957537, -0.1998031496062994405, -2.806430446194225770 ) ) ;
#31305 = CARTESIAN_POINT ( 'NONE',  ( 0.3083989501312343062, -0.3162353388693405765, 0.4822834645669290543 ) ) ;
#31306 = CARTESIAN_POINT ( 'NONE',  ( 1.023622047244095112, -0.1870078740157480601, -0.3641732283464567677 ) ) ;
#31307 = CARTESIAN_POINT ( 'NONE',  ( 0.1443569553805781891, 0.05413385826771626580, -0.4176697321401330321 ) ) ;
#31308 = CARTESIAN_POINT ( 'NONE',  ( 0.4593175853018379162, -0.4281496062992124485, 0.4176697321401328655 ) ) ;
#31309 = CARTESIAN_POINT ( 'NONE',  ( 0.1070741851644053527, 0.3996062992125986590, -2.355643044619422533 ) ) ;
#31310 = CARTESIAN_POINT ( 'NONE',  ( 0.2891555358219910499, 0.2891555358219910499, -1.555118110236220375 ) ) ;
#31311 = CARTESIAN_POINT ( 'NONE',  ( 0.2925321140481932369, -0.2925321140481932369, -2.933070866141732402 ) ) ;
#31312 = CARTESIAN_POINT ( 'NONE',  ( 0.000000000000000000, 2.559055118110236560, 0.000000000000000000 ) ) ;
#31313 = CARTESIAN_POINT ( 'NONE',  ( -0.3917322834645670104, -7.196005306013484475E-17, -0.5039370078740157410 ) ) ;
#31314 = CARTESIAN_POINT ( 'NONE',  ( -0.6496062992125976043, -0.4536011799217367080, 0.2665933059059888421 ) ) ;
#31315 = CARTESIAN_POINT ( 'NONE',  ( -0.5839895013123351797, 0.2952755905511810774, -0.1292274648535930714 ) ) ;
#31316 = CARTESIAN_POINT ( 'NONE',  ( 4.837279021331061486E-17, -0.3949938075777409963, -2.675196850393700920 ) ) ;
#31317 = CARTESIAN_POINT ( 'NONE',  ( 0.7020997375328090762, -0.3162353388693405765, 0.4822834645669290543 ) ) ;
#31318 = CARTESIAN_POINT ( 'NONE',  ( -1.391076115485563314, -0.6046776061558809534, -0.2411417322834644161 ) ) ;
#31319 = CARTESIAN_POINT ( 'NONE',  ( 0.6692913385826777528, 0.2952755905511811885, 0.000000000000000000 ) ) ;
#31320 = CARTESIAN_POINT ( 'NONE',  ( 5.785732909357575061E-17, -0.4724409448818898682, -2.755905511811023612 ) ) ;
#31321 = CARTESIAN_POINT ( 'NONE',  ( -0.3996062992125987146, 0.1070741851644051862, -2.237532808398950301 ) ) ;
#31322 = DIRECTION ( 'NONE',  ( 0.000000000000000000, 0.000000000000000000, -1.000000000000000000 ) ) ;
#31323 = B_SPLINE_CURVE_WITH_KNOTS ( 'NONE', 3,
 ( #4447, #75577, #30933, #11184 ),
 .UNSPECIFIED., .F., .F.,
 ( 4, 4 ),
 ( 3.593986969189856268E-07, 0.001287825409103220521 ),
 .UNSPECIFIED. ) ;
#31324 = CARTESIAN_POINT ( 'NONE',  ( 1.076115485564305141, -0.6046776061558807314, 0.2411417322834647770 ) ) ;
#31325 = CARTESIAN_POINT ( 'NONE',  ( 0.6561679790026253567, 0.2306618581243848609, 0.2411417322834645549 ) ) ;
#31326 = CARTESIAN_POINT ( 'NONE',  ( 0.8923884514435701520, -0.5023911411419708095, -0.1820866141732282451 ) ) ;
#31327 = CARTESIAN_POINT ( 'NONE',  ( 1.259842519685040019, -0.1870078740157480879, -0.4822834645669291653 ) ) ;
#31328 = CARTESIAN_POINT ( 'NONE',  ( 0.2867679344610365999, 0.2867679344610365999, -0.2224409448818898127 ) ) ;
#31329 = PRESENTATION_STYLE_ASSIGNMENT (( #10351 ) ) ;
#31330 = CARTESIAN_POINT ( 'NONE',  ( 0.7020997375328090762, -0.3162353388693405765, 0.4822834645669290543 ) ) ;
#31331 = CARTESIAN_POINT ( 'NONE',  ( 1.692913385826772421, 0.1771653543307087630, 0.000000000000000000 ) ) ;
#31332 = CARTESIAN_POINT ( 'NONE',  ( -0.5314960629921254842, -0.5400638737290845981, -0.3530559997133363437 ) ) ;
#31333 = CARTESIAN_POINT ( 'NONE',  ( -1.174540682414697335, -0.3162353388693409650, -0.4822834645669289433 ) ) ;
#31334 = CARTESIAN_POINT ( 'NONE',  ( 1.115485564304462551, 0.05413385826771666132, 0.4176697321401328100 ) ) ;
#31335 = CARTESIAN_POINT ( 'NONE',  ( 0.3392501089628018329, 0.1958661417322835607, -0.3733595800524935338 ) ) ;
#31336 = CARTESIAN_POINT ( 'NONE',  ( -0.3392501089628017219, -0.1958661417322836718, -1.304461942257217899 ) ) ;
#31337 = CARTESIAN_POINT ( 'NONE',  ( 0.1049643490035303689, 0.3917322834645670104, -2.662729658792650778 ) ) ;
#31338 = ORIENTED_EDGE ( 'NONE', *, *, #64032, .F. ) ;
#31339 = CARTESIAN_POINT ( 'NONE',  ( 0.3949938075777409963, 2.418639510665530435E-17, -2.952755905511811108 ) ) ;
#31340 = ORIENTED_EDGE ( 'NONE', *, *, #35777, .F. ) ;
#31341 = CARTESIAN_POINT ( 'NONE',  ( -0.01968503937007793844, 0.1012011053420775880, -0.2882089793578256898 ) ) ;
#31342 = CARTESIAN_POINT ( 'NONE',  ( 1.502624671916010790, -0.2845877964562161244, -0.3641732283464567121 ) ) ;
#31343 = CARTESIAN_POINT ( 'NONE',  ( -0.3996062992125987146, 0.1070741851644051862, -1.450131233595800317 ) ) ;
#31344 = CARTESIAN_POINT ( 'NONE',  ( 1.351706036745407680, -0.004921259842519576551, 0.3153832671262227771 ) ) ;
#31345 = CARTESIAN_POINT ( 'NONE',  ( -0.7137454485294953965, 2.244094488188976388, 0.4917280318828573527 ) ) ;
#31346 = DIRECTION ( 'NONE',  ( 0.000000000000000000, 1.000000000000000000, 1.734723475976808327E-16 ) ) ;
#31347 = CARTESIAN_POINT ( 'NONE',  ( 0.5314960629921324786, 2.716535433070866645, -1.854472803289050509 ) ) ;
#31348 = CARTESIAN_POINT ( 'NONE',  ( -9.594673741351313045E-17, 0.3917322834645670104, -0.3996062992125985480 ) ) ;
#31349 = VECTOR ( 'NONE', #73680, 39.37007874015748143 ) ;
#31350 = CARTESIAN_POINT ( 'NONE',  ( -0.7545931758530176614, -0.5511811023622048555, -0.09757992244046775898 ) ) ;
#31351 = CARTESIAN_POINT ( 'NONE',  ( -1.509186351706035767, -0.004921259842519870586, -0.3153832671262229437 ) ) ;
#31352 = CARTESIAN_POINT ( 'NONE',  ( -1.279527559055116948, 0.1660481256975883668, -0.3530559997133364547 ) ) ;
#31353 = CARTESIAN_POINT ( 'NONE',  ( -0.01968503937007793844, -0.5400638737290844871, 0.3530559997133364547 ) ) ;
#31354 = CARTESIAN_POINT ( 'NONE',  ( -1.574803149606298192, -0.1870078740157480879, -0.4822834645669291653 ) ) ;
#31355 = EDGE_LOOP ( 'NONE', ( #30423, #78330, #7642, #28983 ) ) ;
#31356 = CARTESIAN_POINT ( 'NONE',  ( 1.489501312335958172, -0.05778040916215560624, -0.4822834645669293319 ) ) ;
#31357 = CYLINDRICAL_SURFACE ( 'NONE', #20562, 0.4744094488188972947 ) ;
#31358 = CARTESIAN_POINT ( 'NONE',  ( 3.941397919331622646, 3.481290980825508807, 4.414141470217288976 ) ) ;
#31359 = CARTESIAN_POINT ( 'NONE',  ( -0.4091458600556405756, 0.2362204724409446288, -2.230971128608923770 ) ) ;
#31360 = CARTESIAN_POINT ( 'NONE',  ( -1.559171609364246924, 0.000000000000000000, 0.4177787735906735578 ) ) ;
#31361 = CARTESIAN_POINT ( 'NONE',  ( -0.4199475065616791736, -0.5023911411419708095, 0.1820866141732285504 ) ) ;
#31362 = EDGE_CURVE ( 'NONE', #46245, #65458, #60203, .T. ) ;
#31363 = CARTESIAN_POINT ( 'NONE',  ( -1.043307086614172041, -0.5400638737290844871, 0.3530559997133364547 ) ) ;
#31364 = CARTESIAN_POINT ( 'NONE',  ( 1.187664041994751285, -0.05778040916215522460, 0.4822834645669289988 ) ) ;
#31365 = ORIENTED_EDGE ( 'NONE', *, *, #69234, .T. ) ;
#31367 = CARTESIAN_POINT ( 'NONE',  ( 0.4724409448818898127, -0.1265901696524988629, -2.708005249343832244 ) ) ;
#31366 = CARTESIAN_POINT ( 'NONE',  ( -0.4091458600556402980, -0.2362204724409451284, -2.257217847769029007 ) ) ;
#31368 = CARTESIAN_POINT ( 'NONE',  ( 1.423884514435696413, -0.3162353388693409650, -0.4822834645669289433 ) ) ;
#31369 = CARTESIAN_POINT ( 'NONE',  ( -1.187664041994750175, -0.05778040916215560624, -0.4822834645669293319 ) ) ;
#31370 = CARTESIAN_POINT ( 'NONE',  ( 4.797336870675655290E-17, -0.3917322834645669549, -0.3162536500974260090 ) ) ;
#31371 = EDGE_CURVE ( 'NONE', #4531, #38373, #23024, .T. ) ;
#31372 = CARTESIAN_POINT ( 'NONE',  ( -0.3280839895013117347, -0.3690944881889763329, 0.3153832671262228327 ) ) ;
#31373 = CARTESIAN_POINT ( 'NONE',  ( 0.3917322834645670104, 2.398668435337828261E-17, -0.9901574803149607584 ) ) ;
#31374 = CARTESIAN_POINT ( 'NONE',  ( -0.6430446194225712953, -0.004921259842519870586, -0.3153832671262229437 ) ) ;
#31375 = CARTESIAN_POINT ( 'NONE',  ( 0.6430446194225728496, -0.004921259842519576551, 0.3153832671262227771 ) ) ;
#31376 = CARTESIAN_POINT ( 'NONE',  ( 0.1181102362204730916, -0.6692913385826771977, 8.415575281601705876E-17 ) ) ;
#31377 = CARTESIAN_POINT ( 'NONE',  ( -0.5249343832020990641, 0.1283753931104748280, 0.1820866141732283561 ) ) ;
#31378 = CARTESIAN_POINT ( 'NONE',  ( 0.3392501089628018884, -0.1958661417322834220, -2.931758530183726563 ) ) ;
#31379 = CARTESIAN_POINT ( 'NONE',  ( 1.108923884514436242, -0.05778040916215522460, 0.4822834645669289988 ) ) ;
#31380 = CARTESIAN_POINT ( 'NONE',  ( -0.8661417322834640276, -0.1870078740157479769, 0.4822834645669291653 ) ) ;
#31381 = CARTESIAN_POINT ( 'NONE',  ( -0.4724409448818895907, -0.1265901696524993070, -1.382545931758530022 ) ) ;
#31382 = CARTESIAN_POINT ( 'NONE',  ( -0.3871391076115479057, -0.3162353388693409650, -0.4822834645669289433 ) ) ;
#31383 = CARTESIAN_POINT ( 'NONE',  ( -1.128608923884513837, 0.2306618581243847221, -0.2411417322834647770 ) ) ;
#31384 = CARTESIAN_POINT ( 'NONE',  ( 1.102362204724410155, -0.1870078740157480601, -0.3641732283464567677 ) ) ;
#31385 = CARTESIAN_POINT ( 'NONE',  ( -0.2362204724409442680, -0.1870078740157480601, -0.3641732283464567677 ) ) ;
#31386 = CARTESIAN_POINT ( 'NONE',  ( -0.6299212598425188991, -0.1870078740157479769, 0.4822834645669291653 ) ) ;
#31387 = CARTESIAN_POINT ( 'NONE',  ( -1.049868766404198794, -0.6046776061558807314, 0.2411417322834647770 ) ) ;
#31388 = CARTESIAN_POINT ( 'NONE',  ( -0.4037097067573596210, -2.567464376874931580E-15, -0.4445507791589072832 ) ) ;
#31389 = CARTESIAN_POINT ( 'NONE',  ( 1.108923884514436686, -0.2845877964562161244, -0.3641732283464567121 ) ) ;
#31390 = CONICAL_SURFACE ( 'NONE', #78472, 3.543307086614173596, 1.047197551196599408 ) ;
#31391 = CARTESIAN_POINT ( 'NONE',  ( -0.2296587926509179312, -0.05778040916215522460, 0.4822834645669289988 ) ) ;
#31392 = CARTESIAN_POINT ( 'NONE',  ( -1.017060367454067249, -0.3162353388693409650, -0.4822834645669289433 ) ) ;
#31393 = ORIENTED_EDGE ( 'NONE', *, *, #58860, .F. ) ;
#31394 = CARTESIAN_POINT ( 'NONE',  ( -0.1998031496062994405, 0.3460692066303957537, -2.452099737532808188 ) ) ;
#31395 = CARTESIAN_POINT ( 'NONE',  ( 1.076115485564305141, -0.6046776061558807314, 0.2411417322834647770 ) ) ;
#31396 = CARTESIAN_POINT ( 'NONE',  ( -0.7086614173228339419, -0.1870078740157480601, -0.3641732283464567677 ) ) ;
#31397 = CARTESIAN_POINT ( 'NONE',  ( 0.1070741851644054776, -0.3996062992125984925, -1.579396325459317740 ) ) ;
#31398 = CARTESIAN_POINT ( 'NONE',  ( -0.8792650918635160906, 0.05413385826771626580, -0.4176697321401330321 ) ) ;
#31399 = CARTESIAN_POINT ( 'NONE',  ( 1.482939632545932307, -0.4281496062992124485, 0.4176697321401328655 ) ) ;
#31400 = CARTESIAN_POINT ( 'NONE',  ( 0.8595800524934390507, -0.3162353388693405765, 0.4822834645669290543 ) ) ;
#31401 = DIRECTION ( 'NONE',  ( -0.000000000000000000, -1.000000000000000000, -0.000000000000000000 ) ) ;
#31402 = CARTESIAN_POINT ( 'NONE',  ( -0.9973753280839886548, -0.5023911411419708095, -0.1820866141732282451 ) ) ;
#31403 = CARTESIAN_POINT ( 'NONE',  ( -0.3460692066303957537, -0.1998031496062994405, -0.7591863517060367661 ) ) ;
#31404 = CARTESIAN_POINT ( 'NONE',  ( 0.3460692066303959757, -0.1998031496062991907, -0.8923884514435694859 ) ) ;
#31405 = AXIS2_PLACEMENT_3D ( 'NONE', #15536, #2899, #79935 ) ;
#31406 = CARTESIAN_POINT ( 'NONE',  ( -0.1058382717557497937, -0.3949938075777411628, -0.2296587926509187083 ) ) ;
#31407 = CARTESIAN_POINT ( 'NONE',  ( 0.03412294937773927700, 1.063915752041795670, 2.873159270261472553 ) ) ;
#31408 = CARTESIAN_POINT ( 'NONE',  ( 1.292650918635171564, -0.5511811023622048555, -0.09757992244046775898 ) ) ;
#31409 = CARTESIAN_POINT ( 'NONE',  ( 0.7874015748031503170, -0.1870078740157479769, 0.3641732283464567677 ) ) ;
#31410 = CARTESIAN_POINT ( 'NONE',  ( 0.4396325459317590445, -0.6692913385826771977, 0.1292274648535927661 ) ) ;
#31411 = CARTESIAN_POINT ( 'NONE',  ( 1.548556430446194954, -0.6046776061558807314, 0.2411417322834647770 ) ) ;
#31412 = CARTESIAN_POINT ( 'NONE',  ( -0.3420746716998660508, -0.1974969037888706924, -1.231627296587926468 ) ) ;
#31413 = CARTESIAN_POINT ( 'NONE',  ( 0.7414698162729663755, 0.1771653543307087630, 0.09757992244046791164 ) ) ;
#31414 = CARTESIAN_POINT ( 'NONE',  ( -0.4461942257217840213, -0.6046776061558809534, -0.2411417322834644161 ) ) ;
#31415 = CARTESIAN_POINT ( 'NONE',  ( -1.174540682414697335, -0.05778040916215522460, 0.4822834645669289988 ) ) ;
#31416 = CARTESIAN_POINT ( 'NONE',  ( 0.9317585301837276734, 0.05413385826771626580, -0.4176697321401330321 ) ) ;
#31417 = CARTESIAN_POINT ( 'NONE',  ( -0.2362204724409451284, 0.4091458600556402425, -1.587926509186351698 ) ) ;
#31418 = CARTESIAN_POINT ( 'NONE',  ( -0.7480314960629914633, 0.2952755905511811885, 0.000000000000000000 ) ) ;
#31419 = CARTESIAN_POINT ( 'NONE',  ( 0.1312335958005255154, -0.5023911411419708095, 0.1820866141732285504 ) ) ;
#31420 = VERTEX_POINT ( 'NONE', #18014 ) ;
#31421 = ORIENTED_EDGE ( 'NONE', *, *, #12583, .F. ) ;
#31422 = CARTESIAN_POINT ( 'NONE',  ( -0.7480314960629914633, 0.2952755905511811885, 0.000000000000000000 ) ) ;
#31423 = EDGE_CURVE ( 'NONE', #16468, #69029, #37359, .T. ) ;
#31424 = CARTESIAN_POINT ( 'NONE',  ( -0.6036745406824141069, -0.6046776061558809534, -0.2411417322834644161 ) ) ;
#31426 = CARTESIAN_POINT ( 'NONE',  ( -0.7217847769028863381, -0.4281496062992124485, 0.4176697321401328655 ) ) ;
#31425 = CARTESIAN_POINT ( 'NONE',  ( -0.9251968503937002541, -0.4536011799217368745, -0.2665933059059886201 ) ) ;
#31427 = CARTESIAN_POINT ( 'NONE',  ( 0.2559055118110243332, 0.1660481256975885056, 0.3530559997133364547 ) ) ;
#31428 = CARTESIAN_POINT ( 'NONE',  ( -0.3740157480314953431, 0.1660481256975885056, 0.3530559997133364547 ) ) ;
#31429 = CARTESIAN_POINT ( 'NONE',  ( -1.391076115485563314, -0.6046776061558809534, -0.2411417322834644161 ) ) ;
#31430 = CARTESIAN_POINT ( 'NONE',  ( -0.6102362204724400829, 0.1660481256975885056, 0.3530559997133364547 ) ) ;
#31431 = CARTESIAN_POINT ( 'NONE',  ( 0.8661417322834652488, -0.1870078740157480879, -0.4822834645669291653 ) ) ;
#31432 = CARTESIAN_POINT ( 'NONE',  ( 0.1958661417322834775, 0.3392501089628018884, -1.396325459317585338 ) ) ;
#31433 = CARTESIAN_POINT ( 'NONE',  ( -0.4986876640419939388, 0.1283753931104746893, -0.1820866141732285504 ) ) ;
#31434 = EDGE_LOOP ( 'NONE', ( #10528, #68909, #4909, #63947, #20579, #53699 ) ) ;
#31435 = CARTESIAN_POINT ( 'NONE',  ( -0.1058382717557497937, -0.3949938075777411628, -1.489501312335957950 ) ) ;
#31436 = ORIENTED_EDGE ( 'NONE', *, *, #22324, .F. ) ;
#31437 = CARTESIAN_POINT ( 'NONE',  ( -1.207349081364828880, 0.1283753931104746893, -0.1820866141732285504 ) ) ;
#31438 = CARTESIAN_POINT ( 'NONE',  ( -1.102362204724408601, -0.1870078740157480879, -0.4822834645669291653 ) ) ;
#31439 = CARTESIAN_POINT ( 'NONE',  ( -1.017060367454067249, -0.05778040916215522460, 0.4822834645669289988 ) ) ;
#31440 = CARTESIAN_POINT ( 'NONE',  ( 0.1998031496062992740, 0.3460692066303959757, -0.3018372703412073310 ) ) ;
#31441 = CARTESIAN_POINT ( 'NONE',  ( -0.9580052493438311334, -0.4281496062992124485, 0.4176697321401328655 ) ) ;
#31442 = CARTESIAN_POINT ( 'NONE',  ( -1.417322834645668772, -0.1870078740157479769, 0.4822834645669291653 ) ) ;
#31443 = CARTESIAN_POINT ( 'NONE',  ( -1.620734908136482577, 0.2952755905511811885, 0.1292274648535926551 ) ) ;
#31444 = CARTESIAN_POINT ( 'NONE',  ( 0.000000000000000000, 0.04921259842519689481, 0.08523872084492503665 ) ) ;
#31445 = CARTESIAN_POINT ( 'NONE',  ( 0.6299212598425204535, -0.1870078740157480601, -0.3641732283464567677 ) ) ;
#31446 = CARTESIAN_POINT ( 'NONE',  ( -0.3149606299212459048, 2.559055118110236560, -3.937007874015763242 ) ) ;
#31447 = CARTESIAN_POINT ( 'NONE',  ( -0.1958661417322836718, 0.3392501089628017219, -0.09776902887139117537 ) ) ;
#31448 = CARTESIAN_POINT ( 'NONE',  ( 0.1181102362204730916, -0.5511811023622047445, 6.969142054262312111E-17 ) ) ;
#31449 = CONICAL_SURFACE ( 'NONE', #24722, 0.09842519685039351207, 1.029744258676651647 ) ;
#31450 = CARTESIAN_POINT ( 'NONE',  ( -0.3083989501312330295, -0.3162353388693409650, -0.4822834645669289433 ) ) ;
#31451 = CARTESIAN_POINT ( 'NONE',  ( 1.194225721784777594, -0.4281496062992127816, -0.4176697321401328100 ) ) ;
#31452 = CARTESIAN_POINT ( 'NONE',  ( -0.5905511811023613777, -0.6692913385826771977, 8.415575281601705876E-17 ) ) ;
#31453 = VERTEX_POINT ( 'NONE', #58791 ) ;
#31454 = CARTESIAN_POINT ( 'NONE',  ( 0.1070741851644053527, 0.3996062992125986590, -2.198162729658792447 ) ) ;
#31455 = CARTESIAN_POINT ( 'NONE',  ( -1.614173228346456712, 2.401574803149606474, 0.1372047244094477536 ) ) ;
#31456 = ORIENTED_EDGE ( 'NONE', *, *, #47038, .F. ) ;
#31457 = CARTESIAN_POINT ( 'NONE',  ( 0.3996062992125985480, 2.446882876249141654E-17, -1.769685039370078927 ) ) ;
#31458 = CARTESIAN_POINT ( 'NONE',  ( -0.7283464566929126471, -0.5400638737290844871, 0.3530559997133364547 ) ) ;
#31459 = CARTESIAN_POINT ( 'NONE',  ( 1.397637795275591177, -0.5400638737290844871, 0.3530559997133364547 ) ) ;
#31460 = CARTESIAN_POINT ( 'NONE',  ( -0.9514435695538050464, -0.2845877964562159024, 0.3641732283464567677 ) ) ;
#31461 = CARTESIAN_POINT ( 'NONE',  ( -1.430446194225721390, -0.4281496062992124485, 0.4176697321401328655 ) ) ;
#31462 = CARTESIAN_POINT ( 'NONE',  ( -0.4091458600556402980, -0.2362204724409451284, -0.6824146981627295938 ) ) ;
#31463 = DIRECTION ( 'NONE',  ( 3.096699300667737957E-16, -1.000000000000000000, 0.000000000000000000 ) ) ;
#31464 = CARTESIAN_POINT ( 'NONE',  ( 0.1958661417322836440, -0.3392501089628017219, -0.08398950131233590133 ) ) ;
#31465 = CARTESIAN_POINT ( 'NONE',  ( 1.122047244094488860, -0.5400638737290845981, -0.3530559997133363437 ) ) ;
#31466 = CARTESIAN_POINT ( 'NONE',  ( 0.1958661417322834775, 0.3392501089628018884, -2.118766404199475151 ) ) ;
#31467 = CARTESIAN_POINT ( 'NONE',  ( 0.04593175853018440641, -0.6692913385826771977, 0.1292274648535927661 ) ) ;
#31468 = CARTESIAN_POINT ( 'NONE',  ( -0.9383202099737524282, -0.2845877964562161244, -0.3641732283464567121 ) ) ;
#31469 = CARTESIAN_POINT ( 'NONE',  ( -0.2690288713910754526, 0.2952755905511810774, -0.1292274648535930714 ) ) ;
#31470 = CARTESIAN_POINT ( 'NONE',  ( -0.4724409448818898682, -8.678599364036362592E-17, -2.635826771653543066 ) ) ;
#31471 = CARTESIAN_POINT ( 'NONE',  ( -0.9973753280839886548, -0.6046776061558809534, -0.2411417322834644161 ) ) ;
#31472 = CARTESIAN_POINT ( 'NONE',  ( -0.7611548556430438595, 0.2306618581243848609, 0.2411417322834645549 ) ) ;
#31473 = AXIS2_PLACEMENT_3D ( 'NONE', #69105, #69519, #18989 ) ;
#31474 = CARTESIAN_POINT ( 'NONE',  ( -0.3420746716998662729, 0.1974969037888702206, -2.307742782152230721 ) ) ;
#31475 = CARTESIAN_POINT ( 'NONE',  ( 0.6758530183727039509, 0.1771653543307087075, -0.09757992244046823083 ) ) ;
#31476 = CARTESIAN_POINT ( 'NONE',  ( -0.1377952755905504645, 0.07958543189024085140, 0.2665933059059887866 ) ) ;
#31477 = CARTESIAN_POINT ( 'NONE',  ( 0.7217847769028878924, -0.004921259842519576551, 0.3153832671262227771 ) ) ;
#31478 = CARTESIAN_POINT ( 'NONE',  ( -1.391076115485563758, 0.2306618581243848609, 0.2411417322834645549 ) ) ;
#31479 = CARTESIAN_POINT ( 'NONE',  ( 1.587926509186352142, 0.05413385826771666132, 0.4176697321401328100 ) ) ;
#31480 = CARTESIAN_POINT ( 'NONE',  ( 0.5380577427821529035, -0.3690944881889763329, 0.3153832671262228327 ) ) ;
#31481 = CARTESIAN_POINT ( 'NONE',  ( -0.8267716535433065062, 0.2952755905511811885, 0.000000000000000000 ) ) ;
#31482 = CARTESIAN_POINT ( 'NONE',  ( 1.318897637795276356, 0.1660481256975883668, -0.3530559997133364547 ) ) ;
#31483 = CARTESIAN_POINT ( 'NONE',  ( -1.863753233923699737, 1.077434660671937161, 0.1173752429317948681 ) ) ;
#31484 = CARTESIAN_POINT ( 'NONE',  ( -0.1443569553805765515, -0.3690944881889765550, -0.3153832671262227771 ) ) ;
#31485 = CARTESIAN_POINT ( 'NONE',  ( 0.06715429112991387617, 0.02791078216816508459, -0.4328096321851889194 ) ) ;
#31486 = CARTESIAN_POINT ( 'NONE',  ( 0.1706036745406830368, -0.4281496062992127816, -0.4176697321401328100 ) ) ;
#31487 = DIRECTION ( 'NONE',  ( 0.000000000000000000, 0.000000000000000000, 1.000000000000000000 ) ) ;
#31488 = CARTESIAN_POINT ( 'NONE',  ( 1.522309711286089939, -0.5023911411419708095, -0.1820866141732282451 ) ) ;
#31489 = CARTESIAN_POINT ( 'NONE',  ( 0.1509186351706042484, -0.2845877964562159024, 0.3641732283464567677 ) ) ;
#31490 = CARTESIAN_POINT ( 'NONE',  ( -1.476377952755905110, -0.5400638737290845981, -0.3530559997133363437 ) ) ;
#31491 = CARTESIAN_POINT ( 'NONE',  ( -0.1902887139107604098, 0.1771653543307087075, -0.09757992244046823083 ) ) ;
#31492 = CARTESIAN_POINT ( 'NONE',  ( 1.034719704380073102, 4.339766966676338660E-16, 0.3954985857520057491 ) ) ;
#31493 = CARTESIAN_POINT ( 'NONE',  ( -1.167979002624671470, -0.4281496062992127816, -0.4176697321401328100 ) ) ;
#31494 = EDGE_CURVE ( 'NONE', #11380, #71856, #46981, .T. ) ;
#31495 = CARTESIAN_POINT ( 'NONE',  ( -0.5183727034120726440, 0.2952755905511811885, 0.1292274648535926551 ) ) ;
#31496 = CARTESIAN_POINT ( 'NONE',  ( -0.3996062992125985480, -7.340648628747423112E-17, -0.7460629921259841479 ) ) ;
#31497 = EDGE_CURVE ( 'NONE', #5170, #9025, #37081, .T. ) ;
#31498 = CARTESIAN_POINT ( 'NONE',  ( 0.3917322834645669549, 0.1049643490035304660, -2.414041994750655729 ) ) ;
#31499 = CARTESIAN_POINT ( 'NONE',  ( 0.7742782152230978099, -0.3690944881889763329, 0.3153832671262228327 ) ) ;
#31500 = CARTESIAN_POINT ( 'NONE',  ( -0.5446194225721777693, -0.05778040916215522460, 0.4822834645669289988 ) ) ;
#31501 = CARTESIAN_POINT ( 'NONE',  ( -0.5708661417322825615, -0.5400638737290844871, 0.3530559997133364547 ) ) ;
#31502 = CARTESIAN_POINT ( 'NONE',  ( -0.8333333333333323711, 0.1771653543307087630, 0.09757992244046791164 ) ) ;
#31503 = LINE ( 'NONE', #12164, #46771 ) ;
#31504 = CARTESIAN_POINT ( 'NONE',  ( -0.2427821522309703550, -0.3162353388693405765, 0.4822834645669290543 ) ) ;
#31505 = CARTESIAN_POINT ( 'NONE',  ( -1.646981627296586703, -0.2845877964562161244, -0.3641732283464567121 ) ) ;
#31506 = CARTESIAN_POINT ( 'NONE',  ( 1.397637795275591177, -0.5400638737290844871, 0.3530559997133364547 ) ) ;
#31507 = CARTESIAN_POINT ( 'NONE',  ( 0.000000000000000000, 0.07874015748031502893, 0.000000000000000000 ) ) ;
#31508 = CARTESIAN_POINT ( 'NONE',  ( -0.3917322834645670104, -0.1049643490035307020, -2.247394643865828545 ) ) ;
#31509 = EDGE_LOOP ( 'NONE', ( #49142, #76909, #25116, #2367, #34287 ) ) ;
#31510 = AXIS2_PLACEMENT_3D ( 'NONE', #64477, #59827, #7237 ) ;
#31511 = DIRECTION ( 'NONE',  ( -0.000000000000000000, -1.000000000000000000, -0.000000000000000000 ) ) ;
#31512 = CARTESIAN_POINT ( 'NONE',  ( -1.272965879265091305, -0.4281496062992124485, 0.4176697321401328655 ) ) ;
#31513 = CARTESIAN_POINT ( 'NONE',  ( -0.8989501312335946848, 0.2952755905511810774, -0.1292274648535930714 ) ) ;
#31514 = EDGE_CURVE ( 'NONE', #17617, #79188, #77320, .T. ) ;
#31515 = CARTESIAN_POINT ( 'NONE',  ( -1.509186351706035767, -0.4281496062992124485, 0.4176697321401328655 ) ) ;
#31516 = CARTESIAN_POINT ( 'NONE',  ( -0.1958661417322834220, -0.3392501089628018884, -1.882545931758530244 ) ) ;
#31517 = DIRECTION ( 'NONE',  ( -0.000000000000000000, -1.000000000000000000, -0.000000000000000000 ) ) ;
#31518 = EDGE_CURVE ( 'NONE', #51195, #31040, #53897, .T. ) ;
#31519 = CARTESIAN_POINT ( 'NONE',  ( 0.7874015748031503170, -0.1870078740157480879, -0.4822834645669291653 ) ) ;
#31520 = CARTESIAN_POINT ( 'NONE',  ( 0.02624671916010564918, -0.6046776061558809534, -0.2411417322834644161 ) ) ;
#31521 = PLANE ( 'NONE',  #1935 ) ;
#31522 = PLANE ( 'NONE',  #19673 ) ;
#31523 = CARTESIAN_POINT ( 'NONE',  ( 1.371391076115485719, -0.5511811023622048555, -0.09757992244046775898 ) ) ;
#31524 = CARTESIAN_POINT ( 'NONE',  ( 0.1998031496062994405, -0.3460692066303958092, -1.509186351706036655 ) ) ;
#31525 = ORIENTED_EDGE ( 'NONE', *, *, #53883, .F. ) ;
#31527 = CARTESIAN_POINT ( 'NONE',  ( 0.1049643490035303689, 0.3917322834645670104, -2.505249343832020248 ) ) ;
#31526 = VECTOR ( 'NONE', #58012, 39.37007874015748143 ) ;
#31528 = VERTEX_POINT ( 'NONE', #723 ) ;
#31529 = CARTESIAN_POINT ( 'NONE',  ( 0.5643044619422579178, -0.4281496062992127816, -0.4176697321401328100 ) ) ;
#31530 = CARTESIAN_POINT ( 'NONE',  ( -0.7939632545931754048, -0.3162353388693405765, 0.4822834645669290543 ) ) ;
#31531 = CARTESIAN_POINT ( 'NONE',  ( -1.601049868766403650, 0.2306618581243847221, -0.2411417322834647770 ) ) ;
#31532 = CARTESIAN_POINT ( 'NONE',  ( 0.8202099737532814183, -0.6692913385826773087, -0.1292274648535924053 ) ) ;
#31533 = CARTESIAN_POINT ( 'NONE',  ( -1.614173228346455824, 0.1771653543307087630, 0.000000000000000000 ) ) ;
#31534 = CARTESIAN_POINT ( 'NONE',  ( 1.548556430446194954, -0.6046776061558807314, 0.2411417322834647770 ) ) ;
#31535 = CARTESIAN_POINT ( 'NONE',  ( -0.2559055118110227234, -0.5400638737290844871, 0.3530559997133364547 ) ) ;
#31536 = CARTESIAN_POINT ( 'NONE',  ( -1.056430446194224881, -0.6692913385826771977, 0.1292274648535927661 ) ) ;
#31537 = CARTESIAN_POINT ( 'NONE',  ( 1.568241469816273437, -0.3162353388693405765, 0.4822834645669290543 ) ) ;
#31538 = CARTESIAN_POINT ( 'NONE',  ( 1.522309711286089939, 0.2306618581243848609, 0.2411417322834645549 ) ) ;
#31539 = CARTESIAN_POINT ( 'NONE',  ( -9.594673741351313045E-17, 0.3917322834645670104, -0.3070866141732283006 ) ) ;
#31540 = CARTESIAN_POINT ( 'NONE',  ( 0.6889763779527566800, -0.4536011799217367080, 0.2665933059059888421 ) ) ;
#31541 = ORIENTED_EDGE ( 'NONE', *, *, #81099, .T. ) ;
#31542 = CARTESIAN_POINT ( 'NONE',  ( 0.1058382717557500713, -0.3949938075777409408, -0.2427821522309712154 ) ) ;
#31543 = ORIENTED_EDGE ( 'NONE', *, *, #67559, .F. ) ;
#31544 = CARTESIAN_POINT ( 'NONE',  ( -0.07217847769028813698, -0.2845877964562161244, -0.3641732283464567121 ) ) ;
#31545 = DIRECTION ( 'NONE',  ( 0.000000000000000000, 0.000000000000000000, 1.000000000000000000 ) ) ;
#31546 = CARTESIAN_POINT ( 'NONE',  ( 0.2493438320209980519, -0.4281496062992127816, -0.4176697321401328100 ) ) ;
#31547 = CARTESIAN_POINT ( 'NONE',  ( 0.6102362204724416372, -0.5400638737290844871, 0.3530559997133364547 ) ) ;
#31548 = CARTESIAN_POINT ( 'NONE',  ( -0.6496062992125976043, -0.5400638737290844871, 0.3530559997133364547 ) ) ;
#31549 = CARTESIAN_POINT ( 'NONE',  ( 0.2867679344610366554, -0.2867679344610365999, -1.512486507382889256 ) ) ;
#31550 = CARTESIAN_POINT ( 'NONE',  ( -1.299212598425196097, 0.2952755905511811885, 0.000000000000000000 ) ) ;
#31551 = CARTESIAN_POINT ( 'NONE',  ( -0.3917322834645670104, -7.196005306013484475E-17, -2.486220472440944906 ) ) ;
#31552 = CARTESIAN_POINT ( 'NONE',  ( 1.167979002624672580, -0.004921259842519870586, -0.3153832671262229437 ) ) ;
#31553 = CARTESIAN_POINT ( 'NONE',  ( 0.9186351706036752773, 0.2306618581243847221, -0.2411417322834647770 ) ) ;
#31554 = CARTESIAN_POINT ( 'NONE',  ( 0.6955380577427828781, -0.4281496062992124485, 0.4176697321401328655 ) ) ;
#31555 = CARTESIAN_POINT ( 'NONE',  ( -0.1998031496062991907, -0.3460692066303959757, -0.6955380577427822120 ) ) ;
#31556 = CARTESIAN_POINT ( 'NONE',  ( -1.272965879265091305, -0.4281496062992124485, 0.4176697321401328655 ) ) ;
#31557 = CARTESIAN_POINT ( 'NONE',  ( 0.3996062992125985480, 2.446882876249141654E-17, -0.5098425196850393526 ) ) ;
#31558 = CARTESIAN_POINT ( 'NONE',  ( -0.2925321140481930149, -0.2925321140481933480, -0.1358267716535433156 ) ) ;
#31559 = CARTESIAN_POINT ( 'NONE',  ( -0.3280839895013117347, -0.4281496062992124485, 0.4176697321401328655 ) ) ;
#31560 = CARTESIAN_POINT ( 'NONE',  ( 0.3996062992125986035, 0.1070741851644054776, -2.801837270341207553 ) ) ;
#31561 = CARTESIAN_POINT ( 'NONE',  ( 0.1049643490035303689, 0.3917322834645670104, -1.810367454068241511 ) ) ;
#31562 = CARTESIAN_POINT ( 'NONE',  ( 1.082677165354331228, -0.5400638737290844871, 0.3530559997133364547 ) ) ;
#31563 = CARTESIAN_POINT ( 'NONE',  ( 1.325459317585302665, -0.4281496062992124485, 0.4176697321401328655 ) ) ;
#31564 = CARTESIAN_POINT ( 'NONE',  ( 0.3346456692913393205, -0.4536011799217368745, -0.2665933059059886201 ) ) ;
#31565 = CARTESIAN_POINT ( 'NONE',  ( 0.6955380577427828781, 0.05413385826771626580, -0.4176697321401330321 ) ) ;
#31566 = CARTESIAN_POINT ( 'NONE',  ( -0.3458507752293909498, 0.3458507752293907833, -1.513779527559054872 ) ) ;
#31567 = CARTESIAN_POINT ( 'NONE',  ( 0.3477690288713918276, -0.5511811023622048555, -0.09757992244046775898 ) ) ;
#31568 =( BOUNDED_SURFACE ( )  B_SPLINE_SURFACE ( 1, 2, ( 
 ( #70129, #12480, #56666, #5339, #57490, #63816, #37731, #82366, #4508, #5740, #31411, #30176, #75227, #24685, #50352, #76465, #18791, #6574, #25925, #58327, #689, #46117, #20880, #71811, #33506, #72232, #77285, #45692, #14162, #33086, #12900, #70973, #51583, #32245, #46947, #45278, #14581, #19616, #26345, #78555, #32660, #13318, #7839, #53262, #38559, #8254, #20464, #1940, #1526, #58753, #65917, #40234, #46532, #38971, #64654, #6992, #33918, #13738, #78131, #59168, #59583, #27602, #52006, #27180, #78973, #52844, #21294, #64239, #57905, #270, #77711, #20041, #71389, #7416, #52421, #39394, #65078, #1115, #26766, #39818, #65507, #9909, #47781, #9496, #53675, #28846, #22945, #23357, #34339, #8668, #2359, #9089, #15406, #16654, #54927, #73483, #55335, #73056, #47365, #29673, #72639, #16236, #74307, #35998, #79383, #48201, #21702, #73896, #41066, #29263, #66755, #34761, #41884, #14988, #79806, #60421, #81044, #40646, #61668, #67577, #22538, #4009, #35581, #66330, #60004, #22122, #15833, #67166, #3182, #61244, #28015, #80634, #42294, #54508, #3598, #2772, #28432, #54091, #41481, #35169, #60830, #80222, #48613, #67991, #10336, #81455, #55747, #23772, #64450, #30906, #50260, #38773, #49443, #75137, #32458, #11571, #13122, #75958, #17482, #24592, #6786, #487, #5242, #37230, #43113, #26142, #30502, #17888, #49849, #19417, #56165, #45068, #4416, #68809, #19843, #70771, #51803, #42710, #81868, #24180, #77508, #71189, #17073, #11156, #64871, #58120, #32881, #68406, #62078, #36814, #62490, #82274, #45492, #13531, #39187, #7211, #30085, #75548, #58550, #69223, #49028, #4824, #43525, #10746, #916, #62907, #74724, #56573, #36403, #8880, #46334, #33314, #21506, #66967, #52226, #21920, #34138, #15624, #15204, #72446, #79604, #53890, #34556, #26981, #60222, #2153, #66131, #8468, #1332, #8060, #7644, #52646, #78350, #60633, #2572, #40452, #33721, #72027, #47582, #27820, #59383, #78770, #59799, #21094, #41281, #45909, #73276, #9300, #34970, #26573, #72856, #20682, #1741, #40865, #77929, #28231, #53058, #14795, #46753, #27398, #66547, #71606, #20260, #53480, #79190, #40041, #13959, #39616, #65305, #58976, #47164, #14383, #65727, #16869, #48822, #67794, #41684, #61462, #29877, #75339, #49647, #17686, #23564, #9711, #67377, #74522, #48406, #29060, #3397, #42097, #22339, #35382, #80020, #10946, #62281, #36603, #43316, #69014, #4619, #30290, #23153, #3810, #55956, #81669, #4213, #42506, #2984, #55539, #68208, #47999, #11366, #37023, #28649, #49235, #61047, #54731, #10545, #74106, #80436, #22746, #10131, #73698, #16452, #16038, #23979, #54309, #35795, #29472, #55130, #80840, #36203, #61872, #81249, #74938, #17283, #42911, #68606, #62704, #18902, #82888, #56375, #82074, #69432, #13019, #76574, #64351, #24387, #75753, #56778, #82478, #50874, #57606, #44552, #12597, #25619, #43728, #18503, #70242, #63523, #5043, #37438, #18094, #50058, #30712, #76166, #11785, #24794, #31530, #6688, #5853, #44146, #44967, #63112, #31111, #5450, #38673, #50462, #69838, #12188, #37845, #57186, #25208, #70663, #38256, #63933, #6269, #31945, #83297, #51282, #76985, #19314, #57154, #12155, #37812, #65484, #1502, #11752, #63080, #71782, #63488, #44520, #1090, #7816, #27154, #43695, #58727, #59144, #52396, #78529, #26742, #20853, #72205, #33482, #52818, #69400, #82853, #18871, #82041, #24355, #50023, #5822, #39789, #14137, #78105, #31493, #25174, #37408, #70208, #46505, #14558, #75722, #18062, #5418, #82445, #31080, #62670, #46090, #44115, #50843, #76543, #7389, #69807, #20436, #56747, #24762, #13712, #39366, #65051, #33056, #5010, #30680, #56341, #50430, #76130, #18472, #48175, #41040, #22094, #60803, #41858, #61217, #21267, #35141, #35554, #28820, #54903, #3157, #80609, #48586, #67550, #9885, #46922, #34734, #79778, #59558, #1913, #27576, #66725, #16211, #73871, #54485, #15378, #60394, #72615, #47755, #3572, #74283, #53233, #78949, #14963, #59975, #66303, #29239, #22514, #9062, #22919, #40620, #8642, #40210, #65893, #67138, #8228, #33892, #34314, #15803, #2334, #41454, #27990, #80196, #53650, #79358 ),
 ( #2745, #28405, #54063, #21677, #47338, #73028, #73453, #9467, #17864, #16627, #82654, #67966, #74701, #75113, #5626, #81019, #17046, #42686, #68384, #49002, #23332, #10723, #30882, #81845, #43499, #5218, #36380, #62054, #82250, #62464, #62883, #69197, #4392, #75525, #56549, #50235, #56140, #4799, #30060, #75931, #24568, #17459, #24156, #37202, #18272, #37611, #55721, #11546, #11956, #43912, #31292, #69610, #56957, #24969, #63286, #50641, #81431, #11130, #49825, #35974, #61644, #3985, #43089, #42269, #10308, #29649, #68786, #36788, #23746, #55311, #49419, #30476, #38023, #12365, #6038, #12781, #19080, #20339, #58629, #77166, #59053, #76750, #51049, #33391, #76345, #19926, #78011, #39696, #83065, #51888, #25386, #77592, #44728, #32962, #70425, #38438, #45576, #27063, #148, #64121, #1407, #18675, #65387, #71269, #26224, #7722, #13616, #44320, #70010, #25803, #51464, #70855, #6870, #39270, #63699, #997, #45991, #32539, #64952, #31710, #57370, #6456, #32126, #19498, #57784, #45152, #13206, #38853, #64533, #58203, #571, #7292, #26651, #52305, #71687, #14039, #59466, #53137, #35043, #15284, #15702, #79682, #21175, #28307, #41359, #3057, #8962, #40945, #78848, #28724, #34216, #21581, #53558, #21998, #59879, #47659, #8136, #46830, #79266, #66624, #27897, #47244, #2233, #72933, #54386, #73775, #1817, #72522, #22416, #34636, #53969, #52722, #35454, #20761, #27479, #60300, #41755, #33801, #14871, #40532, #66211, #8549, #2650, #73354, #67040, #9372, #60708, #80097, #48073, #16111, #67450, #9784, #61120, #3471, #78433, #46411, #72105, #14463, #40115, #65803, #55207, #5116, #10621, #81326, #29951, #56034, #36277, #24052, #67868, #80915, #55615, #17358, #4289, #23640, #61949, #49310, #30783, #50128, #61541, #29545, #37097, #75012, #11023, #49722, #56445, #75828, #10206, #75419, #24463, #17762, #43802, #43393, #69506, #37508, #82147, #18169, #35874, #42987, #68681, #48481, #74182, #16529, #36680, #11855, #62782, #69093, #62355, #4693, #3885, #30367, #63183, #29138, #42173, #23228, #48898, #74600, #16943, #54804, #11441, #81742, #80508, #42585, #68285, #22823, #5522, #32434, #7185, #52201, #12261, #64428, #37919, #6762, #5931, #45468, #31602, #63595, #58097, #39590, #12674, #57262, #71582, #31187, #77905, #462, #38751, #20236, #26118, #45884, #13933, #38334, #64009, #43, #19394, #51780, #56852, #71166, #58525, #69907, #25696, #45045, #24868, #50536, #76240, #32021, #64847, #13506, #77484, #6350, #51357, #82961, #70746, #39162, #82549, #18574, #44217, #25279, #50947, #76644, #32856, #891, #57681, #18975, #44624, #70320, #77060, #13098, #19819, #26548, #28627, #72005, #40839, #14361, #66524, #65706, #21895, #8035, #40018, #34534, #16018, #72422, #33699, #47977, #65279, #54284, #60199, #15182, #80000, #8856, #22314, #73677, #14772, #40427, #59775, #79166, #2550, #7618, #47558, #34949, #21483, #28208, #33291, #58951, #1309, #59359, #66108, #26958, #46311, #1718, #27373, #53034, #78747, #21072, #46730, #79580, #47142, #53867, #73251, #8444, #34114, #15600, #27798, #41260, #66946, #2130, #9278, #60612, #2961, #72832, #53458, #52622, #78327, #20658, #10524, #42481, #68584, #23133, #36582, #80413, #67770, #68185, #29855, #16846, #36179, #74499, #61851, #43295, #62680, #74083, #42075, #49624, #4192, #23542, #62261, #68992, #5022, #22725, #4597, #37001, #30268, #56353, #55932, #82052, #50035, #11342, #75317, #74916, #81647, #17664, #48384, #55518, #17261, #81226, #41664, #16429, #10107, #61022, #75732, #35770, #30690, #54707, #3787, #23956, #61440, #29451, #24365, #67355, #9688, #35359, #49211, #3372, #29036, #42890, #55109, #80818, #48801, #10925, #363, #76963, #57584, #83275, #76142, #12166, #7086, #63910, #52098, #18072, #51678, #31923, #25186, #37823, #13410, #19292, #50853, #70219, #51261, #12575, #32757, #37418, #64748, #58424, #39065, #785, #64329, #18483, #76553, #32337, #69410, #77381, #44530, #6246, #38232, #82864, #57999, #63091, #11764, #44943, #25598, #31505, #26445, #5429, #31090, #56757, #70640, #69817, #26019, #12996, #38652, #18881, #82457, #6665, #19712 ) ),
 .UNSPECIFIED., .F., .F., .F. ) 
 B_SPLINE_SURFACE_WITH_KNOTS ( ( 2, 2 ),
 ( 3, 2, 2, 2, 2, 2, 2, 2, 2, 2, 2, 2, 2, 2, 2, 2, 2, 2, 2, 2, 2, 2, 2, 2, 2, 2, 2, 2, 2, 2, 2, 2, 2, 2, 2, 2, 2, 2, 2, 2, 2, 2, 2, 2, 2, 2, 2, 2, 2, 2, 2, 2, 2, 2, 2, 2, 2, 2, 2, 2, 2, 2, 2, 2, 2, 2, 2, 2, 2, 2, 2, 2, 2, 2, 2, 2, 2, 2, 2, 2, 2, 2, 2, 2, 2, 2, 2, 2, 2, 2, 2, 2, 2, 2, 2, 2, 2, 2, 2, 2, 2, 2, 2, 2, 2, 2, 2, 2, 2, 2, 2, 2, 2, 2, 2, 2, 2, 2, 2, 2, 2, 2, 2, 2, 2, 2, 2, 2, 2, 2, 2, 2, 2, 2, 2, 2, 2, 2, 2, 2, 2, 2, 2, 2, 2, 2, 2, 2, 2, 2, 2, 2, 2, 2, 2, 2, 2, 2, 2, 2, 2, 2, 2, 2, 2, 2, 2, 2, 2, 2, 2, 2, 2, 2, 2, 2, 2, 2, 2, 2, 2, 2, 2, 2, 2, 2, 2, 2, 2, 2, 2, 2, 2, 2, 2, 2, 2, 2, 2, 2, 2, 2, 2, 2, 2, 2, 2, 2, 2, 2, 2, 2, 2, 2, 2, 2, 2, 2, 2, 2, 2, 2, 2, 2, 2, 2, 2, 2, 2, 2, 2, 2, 2, 2, 2, 2, 2, 2, 2, 2, 2, 2, 2, 2, 2, 2, 2, 2, 2, 2, 2, 2, 2, 2, 2, 3 ),
 ( 0.000000000000000000, 1.000000000000000000 ),
 ( 0.000000000000000000, 0.003787878787878787984, 0.007575757575757575968, 0.01136363636363636395, 0.01515151515151515194, 0.01893939393939393992, 0.02272727272727272790, 0.02651515151515151589, 0.03030303030303030387, 0.03409090909090908839, 0.03787878787878787984, 0.04166666666666666435, 0.04545454545454545581, 0.04924242424242424032, 0.05303030303030303177, 0.05681818181818181629, 0.06060606060606060774, 0.06439393939393939226, 0.06818181818181817677, 0.07196969696969697516, 0.07575757575757575968, 0.07954545454545454419, 0.08333333333333332871, 0.08712121212121212710, 0.09090909090909091161, 0.09469696969696969613, 0.09848484848484848064, 0.1022727272727272790, 0.1060606060606060635, 0.1098484848484848481, 0.1136363636363636326, 0.1174242424242424310, 0.1212121212121212155, 0.1250000000000000000, 0.1287878787878787845, 0.1325757575757575690, 0.1363636363636363535, 0.1401515151515151381, 0.1439393939393939503, 0.1477272727272727348, 0.1515151515151515194, 0.1553030303030303039, 0.1590909090909090884, 0.1628787878787878729, 0.1666666666666666574, 0.1704545454545454419, 0.1742424242424242542, 0.1780303030303030387, 0.1818181818181818232, 0.1856060606060606077, 0.1893939393939393923, 0.1931818181818181768, 0.1969696969696969613, 0.2007575757575757458, 0.2045454545454545581, 0.2083333333333333426, 0.2121212121212121271, 0.2159090909090909116, 0.2196969696969696961, 0.2234848484848484806, 0.2272727272727272652, 0.2310606060606060497, 0.2348484848484848619, 0.2386363636363636465, 0.2424242424242424310, 0.2462121212121212155, 0.2500000000000000000, 0.2537878787878787845, 0.2575757575757575690, 0.2613636363636363535, 0.2651515151515151381, 0.2689393939393939226, 0.2727272727272727071, 0.2765151515151514916, 0.2803030303030302761, 0.2840909090909091161, 0.2878787878787879007, 0.2916666666666666852, 0.2954545454545454697, 0.2992424242424242542, 0.3030303030303030387, 0.3068181818181818232, 0.3106060606060606077, 0.3143939393939393923, 0.3181818181818181768, 0.3219696969696969613, 0.3257575757575757458, 0.3295454545454545303, 0.3333333333333333148, 0.3371212121212120993, 0.3409090909090908839, 0.3446969696969697239, 0.3484848484848485084, 0.3522727272727272929, 0.3560606060606060774, 0.3598484848484848619, 0.3636363636363636465, 0.3674242424242424310, 0.3712121212121212155, 0.3750000000000000000, 0.3787878787878787845, 0.3825757575757575690, 0.3863636363636363535, 0.3901515151515151381, 0.3939393939393939226, 0.3977272727272727071, 0.4015151515151514916, 0.4053030303030302761, 0.4090909090909091161, 0.4128787878787879007, 0.4166666666666666852, 0.4204545454545454697, 0.4242424242424242542, 0.4280303030303030387, 0.4318181818181818232, 0.4356060606060606077, 0.4393939393939393923, 0.4431818181818181768, 0.4469696969696969613, 0.4507575757575757458, 0.4545454545454545303, 0.4583333333333333148, 0.4621212121212120993, 0.4659090909090908839, 0.4696969696969697239, 0.4734848484848485084, 0.4772727272727272929, 0.4810606060606060774, 0.4848484848484848619, 0.4886363636363636465, 0.4924242424242424310, 0.4962121212121212155, 0.5000000000000000000, 0.5037878787878787845, 0.5075757575757575690, 0.5113636363636363535, 0.5151515151515151381, 0.5189393939393939226, 0.5227272727272727071, 0.5265151515151514916, 0.5303030303030302761, 0.5340909090909090606, 0.5378787878787878451, 0.5416666666666666297, 0.5454545454545454142, 0.5492424242424241987, 0.5530303030303029832, 0.5568181818181817677, 0.5606060606060605522, 0.5643939393939394478, 0.5681818181818182323, 0.5719696969696970168, 0.5757575757575758013, 0.5795454545454545858, 0.5833333333333333703, 0.5871212121212121549, 0.5909090909090909394, 0.5946969696969697239, 0.5984848484848485084, 0.6022727272727272929, 0.6060606060606060774, 0.6098484848484848619, 0.6136363636363636465, 0.6174242424242424310, 0.6212121212121212155, 0.6250000000000000000, 0.6287878787878787845, 0.6325757575757575690, 0.6363636363636363535, 0.6401515151515151381, 0.6439393939393939226, 0.6477272727272727071, 0.6515151515151514916, 0.6553030303030302761, 0.6590909090909090606, 0.6628787878787878451, 0.6666666666666666297, 0.6704545454545454142, 0.6742424242424241987, 0.6780303030303029832, 0.6818181818181817677, 0.6856060606060605522, 0.6893939393939394478, 0.6931818181818182323, 0.6969696969696970168, 0.7007575757575758013, 0.7045454545454545858, 0.7083333333333333703, 0.7121212121212121549, 0.7159090909090909394, 0.7196969696969697239, 0.7234848484848485084, 0.7272727272727272929, 0.7310606060606060774, 0.7348484848484848619, 0.7386363636363636465, 0.7424242424242424310, 0.7462121212121212155, 0.7500000000000000000, 0.7537878787878787845, 0.7575757575757575690, 0.7613636363636363535, 0.7651515151515151381, 0.7689393939393939226, 0.7727272727272727071, 0.7765151515151514916, 0.7803030303030302761, 0.7840909090909090606, 0.7878787878787878451, 0.7916666666666666297, 0.7954545454545454142, 0.7992424242424241987, 0.8030303030303029832, 0.8068181818181817677, 0.8106060606060605522, 0.8143939393939394478, 0.8181818181818182323, 0.8219696969696970168, 0.8257575757575758013, 0.8295454545454545858, 0.8333333333333333703, 0.8371212121212121549, 0.8409090909090909394, 0.8446969696969697239, 0.8484848484848485084, 0.8522727272727272929, 0.8560606060606060774, 0.8598484848484848619, 0.8636363636363636465, 0.8674242424242424310, 0.8712121212121212155, 0.8750000000000000000, 0.8787878787878787845, 0.8825757575757575690, 0.8863636363636363535, 0.8901515151515151381, 0.8939393939393939226, 0.8977272727272727071, 0.9015151515151514916, 0.9053030303030302761, 0.9090909090909090606, 0.9128787878787878451, 0.9166666666666666297, 0.9204545454545454142, 0.9242424242424241987, 0.9280303030303029832, 0.9318181818181817677, 0.9356060606060605522, 0.9393939393939394478, 0.9431818181818182323, 0.9469696969696970168, 0.9507575757575758013, 0.9545454545454545858, 0.9583333333333333703, 0.9621212121212121549, 0.9659090909090909394 ),
 .UNSPECIFIED. ) 
 GEOMETRIC_REPRESENTATION_ITEM ( )  RATIONAL_B_SPLINE_SURFACE ( (
 ( 1.000000000000000000, 0.9659258262890683122, 1.000000000000000000, 0.9659258262890683122, 1.000000000000000000, 0.9659258262890683122, 1.000000000000000000, 0.9659258262890683122, 1.000000000000000000, 0.9659258262890683122, 1.000000000000000000, 0.9659258262890683122, 1.000000000000000000, 0.9659258262890683122, 1.000000000000000000, 0.9659258262890683122, 1.000000000000000000, 0.9659258262890683122, 1.000000000000000000, 0.9659258262890683122, 1.000000000000000000, 0.9659258262890683122, 1.000000000000000000, 0.9659258262890683122, 1.000000000000000000, 0.9659258262890683122, 1.000000000000000000, 0.9659258262890683122, 1.000000000000000000, 0.9659258262890683122, 1.000000000000000000, 0.9659258262890683122, 1.000000000000000000, 0.9659258262890683122, 1.000000000000000000, 0.9659258262890683122, 1.000000000000000000, 0.9659258262890683122, 1.000000000000000000, 0.9659258262890683122, 1.000000000000000000, 0.9659258262890683122, 1.000000000000000000, 0.9659258262890683122, 1.000000000000000000, 0.9659258262890683122, 1.000000000000000000, 0.9659258262890683122, 1.000000000000000000, 0.9659258262890683122, 1.000000000000000000, 0.9659258262890683122, 1.000000000000000000, 0.9659258262890683122, 1.000000000000000000, 0.9659258262890683122, 1.000000000000000000, 0.9659258262890683122, 1.000000000000000000, 0.9659258262890683122, 1.000000000000000000, 0.9659258262890683122, 1.000000000000000000, 0.9659258262890683122, 1.000000000000000000, 0.9659258262890683122, 1.000000000000000000, 0.9659258262890683122, 1.000000000000000000, 0.9659258262890683122, 1.000000000000000000, 0.9659258262890683122, 1.000000000000000000, 0.9659258262890683122, 1.000000000000000000, 0.9659258262890683122, 1.000000000000000000, 0.9659258262890683122, 1.000000000000000000, 0.9659258262890683122, 1.000000000000000000, 0.9659258262890683122, 1.000000000000000000, 0.9659258262890683122, 1.000000000000000000, 0.9659258262890683122, 1.000000000000000000, 0.9659258262890683122, 1.000000000000000000, 0.9659258262890683122, 1.000000000000000000, 0.9659258262890683122, 1.000000000000000000, 0.9659258262890683122, 1.000000000000000000, 0.9659258262890683122, 1.000000000000000000, 0.9659258262890683122, 1.000000000000000000, 0.9659258262890683122, 1.000000000000000000, 0.9659258262890683122, 1.000000000000000000, 0.9659258262890683122, 1.000000000000000000, 0.9659258262890683122, 1.000000000000000000, 0.9659258262890683122, 1.000000000000000000, 0.9659258262890683122, 1.000000000000000000, 0.9659258262890683122, 1.000000000000000000, 0.9659258262890683122, 1.000000000000000000, 0.9659258262890683122, 1.000000000000000000, 0.9659258262890683122, 1.000000000000000000, 0.9659258262890683122, 1.000000000000000000, 0.9659258262890683122, 1.000000000000000000, 0.9659258262890683122, 1.000000000000000000, 0.9659258262890683122, 1.000000000000000000, 0.9659258262890683122, 1.000000000000000000, 0.9659258262890683122, 1.000000000000000000, 0.9659258262890683122, 1.000000000000000000, 0.9659258262890683122, 1.000000000000000000, 0.9659258262890683122, 1.000000000000000000, 0.9659258262890683122, 1.000000000000000000, 0.9659258262890683122, 1.000000000000000000, 0.9659258262890683122, 1.000000000000000000, 0.9659258262890683122, 1.000000000000000000, 0.9659258262890683122, 1.000000000000000000, 0.9659258262890683122, 1.000000000000000000, 0.9659258262890683122, 1.000000000000000000, 0.9659258262890683122, 1.000000000000000000, 0.9659258262890683122, 1.000000000000000000, 0.9659258262890683122, 1.000000000000000000, 0.9659258262890683122, 1.000000000000000000, 0.9659258262890683122, 1.000000000000000000, 0.9659258262890683122, 1.000000000000000000, 0.9659258262890683122, 1.000000000000000000, 0.9659258262890683122, 1.000000000000000000, 0.9659258262890683122, 1.000000000000000000, 0.9659258262890683122, 1.000000000000000000, 0.9659258262890683122, 1.000000000000000000, 0.9659258262890683122, 1.000000000000000000, 0.9659258262890683122, 1.000000000000000000, 0.9659258262890683122, 1.000000000000000000, 0.9659258262890683122, 1.000000000000000000, 0.9659258262890683122, 1.000000000000000000, 0.9659258262890683122, 1.000000000000000000, 0.9659258262890683122, 1.000000000000000000, 0.9659258262890683122, 1.000000000000000000, 0.9659258262890683122, 1.000000000000000000, 0.9659258262890683122, 1.000000000000000000, 0.9659258262890683122, 1.000000000000000000, 0.9659258262890683122, 1.000000000000000000, 0.9659258262890683122, 1.000000000000000000, 0.9659258262890683122, 1.000000000000000000, 0.9659258262890683122, 1.000000000000000000, 0.9659258262890683122, 1.000000000000000000, 0.9659258262890683122, 1.000000000000000000, 0.9659258262890683122, 1.000000000000000000, 0.9659258262890683122, 1.000000000000000000, 0.9659258262890683122, 1.000000000000000000, 0.9659258262890683122, 1.000000000000000000, 0.9659258262890683122, 1.000000000000000000, 0.9659258262890683122, 1.000000000000000000, 0.9659258262890683122, 1.000000000000000000, 0.9659258262890683122, 1.000000000000000000, 0.9659258262890683122, 1.000000000000000000, 0.9659258262890683122, 1.000000000000000000, 0.9659258262890683122, 1.000000000000000000, 0.9659258262890683122, 1.000000000000000000, 0.9659258262890683122, 1.000000000000000000, 0.9659258262890683122, 1.000000000000000000, 0.9659258262890683122, 1.000000000000000000, 0.9659258262890683122, 1.000000000000000000, 0.9659258262890683122, 1.000000000000000000, 0.9659258262890683122, 1.000000000000000000, 0.9659258262890683122, 1.000000000000000000, 0.9659258262890683122, 1.000000000000000000, 0.9659258262890683122, 1.000000000000000000, 0.9659258262890683122, 1.000000000000000000, 0.9659258262890683122, 1.000000000000000000, 0.9659258262890683122, 1.000000000000000000, 0.9659258262890683122, 1.000000000000000000, 0.9659258262890683122, 1.000000000000000000, 0.9659258262890683122, 1.000000000000000000, 0.9659258262890683122, 1.000000000000000000, 0.9659258262890683122, 1.000000000000000000, 0.9659258262890683122, 1.000000000000000000, 0.9659258262890683122, 1.000000000000000000, 0.9659258262890683122, 1.000000000000000000, 0.9659258262890683122, 1.000000000000000000, 0.9659258262890683122, 1.000000000000000000, 0.9659258262890683122, 1.000000000000000000, 0.9659258262890683122, 1.000000000000000000, 0.9659258262890683122, 1.000000000000000000, 0.9659258262890683122, 1.000000000000000000, 0.9659258262890683122, 1.000000000000000000, 0.9659258262890683122, 1.000000000000000000, 0.9659258262890683122, 1.000000000000000000, 0.9659258262890683122, 1.000000000000000000, 0.9659258262890683122, 1.000000000000000000, 0.9659258262890683122, 1.000000000000000000, 0.9659258262890683122, 1.000000000000000000, 0.9659258262890683122, 1.000000000000000000, 0.9659258262890683122, 1.000000000000000000, 0.9659258262890683122, 1.000000000000000000, 0.9659258262890683122, 1.000000000000000000, 0.9659258262890683122, 1.000000000000000000, 0.9659258262890683122, 1.000000000000000000, 0.9659258262890683122, 1.000000000000000000, 0.9659258262890683122, 1.000000000000000000, 0.9659258262890683122, 1.000000000000000000, 0.9659258262890683122, 1.000000000000000000, 0.9659258262890683122, 1.000000000000000000, 0.9659258262890683122, 1.000000000000000000, 0.9659258262890683122, 1.000000000000000000, 0.9659258262890683122, 1.000000000000000000, 0.9659258262890683122, 1.000000000000000000, 0.9659258262890683122, 1.000000000000000000, 0.9659258262890683122, 1.000000000000000000, 0.9659258262890683122, 1.000000000000000000, 0.9659258262890683122, 1.000000000000000000, 0.9659258262890683122, 1.000000000000000000, 0.9659258262890683122, 1.000000000000000000, 0.9659258262890683122, 1.000000000000000000, 0.9659258262890683122, 1.000000000000000000, 0.9659258262890683122, 1.000000000000000000, 0.9659258262890683122, 1.000000000000000000, 0.9659258262890683122, 1.000000000000000000, 0.9659258262890683122, 1.000000000000000000, 0.9659258262890683122, 1.000000000000000000, 0.9659258262890683122, 1.000000000000000000, 0.9659258262890683122, 1.000000000000000000, 0.9659258262890683122, 1.000000000000000000, 0.9659258262890683122, 1.000000000000000000, 0.9659258262890683122, 1.000000000000000000, 0.9659258262890683122, 1.000000000000000000, 0.9659258262890683122, 1.000000000000000000, 0.9659258262890683122, 1.000000000000000000, 0.9659258262890683122, 1.000000000000000000, 0.9659258262890683122, 1.000000000000000000, 0.9659258262890683122, 1.000000000000000000, 0.9659258262890683122, 1.000000000000000000, 0.9659258262890683122, 1.000000000000000000, 0.9659258262890683122, 1.000000000000000000, 0.9659258262890683122, 1.000000000000000000, 0.9659258262890683122, 1.000000000000000000, 0.9659258262890683122, 1.000000000000000000, 0.9659258262890683122, 1.000000000000000000, 0.9659258262890683122, 1.000000000000000000, 0.9659258262890683122, 1.000000000000000000, 0.9659258262890683122, 1.000000000000000000, 0.9659258262890683122, 1.000000000000000000, 0.9659258262890683122, 1.000000000000000000, 0.9659258262890683122, 1.000000000000000000, 0.9659258262890683122, 1.000000000000000000, 0.9659258262890683122, 1.000000000000000000, 0.9659258262890683122, 1.000000000000000000, 0.9659258262890683122, 1.000000000000000000, 0.9659258262890683122, 1.000000000000000000, 0.9659258262890683122, 1.000000000000000000, 0.9659258262890683122, 1.000000000000000000, 0.9659258262890683122, 1.000000000000000000, 0.9659258262890683122, 1.000000000000000000, 0.9659258262890683122, 1.000000000000000000, 0.9659258262890683122, 1.000000000000000000, 0.9659258262890683122, 1.000000000000000000, 0.9659258262890683122, 1.000000000000000000, 0.9659258262890683122, 1.000000000000000000, 0.9659258262890683122, 1.000000000000000000, 0.9659258262890683122, 1.000000000000000000, 0.9659258262890683122, 1.000000000000000000, 0.9659258262890683122, 1.000000000000000000, 0.9659258262890683122, 1.000000000000000000, 0.9659258262890683122, 1.000000000000000000, 0.9659258262890683122, 1.000000000000000000, 0.9659258262890683122, 1.000000000000000000, 0.9659258262890683122, 1.000000000000000000, 0.9659258262890683122, 1.000000000000000000, 0.9659258262890683122, 1.000000000000000000, 0.9659258262890683122, 1.000000000000000000, 0.9659258262890683122, 1.000000000000000000, 0.9659258262890683122, 1.000000000000000000, 0.9659258262890683122, 1.000000000000000000, 0.9659258262890683122, 1.000000000000000000, 0.9659258262890683122, 1.000000000000000000, 0.9659258262890683122, 1.000000000000000000, 0.9659258262890683122, 1.000000000000000000, 0.9659258262890683122, 1.000000000000000000, 0.9659258262890683122, 1.000000000000000000, 0.9659258262890683122, 1.000000000000000000, 0.9659258262890683122, 1.000000000000000000, 0.9659258262890683122, 1.000000000000000000, 0.9659258262890683122, 1.000000000000000000, 0.9659258262890683122, 1.000000000000000000, 0.9659258262890683122, 1.000000000000000000, 0.9659258262890683122, 1.000000000000000000, 0.9659258262890683122, 1.000000000000000000, 0.9659258262890683122, 1.000000000000000000, 0.9659258262890683122, 1.000000000000000000, 0.9659258262890683122, 1.000000000000000000, 0.9659258262890683122, 1.000000000000000000, 0.9659258262890683122, 1.000000000000000000, 0.9659258262890683122, 1.000000000000000000, 0.9659258262890683122, 1.000000000000000000, 0.9659258262890683122, 1.000000000000000000, 0.9659258262890683122, 1.000000000000000000, 0.9659258262890683122, 1.000000000000000000, 0.9659258262890683122, 1.000000000000000000, 0.9659258262890683122, 1.000000000000000000),
 ( 1.000000000000000000, 0.9659258262890683122, 1.000000000000000000, 0.9659258262890683122, 1.000000000000000000, 0.9659258262890683122, 1.000000000000000000, 0.9659258262890683122, 1.000000000000000000, 0.9659258262890683122, 1.000000000000000000, 0.9659258262890683122, 1.000000000000000000, 0.9659258262890683122, 1.000000000000000000, 0.9659258262890683122, 1.000000000000000000, 0.9659258262890683122, 1.000000000000000000, 0.9659258262890683122, 1.000000000000000000, 0.9659258262890683122, 1.000000000000000000, 0.9659258262890683122, 1.000000000000000000, 0.9659258262890683122, 1.000000000000000000, 0.9659258262890683122, 1.000000000000000000, 0.9659258262890683122, 1.000000000000000000, 0.9659258262890683122, 1.000000000000000000, 0.9659258262890683122, 1.000000000000000000, 0.9659258262890683122, 1.000000000000000000, 0.9659258262890683122, 1.000000000000000000, 0.9659258262890683122, 1.000000000000000000, 0.9659258262890683122, 1.000000000000000000, 0.9659258262890683122, 1.000000000000000000, 0.9659258262890683122, 1.000000000000000000, 0.9659258262890683122, 1.000000000000000000, 0.9659258262890683122, 1.000000000000000000, 0.9659258262890683122, 1.000000000000000000, 0.9659258262890683122, 1.000000000000000000, 0.9659258262890683122, 1.000000000000000000, 0.9659258262890683122, 1.000000000000000000, 0.9659258262890683122, 1.000000000000000000, 0.9659258262890683122, 1.000000000000000000, 0.9659258262890683122, 1.000000000000000000, 0.9659258262890683122, 1.000000000000000000, 0.9659258262890683122, 1.000000000000000000, 0.9659258262890683122, 1.000000000000000000, 0.9659258262890683122, 1.000000000000000000, 0.9659258262890683122, 1.000000000000000000, 0.9659258262890683122, 1.000000000000000000, 0.9659258262890683122, 1.000000000000000000, 0.9659258262890683122, 1.000000000000000000, 0.9659258262890683122, 1.000000000000000000, 0.9659258262890683122, 1.000000000000000000, 0.9659258262890683122, 1.000000000000000000, 0.9659258262890683122, 1.000000000000000000, 0.9659258262890683122, 1.000000000000000000, 0.9659258262890683122, 1.000000000000000000, 0.9659258262890683122, 1.000000000000000000, 0.9659258262890683122, 1.000000000000000000, 0.9659258262890683122, 1.000000000000000000, 0.9659258262890683122, 1.000000000000000000, 0.9659258262890683122, 1.000000000000000000, 0.9659258262890683122, 1.000000000000000000, 0.9659258262890683122, 1.000000000000000000, 0.9659258262890683122, 1.000000000000000000, 0.9659258262890683122, 1.000000000000000000, 0.9659258262890683122, 1.000000000000000000, 0.9659258262890683122, 1.000000000000000000, 0.9659258262890683122, 1.000000000000000000, 0.9659258262890683122, 1.000000000000000000, 0.9659258262890683122, 1.000000000000000000, 0.9659258262890683122, 1.000000000000000000, 0.9659258262890683122, 1.000000000000000000, 0.9659258262890683122, 1.000000000000000000, 0.9659258262890683122, 1.000000000000000000, 0.9659258262890683122, 1.000000000000000000, 0.9659258262890683122, 1.000000000000000000, 0.9659258262890683122, 1.000000000000000000, 0.9659258262890683122, 1.000000000000000000, 0.9659258262890683122, 1.000000000000000000, 0.9659258262890683122, 1.000000000000000000, 0.9659258262890683122, 1.000000000000000000, 0.9659258262890683122, 1.000000000000000000, 0.9659258262890683122, 1.000000000000000000, 0.9659258262890683122, 1.000000000000000000, 0.9659258262890683122, 1.000000000000000000, 0.9659258262890683122, 1.000000000000000000, 0.9659258262890683122, 1.000000000000000000, 0.9659258262890683122, 1.000000000000000000, 0.9659258262890683122, 1.000000000000000000, 0.9659258262890683122, 1.000000000000000000, 0.9659258262890683122, 1.000000000000000000, 0.9659258262890683122, 1.000000000000000000, 0.9659258262890683122, 1.000000000000000000, 0.9659258262890683122, 1.000000000000000000, 0.9659258262890683122, 1.000000000000000000, 0.9659258262890683122, 1.000000000000000000, 0.9659258262890683122, 1.000000000000000000, 0.9659258262890683122, 1.000000000000000000, 0.9659258262890683122, 1.000000000000000000, 0.9659258262890683122, 1.000000000000000000, 0.9659258262890683122, 1.000000000000000000, 0.9659258262890683122, 1.000000000000000000, 0.9659258262890683122, 1.000000000000000000, 0.9659258262890683122, 1.000000000000000000, 0.9659258262890683122, 1.000000000000000000, 0.9659258262890683122, 1.000000000000000000, 0.9659258262890683122, 1.000000000000000000, 0.9659258262890683122, 1.000000000000000000, 0.9659258262890683122, 1.000000000000000000, 0.9659258262890683122, 1.000000000000000000, 0.9659258262890683122, 1.000000000000000000, 0.9659258262890683122, 1.000000000000000000, 0.9659258262890683122, 1.000000000000000000, 0.9659258262890683122, 1.000000000000000000, 0.9659258262890683122, 1.000000000000000000, 0.9659258262890683122, 1.000000000000000000, 0.9659258262890683122, 1.000000000000000000, 0.9659258262890683122, 1.000000000000000000, 0.9659258262890683122, 1.000000000000000000, 0.9659258262890683122, 1.000000000000000000, 0.9659258262890683122, 1.000000000000000000, 0.9659258262890683122, 1.000000000000000000, 0.9659258262890683122, 1.000000000000000000, 0.9659258262890683122, 1.000000000000000000, 0.9659258262890683122, 1.000000000000000000, 0.9659258262890683122, 1.000000000000000000, 0.9659258262890683122, 1.000000000000000000, 0.9659258262890683122, 1.000000000000000000, 0.9659258262890683122, 1.000000000000000000, 0.9659258262890683122, 1.000000000000000000, 0.9659258262890683122, 1.000000000000000000, 0.9659258262890683122, 1.000000000000000000, 0.9659258262890683122, 1.000000000000000000, 0.9659258262890683122, 1.000000000000000000, 0.9659258262890683122, 1.000000000000000000, 0.9659258262890683122, 1.000000000000000000, 0.9659258262890683122, 1.000000000000000000, 0.9659258262890683122, 1.000000000000000000, 0.9659258262890683122, 1.000000000000000000, 0.9659258262890683122, 1.000000000000000000, 0.9659258262890683122, 1.000000000000000000, 0.9659258262890683122, 1.000000000000000000, 0.9659258262890683122, 1.000000000000000000, 0.9659258262890683122, 1.000000000000000000, 0.9659258262890683122, 1.000000000000000000, 0.9659258262890683122, 1.000000000000000000, 0.9659258262890683122, 1.000000000000000000, 0.9659258262890683122, 1.000000000000000000, 0.9659258262890683122, 1.000000000000000000, 0.9659258262890683122, 1.000000000000000000, 0.9659258262890683122, 1.000000000000000000, 0.9659258262890683122, 1.000000000000000000, 0.9659258262890683122, 1.000000000000000000, 0.9659258262890683122, 1.000000000000000000, 0.9659258262890683122, 1.000000000000000000, 0.9659258262890683122, 1.000000000000000000, 0.9659258262890683122, 1.000000000000000000, 0.9659258262890683122, 1.000000000000000000, 0.9659258262890683122, 1.000000000000000000, 0.9659258262890683122, 1.000000000000000000, 0.9659258262890683122, 1.000000000000000000, 0.9659258262890683122, 1.000000000000000000, 0.9659258262890683122, 1.000000000000000000, 0.9659258262890683122, 1.000000000000000000, 0.9659258262890683122, 1.000000000000000000, 0.9659258262890683122, 1.000000000000000000, 0.9659258262890683122, 1.000000000000000000, 0.9659258262890683122, 1.000000000000000000, 0.9659258262890683122, 1.000000000000000000, 0.9659258262890683122, 1.000000000000000000, 0.9659258262890683122, 1.000000000000000000, 0.9659258262890683122, 1.000000000000000000, 0.9659258262890683122, 1.000000000000000000, 0.9659258262890683122, 1.000000000000000000, 0.9659258262890683122, 1.000000000000000000, 0.9659258262890683122, 1.000000000000000000, 0.9659258262890683122, 1.000000000000000000, 0.9659258262890683122, 1.000000000000000000, 0.9659258262890683122, 1.000000000000000000, 0.9659258262890683122, 1.000000000000000000, 0.9659258262890683122, 1.000000000000000000, 0.9659258262890683122, 1.000000000000000000, 0.9659258262890683122, 1.000000000000000000, 0.9659258262890683122, 1.000000000000000000, 0.9659258262890683122, 1.000000000000000000, 0.9659258262890683122, 1.000000000000000000, 0.9659258262890683122, 1.000000000000000000, 0.9659258262890683122, 1.000000000000000000, 0.9659258262890683122, 1.000000000000000000, 0.9659258262890683122, 1.000000000000000000, 0.9659258262890683122, 1.000000000000000000, 0.9659258262890683122, 1.000000000000000000, 0.9659258262890683122, 1.000000000000000000, 0.9659258262890683122, 1.000000000000000000, 0.9659258262890683122, 1.000000000000000000, 0.9659258262890683122, 1.000000000000000000, 0.9659258262890683122, 1.000000000000000000, 0.9659258262890683122, 1.000000000000000000, 0.9659258262890683122, 1.000000000000000000, 0.9659258262890683122, 1.000000000000000000, 0.9659258262890683122, 1.000000000000000000, 0.9659258262890683122, 1.000000000000000000, 0.9659258262890683122, 1.000000000000000000, 0.9659258262890683122, 1.000000000000000000, 0.9659258262890683122, 1.000000000000000000, 0.9659258262890683122, 1.000000000000000000, 0.9659258262890683122, 1.000000000000000000, 0.9659258262890683122, 1.000000000000000000, 0.9659258262890683122, 1.000000000000000000, 0.9659258262890683122, 1.000000000000000000, 0.9659258262890683122, 1.000000000000000000, 0.9659258262890683122, 1.000000000000000000, 0.9659258262890683122, 1.000000000000000000, 0.9659258262890683122, 1.000000000000000000, 0.9659258262890683122, 1.000000000000000000, 0.9659258262890683122, 1.000000000000000000, 0.9659258262890683122, 1.000000000000000000, 0.9659258262890683122, 1.000000000000000000, 0.9659258262890683122, 1.000000000000000000, 0.9659258262890683122, 1.000000000000000000, 0.9659258262890683122, 1.000000000000000000, 0.9659258262890683122, 1.000000000000000000, 0.9659258262890683122, 1.000000000000000000, 0.9659258262890683122, 1.000000000000000000, 0.9659258262890683122, 1.000000000000000000, 0.9659258262890683122, 1.000000000000000000, 0.9659258262890683122, 1.000000000000000000, 0.9659258262890683122, 1.000000000000000000, 0.9659258262890683122, 1.000000000000000000, 0.9659258262890683122, 1.000000000000000000, 0.9659258262890683122, 1.000000000000000000, 0.9659258262890683122, 1.000000000000000000, 0.9659258262890683122, 1.000000000000000000, 0.9659258262890683122, 1.000000000000000000, 0.9659258262890683122, 1.000000000000000000, 0.9659258262890683122, 1.000000000000000000, 0.9659258262890683122, 1.000000000000000000, 0.9659258262890683122, 1.000000000000000000, 0.9659258262890683122, 1.000000000000000000, 0.9659258262890683122, 1.000000000000000000, 0.9659258262890683122, 1.000000000000000000, 0.9659258262890683122, 1.000000000000000000, 0.9659258262890683122, 1.000000000000000000, 0.9659258262890683122, 1.000000000000000000, 0.9659258262890683122, 1.000000000000000000, 0.9659258262890683122, 1.000000000000000000, 0.9659258262890683122, 1.000000000000000000, 0.9659258262890683122, 1.000000000000000000, 0.9659258262890683122, 1.000000000000000000, 0.9659258262890683122, 1.000000000000000000, 0.9659258262890683122, 1.000000000000000000, 0.9659258262890683122, 1.000000000000000000, 0.9659258262890683122, 1.000000000000000000, 0.9659258262890683122, 1.000000000000000000, 0.9659258262890683122, 1.000000000000000000, 0.9659258262890683122, 1.000000000000000000, 0.9659258262890683122, 1.000000000000000000, 0.9659258262890683122, 1.000000000000000000, 0.9659258262890683122, 1.000000000000000000, 0.9659258262890683122, 1.000000000000000000, 0.9659258262890683122, 1.000000000000000000, 0.9659258262890683122, 1.000000000000000000, 0.9659258262890683122, 1.000000000000000000, 0.9659258262890683122, 1.000000000000000000, 0.9659258262890683122, 1.000000000000000000) ) ) 
 REPRESENTATION_ITEM ( '' )  SURFACE ( )  );
#31569 = CARTESIAN_POINT ( 'NONE',  ( 0.2362204724409456558, -0.1870078740157480879, -0.4822834645669291653 ) ) ;
#31570 = CARTESIAN_POINT ( 'NONE',  ( 0.3949938075777408852, 0.1058382717557500435, -0.9888451443569553634 ) ) ;
#31571 = CARTESIAN_POINT ( 'NONE',  ( -0.9908136482939626788, -0.6692913385826773087, -0.1292274648535924053 ) ) ;
#31572 = CARTESIAN_POINT ( 'NONE',  ( 1.023622047244095334, -0.1870078740157479769, 0.4822834645669291653 ) ) ;
#31573 = CARTESIAN_POINT ( 'NONE',  ( 0.8923884514435701520, -0.5023911411419708095, -0.1820866141732282451 ) ) ;
#31574 = DIRECTION ( 'NONE',  ( 0.000000000000000000, 0.000000000000000000, -1.000000000000000000 ) ) ;
#31575 = CARTESIAN_POINT ( 'NONE',  ( -0.1771653543307080136, -0.5400638737290844871, 0.3530559997133364547 ) ) ;
#31576 = CARTESIAN_POINT ( 'NONE',  ( 0.06561679790026316017, -0.3690944881889763329, 0.3153832671262228327 ) ) ;
#31577 = CARTESIAN_POINT ( 'NONE',  ( -2.822444539845162303, 1.119136672863575876, 0.2244172274865353089 ) ) ;
#31578 = CARTESIAN_POINT ( 'NONE',  ( -0.2887139107611542133, 0.2306618581243848609, 0.2411417322834645549 ) ) ;
#31579 = CARTESIAN_POINT ( 'NONE',  ( 0.4133858267716541968, -0.4536011799217368745, -0.2665933059059886201 ) ) ;
#31580 = EDGE_CURVE ( 'NONE', #68837, #77522, #9969, .T. ) ;
#31581 = CARTESIAN_POINT ( 'NONE',  ( -0.1998031496062994405, 0.3460692066303957537, -1.979658792650918597 ) ) ;
#31582 = CARTESIAN_POINT ( 'NONE',  ( -0.09842519685039295696, -0.5400638737290844871, 0.3530559997133364547 ) ) ;
#31583 = CARTESIAN_POINT ( 'NONE',  ( 0.9842519685039378130, -0.5511811023622047445, 6.969142054262312111E-17 ) ) ;
#31584 = CYLINDRICAL_SURFACE ( 'NONE', #48676, 0.4724409448818898682 ) ;
#31585 = CARTESIAN_POINT ( 'NONE',  ( -0.4396325459317579898, 0.1771653543307087630, 0.09757992244046791164 ) ) ;
#31586 = AXIS2_PLACEMENT_3D ( 'NONE', #79734, #68341, #4347 ) ;
#31587 = CARTESIAN_POINT ( 'NONE',  ( -0.7874015748031489847, -0.1870078740157479769, 0.3641732283464567677 ) ) ;
#31588 = CARTESIAN_POINT ( 'NONE',  ( -0.2362204724409440182, -0.1870078740157479769, 0.4822834645669291653 ) ) ;
#31589 = CARTESIAN_POINT ( 'NONE',  ( -0.1509186351706028884, -0.05778040916215522460, 0.4822834645669289988 ) ) ;
#31590 = CARTESIAN_POINT ( 'NONE',  ( 1.062992125984252745, 0.1771653543307087630, 0.000000000000000000 ) ) ;
#31591 = CARTESIAN_POINT ( 'NONE',  ( -1.581364829396324945, -0.2845877964562159024, 0.3641732283464567677 ) ) ;
#31592 = CARTESIAN_POINT ( 'NONE',  ( 1.555118110236221041, -0.4536011799217367080, 0.2665933059059888421 ) ) ;
#31593 = CARTESIAN_POINT ( 'NONE',  ( 0.6036745406824154392, 0.2306618581243847221, -0.2411417322834647770 ) ) ;
#31594 = CARTESIAN_POINT ( 'NONE',  ( 0.1654213697349169176, 1.092461187568466219, -1.877587376364790339 ) ) ;
#31595 = CARTESIAN_POINT ( 'NONE',  ( -0.4461942257217840213, 0.2306618581243848609, 0.2411417322834645549 ) ) ;
#31596 = CARTESIAN_POINT ( 'NONE',  ( 0.3917322834645670104, 2.398668435337828261E-17, -0.8326771653543307838 ) ) ;
#31597 = CARTESIAN_POINT ( 'NONE',  ( 0.8923884514435703741, 0.2306618581243848609, 0.2411417322834645549 ) ) ;
#31598 = CARTESIAN_POINT ( 'NONE',  ( 0.7283464566929143125, 0.1660481256975885056, 0.3530559997133364547 ) ) ;
#31599 = DIRECTION ( 'NONE',  ( -0.000000000000000000, 1.000000000000000000, -0.000000000000000000 ) ) ;
#31600 = CARTESIAN_POINT ( 'NONE',  ( 0.5183727034120741983, -0.5511811023622046335, 0.09757992244046803654 ) ) ;
#31601 = CARTESIAN_POINT ( 'NONE',  ( 1.338582677165355062, -0.1870078740157479769, 0.4822834645669291653 ) ) ;
#31602 = CARTESIAN_POINT ( 'NONE',  ( -0.1837270341207343505, -0.5023911411419708095, 0.1820866141732285504 ) ) ;
#31603 = CARTESIAN_POINT ( 'NONE',  ( -0.4265091863517051496, -0.6692913385826771977, 0.1292274648535927661 ) ) ;
#31604 = LINE ( 'NONE', #464, #50150 ) ;
#31605 = CARTESIAN_POINT ( 'NONE',  ( 0.3083989501312343062, -0.3162353388693405765, 0.4822834645669290543 ) ) ;
#31606 = CARTESIAN_POINT ( 'NONE',  ( -0.9711286089238838626, 0.2306618581243847221, -0.2411417322834647770 ) ) ;
#31607 = CARTESIAN_POINT ( 'NONE',  ( -0.8661417322834640276, -0.1870078740157480601, -0.3641732283464567677 ) ) ;
#31608 = CARTESIAN_POINT ( 'NONE',  ( 0.4724409448818904789, -0.1870078740157479769, 0.4822834645669291653 ) ) ;
#31609 = CARTESIAN_POINT ( 'NONE',  ( -1.410761154855642463, -0.05778040916215522460, 0.4822834645669289988 ) ) ;
#31610 = CARTESIAN_POINT ( 'NONE',  ( -0.1771653543307080136, 0.1660481256975883668, -0.3530559997133364547 ) ) ;
#31611 = CARTESIAN_POINT ( 'NONE',  ( -0.3458507752293906723, -0.3458507752293910609, -0.5314960629921260393 ) ) ;
#31613 = CARTESIAN_POINT ( 'NONE',  ( 1.391076115485564868, -0.6046776061558807314, 0.2411417322834647770 ) ) ;
#31612 = CARTESIAN_POINT ( 'NONE',  ( -0.4724409448818898682, -8.678599364036362592E-17, -2.244094488188976388 ) ) ;
#31614 = CARTESIAN_POINT ( 'NONE',  ( 1.279527559055118724, -0.5400638737290845981, -0.3530559997133363437 ) ) ;
#31615 = CARTESIAN_POINT ( 'NONE',  ( 0.2867679344610366554, 0.2867679344610366554, -2.019685039370078261 ) ) ;
#31616 = CARTESIAN_POINT ( 'NONE',  ( -1.607611548556429737, 0.2952755905511810774, -0.1292274648535930714 ) ) ;
#31617 = CARTESIAN_POINT ( 'NONE',  ( -1.069553805774277722, 0.2952755905511811885, 0.1292274648535926551 ) ) ;
#31618 = CARTESIAN_POINT ( 'NONE',  ( 0.3458507752293908943, 0.3458507752293908943, -0.1377952755905511861 ) ) ;
#31619 = CARTESIAN_POINT ( 'NONE',  ( -0.1974969037888706647, 0.3420746716998658843, -2.690288713910760965 ) ) ;
#31620 = VERTEX_POINT ( 'NONE', #7875 ) ;
#31621 = CARTESIAN_POINT ( 'NONE',  ( -0.2690288713910754526, -0.5511811023622046335, 0.09757992244046803654 ) ) ;
#31622 = CARTESIAN_POINT ( 'NONE',  ( -9.594673741351313045E-17, 0.3917322834645670104, -1.566929133858267820 ) ) ;
#31623 = CARTESIAN_POINT ( 'NONE',  ( 0.6364829396325465405, -0.05778040916215522460, 0.4822834645669289988 ) ) ;
#31624 = EDGE_CURVE ( 'NONE', #2780, #55113, #51168, .T. ) ;
#31625 = CARTESIAN_POINT ( 'NONE',  ( -0.2087913723976025926, 0.2087913723976025371, 0.1248231986745539646 ) ) ;
#31626 = CARTESIAN_POINT ( 'NONE',  ( -1.614173228346457378, 0.5038684218300931716, 0.1372047244094476981 ) ) ;
#31627 = CARTESIAN_POINT ( 'NONE',  ( -0.3674540682414689785, 0.1283753931104748280, 0.1820866141732283561 ) ) ;
#31628 = CARTESIAN_POINT ( 'NONE',  ( -0.2114133405073580496, -0.2061694042878472466, 0.1284558427095352229 ) ) ;
#31629 = CARTESIAN_POINT ( 'NONE',  ( 1.345144356955381593, -0.05778040916215522460, 0.4822834645669289988 ) ) ;
#31630 = CARTESIAN_POINT ( 'NONE',  ( 1.122047244094488860, 0.07958543189024085140, 0.2665933059059887866 ) ) ;
#31631 = CARTESIAN_POINT ( 'NONE',  ( -0.006561679790025524116, -0.05778040916215560624, -0.4822834645669293319 ) ) ;
#31632 = CARTESIAN_POINT ( 'NONE',  ( 4.797336870675655290E-17, -0.3917322834645669549, -0.6312142800186859581 ) ) ;
#31633 = CARTESIAN_POINT ( 'NONE',  ( -0.3937007874015740483, -0.1870078740157479769, 0.4822834645669291653 ) ) ;
#31634 = CARTESIAN_POINT ( 'NONE',  ( -1.463254593175852492, -0.5511811023622048555, -0.09757992244046775898 ) ) ;
#31635 = CARTESIAN_POINT ( 'NONE',  ( -0.5183727034120726440, -0.6692913385826773087, -0.1292274648535924053 ) ) ;
#31636 = CARTESIAN_POINT ( 'NONE',  ( 1.574803149606299746, -0.1870078740157480879, -0.4822834645669291653 ) ) ;
#31637 = CARTESIAN_POINT ( 'NONE',  ( 0.6402603868039153934, -2.736035270306112984E-15, 0.4281989832122460871 ) ) ;
#31638 = VERTEX_POINT ( 'NONE', #301 ) ;
#31639 = CARTESIAN_POINT ( 'NONE',  ( -0.1958661417322833942, -0.3392501089628018884, -2.109599368275277609 ) ) ;
#31640 = CARTESIAN_POINT ( 'NONE',  ( 0.2690288713910767848, 0.2952755905511811885, 0.1292274648535926551 ) ) ;
#31641 = ORIENTED_EDGE ( 'NONE', *, *, #19980, .F. ) ;
#31642 = VECTOR ( 'NONE', #48065, 39.37007874015748143 ) ;
#31643 = CARTESIAN_POINT ( 'NONE',  ( -0.7349081364829390672, 0.2306618581243847221, -0.2411417322834647770 ) ) ;
#31644 = CARTESIAN_POINT ( 'NONE',  ( -1.496062992125983815, -0.1870078740157479769, 0.4822834645669291653 ) ) ;
#31645 = EDGE_CURVE ( 'NONE', #45904, #69925, #79671, .T. ) ;
#31646 = CARTESIAN_POINT ( 'NONE',  ( 0.4986876640419954376, 0.2306618581243848609, 0.2411417322834645549 ) ) ;
#31647 = CARTESIAN_POINT ( 'NONE',  ( -0.1377952755905504645, -0.5400638737290845981, -0.3530559997133363437 ) ) ;
#31648 = CARTESIAN_POINT ( 'NONE',  ( -0.1049643490035302024, -0.3917322834645671215, -1.259186351706037099 ) ) ;
#31649 = CARTESIAN_POINT ( 'NONE',  ( -0.6824146981627291497, -0.6046776061558809534, -0.2411417322834644161 ) ) ;
#31650 = CARTESIAN_POINT ( 'NONE',  ( -0.2099737532808391705, 0.2306618581243848609, 0.2411417322834645549 ) ) ;
#31651 = CARTESIAN_POINT ( 'NONE',  ( -1.056430446194224881, -0.6692913385826771977, 0.1292274648535927661 ) ) ;
#31652 = EDGE_CURVE ( 'NONE', #44157, #40053, #33435, .T. ) ;
#31653 = CARTESIAN_POINT ( 'NONE',  ( -0.1312335958005241554, -0.5023911411419708095, -0.1820866141732282451 ) ) ;
#31654 = CARTESIAN_POINT ( 'NONE',  ( -0.005815251566291224430, 0.3972027188793958996, 2.415985422253608372E-12 ) ) ;
#31655 = CARTESIAN_POINT ( 'NONE',  ( -0.1640419947506555343, -0.3162353388693405765, 0.4822834645669290543 ) ) ;
#31656 = FACE_OUTER_BOUND ( 'NONE', #73292, .T. ) ;
#31657 = CARTESIAN_POINT ( 'NONE',  ( 1.227034120734908917, -0.6692913385826771977, 0.1292274648535927661 ) ) ;
#31658 = CARTESIAN_POINT ( 'NONE',  ( -0.3917322834645669549, -0.1049643490035306603, -2.872703412073490448 ) ) ;
#31659 = ORIENTED_EDGE ( 'NONE', *, *, #38333, .T. ) ;
#31660 = EDGE_LOOP ( 'NONE', ( #62060, #3902, #32613, #65002 ) ) ;
#31661 = CARTESIAN_POINT ( 'NONE',  ( 0.1574803149606306130, -0.1870078740157480879, -0.4822834645669291653 ) ) ;
#31662 = CARTESIAN_POINT ( 'NONE',  ( -0.06561679790026180015, -0.3690944881889765550, -0.3153832671262227771 ) ) ;
#31664 = CARTESIAN_POINT ( 'NONE',  ( 0.4724409448818898127, -0.1265901696524988629, -0.4265091863517060378 ) ) ;
#31663 = CARTESIAN_POINT ( 'NONE',  ( 1.423884514435696413, -0.2845877964562161244, -0.3641732283464567121 ) ) ;
#31665 = CARTESIAN_POINT ( 'NONE',  ( 0.3917322834645670104, 2.398668435337828261E-17, -1.147637795275590733 ) ) ;
#31666 = CARTESIAN_POINT ( 'NONE',  ( -0.3458507752293909498, 0.3458507752293907833, -0.4114173228346455491 ) ) ;
#31667 = CARTESIAN_POINT ( 'NONE',  ( 1.482939632545932307, -0.3690944881889763329, 0.3153832671262228327 ) ) ;
#31668 = CARTESIAN_POINT ( 'NONE',  ( -1.522309711286088607, -0.6046776061558807314, 0.2411417322834647770 ) ) ;
#31669 = CARTESIAN_POINT ( 'NONE',  ( 0.3420746716998660508, -0.1974969037888704149, 0.1332020997375328031 ) ) ;
#31670 = CARTESIAN_POINT ( 'NONE',  ( 0.6496062992125991586, 0.1660481256975885056, 0.3530559997133364547 ) ) ;
#31671 = CARTESIAN_POINT ( 'NONE',  ( -1.148293963254592542, 0.2952755905511811885, 0.1292274648535926551 ) ) ;
#31672 = CARTESIAN_POINT ( 'NONE',  ( -0.9580052493438311334, -0.4281496062992124485, 0.4176697321401328655 ) ) ;
#31673 = CARTESIAN_POINT ( 'NONE',  ( 0.08530183727034192087, -0.3162353388693409650, -0.4822834645669289433 ) ) ;
#31674 = CARTESIAN_POINT ( 'NONE',  ( 0.7939632545931766261, -0.05778040916215522460, 0.4822834645669289988 ) ) ;
#31675 = CARTESIAN_POINT ( 'NONE',  ( 1.345144356955381593, -0.08942795157527998196, 0.3641732283464567121 ) ) ;
#31676 = CONTEXT_DEPENDENT_SHAPE_REPRESENTATION ( #23980, #20440 ) ;
#31677 = CARTESIAN_POINT ( 'NONE',  ( 0.8005249343832028242, -0.3690944881889765550, -0.3153832671262227771 ) ) ;
#31678 = CARTESIAN_POINT ( 'NONE',  ( -0.9645669291338575535, 0.1660481256975883668, -0.3530559997133364547 ) ) ;
#31679 = EDGE_CURVE ( 'NONE', #44891, #68517, #33953, .T. ) ;
#31680 = CARTESIAN_POINT ( 'NONE',  ( -0.2925321140481932369, 0.2925321140481931259, -0.5688976377952755792 ) ) ;
#31681 = CARTESIAN_POINT ( 'NONE',  ( 1.646981627296588035, -0.3162353388693405765, 0.4822834645669290543 ) ) ;
#31682 = CARTESIAN_POINT ( 'NONE',  ( 0.1049643490035303689, 0.3917322834645670104, -0.1430446194225721002 ) ) ;
#31683 = VECTOR ( 'NONE', #64613, 39.37007874015748143 ) ;
#31685 = CARTESIAN_POINT ( 'NONE',  ( 0.5314960629921064994, 2.716535433070866645, 1.854472803289057836 ) ) ;
#31684 = CARTESIAN_POINT ( 'NONE',  ( 0.7939632545931766261, -0.3162353388693409650, -0.4822834645669289433 ) ) ;
#31686 = CARTESIAN_POINT ( 'NONE',  ( -1.397637795275589623, 0.07958543189024085140, 0.2665933059059887866 ) ) ;
#31687 = CARTESIAN_POINT ( 'NONE',  ( -0.006561679790025524116, -0.05778040916215560624, -0.4822834645669293319 ) ) ;
#31688 = CARTESIAN_POINT ( 'NONE',  ( 0.8595800524934390507, -0.08942795157528024563, -0.3641732283464568787 ) ) ;
#31689 = EDGE_CURVE ( 'NONE', #31856, #66355, #4419, .T. ) ;
#31690 = CARTESIAN_POINT ( 'NONE',  ( 1.030183727034121421, -0.05778040916215522460, 0.4822834645669289988 ) ) ;
#31691 = CARTESIAN_POINT ( 'NONE',  ( -0.3543307086614165824, -0.5511811023622047445, 6.969142054262312111E-17 ) ) ;
#31692 = CARTESIAN_POINT ( 'NONE',  ( -0.4790026246719154557, -0.3162353388693405765, 0.4822834645669290543 ) ) ;
#31693 = CARTESIAN_POINT ( 'NONE',  ( -1.587926509186350810, -0.004921259842519870586, -0.3153832671262229437 ) ) ;
#31694 = CARTESIAN_POINT ( 'NONE',  ( -1.299212598425196097, -0.6692913385826771977, 8.415575281601705876E-17 ) ) ;
#31695 = CARTESIAN_POINT ( 'NONE',  ( 0.9448818897637802916, -0.1870078740157480879, -0.4822834645669291653 ) ) ;
#31696 = CARTESIAN_POINT ( 'NONE',  ( 0.2867679344610366554, -0.2867679344610365999, -0.7250849325797394940 ) ) ;
#31697 = CARTESIAN_POINT ( 'NONE',  ( -1.437007874015747477, 0.07958543189024071263, -0.2665933059059888421 ) ) ;
#31698 =( BOUNDED_CURVE ( )  B_SPLINE_CURVE ( 2, ( #59472, #1825, #66217, #53143, #45998, #78440, #47250, #78856, #21181, #72530, #53564, #71694, #8968 ),
 .UNSPECIFIED., .F., .F. ) 
 B_SPLINE_CURVE_WITH_KNOTS ( ( 3, 2, 2, 2, 2, 2, 3 ),
 ( 0.5376696296615053328, 0.5378787878787878451, 0.5416666666666666297, 0.5454545454545454142, 0.5492424242424241987, 0.5530303030303029832, 0.5532394612475854956 ),
 .UNSPECIFIED. ) 
 CURVE ( )  GEOMETRIC_REPRESENTATION_ITEM ( )  RATIONAL_B_SPLINE_CURVE ( ( 0.9964447847208419695, 0.9981185001348091834, 1.000000000000000000, 0.9659258262890683122, 1.000000000000000000, 0.9659258262890683122, 1.000000000000000000, 0.9659258262890683122, 1.000000000000000000, 0.9659258262890683122, 1.000000000000000000, 0.9981185001348091834, 0.9964447847208420805 ) ) 
 REPRESENTATION_ITEM ( '' )  );
#31699 = CARTESIAN_POINT ( 'NONE',  ( 1.030613340552999135, 1.368770328279408144, 0.4436984845053965065 ) ) ;
#31700 = CARTESIAN_POINT ( 'NONE',  ( 0.8923884514435701520, -0.6046776061558809534, -0.2411417322834644161 ) ) ;
#31701 = CARTESIAN_POINT ( 'NONE',  ( 0.4724409448818898682, 2.892866454678787531E-17, -2.399606299212598604 ) ) ;
#31702 = AXIS2_PLACEMENT_3D ( 'NONE', #72983, #8598, #60762 ) ;
#31703 = CARTESIAN_POINT ( 'NONE',  ( -1.581364829396324945, -0.3162353388693405765, 0.4822834645669290543 ) ) ;
#31704 = CARTESIAN_POINT ( 'NONE',  ( 1.640419947506562393, -0.4281496062992124485, 0.4176697321401328655 ) ) ;
#31705 = CARTESIAN_POINT ( 'NONE',  ( -1.122047244094487306, -0.4536011799217367080, 0.2665933059059888421 ) ) ;
#31706 = CARTESIAN_POINT ( 'NONE',  ( 1.607611548556431069, -0.5511811023622048555, -0.09757992244046775898 ) ) ;
#31707 = CARTESIAN_POINT ( 'NONE',  ( -0.4199475065616791736, -0.6046776061558807314, 0.2411417322834647770 ) ) ;
#31708 = CARTESIAN_POINT ( 'NONE',  ( -0.6102362204724400829, -0.4536011799217368745, -0.2665933059059886201 ) ) ;
#31709 = CARTESIAN_POINT ( 'NONE',  ( -1.725721784776902190, -0.08942795157527998196, 0.3641732283464567121 ) ) ;
#31710 = CARTESIAN_POINT ( 'NONE',  ( 0.8333333333333340365, 0.1771653543307087075, -0.09757992244046823083 ) ) ;
#31711 = CARTESIAN_POINT ( 'NONE',  ( 1.069553805774278832, 0.2952755905511810774, -0.1292274648535930714 ) ) ;
#31712 = CYLINDRICAL_SURFACE ( 'NONE', #52840, 0.3937007874015748254 ) ;
#31713 = CARTESIAN_POINT ( 'NONE',  ( -0.08530183727034056085, -0.2845877964562159024, 0.3641732283464567677 ) ) ;
#31714 = MANIFOLD_SOLID_BREP ( 'Cut-Sweep1', #11102 ) ;
#31715 = CARTESIAN_POINT ( 'NONE',  ( 0.3608923884514443348, -0.6692913385826771977, 0.1292274648535927661 ) ) ;
#31716 = CARTESIAN_POINT ( 'NONE',  ( 0.6299212598425204535, -0.1870078740157479769, 0.3641732283464567677 ) ) ;
#31717 = CARTESIAN_POINT ( 'NONE',  ( 1.574803149606299746, -0.1870078740157479769, 0.4822834645669291653 ) ) ;
#31718 = CARTESIAN_POINT ( 'NONE',  ( -1.128608923884513837, 0.2306618581243847221, -0.2411417322834647770 ) ) ;
#31719 = CARTESIAN_POINT ( 'NONE',  ( -0.4658792650918627265, -0.05778040916215522460, 0.4822834645669289988 ) ) ;
#31720 = CARTESIAN_POINT ( 'NONE',  ( -0.1070741851644057135, 0.3996062992125985480, -0.4790026246719158998 ) ) ;
#31721 = CARTESIAN_POINT ( 'NONE',  ( 0.3996062992125984925, 0.1070741851644054637, -2.721128608923884418 ) ) ;
#31722 = CARTESIAN_POINT ( 'NONE',  ( 0.3871391076115492380, -0.05778040916215560624, -0.4822834645669293319 ) ) ;
#31723 = CARTESIAN_POINT ( 'NONE',  ( 0.9776902887139113929, 0.1771653543307087630, 0.09757992244046791164 ) ) ;
#31724 = CARTESIAN_POINT ( 'NONE',  ( -0.4986876640419939388, 0.2306618581243847221, -0.2411417322834647770 ) ) ;
#31725 = CARTESIAN_POINT ( 'NONE',  ( 0.3149606299212603933, -0.1870078740157479769, 0.4822834645669291653 ) ) ;
#31726 = CARTESIAN_POINT ( 'NONE',  ( 0.3460692066303959202, 0.1998031496062993295, -2.020997375328084100 ) ) ;
#31727 = CARTESIAN_POINT ( 'NONE',  ( -0.2891555358219911054, 0.2891555358219909388, -1.437007874015748143 ) ) ;
#31728 = CARTESIAN_POINT ( 'NONE',  ( -0.1998031496062991907, -0.3460692066303959757, -2.742782152230971437 ) ) ;
#31729 = LINE ( 'NONE', #38456, #51975 ) ;
#31730 = CARTESIAN_POINT ( 'NONE',  ( -0.1049643490035307020, 0.3917322834645669549, -0.9435695538057738974 ) ) ;
#31731 = CARTESIAN_POINT ( 'NONE',  ( -0.3674540682414692561, -0.5023911411419708095, -0.1820866141732282451 ) ) ;
#31732 = CARTESIAN_POINT ( 'NONE',  ( -1.233595800524933894, 0.2306618581243848609, 0.2411417322834645549 ) ) ;
#31733 = CARTESIAN_POINT ( 'NONE',  ( 0.1974969037888704704, 0.3420746716998660508, -2.583333333333333481 ) ) ;
#31734 = CARTESIAN_POINT ( 'NONE',  ( 0.8727034120734913358, -0.05778040916215522460, 0.4822834645669289988 ) ) ;
#31735 = CARTESIAN_POINT ( 'NONE',  ( 1.456692913385827515, 0.2952755905511811885, 0.000000000000000000 ) ) ;
#31736 = CARTESIAN_POINT ( 'NONE',  ( 0.6627296587926515548, 0.2952755905511811885, 0.1292274648535926551 ) ) ;
#31737 = CARTESIAN_POINT ( 'NONE',  ( -1.157146581871515012E-16, 0.4724409448818898682, -2.677165354330708347 ) ) ;
#31738 = AXIS2_PLACEMENT_3D ( 'NONE', #50721, #32201, #70498 ) ;
#31739 = CARTESIAN_POINT ( 'NONE',  ( 0.3460692066303959757, -0.1998031496062991907, -1.994750656167979086 ) ) ;
#31740 = DIRECTION ( 'NONE',  ( 0.000000000000000000, 0.000000000000000000, -1.000000000000000000 ) ) ;
#31741 = AXIS2_PLACEMENT_3D ( 'NONE', #7070, #13394, #33579 ) ;
#31742 = CARTESIAN_POINT ( 'NONE',  ( 0.6496062992125991586, 0.1660481256975885056, 0.3530559997133364547 ) ) ;
#31743 = EDGE_CURVE ( 'NONE', #2914, #79410, #78086, .T. ) ;
#31744 = CARTESIAN_POINT ( 'NONE',  ( 0.7086614173228352742, -0.1870078740157480879, -0.4822834645669291653 ) ) ;
#31745 = CARTESIAN_POINT ( 'NONE',  ( 0.6889763779527563470, 0.07958543189024071263, -0.2665933059059888421 ) ) ;
#31746 = CARTESIAN_POINT ( 'NONE',  ( 1.292650918635171564, -0.6692913385826773087, -0.1292274648535924053 ) ) ;
#31747 = CARTESIAN_POINT ( 'NONE',  ( -0.1958661417322836718, 0.3392501089628017219, 0.05971128608923875758 ) ) ;
#31748 = CARTESIAN_POINT ( 'NONE',  ( 0.5839895013123367340, -0.6692913385826773087, -0.1292274648535924053 ) ) ;
#31749 = CARTESIAN_POINT ( 'NONE',  ( 1.115485564304462551, -0.4281496062992127816, -0.4176697321401328100 ) ) ;
#31750 = CARTESIAN_POINT ( 'NONE',  ( 0.2362204724409456558, -0.1870078740157479769, 0.4822834645669291653 ) ) ;
#31751 = CARTESIAN_POINT ( 'NONE',  ( 1.377952755905512472, 0.1771653543307087630, 0.000000000000000000 ) ) ;
#31752 = CARTESIAN_POINT ( 'NONE',  ( -0.7611548556430438595, 0.2306618581243848609, 0.2411417322834645549 ) ) ;
#31753 = CARTESIAN_POINT ( 'NONE',  ( -0.8398950131233589023, -0.6046776061558809534, -0.2411417322834644161 ) ) ;
#31754 = CARTESIAN_POINT ( 'NONE',  ( 1.279527559055118724, 0.1660481256975885056, 0.3530559997133364547 ) ) ;
#31755 = CARTESIAN_POINT ( 'NONE',  ( 0.3392501089628018329, 0.1958661417322835607, -0.6883202099737534274 ) ) ;
#31756 = CARTESIAN_POINT ( 'NONE',  ( 0.3917322834645670104, 2.398668435337828261E-17, -1.527559055118110409 ) ) ;
#31757 = CARTESIAN_POINT ( 'NONE',  ( -0.1958661417322836718, 0.3392501089628017219, -2.839895013123359568 ) ) ;
#31758 = ORIENTED_EDGE ( 'NONE', *, *, #72915, .F. ) ;
#31759 = CARTESIAN_POINT ( 'NONE',  ( 0.3949938075777411073, -0.1058382717557499464, -2.946194225721785909 ) ) ;
#31760 = ORIENTED_EDGE ( 'NONE', *, *, #5222, .T. ) ;
#31761 = CARTESIAN_POINT ( 'NONE',  ( 1.646981627296588035, -0.3162353388693405765, 0.4822834645669290543 ) ) ;
#31762 = CIRCLE ( 'NONE', #15695, 1.968503937007874072 ) ;
#31763 = CARTESIAN_POINT ( 'NONE',  ( 1.312335958005249825, 0.1283753931104746893, -0.1820866141732285504 ) ) ;
#31764 = CARTESIAN_POINT ( 'NONE',  ( 0.1070741851644053527, 0.3996062992125986590, -1.568241469816272993 ) ) ;
#31765 = CARTESIAN_POINT ( 'NONE',  ( 1.312335958005250269, -0.5023911411419708095, 0.1820866141732285504 ) ) ;
#31766 = CARTESIAN_POINT ( 'NONE',  ( -0.1674892343164145203, -2.567464376874931580E-15, -0.4445507791589072832 ) ) ;
#31767 = CARTESIAN_POINT ( 'NONE',  ( 0.000000000000000000, 0.07874015748031502893, 0.000000000000000000 ) ) ;
#31768 = CARTESIAN_POINT ( 'NONE',  ( 0.4581547954228972763, 1.765968763542725251, 0.5309055118110234117 ) ) ;
#31769 = CARTESIAN_POINT ( 'NONE',  ( -0.3392501089628017219, -0.1958661417322836718, -0.9245406824146982228 ) ) ;
#31770 = CARTESIAN_POINT ( 'NONE',  ( -0.6233595800524928121, -0.2845877964562161244, -0.3641732283464567121 ) ) ;
#31771 = CARTESIAN_POINT ( 'NONE',  ( -1.692913385826770645, 0.1771653543307087630, 0.000000000000000000 ) ) ;
#31772 = CARTESIAN_POINT ( 'NONE',  ( -1.384514435695537005, -0.6692913385826773087, -0.1292274648535924053 ) ) ;
#31773 = CARTESIAN_POINT ( 'NONE',  ( 0.006561679790026889343, -0.05778040916215522460, 0.4822834645669289988 ) ) ;
#31774 = CARTESIAN_POINT ( 'NONE',  ( 1.568241469816273437, -0.3162353388693405765, 0.4822834645669290543 ) ) ;
#31775 = ORIENTED_EDGE ( 'NONE', *, *, #42014, .F. ) ;
#31776 = CYLINDRICAL_SURFACE ( 'NONE', #52739, 0.5120078740157480990 ) ;
#31777 = CARTESIAN_POINT ( 'NONE',  ( -0.3458507752293909498, 0.3458507752293907833, -1.909448818897637512 ) ) ;
#31778 = CARTESIAN_POINT ( 'NONE',  ( -0.4091458600556405756, 0.2362204724409446288, -2.703412073490813583 ) ) ;
#31779 = CARTESIAN_POINT ( 'NONE',  ( -0.6364829396325453192, -0.08942795157528024563, -0.3641732283464568787 ) ) ;
#31780 = CARTESIAN_POINT ( 'NONE',  ( -1.010498687664041384, 0.05413385826771666132, 0.4176697321401328100 ) ) ;
#31781 = CARTESIAN_POINT ( 'NONE',  ( 0.9842519685039378130, -0.6692913385826771977, 8.415575281601705876E-17 ) ) ;
#31782 = ORIENTED_EDGE ( 'NONE', *, *, #78407, .T. ) ;
#31784 = DIRECTION ( 'NONE',  ( -0.000000000000000000, -1.000000000000000000, -0.000000000000000000 ) ) ;
#31783 = CARTESIAN_POINT ( 'NONE',  ( 0.4724409448818898682, 2.892866454678787531E-17, -0.6673228346456693272 ) ) ;
#31785 = CARTESIAN_POINT ( 'NONE',  ( 1.253280839895013710, -0.05778040916215560624, -0.4822834645669293319 ) ) ;
#31786 = CARTESIAN_POINT ( 'NONE',  ( -1.397637795275589623, 0.1660481256975885056, 0.3530559997133364547 ) ) ;
#31787 = CARTESIAN_POINT ( 'NONE',  ( -0.1049643490035301746, -0.3917322834645670659, -0.6246526002286596491 ) ) ;
#31788 = CARTESIAN_POINT ( 'NONE',  ( -0.5183727034120726440, -0.5511811023622048555, -0.09757992244046775898 ) ) ;
#31789 = CARTESIAN_POINT ( 'NONE',  ( -0.3917322834645670104, -7.196005306013484475E-17, -0.9114173228346457156 ) ) ;
#31790 = CARTESIAN_POINT ( 'NONE',  ( -0.3149606299212590610, -0.1870078740157480601, -0.3641732283464567677 ) ) ;
#31791 = CARTESIAN_POINT ( 'NONE',  ( -0.1049868766404193215, 0.1283753931104746893, -0.1820866141732285504 ) ) ;
#31792 = CARTESIAN_POINT ( 'NONE',  ( 0.1443569553805781891, -0.4281496062992124485, 0.4176697321401328655 ) ) ;
#31793 = CARTESIAN_POINT ( 'NONE',  ( -0.8398950131233585692, 0.1283753931104748280, 0.1820866141732283561 ) ) ;
#31794 = CARTESIAN_POINT ( 'NONE',  ( -9.594673741351313045E-17, 0.3917322834645670104, -2.826771653543306506 ) ) ;
#31795 = CARTESIAN_POINT ( 'NONE',  ( 1.338582677165355062, -0.1870078740157480879, -0.4822834645669291653 ) ) ;
#31796 = CIRCLE ( 'NONE', #49291, 0.4822834645669291653 ) ;
#31797 = CARTESIAN_POINT ( 'NONE',  ( -1.509186351706035767, -0.4281496062992124485, 0.4176697321401328655 ) ) ;
#31798 = AXIS2_PLACEMENT_3D ( 'NONE', #926, #14393, #47175 ) ;
#31799 = CARTESIAN_POINT ( 'NONE',  ( -0.1265901696524993347, 0.4724409448818895907, -1.028215223097112663 ) ) ;
#31800 = VECTOR ( 'NONE', #58221, 39.37007874015748143 ) ;
#31801 = CARTESIAN_POINT ( 'NONE',  ( -0.2887139107611542133, 0.2306618581243848609, 0.2411417322834645549 ) ) ;
#31802 = CARTESIAN_POINT ( 'NONE',  ( -1.141732283464566011, 0.2952755905511811885, 0.000000000000000000 ) ) ;
#31803 = CARTESIAN_POINT ( 'NONE',  ( 1.095800524934383846, -0.08942795157528024563, -0.3641732283464568787 ) ) ;
#31804 = CARTESIAN_POINT ( 'NONE',  ( -0.3149606299212590610, -0.1870078740157479769, 0.3641732283464567677 ) ) ;
#31805 = CARTESIAN_POINT ( 'NONE',  ( -0.7480314960629914633, 0.2952755905511811885, 0.000000000000000000 ) ) ;
#31806 = CARTESIAN_POINT ( 'NONE',  ( -1.279527559055116948, 0.1660481256975883668, -0.3530559997133364547 ) ) ;
#31807 = CARTESIAN_POINT ( 'NONE',  ( -0.4056338187708053988, 4.650002066398565039E-15, -0.3627989612356129490 ) ) ;
#31808 = CARTESIAN_POINT ( 'NONE',  ( 1.338582677165355062, -0.1870078740157479769, 0.3641732283464567677 ) ) ;
#31809 = CARTESIAN_POINT ( 'NONE',  ( -0.2952755905511803003, -0.5400638737290845981, -0.3530559997133363437 ) ) ;
#31810 = CARTESIAN_POINT ( 'NONE',  ( -1.706036745406823485, 0.2306618581243848609, 0.2411417322834645549 ) ) ;
#31811 = ORIENTED_EDGE ( 'NONE', *, *, #22393, .F. ) ;
#31812 = CARTESIAN_POINT ( 'NONE',  ( -0.3460692066303960313, 0.1998031496062989965, -2.307742782152230721 ) ) ;
#31813 = CARTESIAN_POINT ( 'NONE',  ( -0.9055118110236215490, -0.5511811023622047445, 6.969142054262312111E-17 ) ) ;
#31814 = CARTESIAN_POINT ( 'NONE',  ( 0.7874015748031503170, -0.1870078740157479769, 0.4822834645669291653 ) ) ;
#31815 = CARTESIAN_POINT ( 'NONE',  ( -1.082677165354329896, 0.07958543189024085140, 0.2665933059059887866 ) ) ;
#31816 = CARTESIAN_POINT ( 'NONE',  ( 0.1998031496062994128, -0.3460692066303957537, -1.428477690288713964 ) ) ;
#31817 = CARTESIAN_POINT ( 'NONE',  ( -1.135170603674539924, -0.6692913385826771977, 0.1292274648535927661 ) ) ;
#31818 = CARTESIAN_POINT ( 'NONE',  ( 0.9908136482939640111, -0.6692913385826771977, 0.1292274648535927661 ) ) ;
#31819 = CARTESIAN_POINT ( 'NONE',  ( 0.8398950131233602345, -0.6046776061558807314, 0.2411417322834647770 ) ) ;
#31820 = CARTESIAN_POINT ( 'NONE',  ( 1.601049868766404982, 0.2306618581243848609, 0.2411417322834645549 ) ) ;
#31821 = CARTESIAN_POINT ( 'NONE',  ( -1.338582677165353729, -0.1870078740157480601, -0.3641732283464567677 ) ) ;
#31822 = CARTESIAN_POINT ( 'NONE',  ( -0.1998031496062994405, 0.3460692066303957537, -0.5623359580052492701 ) ) ;
#31823 = CARTESIAN_POINT ( 'NONE',  ( -0.3996062992125986035, -0.1070741851644056997, -0.8333333333333332593 ) ) ;
#31824 = CARTESIAN_POINT ( 'NONE',  ( 0.1058382717557499880, 0.3949938075777411073, -0.1509186351706037210 ) ) ;
#31825 = CARTESIAN_POINT ( 'NONE',  ( 0.4567021909596065687, 1.408136488465070002, 2.593432289528808887 ) ) ;
#31826 = CARTESIAN_POINT ( 'NONE',  ( 1.345144356955381593, -0.08942795157527998196, 0.3641732283464567121 ) ) ;
#31827 = CARTESIAN_POINT ( 'NONE',  ( 0.6167979002624678353, -0.3690944881889763329, 0.3153832671262228327 ) ) ;
#31828 = CARTESIAN_POINT ( 'NONE',  ( -0.01312335958005186876, -0.4281496062992124485, 0.4176697321401328655 ) ) ;
#31829 = CARTESIAN_POINT ( 'NONE',  ( -3.937007874015748143, 2.755905511811024056, -0.5314960629921260393 ) ) ;
#31830 = CARTESIAN_POINT ( 'NONE',  ( 0.3949938075777409408, -0.1058382717557499186, -1.133202099737532720 ) ) ;
#31831 = CARTESIAN_POINT ( 'NONE',  ( 0.2362204724409456558, -0.1870078740157479769, 0.3641732283464567677 ) ) ;
#31832 = ADVANCED_FACE ( 'NONE', ( #28880 ), #134, .F. ) ;
#31833 = CARTESIAN_POINT ( 'NONE',  ( -0.8005249343832011588, 0.05413385826771626580, -0.4176697321401330321 ) ) ;
#31834 = CARTESIAN_POINT ( 'NONE',  ( -1.095800524934382292, -0.3162353388693409650, -0.4822834645669289433 ) ) ;
#31835 = CARTESIAN_POINT ( 'NONE',  ( 0.7414698162729663755, 0.2952755905511811885, 0.1292274648535926551 ) ) ;
#31836 = CARTESIAN_POINT ( 'NONE',  ( -0.4724409448818899238, 0.1265901696524986686, -1.607611548556430403 ) ) ;
#31837 = CARTESIAN_POINT ( 'NONE',  ( 0.3460692066303959202, 0.1998031496062993295, -2.650918635170603554 ) ) ;
#31838 = ORIENTED_EDGE ( 'NONE', *, *, #40285, .T. ) ;
#31839 = VERTEX_POINT ( 'NONE', #22157 ) ;
#31840 = CARTESIAN_POINT ( 'NONE',  ( -1.325459317585300889, -0.4281496062992127816, -0.4176697321401328100 ) ) ;
#31841 = CARTESIAN_POINT ( 'NONE',  ( -0.8005249343832011588, 0.05413385826771626580, -0.4176697321401330321 ) ) ;
#31843 = CARTESIAN_POINT ( 'NONE',  ( -0.6758530183727028406, 0.2952755905511811885, 0.1292274648535926551 ) ) ;
#31842 = CARTESIAN_POINT ( 'NONE',  ( -0.8727034120734901146, -0.2845877964562159024, 0.3641732283464567677 ) ) ;
#31844 = CARTESIAN_POINT ( 'NONE',  ( -0.3917322834645669549, -7.196005306013483243E-17, -2.166647350884827183 ) ) ;
#31845 = CARTESIAN_POINT ( 'NONE',  ( -0.3805774278215216522, 0.05413385826771666132, 0.4176697321401328100 ) ) ;
#31846 = CARTESIAN_POINT ( 'NONE',  ( 1.528871391076116026, -0.6692913385826773087, -0.1292274648535924053 ) ) ;
#31847 = CARTESIAN_POINT ( 'NONE',  ( -0.7086614173228339419, -0.1870078740157480879, -0.4822834645669291653 ) ) ;
#31848 = CARTESIAN_POINT ( 'NONE',  ( 0.4527559055118117182, -0.5400638737290844871, 0.3530559997133364547 ) ) ;
#31849 = CARTESIAN_POINT ( 'NONE',  ( -0.8070866141732276899, 0.1660481256975883668, -0.3530559997133364547 ) ) ;
#31850 = VECTOR ( 'NONE', #1836, 39.37007874015748143 ) ;
#31851 = CARTESIAN_POINT ( 'NONE',  ( 0.1958661417322834775, 0.3392501089628018884, -1.553805774278215202 ) ) ;
#31852 = CARTESIAN_POINT ( 'NONE',  ( -0.7020997375328074108, -0.08942795157527998196, 0.3641732283464567121 ) ) ;
#31853 = ORIENTED_EDGE ( 'NONE', *, *, #47538, .F. ) ;
#31854 = CARTESIAN_POINT ( 'NONE',  ( -0.3420746716998661618, 0.1974969037888702206, -1.916010498687664043 ) ) ;
#31855 = AXIS2_PLACEMENT_3D ( 'NONE', #31903, #76535, #32316 ) ;
#31856 = VERTEX_POINT ( 'NONE', #42327 ) ;
#31857 = LINE ( 'NONE', #77314, #56977 ) ;
#31858 = PRESENTATION_LAYER_ASSIGNMENT (  '', '', ( #2325 ) ) ;
#31859 = AXIS2_PLACEMENT_3D ( 'NONE', #29518, #62327, #23613 ) ;
#31860 = CARTESIAN_POINT ( 'NONE',  ( -1.240157480314959759, -0.5400638737290845981, -0.3530559997133363437 ) ) ;
#31861 = CARTESIAN_POINT ( 'NONE',  ( -0.9186351706036736120, -0.6046776061558809534, -0.2411417322834644161 ) ) ;
#31862 = CARTESIAN_POINT ( 'NONE',  ( 4.893765752498283924E-17, -0.3996062992125986035, -0.3937007874015748254 ) ) ;
#31863 = CARTESIAN_POINT ( 'NONE',  ( -1.095800524934382292, -0.05778040916215522460, 0.4822834645669289988 ) ) ;
#31864 = CARTESIAN_POINT ( 'NONE',  ( -1.115485564304461219, -0.4281496062992124485, 0.4176697321401328655 ) ) ;
#31865 = LINE ( 'NONE', #30209, #5528 ) ;
#31866 = CARTESIAN_POINT ( 'NONE',  ( 0.000000000000000000, 0.5905511811023621549, -0.1574803149606299746 ) ) ;
#31867 = CARTESIAN_POINT ( 'NONE',  ( 0.4396325459317593221, 0.1771653543307087075, -0.09757992244046823083 ) ) ;
#31868 = CARTESIAN_POINT ( 'NONE',  ( 1.603475055217291612, 0.4410854135902468887, -0.04573490813648244807 ) ) ;
#31869 = CARTESIAN_POINT ( 'NONE',  ( 0.3917322834645670104, -0.1049643490035303411, -0.3536745406824148286 ) ) ;
#31870 = CARTESIAN_POINT ( 'NONE',  ( -0.1771653543307080136, -0.4536011799217367080, 0.2665933059059888421 ) ) ;
#31871 = CARTESIAN_POINT ( 'NONE',  ( -0.7742782152230962556, -0.4281496062992127816, -0.4176697321401328100 ) ) ;
#31872 = CARTESIAN_POINT ( 'NONE',  ( 1.371391076115485719, -0.6692913385826773087, -0.1292274648535924053 ) ) ;
#31873 = CARTESIAN_POINT ( 'NONE',  ( -0.5118110236220466680, 0.2952755905511811885, 0.000000000000000000 ) ) ;
#31874 = EDGE_LOOP ( 'NONE', ( #61744, #56388, #55522, #23401 ) ) ;
#31875 = ORIENTED_EDGE ( 'NONE', *, *, #8916, .T. ) ;
#31876 = CARTESIAN_POINT ( 'NONE',  ( -0.2925321140481932369, 0.2925321140481931259, -2.143700787401574548 ) ) ;
#31877 = CARTESIAN_POINT ( 'NONE',  ( -0.6364829396325453192, -0.05778040916215560624, -0.4822834645669293319 ) ) ;
#31878 = CARTESIAN_POINT ( 'NONE',  ( 1.443569553805774897, 0.2306618581243848609, 0.2411417322834645549 ) ) ;
#31879 = CARTESIAN_POINT ( 'NONE',  ( -1.266404199475064773, -0.2845877964562159024, 0.3641732283464567677 ) ) ;
#31880 = CARTESIAN_POINT ( 'NONE',  ( -1.325459317585300889, -0.4281496062992127816, -0.4176697321401328100 ) ) ;
#31881 = CARTESIAN_POINT ( 'NONE',  ( -0.2362204724409447953, -0.4091458600556404646, -0.6955380577427822120 ) ) ;
#31882 = CARTESIAN_POINT ( 'NONE',  ( 2.131037067002786944, 1.408244132531265791, 0.4567322424080934584 ) ) ;
#31883 = CARTESIAN_POINT ( 'NONE',  ( 0.2867679344610365999, -0.2867679344610365444, -2.860236220472440749 ) ) ;
#31884 = CARTESIAN_POINT ( 'NONE',  ( 4.797336870675656522E-17, -0.3917322834645670104, -2.210629921259842590 ) ) ;
#31885 = CARTESIAN_POINT ( 'NONE',  ( 0.3018372703412079971, 0.05413385826771626580, -0.4176697321401330321 ) ) ;
#31886 = CARTESIAN_POINT ( 'NONE',  ( -1.095800524934382292, -0.2845877964562161244, -0.3641732283464567121 ) ) ;
#31887 = CARTESIAN_POINT ( 'NONE',  ( -0.6036745406824141069, 0.2306618581243848609, 0.2411417322834645549 ) ) ;
#31888 = CARTESIAN_POINT ( 'NONE',  ( -0.4724409448818898682, -8.678599364036362592E-17, -2.793307086614173151 ) ) ;
#31889 = CARTESIAN_POINT ( 'NONE',  ( -0.8989501312335946848, 0.2952755905511810774, -0.1292274648535930714 ) ) ;
#31890 = CARTESIAN_POINT ( 'NONE',  ( -0.9514435695538050464, -0.3162353388693405765, 0.4822834645669290543 ) ) ;
#31891 = CARTESIAN_POINT ( 'NONE',  ( 0.1974969037888706092, -0.3420746716998660508, -2.373359580052493811 ) ) ;
#31892 = CARTESIAN_POINT ( 'NONE',  ( 1.043307086614173818, -0.4536011799217368745, -0.2665933059059886201 ) ) ;
#31893 = CARTESIAN_POINT ( 'NONE',  ( -0.6692913385826764205, -0.5511811023622047445, 6.969142054262312111E-17 ) ) ;
#31894 = CARTESIAN_POINT ( 'NONE',  ( 0.5971128608923891301, 0.1771653543307087075, -0.09757992244046823083 ) ) ;
#31895 = CARTESIAN_POINT ( 'NONE',  ( -1.522309711286088607, 0.2306618581243847221, -0.2411417322834647770 ) ) ;
#31896 = CARTESIAN_POINT ( 'NONE',  ( 1.430446194225722500, 0.05413385826771666132, 0.4176697321401328100 ) ) ;
#31897 = CARTESIAN_POINT ( 'NONE',  ( 0.4658792650918641698, -0.08942795157528024563, -0.3641732283464568787 ) ) ;
#31898 = CARTESIAN_POINT ( 'NONE',  ( 0.1049643490035303689, 0.3917322834645670104, -1.560367454068241511 ) ) ;
#31899 = CARTESIAN_POINT ( 'NONE',  ( -0.8661417322834640276, -0.1870078740157479769, 0.4822834645669291653 ) ) ;
#31900 = CARTESIAN_POINT ( 'NONE',  ( 1.128608923884514947, 0.2306618581243848609, 0.2411417322834645549 ) ) ;
#31901 = CARTESIAN_POINT ( 'NONE',  ( -0.4724409448818898682, -8.678599364036362592E-17, 0.04133858267716534335 ) ) ;
#31902 = CARTESIAN_POINT ( 'NONE',  ( 0.05905511811023709395, -0.4536011799217367080, 0.2665933059059888421 ) ) ;
#31903 = CARTESIAN_POINT ( 'NONE',  ( 0.000000000000000000, 2.755905511811024056, 0.000000000000000000 ) ) ;
#31904 = CARTESIAN_POINT ( 'NONE',  ( 0.4724409448818904789, -0.1870078740157480879, -0.4822834645669291653 ) ) ;
#31905 = DIRECTION ( 'NONE',  ( 1.000000000000000000, 0.000000000000000000, 0.000000000000000000 ) ) ;
#31906 = CARTESIAN_POINT ( 'NONE',  ( 1.010498687664042716, -0.004921259842519870586, -0.3153832671262229437 ) ) ;
#31907 = CARTESIAN_POINT ( 'NONE',  ( 0.3608923884514443348, 0.1771653543307087075, -0.09757992244046823083 ) ) ;
#31908 = CARTESIAN_POINT ( 'NONE',  ( 0.08530183727034192087, -0.05778040916215522460, 0.4822834645669289988 ) ) ;
#31909 = CARTESIAN_POINT ( 'NONE',  ( -1.417322834645668772, -0.1870078740157479769, 0.4822834645669291653 ) ) ;
#31910 = CARTESIAN_POINT ( 'NONE',  ( -0.6102362204724400829, -0.4536011799217368745, -0.2665933059059886201 ) ) ;
#31911 = FACE_OUTER_BOUND ( 'NONE', #80145, .T. ) ;
#31912 = CARTESIAN_POINT ( 'NONE',  ( -0.4199475065616791736, -0.6046776061558807314, 0.2411417322834647770 ) ) ;
#31913 = CARTESIAN_POINT ( 'NONE',  ( -0.1998031496062994405, 0.3460692066303957537, -1.349737532808398921 ) ) ;
#31914 = CARTESIAN_POINT ( 'NONE',  ( 0.3917322834645670104, 2.398668435337828261E-17, -2.250000000000000000 ) ) ;
#31915 = CARTESIAN_POINT ( 'NONE',  ( 0.1771653543307093182, 0.07958543189024085140, 0.2665933059059887866 ) ) ;
#31917 = COLOUR_RGB ( '', 0.66274510, 0.83137255, 0.94901961) ;
#31916 = CARTESIAN_POINT ( 'NONE',  ( -0.4527559055118102749, -0.5400638737290845981, -0.3530559997133363437 ) ) ;
#31918 = CARTESIAN_POINT ( 'NONE',  ( -1.187664041994749731, -0.3162353388693405765, 0.4822834645669290543 ) ) ;
#31919 = CARTESIAN_POINT ( 'NONE',  ( -1.122047244094487306, 0.07958543189024071263, -0.2665933059059888421 ) ) ;
#31920 = FACE_OUTER_BOUND ( 'NONE', #14510, .T. ) ;
#31921 = CARTESIAN_POINT ( 'NONE',  ( -0.6496062992125976043, 0.1660481256975883668, -0.3530559997133364547 ) ) ;
#31922 = CARTESIAN_POINT ( 'NONE',  ( -1.036745406824146176, -0.3690944881889763329, 0.3153832671262228327 ) ) ;
#31923 = CARTESIAN_POINT ( 'NONE',  ( -1.450131233595799651, -0.5511811023622046335, 0.09757992244046803654 ) ) ;
#31924 = CARTESIAN_POINT ( 'NONE',  ( 1.240157480314961314, -0.5400638737290844871, 0.3530559997133364547 ) ) ;
#31925 = DIRECTION ( 'NONE',  ( 9.381338752702771457E-17, -0.6427876096865352551, 0.7660444431189814551 ) ) ;
#31926 = CARTESIAN_POINT ( 'NONE',  ( 0.1049643490035303967, 0.3917322834645670659, -2.037420890584989319 ) ) ;
#31927 = ORIENTED_EDGE ( 'NONE', *, *, #45702, .F. ) ;
#31928 = CARTESIAN_POINT ( 'NONE',  ( -0.2255212960314310344, -4.992347309556208597E-15, 0.4118484887281982920 ) ) ;
#31929 = CARTESIAN_POINT ( 'NONE',  ( -1.496062992125983815, -0.1870078740157480879, -0.4822834645669291653 ) ) ;
#31930 = CARTESIAN_POINT ( 'NONE',  ( -0.9776902887139098386, -0.6692913385826771977, 0.1292274648535927661 ) ) ;
#31931 = CARTESIAN_POINT ( 'NONE',  ( 1.535433070866142335, -0.6692913385826771977, 8.415575281601705876E-17 ) ) ;
#31932 = CARTESIAN_POINT ( 'NONE',  ( -0.2867679344610365999, 0.2867679344610364889, -2.151574803149605586 ) ) ;
#31933 = CARTESIAN_POINT ( 'NONE',  ( -0.1584414948821151747, 0.3588842212258044340, -1.220472440944881942 ) ) ;
#31934 = EDGE_CURVE ( 'NONE', #34136, #36844, #47816, .T. ) ;
#31935 = CARTESIAN_POINT ( 'NONE',  ( 1.056430446194226658, 0.2952755905511811885, 0.1292274648535926551 ) ) ;
#31936 = CARTESIAN_POINT ( 'NONE',  ( 0.1246719160104994284, 0.2952755905511810774, -0.1292274648535930714 ) ) ;
#31937 = CARTESIAN_POINT ( 'NONE',  ( 0.000000000000000000, 0.000000000000000000, -2.755905511811024056 ) ) ;
#31938 = LINE ( 'NONE', #38666, #68061 ) ;
#31939 = CARTESIAN_POINT ( 'NONE',  ( 1.115485564304462551, -0.004921259842519576551, 0.3153832671262227771 ) ) ;
#31940 = CARTESIAN_POINT ( 'NONE',  ( 0.1070741851644054915, -0.3996062992125986035, -1.187664041994750619 ) ) ;
#31941 = ORIENTED_EDGE ( 'NONE', *, *, #69249, .F. ) ;
#31942 = CARTESIAN_POINT ( 'NONE',  ( -0.3917322834645670659, -7.196005306013484475E-17, -0.03610855462698352170 ) ) ;
#31943 = ORIENTED_EDGE ( 'NONE', *, *, #70814, .F. ) ;
#31944 = CARTESIAN_POINT ( 'NONE',  ( -0.1771653543307080136, -0.5400638737290844871, 0.3530559997133364547 ) ) ;
#31945 = CARTESIAN_POINT ( 'NONE',  ( -0.9186351706036736120, 0.2306618581243848609, 0.2411417322834645549 ) ) ;
#31946 = CARTESIAN_POINT ( 'NONE',  ( -1.541994750656167090, -0.6692913385826773087, -0.1292274648535924053 ) ) ;
#31947 = CARTESIAN_POINT ( 'NONE',  ( 0.7939632545931766261, -0.3162353388693409650, -0.4822834645669289433 ) ) ;
#31948 = CARTESIAN_POINT ( 'NONE',  ( -1.568241469816272105, -0.2845877964562161244, -0.3641732283464567121 ) ) ;
#31949 = CARTESIAN_POINT ( 'NONE',  ( 1.351706036745407458, -0.4281496062992127816, -0.4176697321401328100 ) ) ;
#31950 = CARTESIAN_POINT ( 'NONE',  ( -0.5118110236220466680, 0.2952755905511811885, 0.000000000000000000 ) ) ;
#31951 = CARTESIAN_POINT ( 'NONE',  ( 0.4986876640419954376, 0.2306618581243848609, 0.2411417322834645549 ) ) ;
#31952 = CARTESIAN_POINT ( 'NONE',  ( -1.115485564304461219, 0.05413385826771626580, -0.4176697321401330321 ) ) ;
#31953 = CARTESIAN_POINT ( 'NONE',  ( 1.253280839895013710, -0.3162353388693405765, 0.4822834645669290543 ) ) ;
#31954 = CARTESIAN_POINT ( 'NONE',  ( 1.476377952755906442, -0.5400638737290844871, 0.3530559997133364547 ) ) ;
#31955 = CARTESIAN_POINT ( 'NONE',  ( -0.01312335958005186876, -0.4281496062992124485, 0.4176697321401328655 ) ) ;
#31956 = CARTESIAN_POINT ( 'NONE',  ( -0.3392501089628019995, 0.1958661417322832277, -0.01837270341207344546 ) ) ;
#31957 = CARTESIAN_POINT ( 'NONE',  ( 0.3674540682414705883, -0.5023911411419708095, 0.1820866141732285504 ) ) ;
#31958 = ORIENTED_EDGE ( 'NONE', *, *, #59409, .F. ) ;
#31959 = CARTESIAN_POINT ( 'NONE',  ( -9.674558042662121740E-17, 0.3949938075777409963, -0.6299212598425196763 ) ) ;
#31960 = EDGE_LOOP ( 'NONE', ( #71748, #28458, #46666, #292 ) ) ;
#31961 = CARTESIAN_POINT ( 'NONE',  ( -0.1837270341207343505, -0.5023911411419708095, 0.1820866141732285504 ) ) ;
#31962 = CARTESIAN_POINT ( 'NONE',  ( 2.867114984585486859, 1.070443199938755807, -0.08545185031212575166 ) ) ;
#31963 = CARTESIAN_POINT ( 'NONE',  ( 0.3018372703412079971, -0.4281496062992124485, 0.4176697321401328655 ) ) ;
#31964 = CARTESIAN_POINT ( 'NONE',  ( -0.1443569553805768291, 0.05413385826771666132, 0.4176697321401328100 ) ) ;
#31965 = CARTESIAN_POINT ( 'NONE',  ( -0.4265091863517051496, 0.2952755905511810774, -0.1292274648535930714 ) ) ;
#31966 = CARTESIAN_POINT ( 'NONE',  ( 0.3917322834645670659, 2.398668435337828261E-17, -1.532171546752967739 ) ) ;
#31967 = CARTESIAN_POINT ( 'NONE',  ( -1.089238845144356427, -0.4281496062992127816, -0.4176697321401328100 ) ) ;
#31968 = CARTESIAN_POINT ( 'NONE',  ( 4.797336870675656522E-17, -0.3917322834645670104, -2.683070866141731958 ) ) ;
#31969 = CARTESIAN_POINT ( 'NONE',  ( 0.7086614173228352742, -0.1870078740157480601, -0.3641732283464567677 ) ) ;
#31970 = CARTESIAN_POINT ( 'NONE',  ( 1.069553805774278832, 0.2952755905511810774, -0.1292274648535930714 ) ) ;
#31971 = CARTESIAN_POINT ( 'NONE',  ( 0.7020997375328090762, -0.3162353388693405765, 0.4822834645669290543 ) ) ;
#31972 = EDGE_CURVE ( 'NONE', #6163, #5170, #82841, .T. ) ;
#31973 = CARTESIAN_POINT ( 'NONE',  ( -0.3460692066303958092, -0.1998031496062994683, -0.8398950131233595684 ) ) ;
#31974 = CARTESIAN_POINT ( 'NONE',  ( -1.207349081364828880, 0.2306618581243847221, -0.2411417322834647770 ) ) ;
#31975 = CARTESIAN_POINT ( 'NONE',  ( 0.2925321140481932369, -0.2925321140481931814, -0.1751968503937007537 ) ) ;
#31976 = CARTESIAN_POINT ( 'NONE',  ( 0.1998031496062992463, 0.3460692066303959202, -0.2211286089238845565 ) ) ;
#31977 = CARTESIAN_POINT ( 'NONE',  ( -0.04593175853018302557, -0.6692913385826773087, -0.1292274648535924053 ) ) ;
#31978 = CARTESIAN_POINT ( 'NONE',  ( -0.3996062992125987146, 0.1070741851644051862, -2.709973753280840114 ) ) ;
#31979 = CARTESIAN_POINT ( 'NONE',  ( -9.594673741351313045E-17, 0.3917322834645670104, -1.659448818897637734 ) ) ;
#31980 = CARTESIAN_POINT ( 'NONE',  ( 1.437007874015748810, 0.1660481256975885056, 0.3530559997133364547 ) ) ;
#31981 = CONICAL_SURFACE ( 'NONE', #79064, 3.307086614173228689, 0.7853981633974500554 ) ;
#31982 = CARTESIAN_POINT ( 'NONE',  ( 1.200787401574803681, 0.1660481256975885056, 0.3530559997133364547 ) ) ;
#31983 = CARTESIAN_POINT ( 'NONE',  ( 0.1181102362204730916, 0.1771653543307087630, 0.000000000000000000 ) ) ;
#31984 = CARTESIAN_POINT ( 'NONE',  ( 0.7349081364829402885, -0.6046776061558809534, -0.2411417322834644161 ) ) ;
#31985 = CARTESIAN_POINT ( 'NONE',  ( 0.2362204724409451007, -0.4091458600556402980, -1.585958005249344049 ) ) ;
#31986 = CARTESIAN_POINT ( 'NONE',  ( 0.1443569553805781891, -0.004921259842519870586, -0.3153832671262229437 ) ) ;
#31987 = CARTESIAN_POINT ( 'NONE',  ( 0.5774278215223103139, -0.6046776061558809534, -0.2411417322834644161 ) ) ;
#31988 = CARTESIAN_POINT ( 'NONE',  ( 0.3420746716998660508, 0.1974969037888705814, -0.9954068241469814504 ) ) ;
#31989 = CARTESIAN_POINT ( 'NONE',  ( -1.128608923884513837, -0.6046776061558807314, 0.2411417322834647770 ) ) ;
#31990 = CARTESIAN_POINT ( 'NONE',  ( 0.9251968503937015864, -0.4536011799217367080, 0.2665933059059888421 ) ) ;
#31991 = CARTESIAN_POINT ( 'NONE',  ( -1.154855643044618851, 0.2306618581243848609, 0.2411417322834645549 ) ) ;
#31992 = CARTESIAN_POINT ( 'NONE',  ( -0.2624671916010490880, 0.2306618581243847221, -0.2411417322834647770 ) ) ;
#31993 = B_SPLINE_CURVE_WITH_KNOTS ( 'NONE', 3,
 ( #62872, #63689, #81834, #76335 ),
 .UNSPECIFIED., .F., .F.,
 ( 4, 4 ),
 ( 0.000000000000000000, 0.001510660848369282418 ),
 .UNSPECIFIED. ) ;
#31994 = CARTESIAN_POINT ( 'NONE',  ( -0.4002624671916004129, -0.2845877964562159024, 0.3641732283464567677 ) ) ;
#31995 = CARTESIAN_POINT ( 'NONE',  ( -0.5314960629921122726, 2.755905511811024056, -3.937007874015763687 ) ) ;
#31996 = CARTESIAN_POINT ( 'NONE',  ( -0.4396325459317579898, 0.2952755905511811885, 0.1292274648535926551 ) ) ;
#31997 = CARTESIAN_POINT ( 'NONE',  ( 0.3083989501312343062, -0.2845877964562159024, 0.3641732283464567677 ) ) ;
#31998 = CARTESIAN_POINT ( 'NONE',  ( -0.3460692066303957537, -0.1998031496062994405, -2.019028871391076230 ) ) ;
#31999 = CARTESIAN_POINT ( 'NONE',  ( 0.04593175853018440641, -0.6692913385826771977, 0.1292274648535927661 ) ) ;
#32000 = EDGE_CURVE ( 'NONE', #81066, #78139, #35203, .T. ) ;
#32001 = CARTESIAN_POINT ( 'NONE',  ( 0.1958661417322834497, 0.3392501089628018329, -1.484232652722097923 ) ) ;
#32002 = CARTESIAN_POINT ( 'NONE',  ( 1.187664041994751285, -0.08942795157527998196, 0.3641732283464567121 ) ) ;
#32003 = CARTESIAN_POINT ( 'NONE',  ( 0.000000000000000000, 0.000000000000000000, -2.755905511811024056 ) ) ;
#32004 = CARTESIAN_POINT ( 'NONE',  ( -0.6364829396325453192, -0.2845877964562159024, 0.3641732283464567677 ) ) ;
#32005 = CARTESIAN_POINT ( 'NONE',  ( -0.6299212598425188991, -0.1870078740157479769, 0.3641732283464567677 ) ) ;
#32006 = CARTESIAN_POINT ( 'NONE',  ( -0.8398950131233585692, 0.2306618581243848609, 0.2411417322834645549 ) ) ;
#32007 = CARTESIAN_POINT ( 'NONE',  ( -0.1837270341207343505, -0.6046776061558807314, 0.2411417322834647770 ) ) ;
#32008 = CARTESIAN_POINT ( 'NONE',  ( 0.6299212598425204535, -0.1870078740157480601, -0.3641732283464567677 ) ) ;
#32009 = CARTESIAN_POINT ( 'NONE',  ( -0.2371566215357294172, 0.1759343135753352327, 5.725906639596367143 ) ) ;
#32010 = CARTESIAN_POINT ( 'NONE',  ( 1.364829396325459854, -0.5023911411419708095, -0.1820866141732282451 ) ) ;
#32011 = CARTESIAN_POINT ( 'NONE',  ( 0.7152230971128616943, -0.05778040916215522460, 0.4822834645669289988 ) ) ;
#32012 = CARTESIAN_POINT ( 'NONE',  ( 4.893765752498283308E-17, -0.3996062992125985480, 0.001968503937007862279 ) ) ;
#32013 = CARTESIAN_POINT ( 'NONE',  ( -0.2624671916010490880, 0.2306618581243847221, -0.2411417322834647770 ) ) ;
#32014 = CARTESIAN_POINT ( 'NONE',  ( -9.594673741351313045E-17, 0.3917322834645670104, -0.8720472440944883052 ) ) ;
#32015 = CARTESIAN_POINT ( 'NONE',  ( -1.581364829396324945, -0.3162353388693405765, 0.4822834645669290543 ) ) ;
#32016 = CARTESIAN_POINT ( 'NONE',  ( 0.8530183727034128527, -0.4281496062992124485, 0.4176697321401328655 ) ) ;
#32017 = CARTESIAN_POINT ( 'NONE',  ( 0.3674540682414705883, -0.6046776061558807314, 0.2411417322834647770 ) ) ;
#32018 = LINE ( 'NONE', #64425, #66983 ) ;
#32019 = CARTESIAN_POINT ( 'NONE',  ( 0.1771653543307093182, -0.4536011799217368745, -0.2665933059059886201 ) ) ;
#32020 = CARTESIAN_POINT ( 'NONE',  ( 1.377952755905512472, 0.2952755905511811885, 0.000000000000000000 ) ) ;
#32021 = CARTESIAN_POINT ( 'NONE',  ( -0.3740157480314953431, -0.4536011799217368745, -0.2665933059059886201 ) ) ;
#32022 = CARTESIAN_POINT ( 'NONE',  ( -0.5380577427821514602, 0.05413385826771666132, 0.4176697321401328100 ) ) ;
#32023 = CARTESIAN_POINT ( 'NONE',  ( 0.8545558659330633189, 0.02791078216816508459, -0.4328096321851889194 ) ) ;
#32024 = CARTESIAN_POINT ( 'NONE',  ( 0.08530183727034192087, -0.3162353388693409650, -0.4822834645669289433 ) ) ;
#32025 = CARTESIAN_POINT ( 'NONE',  ( -0.6627296587926501115, 0.2952755905511810774, -0.1292274648535930714 ) ) ;
#32026 = CARTESIAN_POINT ( 'NONE',  ( -0.8267716535433065062, -0.5511811023622047445, 6.969142054262312111E-17 ) ) ;
#32027 = CARTESIAN_POINT ( 'NONE',  ( 0.3149606299212603933, -0.1870078740157479769, 0.4822834645669291653 ) ) ;
#32028 = B_SPLINE_CURVE_WITH_KNOTS ( 'NONE', 3,
 ( #45293, #20478, #13753, #20056, #70989, #33520, #45709 ),
 .UNSPECIFIED., .F., .F.,
 ( 4, 3, 4 ),
 ( 1.387778780781445676E-17, 0.001246230184515618360, 0.002492489877932651567 ),
 .UNSPECIFIED. ) ;
#32029 = CARTESIAN_POINT ( 'NONE',  ( -1.220472440944881054, 0.2952755905511811885, 0.000000000000000000 ) ) ;
#32030 = CARTESIAN_POINT ( 'NONE',  ( -0.3346456692913377662, 0.1660481256975883668, -0.3530559997133364547 ) ) ;
#32031 = LINE ( 'NONE', #30375, #9540 ) ;
#32033 = CARTESIAN_POINT ( 'NONE',  ( 1.528871391076116026, -0.6692913385826773087, -0.1292274648535924053 ) ) ;
#32032 = DIRECTION ( 'NONE',  ( 0.000000000000000000, 0.000000000000000000, 1.000000000000000000 ) ) ;
#32034 = CARTESIAN_POINT ( 'NONE',  ( 1.122047244094488860, -0.5400638737290845981, -0.3530559997133363437 ) ) ;
#32035 = CARTESIAN_POINT ( 'NONE',  ( -0.1049643490035301885, -0.3917322834645671215, -2.583989501312335513 ) ) ;
#32036 = CARTESIAN_POINT ( 'NONE',  ( -1.496062992125983815, -0.1870078740157479769, 0.4822834645669291653 ) ) ;
#32037 = CARTESIAN_POINT ( 'NONE',  ( -0.8005249343832013809, -0.4281496062992124485, 0.4176697321401328655 ) ) ;
#32038 = CARTESIAN_POINT ( 'NONE',  ( -0.2362204724409451284, 0.4091458600556402425, -0.1706036745406823985 ) ) ;
#32039 = CARTESIAN_POINT ( 'NONE',  ( -0.1070741851644051862, -0.3996062992125987146, 0.08530183727034119923 ) ) ;
#32040 = EDGE_LOOP ( 'NONE', ( #30693, #77229, #39525, #51699 ) ) ;
#32041 = CARTESIAN_POINT ( 'NONE',  ( -0.05249343832020911260, 0.1283753931104748280, 0.1820866141732283561 ) ) ;
#32042 = CARTESIAN_POINT ( 'NONE',  ( 0.3392501089628018329, 0.1958661417322835607, -1.698162729658792891 ) ) ;
#32043 = CARTESIAN_POINT ( 'NONE',  ( 0.6889763779527563470, 0.1660481256975883668, -0.3530559997133364547 ) ) ;
#32044 = CARTESIAN_POINT ( 'NONE',  ( 0.3458507752293908943, 0.3458507752293908943, -2.814960629921259727 ) ) ;
#32045 = CARTESIAN_POINT ( 'NONE',  ( -1.586052503253846169, 1.850393700787402729, -0.1653254495020583803 ) ) ;
#32046 = CARTESIAN_POINT ( 'NONE',  ( -0.3740157480314953431, 0.07958543189024085140, 0.2665933059059887866 ) ) ;
#32047 = DIRECTION ( 'NONE',  ( -0.000000000000000000, -1.000000000000000000, -0.000000000000000000 ) ) ;
#32048 = CARTESIAN_POINT ( 'NONE',  ( 1.279527559055118724, -0.5400638737290845981, -0.3530559997133363437 ) ) ;
#32049 = CARTESIAN_POINT ( 'NONE',  ( 0.7414698162729663755, -0.5511811023622048555, -0.09757992244046775898 ) ) ;
#32050 = CARTESIAN_POINT ( 'NONE',  ( -0.06561679790026180015, 0.05413385826771666132, 0.4176697321401328100 ) ) ;
#32051 = CARTESIAN_POINT ( 'NONE',  ( 0.2867679344610365999, 0.2867679344610365999, -0.6902693981289222958 ) ) ;
#32052 = CARTESIAN_POINT ( 'NONE',  ( -1.023622047244093558, -0.1870078740157479769, 0.4822834645669291653 ) ) ;
#32053 = CARTESIAN_POINT ( 'NONE',  ( -1.148293963254592542, -0.5511811023622048555, -0.09757992244046775898 ) ) ;
#32054 = CARTESIAN_POINT ( 'NONE',  ( -0.4790026246719154557, -0.3162353388693405765, 0.4822834645669290543 ) ) ;
#32055 = LINE ( 'NONE', #62815, #11246 ) ;
#32056 = CARTESIAN_POINT ( 'NONE',  ( -0.4426658557721557807, 1.366171107244632310, -2.105078266945731080 ) ) ;
#32057 = VERTEX_POINT ( 'NONE', #9125 ) ;
#32058 = CARTESIAN_POINT ( 'NONE',  ( 0.1958661417322834775, 0.3392501089628018884, -2.188339525755591986 ) ) ;
#32059 = CARTESIAN_POINT ( 'NONE',  ( 0.4593175853018380828, 0.05413385826771626580, -0.4176697321401330321 ) ) ;
#32060 = ORIENTED_EDGE ( 'NONE', *, *, #67691, .F. ) ;
#32061 = CARTESIAN_POINT ( 'NONE',  ( -0.5774278215223089816, 0.2306618581243847221, -0.2411417322834647770 ) ) ;
#32062 = CARTESIAN_POINT ( 'NONE',  ( 1.574803149606299746, -0.1870078740157479769, 0.4822834645669291653 ) ) ;
#32063 = CARTESIAN_POINT ( 'NONE',  ( 0.6692913385826777528, 0.2952755905511811885, 0.000000000000000000 ) ) ;
#32064 = CARTESIAN_POINT ( 'NONE',  ( 0.2362204724409456558, -0.1870078740157479769, 0.4822834645669291653 ) ) ;
#32065 = CARTESIAN_POINT ( 'NONE',  ( -9.594673741351313045E-17, 0.3917322834645670104, -1.187007874015748143 ) ) ;
#32066 = CARTESIAN_POINT ( 'NONE',  ( -0.8005249343832013809, -0.4281496062992124485, 0.4176697321401328655 ) ) ;
#32067 = CARTESIAN_POINT ( 'NONE',  ( -0.05249343832020911260, 0.2306618581243848609, 0.2411417322834645549 ) ) ;
#32068 = CARTESIAN_POINT ( 'NONE',  ( -0.05905511811023545637, 0.07958543189024085140, 0.2665933059059887866 ) ) ;
#32069 = CARTESIAN_POINT ( 'NONE',  ( -0.2397245358942217408, -0.1724005034516534474, 5.660736073501680288 ) ) ;
#32070 = EDGE_CURVE ( 'NONE', #38656, #7120, #82153, .T. ) ;
#32071 = CARTESIAN_POINT ( 'NONE',  ( -0.01312335958005186876, -0.4281496062992124485, 0.4176697321401328655 ) ) ;
#32072 = PLANE ( 'NONE',  #39930 ) ;
#32073 = CARTESIAN_POINT ( 'NONE',  ( 1.135170603674541256, 0.2952755905511811885, 0.1292274648535926551 ) ) ;
#32074 = CARTESIAN_POINT ( 'NONE',  ( 3.935112320374951178, 1.078966695441597512, -0.1230623252665035139 ) ) ;
#32075 = ORIENTED_EDGE ( 'NONE', *, *, #60399, .F. ) ;
#32076 = VERTEX_POINT ( 'NONE', #53710 ) ;
#32077 = CARTESIAN_POINT ( 'NONE',  ( 0.08530183727034192087, -0.05778040916215522460, 0.4822834645669289988 ) ) ;
#32078 = CARTESIAN_POINT ( 'NONE',  ( -0.1443569553805768291, -0.004921259842519576551, 0.3153832671262227771 ) ) ;
#32080 = DIRECTION ( 'NONE',  ( 1.000000000000000000, -0.000000000000000000, -0.000000000000000000 ) ) ;
#32079 = CARTESIAN_POINT ( 'NONE',  ( 1.456692913385827515, -0.5511811023622047445, 6.969142054262312111E-17 ) ) ;
#32081 = CARTESIAN_POINT ( 'NONE',  ( -0.3917322834645670104, -7.196005306013484475E-17, -1.226377952755905776 ) ) ;
#32082 = CARTESIAN_POINT ( 'NONE',  ( 0.2362204724409451007, -0.4091458600556402980, -0.1686351706036745557 ) ) ;
#32083 = CARTESIAN_POINT ( 'NONE',  ( 1.423884514435696413, -0.2845877964562161244, -0.3641732283464567121 ) ) ;
#32084 = CARTESIAN_POINT ( 'NONE',  ( 1.456692913385827515, 0.2952755905511811885, 0.000000000000000000 ) ) ;
#32085 = CARTESIAN_POINT ( 'NONE',  ( 0.3996062992125985480, 2.446882876249141654E-17, -2.872047244094488416 ) ) ;
#32086 = CARTESIAN_POINT ( 'NONE',  ( -0.07874015748031421014, -0.1870078740157480879, -0.4822834645669291653 ) ) ;
#32087 = CARTESIAN_POINT ( 'NONE',  ( -1.338582677165353729, -0.1870078740157479769, 0.4822834645669291653 ) ) ;
#32088 = CARTESIAN_POINT ( 'NONE',  ( -1.069553805774277722, 0.2952755905511811885, 0.1292274648535926551 ) ) ;
#32089 = CARTESIAN_POINT ( 'NONE',  ( 0.3412073490813655186, 0.2306618581243848609, 0.2411417322834645549 ) ) ;
#32090 = CARTESIAN_POINT ( 'NONE',  ( 0.3949938075777409408, -0.1058382717557499186, -0.1883202099737532886 ) ) ;
#32091 = CARTESIAN_POINT ( 'NONE',  ( -1.581364829396324945, -0.08942795157528024563, -0.3641732283464568787 ) ) ;
#32092 = CARTESIAN_POINT ( 'NONE',  ( 1.102362204724410155, -0.1870078740157479769, 0.4822834645669291653 ) ) ;
#32093 = CARTESIAN_POINT ( 'NONE',  ( 0.7677165354330716118, 0.07958543189024071263, -0.2665933059059888421 ) ) ;
#32094 = CARTESIAN_POINT ( 'NONE',  ( 0.8136482939632553313, 0.1539470093639523085, 0.1968503937007873850 ) ) ;
#32095 = CARTESIAN_POINT ( 'NONE',  ( 0.9383202099737538715, -0.08942795157528024563, -0.3641732283464568787 ) ) ;
#32096 = CARTESIAN_POINT ( 'NONE',  ( -1.482939632545930975, 0.05413385826771666132, 0.4176697321401328100 ) ) ;
#32097 = CARTESIAN_POINT ( 'NONE',  ( 0.1998031496062994128, -0.3460692066303957537, -0.7985564304461942875 ) ) ;
#32098 = CARTESIAN_POINT ( 'NONE',  ( 1.220472440944882608, 0.2952755905511811885, 0.000000000000000000 ) ) ;
#32099 = EDGE_CURVE ( 'NONE', #64782, #39936, #83143, .T. ) ;
#32100 = CARTESIAN_POINT ( 'NONE',  ( -0.2867679344610365999, 0.2867679344610364889, -0.1692913385826771144 ) ) ;
#32101 = EDGE_CURVE ( 'NONE', #65284, #9834, #66365, .T. ) ;
#32103 = CARTESIAN_POINT ( 'NONE',  ( 1.586052503253845281, 0.7480314960629931287, -0.1653254495020588799 ) ) ;
#32102 = CARTESIAN_POINT ( 'NONE',  ( 0.5380577427821529035, -0.4281496062992124485, 0.4176697321401328655 ) ) ;
#32104 = CARTESIAN_POINT ( 'NONE',  ( -1.568241469816272105, -0.08942795157527998196, 0.3641732283464567121 ) ) ;
#32105 = CARTESIAN_POINT ( 'NONE',  ( 0.06561679790026316017, -0.4281496062992124485, 0.4176697321401328655 ) ) ;
#32106 = CARTESIAN_POINT ( 'NONE',  ( 0.5183727034120741983, 0.1771653543307087075, -0.09757992244046823083 ) ) ;
#32107 = CARTESIAN_POINT ( 'NONE',  ( 0.9842519685039378130, -0.6692913385826771977, 8.415575281601705876E-17 ) ) ;
#32108 = PRODUCT_DEFINITION ( 'UNKNOWN', '', #28886, #61306 ) ;
#32109 = CARTESIAN_POINT ( 'NONE',  ( 0.7746288504648943807, 0.004960608223779807216, -0.3437734562760184631 ) ) ;
#32110 = CARTESIAN_POINT ( 'NONE',  ( -0.6955380577427815458, -0.3690944881889765550, -0.3153832671262227771 ) ) ;
#32111 = CARTESIAN_POINT ( 'NONE',  ( -0.7677165354330699465, 0.1660481256975885056, 0.3530559997133364547 ) ) ;
#32112 = CARTESIAN_POINT ( 'NONE',  ( 1.607611548556431069, -0.6692913385826773087, -0.1292274648535924053 ) ) ;
#32113 = CARTESIAN_POINT ( 'NONE',  ( -1.167979002624671470, -0.4281496062992127816, -0.4176697321401328100 ) ) ;
#32114 = CARTESIAN_POINT ( 'NONE',  ( 0.9251968503937015864, 0.1660481256975883668, -0.3530559997133364547 ) ) ;
#32115 = CARTESIAN_POINT ( 'NONE',  ( -1.358267716535432434, -0.4536011799217367080, 0.2665933059059888421 ) ) ;
#32116 = CARTESIAN_POINT ( 'NONE',  ( 1.057189182743691225, 1.247828027546490803, 0.3760955751420046456 ) ) ;
#32117 = CARTESIAN_POINT ( 'NONE',  ( 0.8398950131233602345, 0.2306618581243847221, -0.2411417322834647770 ) ) ;
#32118 = CARTESIAN_POINT ( 'NONE',  ( -0.3458507752293909498, 0.3458507752293907833, -2.458661417322834719 ) ) ;
#32119 = CARTESIAN_POINT ( 'NONE',  ( -1.502624671916009680, -0.05778040916215560624, -0.4822834645669293319 ) ) ;
#32120 = CARTESIAN_POINT ( 'NONE',  ( -1.594488188976377119, 0.07958543189024071263, -0.2665933059059888421 ) ) ;
#32121 = CARTESIAN_POINT ( 'NONE',  ( -1.167979002624671470, -0.3690944881889765550, -0.3153832671262227771 ) ) ;
#32122 = CARTESIAN_POINT ( 'NONE',  ( 1.535433070866142558, 0.1771653543307087630, 0.000000000000000000 ) ) ;
#32123 = CARTESIAN_POINT ( 'NONE',  ( -0.5511811023622038563, -0.1870078740157479769, 0.4822834645669291653 ) ) ;
#32124 = CARTESIAN_POINT ( 'NONE',  ( -0.2755905511811015396, -0.5511811023622047445, 6.969142054262312111E-17 ) ) ;
#32125 = CARTESIAN_POINT ( 'NONE',  ( -1.561679790026246017, -0.004921259842519576551, 0.3153832671262227771 ) ) ;
#32126 = CARTESIAN_POINT ( 'NONE',  ( 0.8136482939632553313, 0.1283753931104748280, 0.1820866141732283561 ) ) ;
#32127 = CARTESIAN_POINT ( 'NONE',  ( 0.4133858267716541968, 0.1660481256975885056, 0.3530559997133364547 ) ) ;
#32128 = CARTESIAN_POINT ( 'NONE',  ( 1.417322834645670104, -0.1870078740157479769, 0.4822834645669291653 ) ) ;
#32129 = CARTESIAN_POINT ( 'NONE',  ( 0.6233595800524942554, -0.05778040916215560624, -0.4822834645669293319 ) ) ;
#32130 = EDGE_CURVE ( 'NONE', #39843, #18816, #15024, .T. ) ;
#32131 = CARTESIAN_POINT ( 'NONE',  ( 0.5118110236220478892, 0.1771653543307087630, 0.000000000000000000 ) ) ;
#32132 = CARTESIAN_POINT ( 'NONE',  ( 1.515748031496063186, -0.5400638737290845981, -0.3530559997133363437 ) ) ;
#32133 = CARTESIAN_POINT ( 'NONE',  ( -1.181102362204723644, -0.1870078740157479769, 0.4822834645669291653 ) ) ;
#32134 = CARTESIAN_POINT ( 'NONE',  ( -0.5249343832020990641, -0.6046776061558809534, -0.2411417322834644161 ) ) ;
#32135 = CARTESIAN_POINT ( 'NONE',  ( 0.3996062992125986035, 2.446882876249141962E-17, -0.2755905511811024278 ) ) ;
#32136 = CARTESIAN_POINT ( 'NONE',  ( -0.1998031496062994405, 0.3460692066303957537, -2.609580052493438274 ) ) ;
#32137 = CARTESIAN_POINT ( 'NONE',  ( 0.4330708661417329575, -0.6692913385826771977, 8.415575281601705876E-17 ) ) ;
#32138 = CARTESIAN_POINT ( 'NONE',  ( 1.266404199475066328, -0.08942795157527998196, 0.3641732283464567121 ) ) ;
#32139 = CARTESIAN_POINT ( 'NONE',  ( -0.3543307086614165824, 0.2952755905511811885, 0.000000000000000000 ) ) ;
#32141 = VECTOR ( 'NONE', #14018, 39.37007874015748143 ) ;
#32140 = CARTESIAN_POINT ( 'NONE',  ( 0.3805774278215230400, 0.05413385826771626580, -0.4176697321401330321 ) ) ;
#32142 = CARTESIAN_POINT ( 'NONE',  ( 0.3460692066303959202, 0.1998031496062993295, -2.335958005249343827 ) ) ;
#32143 = CARTESIAN_POINT ( 'NONE',  ( 0.1974969037888704704, 0.3420746716998660508, -2.034120734908136718 ) ) ;
#32144 = CARTESIAN_POINT ( 'NONE',  ( 0.1049643490035304938, -0.3917322834645669549, -0.5498687664041993495 ) ) ;
#32145 = CARTESIAN_POINT ( 'NONE',  ( 3.910334576242769256, 1.663832811914786936, 0.4575345774109204622 ) ) ;
#32146 = CARTESIAN_POINT ( 'NONE',  ( 0.1958661417322834775, 0.3392501089628018884, -0.9238845144356954142 ) ) ;
#32147 = CARTESIAN_POINT ( 'NONE',  ( -0.8661417322834640276, -0.1870078740157480601, -0.3641732283464567677 ) ) ;
#32148 = CARTESIAN_POINT ( 'NONE',  ( -1.010498687664041384, -0.4281496062992127816, -0.4176697321401328100 ) ) ;
#32149 = CARTESIAN_POINT ( 'NONE',  ( 0.1058382717557499880, 0.3949938075777409408, -2.747375328083990098 ) ) ;
#32150 = ADVANCED_FACE ( 'NONE', ( #73091 ), #20200, .F. ) ;
#32151 = CARTESIAN_POINT ( 'NONE',  ( 0.9186351706036752773, 0.2306618581243847221, -0.2411417322834647770 ) ) ;
#32152 = CARTESIAN_POINT ( 'NONE',  ( 1.305774278215223960, 0.2952755905511810774, -0.1292274648535930714 ) ) ;
#32153 = CARTESIAN_POINT ( 'NONE',  ( 0.8333333333333340365, 0.2952755905511810774, -0.1292274648535930714 ) ) ;
#32154 = CARTESIAN_POINT ( 'NONE',  ( -0.6195821328811238482, -4.378520898609941727E-15, 0.4281989832122462536 ) ) ;
#32155 = CARTESIAN_POINT ( 'NONE',  ( 0.2925321140481932369, -0.2925321140481932369, -1.988188976377952777 ) ) ;
#32156 = CARTESIAN_POINT ( 'NONE',  ( 0.3917322834645670104, 0.1049643490035304660, -0.7513316517398445082 ) ) ;
#32157 = CARTESIAN_POINT ( 'NONE',  ( -0.7443564587111901609, 2.201272808314826079, 0.5309055118110236338 ) ) ;
#32158 = CARTESIAN_POINT ( 'NONE',  ( 0.5839895013123367340, -0.6692913385826773087, -0.1292274648535924053 ) ) ;
#32159 = CARTESIAN_POINT ( 'NONE',  ( 0.2230971128608929543, 0.05413385826771626580, -0.4176697321401330321 ) ) ;
#32160 = CARTESIAN_POINT ( 'NONE',  ( 0.8136482939632553313, 0.1283753931104748280, 0.1820866141732283561 ) ) ;
#32161 = CARTESIAN_POINT ( 'NONE',  ( 1.515748031496063408, 0.1660481256975885056, 0.3530559997133364547 ) ) ;
#32162 = CARTESIAN_POINT ( 'NONE',  ( 0.3392501089628018329, 0.1958661417322835607, -0.05839895013123368173 ) ) ;
#32163 = CARTESIAN_POINT ( 'NONE',  ( 0.5774278215223103139, -0.6046776061558809534, -0.2411417322834644161 ) ) ;
#32164 = CARTESIAN_POINT ( 'NONE',  ( 1.253280839895013710, -0.05778040916215560624, -0.4822834645669293319 ) ) ;
#32165 = CARTESIAN_POINT ( 'NONE',  ( 0.1968503937007881344, -0.6692913385826771977, 8.415575281601705876E-17 ) ) ;
#32166 = CARTESIAN_POINT ( 'NONE',  ( 1.135170603674541256, -0.5511811023622048555, -0.09757992244046775898 ) ) ;
#32167 = CARTESIAN_POINT ( 'NONE',  ( -1.030183727034119867, -0.05778040916215560624, -0.4822834645669293319 ) ) ;
#32168 = CARTESIAN_POINT ( 'NONE',  ( -0.8464566929133852113, -0.5400638737290845981, -0.3530559997133363437 ) ) ;
#32169 = CARTESIAN_POINT ( 'NONE',  ( 1.108923884514436242, -0.05778040916215522460, 0.4822834645669289988 ) ) ;
#32170 = CARTESIAN_POINT ( 'NONE',  ( -0.1958661417322834220, -0.3392501089628018884, -0.4652230971128609727 ) ) ;
#32171 = CARTESIAN_POINT ( 'NONE',  ( -0.1958661417322834220, -0.3392501089628018884, -1.317585301837270295 ) ) ;
#32172 = CARTESIAN_POINT ( 'NONE',  ( 0.3917322834645670104, -0.1049643490035303411, -2.623359580052493367 ) ) ;
#32173 = EDGE_CURVE ( 'NONE', #6265, #7002, #68844, .T. ) ;
#32174 = EDGE_LOOP ( 'NONE', ( #67055, #63431, #56708, #2134, #26995, #74416, #78364, #48209, #47489, #52224, #75653, #12028, #28247, #10379, #41523, #39437, #33130, #3521, #22761, #9388, #56891, #18279, #33006, #82389, #44873, #5849, #26877, #36698, #11891, #58275, #61800, #36330, #81576, #66879, #56676, #20412, #20661, #8896, #48953, #79493, #64679, #8711, #13686, #71623, #38901, #34265, #77213, #76699, #45805, #27712, #49967, #47886, #34685, #52050, #74013, #2247, #30888, #32774, #41928, #82407, #28665, #58762, #61169, #12019, #41989, #52969, #33716, #72725, #10415 ) ) ;
#32175 = CARTESIAN_POINT ( 'NONE',  ( -0.3460692066303958092, -0.1998031496062994683, -0.05249343832020999384 ) ) ;
#32176 = VERTEX_POINT ( 'NONE', #50702 ) ;
#32177 = CARTESIAN_POINT ( 'NONE',  ( 1.377952755905512472, 0.2952755905511811885, 0.000000000000000000 ) ) ;
#32178 = CARTESIAN_POINT ( 'NONE',  ( 1.122047244094488860, 0.07958543189024085140, 0.2665933059059887866 ) ) ;
#32179 = CARTESIAN_POINT ( 'NONE',  ( -0.2925321140481932924, 0.2925321140481931814, -1.594488188976378229 ) ) ;
#32180 = CARTESIAN_POINT ( 'NONE',  ( 1.233595800524935227, 0.1283753931104746893, -0.1820866141732285504 ) ) ;
#32181 = CARTESIAN_POINT ( 'NONE',  ( 0.4556365139439955136, 1.537493841899424618, -0.5309055118110237448 ) ) ;
#32182 = CARTESIAN_POINT ( 'NONE',  ( -0.1377952755905504645, 0.1660481256975885056, 0.3530559997133364547 ) ) ;
#32183 = LINE ( 'NONE', #65443, #78199 ) ;
#32184 = CARTESIAN_POINT ( 'NONE',  ( -9.594673741351313045E-17, 0.3917322834645670104, -1.029527559055118280 ) ) ;
#32185 = CARTESIAN_POINT ( 'NONE',  ( -1.213910761154854745, -0.5511811023622046335, 0.09757992244046803654 ) ) ;
#32186 = CARTESIAN_POINT ( 'NONE',  ( -1.423884514435694859, -0.2845877964562159024, 0.3641732283464567677 ) ) ;
#32187 = CARTESIAN_POINT ( 'NONE',  ( -1.122047244094487306, 0.1660481256975883668, -0.3530559997133364547 ) ) ;
#32188 = CARTESIAN_POINT ( 'NONE',  ( 0.03937007874015806264, 0.2952755905511811885, 0.000000000000000000 ) ) ;
#32189 = CARTESIAN_POINT ( 'NONE',  ( 1.423884514435696191, -0.05778040916215522460, 0.4822834645669289988 ) ) ;
#32190 = ORIENTED_EDGE ( 'NONE', *, *, #55183, .F. ) ;
#32191 = CARTESIAN_POINT ( 'NONE',  ( -1.141732283464566011, 0.2066929133858268208, 0.000000000000000000 ) ) ;
#32192 = CARTESIAN_POINT ( 'NONE',  ( -0.2362204724409451284, 0.4091458600556402425, -1.902887139107611647 ) ) ;
#32193 = LINE ( 'NONE', #26290, #8954 ) ;
#32194 = PLANE ( 'NONE',  #53251 ) ;
#32195 = CARTESIAN_POINT ( 'NONE',  ( -0.9973753280839886548, 0.1283753931104748280, 0.1820866141732283561 ) ) ;
#32196 =( BOUNDED_CURVE ( )  B_SPLINE_CURVE ( 3, ( #46281, #7588, #861, #58497 ),
 .UNSPECIFIED., .F., .F. ) 
 B_SPLINE_CURVE_WITH_KNOTS ( ( 4, 4 ),
 ( 1.859270518042426046, 2.743397753083149482 ),
 .UNSPECIFIED. ) 
 CURVE ( )  GEOMETRIC_REPRESENTATION_ITEM ( )  RATIONAL_B_SPLINE_CURVE ( ( 1.000000000000000000, 0.9359138408343250504, 0.9359138408343250504, 1.000000000000000000 ) ) 
 REPRESENTATION_ITEM ( '' )  );
#32197 = CARTESIAN_POINT ( 'NONE',  ( -1.272965879265091305, 0.05413385826771626580, -0.4176697321401330321 ) ) ;
#32198 = CARTESIAN_POINT ( 'NONE',  ( 1.194225721784777594, 0.05413385826771666132, 0.4176697321401328100 ) ) ;
#32199 = VERTEX_POINT ( 'NONE', #50292 ) ;
#32201 = DIRECTION ( 'NONE',  ( -0.000000000000000000, 1.000000000000000000, -0.000000000000000000 ) ) ;
#32200 = CARTESIAN_POINT ( 'NONE',  ( 0.000000000000000000, 0.000000000000000000, 1.850393700787401619 ) ) ;
#32202 = CARTESIAN_POINT ( 'NONE',  ( 1.286089238845145033, -0.6046776061558809534, -0.2411417322834644161 ) ) ;
#32203 = CARTESIAN_POINT ( 'NONE',  ( -1.167979002624671470, -0.4281496062992127816, -0.4176697321401328100 ) ) ;
#32204 = CARTESIAN_POINT ( 'NONE',  ( -0.2867679344610366554, 0.2867679344610365444, -0.7296394768690795951 ) ) ;
#32205 = CARTESIAN_POINT ( 'NONE',  ( -0.4461942257217840213, 0.1283753931104748280, 0.1820866141732283561 ) ) ;
#32206 = CARTESIAN_POINT ( 'NONE',  ( 0.1049643490035304799, -0.3917322834645669549, -0.7998687664041994605 ) ) ;
#32207 = CARTESIAN_POINT ( 'NONE',  ( -0.6758530183727028406, 0.1771653543307087630, 0.09757992244046791164 ) ) ;
#32208 = CARTESIAN_POINT ( 'NONE',  ( -0.05905511811023545637, -0.4536011799217368745, -0.2665933059059886201 ) ) ;
#32209 = CARTESIAN_POINT ( 'NONE',  ( 0.2034120734908142214, 0.2952755905511810774, -0.1292274648535930714 ) ) ;
#32210 = CARTESIAN_POINT ( 'NONE',  ( -1.345144356955379816, -0.2845877964562159024, 0.3641732283464567677 ) ) ;
#32211 = CARTESIAN_POINT ( 'NONE',  ( 0.3917322834645670104, -0.1049643490035303411, -2.780839895013122565 ) ) ;
#32212 = CARTESIAN_POINT ( 'NONE',  ( 1.194225721784777594, -0.4281496062992127816, -0.4176697321401328100 ) ) ;
#32213 = CARTESIAN_POINT ( 'NONE',  ( -1.541994750656167090, -0.6692913385826773087, -0.1292274648535924053 ) ) ;
#32214 = CARTESIAN_POINT ( 'NONE',  ( 5.785732909357575061E-17, -0.4724409448818898682, -1.257874015748031260 ) ) ;
#32215 = CARTESIAN_POINT ( 'NONE',  ( -0.2296587926509179312, -0.3162353388693409650, -0.4822834645669289433 ) ) ;
#32216 = EDGE_CURVE ( 'NONE', #12593, #9282, #31117, .T. ) ;
#32217 = CARTESIAN_POINT ( 'NONE',  ( -0.8464566929133852113, 0.1660481256975885056, 0.3530559997133364547 ) ) ;
#32218 = CARTESIAN_POINT ( 'NONE',  ( 0.7545931758530189937, 0.1771653543307087075, -0.09757992244046823083 ) ) ;
#32219 = CARTESIAN_POINT ( 'NONE',  ( -0.3215223097112853146, -0.2845877964562159024, 0.3641732283464567677 ) ) ;
#32220 = CARTESIAN_POINT ( 'NONE',  ( -0.6496062992125976043, -0.5400638737290844871, 0.3530559997133364547 ) ) ;
#32221 = CARTESIAN_POINT ( 'NONE',  ( -1.614173228346455824, 0.2952755905511811885, 0.000000000000000000 ) ) ;
#32222 = CARTESIAN_POINT ( 'NONE',  ( -3.937007874015748143, 2.559055118110236560, 0.5314960629921260393 ) ) ;
#32223 = CARTESIAN_POINT ( 'NONE',  ( 1.213910761154856299, 0.1771653543307087630, 0.09757992244046791164 ) ) ;
#32224 = EDGE_CURVE ( 'NONE', #72153, #2295, #71069, .T. ) ;
#32225 = CARTESIAN_POINT ( 'NONE',  ( -0.1312335958005241554, -0.6046776061558809534, -0.2411417322834644161 ) ) ;
#32226 = CARTESIAN_POINT ( 'NONE',  ( -1.509186351706035767, 0.05413385826771626580, -0.4176697321401330321 ) ) ;
#32227 = ORIENTED_EDGE ( 'NONE', *, *, #53218, .F. ) ;
#32228 = CARTESIAN_POINT ( 'NONE',  ( 0.2925321140481932369, 0.2925321140481932369, -2.419291338582676865 ) ) ;
#32229 = CARTESIAN_POINT ( 'NONE',  ( -0.8333333333333323711, 0.1771653543307087630, 0.09757992244046791164 ) ) ;
#32230 = CARTESIAN_POINT ( 'NONE',  ( 0.9317585301837276734, -0.4281496062992124485, 0.4176697321401328655 ) ) ;
#32231 = CARTESIAN_POINT ( 'NONE',  ( -1.213910761154854745, 0.1771653543307087075, -0.09757992244046823083 ) ) ;
#32232 = CARTESIAN_POINT ( 'NONE',  ( -0.3996062992125985480, -7.340648628747423112E-17, -1.218503937007874072 ) ) ;
#32233 = CARTESIAN_POINT ( 'NONE',  ( -0.9383202099737524282, -0.05778040916215522460, 0.4822834645669289988 ) ) ;
#32234 = CARTESIAN_POINT ( 'NONE',  ( 0.7545931758530189937, 0.2952755905511810774, -0.1292274648535930714 ) ) ;
#32235 = CARTESIAN_POINT ( 'NONE',  ( 0.5446194225721792126, -0.3162353388693405765, 0.4822834645669290543 ) ) ;
#32236 = CARTESIAN_POINT ( 'NONE',  ( 1.581364829396326277, -0.05778040916215522460, 0.4822834645669289988 ) ) ;
#32237 = CARTESIAN_POINT ( 'NONE',  ( -1.358267716535432434, 0.07958543189024071263, -0.2665933059059888421 ) ) ;
#32238 = CARTESIAN_POINT ( 'NONE',  ( 0.2925321140481931814, -0.2925321140481931259, -0.6476377952755905110 ) ) ;
#32239 = CARTESIAN_POINT ( 'NONE',  ( -0.1998031496062994683, 0.3460692066303958092, -0.8005249343832020470 ) ) ;
#32240 = CARTESIAN_POINT ( 'NONE',  ( 0.3949938075777409408, 0.1058382717557500574, -0.1246719160104987345 ) ) ;
#32241 = CARTESIAN_POINT ( 'NONE',  ( 0.000000000000000000, 0.000000000000000000, -3.444881889763779625 ) ) ;
#32242 = CARTESIAN_POINT ( 'NONE',  ( 1.049868766404200349, 0.1283753931104748280, 0.1820866141732283561 ) ) ;
#32243 = CARTESIAN_POINT ( 'NONE',  ( 0.4855643044619428750, -0.004921259842519576551, 0.3153832671262227771 ) ) ;
#32244 = CARTESIAN_POINT ( 'NONE',  ( 0.3018372703412079971, -0.4281496062992124485, 0.4176697321401328655 ) ) ;
#32245 = CARTESIAN_POINT ( 'NONE',  ( 1.397637795275591177, -0.5400638737290844871, 0.3530559997133364547 ) ) ;
#32246 = CARTESIAN_POINT ( 'NONE',  ( -0.2891555358219911054, 0.2891555358219909388, -1.198818897637795589 ) ) ;
#32247 = CARTESIAN_POINT ( 'NONE',  ( 0.2952755905511819101, 0.07958543189024071263, -0.2665933059059888421 ) ) ;
#32248 = CARTESIAN_POINT ( 'NONE',  ( -0.8858267716535425107, -0.5400638737290844871, 0.3530559997133364547 ) ) ;
#32249 = CARTESIAN_POINT ( 'NONE',  ( -1.430446194225720724, 0.05413385826771626580, -0.4176697321401330321 ) ) ;
#32250 = CARTESIAN_POINT ( 'NONE',  ( 0.9251968503937015864, 0.1660481256975883668, -0.3530559997133364547 ) ) ;
#32251 = CARTESIAN_POINT ( 'NONE',  ( 0.4724409448818896462, 0.1265901696524990294, -1.541994750656167978 ) ) ;
#32252 = CARTESIAN_POINT ( 'NONE',  ( -1.220472440944881276, 0.4405861044731111953, 0.5309055118110234117 ) ) ;
#32253 = VERTEX_POINT ( 'NONE', #76400 ) ;
#32254 = ORIENTED_EDGE ( 'NONE', *, *, #73728, .F. ) ;
#32255 = CARTESIAN_POINT ( 'NONE',  ( -1.259842519685038686, -0.1870078740157479769, 0.4822834645669291653 ) ) ;
#32256 = CARTESIAN_POINT ( 'NONE',  ( -0.6758530183727028406, 0.2952755905511811885, 0.1292274648535926551 ) ) ;
#32258 = CARTESIAN_POINT ( 'NONE',  ( -0.6824146981627288167, 0.2306618581243848609, 0.2411417322834645549 ) ) ;
#32257 = CARTESIAN_POINT ( 'NONE',  ( -0.9317585301837263412, -0.3690944881889765550, -0.3153832671262227771 ) ) ;
#32259 = CARTESIAN_POINT ( 'NONE',  ( 0.1049643490035304522, -0.3917322834645668994, -2.055098794454381927 ) ) ;
#32260 = CARTESIAN_POINT ( 'NONE',  ( 0.1070741851644054776, -0.3996062992125984925, -2.839238845144356649 ) ) ;
#32261 = CARTESIAN_POINT ( 'NONE',  ( -1.581364829396324945, -0.08942795157528024563, -0.3641732283464568787 ) ) ;
#32262 = CARTESIAN_POINT ( 'NONE',  ( -1.345144356955379816, -0.05778040916215560624, -0.4822834645669293319 ) ) ;
#32263 = CARTESIAN_POINT ( 'NONE',  ( 0.5249343832021003964, 0.2306618581243847221, -0.2411417322834647770 ) ) ;
#32264 = CARTESIAN_POINT ( 'NONE',  ( -1.010498687664041384, 0.05413385826771666132, 0.4176697321401328100 ) ) ;
#32265 = B_SPLINE_CURVE_WITH_KNOTS ( 'NONE', 3,
 ( #37568, #76703, #5582, #103, #25757, #19454, #70811 ),
 .UNSPECIFIED., .F., .F.,
 ( 4, 3, 4 ),
 ( 7.287419555744632558E-17, 0.001246232571205270478, 0.002492492258783315755 ),
 .UNSPECIFIED. ) ;
#32266 = CARTESIAN_POINT ( 'NONE',  ( 0.1049643490035304938, -0.3917322834645669549, -1.652230971128608505 ) ) ;
#32267 = CARTESIAN_POINT ( 'NONE',  ( -0.6561679790026240244, 0.1283753931104746893, -0.1820866141732285504 ) ) ;
#32268 = ORIENTED_EDGE ( 'NONE', *, *, #20062, .T. ) ;
#32269 = CARTESIAN_POINT ( 'NONE',  ( 0.1058382717557500713, -0.3949938075777409408, -1.975065616797900159 ) ) ;
#32270 = ORIENTED_EDGE ( 'NONE', *, *, #14233, .T. ) ;
#32271 = CARTESIAN_POINT ( 'NONE',  ( -1.706036745406823485, 0.1283753931104748280, 0.1820866141732283561 ) ) ;
#32272 = CARTESIAN_POINT ( 'NONE',  ( -1.253280839895012377, -0.3162353388693409650, -0.4822834645669289433 ) ) ;
#32273 = CARTESIAN_POINT ( 'NONE',  ( -0.8136482939632537770, 0.2306618581243847221, -0.2411417322834647770 ) ) ;
#32274 = CARTESIAN_POINT ( 'NONE',  ( 0.2925321140481932369, -0.2925321140481932369, -0.09842519685039373412 ) ) ;
#32275 = CARTESIAN_POINT ( 'NONE',  ( -1.253280839895012377, -0.05778040916215522460, 0.4822834645669289988 ) ) ;
#32276 = CARTESIAN_POINT ( 'NONE',  ( -1.377952755905511140, 0.2952755905511811885, 0.000000000000000000 ) ) ;
#32277 =( LENGTH_UNIT ( ) NAMED_UNIT ( * ) SI_UNIT ( $, .METRE. ) );
#32278 = CARTESIAN_POINT ( 'NONE',  ( 0.6627296587926517768, -0.5511811023622048555, -0.09757992244046775898 ) ) ;
#32279 = CARTESIAN_POINT ( 'NONE',  ( 0.4744094488188901337, 1.554943921348594493, 2.170146923806597350 ) ) ;
#32280 = CARTESIAN_POINT ( 'NONE',  ( 0.3392501089628018884, -0.1958661417322834220, -0.5045931758530184386 ) ) ;
#32281 = CARTESIAN_POINT ( 'NONE',  ( -0.3412073490813641308, -0.5023911411419708095, 0.1820866141732285504 ) ) ;
#32282 = CARTESIAN_POINT ( 'NONE',  ( -0.7217847769028863381, -0.4281496062992124485, 0.4176697321401328655 ) ) ;
#32283 = CARTESIAN_POINT ( 'NONE',  ( 1.286089238845145033, 0.2306618581243848609, 0.2411417322834645549 ) ) ;
#32284 = CARTESIAN_POINT ( 'NONE',  ( -0.4461942257217840213, -0.6046776061558809534, -0.2411417322834644161 ) ) ;
#32285 = VERTEX_POINT ( 'NONE', #36851 ) ;
#32286 = ORIENTED_EDGE ( 'NONE', *, *, #79536, .T. ) ;
#32287 = CARTESIAN_POINT ( 'NONE',  ( -0.3460692066303957537, -0.1998031496062994405, -1.861548556430446144 ) ) ;
#32288 = CARTESIAN_POINT ( 'NONE',  ( -1.043307086614172041, -0.5400638737290844871, 0.3530559997133364547 ) ) ;
#32289 = CARTESIAN_POINT ( 'NONE',  ( 1.128608923884514947, 0.2306618581243848609, 0.2411417322834645549 ) ) ;
#32290 = CARTESIAN_POINT ( 'NONE',  ( -1.148293963254592542, -0.5511811023622048555, -0.09757992244046775898 ) ) ;
#32291 = CARTESIAN_POINT ( 'NONE',  ( -1.240157480314959759, 0.1660481256975885056, 0.3530559997133364547 ) ) ;
#32292 = CARTESIAN_POINT ( 'NONE',  ( -0.2362204724409451284, 0.4091458600556402425, -0.9580052493438320216 ) ) ;
#32293 = DIRECTION ( 'NONE',  ( 0.000000000000000000, 0.000000000000000000, -1.000000000000000000 ) ) ;
#32294 = CARTESIAN_POINT ( 'NONE',  ( -0.3917322834645671215, 0.1049643490035301469, -0.1824146981627296216 ) ) ;
#32295 = CARTESIAN_POINT ( 'NONE',  ( 4.797336870675656522E-17, -0.3917322834645670104, -2.053149606299212948 ) ) ;
#32296 = CARTESIAN_POINT ( 'NONE',  ( 0.2755905511811031494, 0.2952755905511811885, 0.000000000000000000 ) ) ;
#32297 = CARTESIAN_POINT ( 'NONE',  ( -0.9448818897637790704, -0.1870078740157480601, -0.3641732283464567677 ) ) ;
#32298 = CARTESIAN_POINT ( 'NONE',  ( -0.5708661417322828946, 0.1660481256975883668, -0.3530559997133364547 ) ) ;
#32299 = CARTESIAN_POINT ( 'NONE',  ( -0.4091458600556402980, -0.2362204724409451284, -2.806430446194225770 ) ) ;
#32300 = CARTESIAN_POINT ( 'NONE',  ( -1.108923884514435132, -0.3162353388693405765, 0.4822834645669290543 ) ) ;
#32301 = CARTESIAN_POINT ( 'NONE',  ( -0.9448818897637790704, -0.1870078740157479769, 0.4822834645669291653 ) ) ;
#32302 = CARTESIAN_POINT ( 'NONE',  ( 0.1181102362204730916, -0.6692913385826771977, 8.415575281601705876E-17 ) ) ;
#32303 = CARTESIAN_POINT ( 'NONE',  ( 0.3420746716998660508, -0.1974969037888704149, -2.701443569553805713 ) ) ;
#32304 = CARTESIAN_POINT ( 'NONE',  ( 1.076115485564305141, -0.5023911411419708095, 0.1820866141732285504 ) ) ;
#32305 = CARTESIAN_POINT ( 'NONE',  ( -0.5774278215223089816, 0.1283753931104746893, -0.1820866141732285504 ) ) ;
#32306 = CARTESIAN_POINT ( 'NONE',  ( -0.07064761070677771926, 1.068257286200871681, -1.454808247151501588 ) ) ;
#32307 = CARTESIAN_POINT ( 'NONE',  ( 0.6692913385826778638, -0.5511811023622047445, 6.969142054262312111E-17 ) ) ;
#32308 = CARTESIAN_POINT ( 'NONE',  ( 1.541994750656168645, -0.5511811023622046335, 0.09757992244046803654 ) ) ;
#32309 = CARTESIAN_POINT ( 'NONE',  ( 1.207349081364829990, -0.6046776061558809534, -0.2411417322834644161 ) ) ;
#32310 = CARTESIAN_POINT ( 'NONE',  ( 0.1115485564304470323, 0.1771653543307087630, 0.09757992244046791164 ) ) ;
#32311 = CARTESIAN_POINT ( 'NONE',  ( -0.3917322834645670104, -7.196005306013484475E-17, -1.448818897637795367 ) ) ;
#32312 = CARTESIAN_POINT ( 'NONE',  ( -1.003937007874014853, 0.1660481256975885056, 0.3530559997133364547 ) ) ;
#32313 = CARTESIAN_POINT ( 'NONE',  ( 1.207349081364829990, -0.6046776061558809534, -0.2411417322834644161 ) ) ;
#32314 = CARTESIAN_POINT ( 'NONE',  ( -0.1265901696524986964, -0.4724409448818899238, 0.1660104986876640432 ) ) ;
#32315 = CARTESIAN_POINT ( 'NONE',  ( -0.3083989501312330295, -0.2845877964562161244, -0.3641732283464567121 ) ) ;
#32316 = DIRECTION ( 'NONE',  ( 0.000000000000000000, 0.000000000000000000, 1.000000000000000000 ) ) ;
#32317 = ADVANCED_FACE ( 'NONE', ( #69260 ), #4453, .F. ) ;
#32318 = CARTESIAN_POINT ( 'NONE',  ( 0.1181102362204730916, 0.2952755905511811885, 0.000000000000000000 ) ) ;
#32319 = CARTESIAN_POINT ( 'NONE',  ( -1.028550503362776425, 1.694972584785692904, -0.4486219446274117839 ) ) ;
#32320 = CARTESIAN_POINT ( 'NONE',  ( 1.148293963254593653, 0.1771653543307087075, -0.09757992244046823083 ) ) ;
#32321 = CARTESIAN_POINT ( 'NONE',  ( 0.3543307086614179147, 0.1771653543307087630, 0.000000000000000000 ) ) ;
#32322 = CARTESIAN_POINT ( 'NONE',  ( 0.09186351706036827158, 0.05413385826771666132, 0.4176697321401328100 ) ) ;
#32323 = CARTESIAN_POINT ( 'NONE',  ( -1.332020997375327642, -0.3162353388693409650, -0.4822834645669289433 ) ) ;
#32324 = CARTESIAN_POINT ( 'NONE',  ( -0.6561679790026240244, 0.1283753931104746893, -0.1820866141732285504 ) ) ;
#32325 = DIRECTION ( 'NONE',  ( -0.000000000000000000, -1.000000000000000000, -0.000000000000000000 ) ) ;
#32326 = VECTOR ( 'NONE', #76085, 39.37007874015748143 ) ;
#32327 = CARTESIAN_POINT ( 'NONE',  ( -0.8333333333333323711, 0.2952755905511811885, 0.1292274648535926551 ) ) ;
#32328 = CARTESIAN_POINT ( 'NONE',  ( -0.2925321140481932369, 0.2925321140481931259, -1.041338582677165281 ) ) ;
#32329 = CARTESIAN_POINT ( 'NONE',  ( -0.2867679344610364334, -0.2867679344610367109, -2.505905511811023612 ) ) ;
#32330 = CARTESIAN_POINT ( 'NONE',  ( 0.3937007874015754361, -0.1870078740157480601, -0.3641732283464567677 ) ) ;
#32331 = CARTESIAN_POINT ( 'NONE',  ( -0.9842519685039360366, 0.2952755905511811885, 0.000000000000000000 ) ) ;
#32332 = CARTESIAN_POINT ( 'NONE',  ( -0.9711286089238838626, 0.2306618581243847221, -0.2411417322834647770 ) ) ;
#32333 = CARTESIAN_POINT ( 'NONE',  ( -1.377952755905511140, -0.5511811023622047445, 6.969142054262312111E-17 ) ) ;
#32334 = CARTESIAN_POINT ( 'NONE',  ( 1.561679790026247350, 0.05413385826771626580, -0.4176697321401330321 ) ) ;
#32335 = CARTESIAN_POINT ( 'NONE',  ( -0.6299212598425188991, -0.1870078740157480879, -0.4822834645669291653 ) ) ;
#32336 = CARTESIAN_POINT ( 'NONE',  ( -0.9120734908136475250, -0.5511811023622048555, -0.09757992244046775898 ) ) ;
#32337 = CARTESIAN_POINT ( 'NONE',  ( -1.568241469816272105, -0.08942795157527998196, 0.3641732283464567121 ) ) ;
#32338 = CARTESIAN_POINT ( 'NONE',  ( 1.463254593175853824, 0.2952755905511810774, -0.1292274648535930714 ) ) ;
#32339 = CARTESIAN_POINT ( 'NONE',  ( -0.2925321140481932924, 0.2925321140481931814, 0.1377952755905511584 ) ) ;
#32340 = CARTESIAN_POINT ( 'NONE',  ( 0.2867679344610366554, 0.2867679344610366554, -2.181777845965566343 ) ) ;
#32341 = ORIENTED_EDGE ( 'NONE', *, *, #68594, .F. ) ;
#32342 = CONICAL_SURFACE ( 'NONE', #1488, 1.220472440944881942, 0.7853981633974621568 ) ;
#32343 = DIRECTION ( 'NONE',  ( -0.000000000000000000, 1.000000000000000000, 0.000000000000000000 ) ) ;
#32344 = CARTESIAN_POINT ( 'NONE',  ( -1.227034120734907585, 0.2952755905511811885, 0.1292274648535926551 ) ) ;
#32345 = CARTESIAN_POINT ( 'NONE',  ( -0.9383202099737524282, -0.05778040916215522460, 0.4822834645669289988 ) ) ;
#32346 = CARTESIAN_POINT ( 'NONE',  ( -1.587926509186350810, 0.05413385826771626580, -0.4176697321401330321 ) ) ;
#32347 = CARTESIAN_POINT ( 'NONE',  ( -0.3917322834645670104, -7.196005306013484475E-17, -2.171259842519685179 ) ) ;
#32348 = CARTESIAN_POINT ( 'NONE',  ( 1.614173228346457378, -0.5511811023622047445, 6.969142054262312111E-17 ) ) ;
#32349 = CARTESIAN_POINT ( 'NONE',  ( 0.6561679790026253567, -0.6046776061558809534, -0.2411417322834644161 ) ) ;
#32350 = CARTESIAN_POINT ( 'NONE',  ( -0.1115485564304453947, -0.6692913385826771977, 0.1292274648535927661 ) ) ;
#32351 = CARTESIAN_POINT ( 'NONE',  ( -0.03757601356356682354, 0.4709442531824372113, -2.755905511811023612 ) ) ;
#32352 = CARTESIAN_POINT ( 'NONE',  ( 0.2925321140481931814, -0.2925321140481931259, -2.694881889763779625 ) ) ;
#32353 = CARTESIAN_POINT ( 'NONE',  ( 0.8595800524934390507, -0.08942795157528024563, -0.3641732283464568787 ) ) ;
#32354 = CARTESIAN_POINT ( 'NONE',  ( 0.3460692066303959202, 0.1998031496062993295, -1.391076115485564424 ) ) ;
#32355 = VERTEX_POINT ( 'NONE', #25029 ) ;
#32356 = CARTESIAN_POINT ( 'NONE',  ( -0.3392501089628019995, 0.1958661417322831999, -0.02298519504693102150 ) ) ;
#32357 = VERTEX_POINT ( 'NONE', #62942 ) ;
#32358 = CARTESIAN_POINT ( 'NONE',  ( -0.006561679790025524116, -0.3162353388693405765, 0.4822834645669290543 ) ) ;
#32359 = CARTESIAN_POINT ( 'NONE',  ( -1.509186351706035767, -0.4281496062992124485, 0.4176697321401328655 ) ) ;
#32360 = CARTESIAN_POINT ( 'NONE',  ( 0.8398950131233602345, -0.6046776061558807314, 0.2411417322834647770 ) ) ;
#32361 = CARTESIAN_POINT ( 'NONE',  ( -1.646981627296586703, -0.08942795157527998196, 0.3641732283464567121 ) ) ;
#32362 = CARTESIAN_POINT ( 'NONE',  ( 1.384514435695538337, -0.6692913385826771977, 0.1292274648535927661 ) ) ;
#32363 = CARTESIAN_POINT ( 'NONE',  ( -0.2887139107611542133, -0.6046776061558809534, -0.2411417322834644161 ) ) ;
#32364 = CARTESIAN_POINT ( 'NONE',  ( 0.4199475065616803948, -0.6046776061558809534, -0.2411417322834644161 ) ) ;
#32365 = CARTESIAN_POINT ( 'NONE',  ( 1.548556430446194954, -0.6046776061558807314, 0.2411417322834647770 ) ) ;
#32366 = CARTESIAN_POINT ( 'NONE',  ( 1.515748031496063186, -0.5400638737290845981, -0.3530559997133363437 ) ) ;
#32367 = CARTESIAN_POINT ( 'NONE',  ( -0.2887139107611542133, 0.2306618581243848609, 0.2411417322834645549 ) ) ;
#32368 = CARTESIAN_POINT ( 'NONE',  ( -0.3392501089628019995, 0.1958661417322832277, -0.1758530183727033402 ) ) ;
#32369 = CARTESIAN_POINT ( 'NONE',  ( 0.3018372703412079971, -0.004921259842519870586, -0.3153832671262229437 ) ) ;
#32370 = ORIENTED_EDGE ( 'NONE', *, *, #23484, .F. ) ;
#32371 = CARTESIAN_POINT ( 'NONE',  ( -0.1058382717557503211, 0.3949938075777409408, -0.4790026246719162328 ) ) ;
#32372 = VERTEX_POINT ( 'NONE', #6093 ) ;
#32373 = CARTESIAN_POINT ( 'NONE',  ( -0.5380577427821514602, -0.3690944881889765550, -0.3153832671262227771 ) ) ;
#32374 = CARTESIAN_POINT ( 'NONE',  ( 2.557140022784311295, 1.502969453419624735, -0.4732359647714761697 ) ) ;
#32375 = CARTESIAN_POINT ( 'NONE',  ( 0.3477690288713918276, 0.2952755905511811885, 0.1292274648535926551 ) ) ;
#32376 = CARTESIAN_POINT ( 'NONE',  ( -0.1640419947506555343, -0.3162353388693405765, 0.4822834645669290543 ) ) ;
#32377 = CARTESIAN_POINT ( 'NONE',  ( -1.017060367454067249, -0.3162353388693409650, -0.4822834645669289433 ) ) ;
#32378 = CARTESIAN_POINT ( 'NONE',  ( 0.1049643490035304799, -0.3917322834645670104, -1.656843462763466723 ) ) ;
#32379 = CARTESIAN_POINT ( 'NONE',  ( -1.246719160104985846, -0.4281496062992127816, -0.4176697321401328100 ) ) ;
#32380 = CARTESIAN_POINT ( 'NONE',  ( 0.5314960629921346991, 2.755905511811024056, -2.503252890251014495 ) ) ;
#32381 = CARTESIAN_POINT ( 'NONE',  ( 0.7677165354330716118, -0.4536011799217367080, 0.2665933059059888421 ) ) ;
#32382 = CARTESIAN_POINT ( 'NONE',  ( 0.3608923884514443348, -0.6692913385826771977, 0.1292274648535927661 ) ) ;
#32383 = CARTESIAN_POINT ( 'NONE',  ( 0.6430446194225729606, -0.4281496062992127816, -0.4176697321401328100 ) ) ;
#32384 = VECTOR ( 'NONE', #60864, 39.37007874015748143 ) ;
#32385 = CARTESIAN_POINT ( 'NONE',  ( 0.1070741851644054915, -0.3996062992125986035, -1.345144356955380704 ) ) ;
#32386 = CARTESIAN_POINT ( 'NONE',  ( 0.3273801728231982566, 0.000000000000000000, 0.3464511005275205946 ) ) ;
#32387 = CARTESIAN_POINT ( 'NONE',  ( -0.1070741851644051862, -0.3996062992125986590, -0.6213910761154856077 ) ) ;
#32388 = CARTESIAN_POINT ( 'NONE',  ( -0.1070741851644056997, 0.3996062992125984925, 0.07414698162729654873 ) ) ;
#32389 = CARTESIAN_POINT ( 'NONE',  ( -0.1181102362204717315, 0.2952755905511811885, 0.000000000000000000 ) ) ;
#32390 = CARTESIAN_POINT ( 'NONE',  ( 0.2925321140481932369, -0.2925321140481932369, -2.775590551181101429 ) ) ;
#32391 = CARTESIAN_POINT ( 'NONE',  ( -0.1049643490035307020, 0.3917322834645669549, -1.666010498687664043 ) ) ;
#32392 = CARTESIAN_POINT ( 'NONE',  ( -1.207349081364828436, -0.5023911411419708095, 0.1820866141732285504 ) ) ;
#32393 = CARTESIAN_POINT ( 'NONE',  ( 1.351706036745407458, -0.4281496062992127816, -0.4176697321401328100 ) ) ;
#32394 = CARTESIAN_POINT ( 'NONE',  ( 1.279527559055118724, -0.5400638737290845981, -0.3530559997133363437 ) ) ;
#32395 = CARTESIAN_POINT ( 'NONE',  ( 0.3149606299212606708, -0.1870078740157480601, -0.3641732283464567677 ) ) ;
#32396 = CARTESIAN_POINT ( 'NONE',  ( 0.3083989501312343062, -0.3162353388693405765, 0.4822834645669290543 ) ) ;
#32397 = CARTESIAN_POINT ( 'NONE',  ( 0.4724409448818896462, 0.1265901696524990294, -1.461286089238844843 ) ) ;
#32398 = CARTESIAN_POINT ( 'NONE',  ( 0.4199475065616805614, 0.1283753931104748280, 0.1820866141732283561 ) ) ;
#32399 = CARTESIAN_POINT ( 'NONE',  ( -0.08530183727034056085, -0.05778040916215560624, -0.4822834645669293319 ) ) ;
#32400 = CARTESIAN_POINT ( 'NONE',  ( -0.3420746716998662729, 0.1974969037888702206, -1.205380577427821454 ) ) ;
#32401 = CARTESIAN_POINT ( 'NONE',  ( -1.082677165354329896, 0.1660481256975885056, 0.3530559997133364547 ) ) ;
#32402 = CARTESIAN_POINT ( 'NONE',  ( 0.4199475065616803948, -0.5023911411419708095, -0.1820866141732282451 ) ) ;
#32403 = VECTOR ( 'NONE', #73321, 39.37007874015748854 ) ;
#32404 = CARTESIAN_POINT ( 'NONE',  ( 0.3608923884514443348, 0.2066929133858267098, -0.1054918080437494132 ) ) ;
#32405 = CARTESIAN_POINT ( 'NONE',  ( -0.5446194225721777693, -0.3162353388693409650, -0.4822834645669289433 ) ) ;
#32406 = CARTESIAN_POINT ( 'NONE',  ( -0.4724409448818890911, -0.1870078740157480601, -0.3641732283464567677 ) ) ;
#32407 = LINE ( 'NONE', #52173, #62816 ) ;
#32408 = CARTESIAN_POINT ( 'NONE',  ( -0.4921259842519677963, -0.5400638737290844871, 0.3530559997133364547 ) ) ;
#32409 = CARTESIAN_POINT ( 'NONE',  ( -0.1115485564304453947, -0.6692913385826771977, 0.1292274648535927661 ) ) ;
#32410 = CARTESIAN_POINT ( 'NONE',  ( 0.3149606299212603933, -0.1870078740157479769, 0.3641732283464567677 ) ) ;
#32411 = CARTESIAN_POINT ( 'NONE',  ( -0.1070741851644051862, -0.3996062992125986590, -2.196194225721784576 ) ) ;
#32412 = CARTESIAN_POINT ( 'NONE',  ( -0.1246719160104980823, -0.6692913385826773087, -0.1292274648535924053 ) ) ;
#32413 = EDGE_CURVE ( 'NONE', #9951, #36503, #50038, .T. ) ;
#32414 = CARTESIAN_POINT ( 'NONE',  ( -0.1958661417322834497, -0.3392501089628018884, -1.720453125163043051 ) ) ;
#32415 = CARTESIAN_POINT ( 'NONE',  ( 0.6758530183727039509, -0.5511811023622046335, 0.09757992244046803654 ) ) ;
#32416 = CARTESIAN_POINT ( 'NONE',  ( 1.515748031496063186, -0.5400638737290845981, -0.3530559997133363437 ) ) ;
#32417 = CARTESIAN_POINT ( 'NONE',  ( -0.7874015748031489847, -0.1870078740157479769, 0.3641732283464567677 ) ) ;
#32418 = CARTESIAN_POINT ( 'NONE',  ( -0.7217847769028863381, -0.004921259842519870586, -0.3153832671262229437 ) ) ;
#32419 = CARTESIAN_POINT ( 'NONE',  ( -0.8595800524934373854, -0.05778040916215522460, 0.4822834645669289988 ) ) ;
#32420 = CARTESIAN_POINT ( 'NONE',  ( -0.1443569553805768291, 0.05413385826771666132, 0.4176697321401328100 ) ) ;
#32421 = CARTESIAN_POINT ( 'NONE',  ( 0.4658792650918641698, -0.08942795157528024563, -0.3641732283464568787 ) ) ;
#32422 = CARTESIAN_POINT ( 'NONE',  ( 0.3458507752293908943, 0.3458507752293908943, -2.342519685039369914 ) ) ;
#32423 = CARTESIAN_POINT ( 'NONE',  ( 1.128608923884514947, 0.1283753931104748280, 0.1820866141732283561 ) ) ;
#32424 = CARTESIAN_POINT ( 'NONE',  ( 0.8005249343832028242, -0.4281496062992127816, -0.4176697321401328100 ) ) ;
#32425 = CARTESIAN_POINT ( 'NONE',  ( 1.614173228346456712, 0.7166040191147866611, 0.1372047244094478646 ) ) ;
#32426 = CARTESIAN_POINT ( 'NONE',  ( -0.1115485564304456306, 0.2952755905511810774, -0.1292274648535930714 ) ) ;
#32427 = CARTESIAN_POINT ( 'NONE',  ( -0.1958661417322834220, -0.3392501089628018884, -1.567585301837270295 ) ) ;
#32428 = CARTESIAN_POINT ( 'NONE',  ( 1.371391076115485719, -0.5511811023622048555, -0.09757992244046775898 ) ) ;
#32429 = CARTESIAN_POINT ( 'NONE',  ( 0.6167979002624679463, 0.05413385826771626580, -0.4176697321401330321 ) ) ;
#32430 = CARTESIAN_POINT ( 'NONE',  ( 0.2296587926509192634, -0.3162353388693405765, 0.4822834645669290543 ) ) ;
#32431 = DIRECTION ( 'NONE',  ( 0.000000000000000000, 0.000000000000000000, 1.000000000000000000 ) ) ;
#32432 = CARTESIAN_POINT ( 'NONE',  ( 0.2362204724409456558, -0.1870078740157479769, 0.3641732283464567677 ) ) ;
#32433 = CARTESIAN_POINT ( 'NONE',  ( 0.7742782152230979209, 0.05413385826771626580, -0.4176697321401330321 ) ) ;
#32434 = CARTESIAN_POINT ( 'NONE',  ( -0.1246719160104980823, 0.1771653543307087630, 0.09757992244046791164 ) ) ;
#32435 = CARTESIAN_POINT ( 'NONE',  ( -0.5643044619422565855, -0.4281496062992124485, 0.4176697321401328655 ) ) ;
#32436 = CARTESIAN_POINT ( 'NONE',  ( -0.4091458600556402980, -0.2362204724409451284, -2.572178477690288734 ) ) ;
#32437 = CARTESIAN_POINT ( 'NONE',  ( -0.1574803149606292529, -0.1870078740157479769, 0.4822834645669291653 ) ) ;
#32438 = CARTESIAN_POINT ( 'NONE',  ( -1.410761154855641575, -0.3162353388693409650, -0.4822834645669289433 ) ) ;
#32439 = CARTESIAN_POINT ( 'NONE',  ( -0.6036745406824141069, 0.1283753931104748280, 0.1820866141732283561 ) ) ;
#32440 = VECTOR ( 'NONE', #14920, 39.37007874015748143 ) ;
#32441 = CARTESIAN_POINT ( 'NONE',  ( 0.2034120734908142214, 0.2952755905511810774, -0.1292274648535930714 ) ) ;
#32442 = CARTESIAN_POINT ( 'NONE',  ( -1.338582677165353729, -0.1870078740157480879, -0.4822834645669291653 ) ) ;
#32443 = CARTESIAN_POINT ( 'NONE',  ( -0.4790026246719152336, -0.05778040916215560624, -0.4822834645669293319 ) ) ;
#32444 = CARTESIAN_POINT ( 'NONE',  ( 0.4418084573054713027, 1.710857756487497383, -2.103595027339961732 ) ) ;
#32446 = CARTESIAN_POINT ( 'NONE',  ( 1.207349081364829990, -0.6046776061558809534, -0.2411417322834644161 ) ) ;
#32445 = CARTESIAN_POINT ( 'NONE',  ( -2.094141031015012366, 1.724409448818897905, 0.4359958488159718093 ) ) ;
#32447 = CARTESIAN_POINT ( 'NONE',  ( 1.345144356955381593, -0.05778040916215522460, 0.4822834645669289988 ) ) ;
#32448 = CARTESIAN_POINT ( 'NONE',  ( -0.3392501089628017219, -0.1958661417322836718, -2.406824146981627166 ) ) ;
#32449 = CARTESIAN_POINT ( 'NONE',  ( -1.646981627296586703, -0.05778040916215522460, 0.4822834645669289988 ) ) ;
#32450 = CARTESIAN_POINT ( 'NONE',  ( -1.200787401574802349, 0.1660481256975883668, -0.3530559997133364547 ) ) ;
#32451 = CARTESIAN_POINT ( 'NONE',  ( 5.785732909357575061E-17, -0.4724409448818898682, -0.7086614173228346081 ) ) ;
#32452 = CARTESIAN_POINT ( 'NONE',  ( 0.1070741851644054915, -0.3996062992125986035, -0.08530183727034119923 ) ) ;
#32453 = ORIENTED_EDGE ( 'NONE', *, *, #63059, .F. ) ;
#32454 = CARTESIAN_POINT ( 'NONE',  ( 0.006561679790026889343, -0.2845877964562161244, -0.3641732283464567121 ) ) ;
#32455 = CARTESIAN_POINT ( 'NONE',  ( 0.3917322834645670104, -0.1049643490035303411, -1.678477690288713964 ) ) ;
#32456 = VERTEX_POINT ( 'NONE', #75990 ) ;
#32457 = CARTESIAN_POINT ( 'NONE',  ( 0.1049868766404206816, -0.6046776061558809534, -0.2411417322834644161 ) ) ;
#32458 = CARTESIAN_POINT ( 'NONE',  ( 0.6036745406824153282, -0.6046776061558807314, 0.2411417322834647770 ) ) ;
#32459 = CARTESIAN_POINT ( 'NONE',  ( -0.1265901696524986964, -0.4724409448818899238, -2.749343832020996636 ) ) ;
#32460 = CARTESIAN_POINT ( 'NONE',  ( 1.614173228346457378, 0.7794589730112001513, -0.1372047244094476148 ) ) ;
#32461 = CARTESIAN_POINT ( 'NONE',  ( -0.2690288713910754526, -0.5511811023622046335, 0.09757992244046803654 ) ) ;
#32462 = CARTESIAN_POINT ( 'NONE',  ( 0.1181102362204724532, 0.09842519685039372024, -1.432673802628665356E-17 ) ) ;
#32463 = CARTESIAN_POINT ( 'NONE',  ( 0.8661417322834653598, -0.1870078740157479769, 0.4822834645669291653 ) ) ;
#32464 = CARTESIAN_POINT ( 'NONE',  ( 1.030183727034121421, -0.2845877964562161244, -0.3641732283464567121 ) ) ;
#32465 = CARTESIAN_POINT ( 'NONE',  ( -0.6167979002624665030, -0.4281496062992127816, -0.4176697321401328100 ) ) ;
#32466 = CARTESIAN_POINT ( 'NONE',  ( -0.3392501089628018329, -0.1958661417322836440, -1.234888820701100398 ) ) ;
#32467 = CARTESIAN_POINT ( 'NONE',  ( -0.8202099737532799750, 0.2952755905511810774, -0.1292274648535930714 ) ) ;
#32468 = CARTESIAN_POINT ( 'NONE',  ( -1.220472440944881054, 0.1771653543307087630, 0.000000000000000000 ) ) ;
#32469 = CARTESIAN_POINT ( 'NONE',  ( -1.017060367454067249, -0.3162353388693409650, -0.4822834645669289433 ) ) ;
#32470 = CARTESIAN_POINT ( 'NONE',  ( 1.194225721784777594, 0.05413385826771666132, 0.4176697321401328100 ) ) ;
#32471 = CARTESIAN_POINT ( 'NONE',  ( -0.4252607725274083483, 1.326635381343780562, -2.077176919885365791 ) ) ;
#32472 = VERTEX_POINT ( 'NONE', #82306 ) ;
#32473 = CARTESIAN_POINT ( 'NONE',  ( -0.3917322834645671770, 0.1049643490035302024, -2.549231914207035654 ) ) ;
#32474 = CARTESIAN_POINT ( 'NONE',  ( 0.1640419947506569498, -0.3162353388693409650, -0.4822834645669289433 ) ) ;
#32475 = VERTEX_POINT ( 'NONE', #63344 ) ;
#32476 = CARTESIAN_POINT ( 'NONE',  ( -0.9251968503937002541, 0.1660481256975885056, 0.3530559997133364547 ) ) ;
#32477 = CARTESIAN_POINT ( 'NONE',  ( 1.259842519685040019, -0.1870078740157479769, 0.4822834645669291653 ) ) ;
#32478 = CARTESIAN_POINT ( 'NONE',  ( 1.220472440944882386, -0.6692913385826771977, 8.415575281601705876E-17 ) ) ;
#32479 = CARTESIAN_POINT ( 'NONE',  ( 0.07217847769028949700, -0.05778040916215560624, -0.4822834645669293319 ) ) ;
#32480 = CARTESIAN_POINT ( 'NONE',  ( 0.1181102362204730916, 0.2952755905511811885, 0.000000000000000000 ) ) ;
#32481 = CARTESIAN_POINT ( 'NONE',  ( -0.1958661417322836718, 0.3392501089628017219, -1.830052493438320216 ) ) ;
#32482 = CARTESIAN_POINT ( 'NONE',  ( -1.187664041994750175, -0.05778040916215560624, -0.4822834645669293319 ) ) ;
#32483 = CARTESIAN_POINT ( 'NONE',  ( -0.3149606299212590610, -0.1870078740157480879, -0.4822834645669291653 ) ) ;
#32484 = CARTESIAN_POINT ( 'NONE',  ( -0.2362204724409440182, -0.1870078740157479769, 0.3641732283464567677 ) ) ;
#32485 = CARTESIAN_POINT ( 'NONE',  ( 1.080276388343102000E-18, 0.000000000000000000, 0.000000000000000000 ) ) ;
#32486 = CARTESIAN_POINT ( 'NONE',  ( 1.476377952755906442, -0.5400638737290844871, 0.3530559997133364547 ) ) ;
#32487 = CARTESIAN_POINT ( 'NONE',  ( -0.4265091863517051496, 0.2952755905511810774, -0.1292274648535930714 ) ) ;
#32488 = FACE_OUTER_BOUND ( 'NONE', #57317, .T. ) ;
#32489 = CARTESIAN_POINT ( 'NONE',  ( 1.069553805774278610, -0.6692913385826771977, 0.1292274648535927661 ) ) ;
#32490 = CARTESIAN_POINT ( 'NONE',  ( 0.5380577427821529035, 0.009842519685039144428, -0.3409548833797004797 ) ) ;
#32491 = ORIENTED_EDGE ( 'NONE', *, *, #16141, .F. ) ;
#32492 = ORIENTED_EDGE ( 'NONE', *, *, #65884, .T. ) ;
#32493 = CARTESIAN_POINT ( 'NONE',  ( 0.4133858267716541968, 0.1660481256975885056, 0.3530559997133364547 ) ) ;
#32494 = CARTESIAN_POINT ( 'NONE',  ( -0.3215223097112853146, -0.2845877964562159024, 0.3641732283464567677 ) ) ;
#32496 = CARTESIAN_POINT ( 'NONE',  ( -1.220472440944881054, 0.2952755905511811885, 0.000000000000000000 ) ) ;
#32495 = CARTESIAN_POINT ( 'NONE',  ( 1.601049868766404982, -0.5023911411419708095, -0.1820866141732282451 ) ) ;
#32497 = CARTESIAN_POINT ( 'NONE',  ( 0.4724409448818897572, -0.1265901696524988906, -0.3458005249343831244 ) ) ;
#32498 = CARTESIAN_POINT ( 'NONE',  ( 1.673228346456693494, 0.07958543189024085140, 0.2665933059059887866 ) ) ;
#32499 = CARTESIAN_POINT ( 'NONE',  ( 1.568241469816273437, -0.3162353388693405765, 0.4822834645669290543 ) ) ;
#32500 = CARTESIAN_POINT ( 'NONE',  ( 4.893765752498283308E-17, -0.3996062992125985480, -2.832677165354331006 ) ) ;
#32501 = PRODUCT_DEFINITION_SHAPE ( 'NONE', 'NONE',  #83312 ) ;
#32502 = CARTESIAN_POINT ( 'NONE',  ( -0.1574803149606292529, -0.1870078740157479769, 0.4822834645669291653 ) ) ;
#32503 = CARTESIAN_POINT ( 'NONE',  ( 1.928577636452524918E-17, 0.5905511811023621549, 0.1574803149606299746 ) ) ;
#32504 = CARTESIAN_POINT ( 'NONE',  ( -1.594488188976377563, -0.5400638737290844871, 0.3530559997133364547 ) ) ;
#32505 = CARTESIAN_POINT ( 'NONE',  ( 0.2952755905511816326, -0.5400638737290844871, 0.3530559997133364547 ) ) ;
#32506 = CARTESIAN_POINT ( 'NONE',  ( 0.3949938075777409408, -0.1058382717557499186, 0.1266404199475065773 ) ) ;
#32507 = CARTESIAN_POINT ( 'NONE',  ( -1.627296587926508442, 0.1283753931104748280, 0.1820866141732283561 ) ) ;
#32508 = CARTESIAN_POINT ( 'NONE',  ( 0.8136482939632553313, 0.2306618581243848609, 0.2411417322834645549 ) ) ;
#32509 = AXIS2_PLACEMENT_3D ( 'NONE', #82158, #38760, #64437 ) ;
#32510 = CARTESIAN_POINT ( 'NONE',  ( 1.062992125984252745, 0.1771653543307087630, 0.000000000000000000 ) ) ;
#32511 = CARTESIAN_POINT ( 'NONE',  ( 0.2063662664111909073, 1.075973491904217871, 0.2356306219338031305 ) ) ;
#32512 = CARTESIAN_POINT ( 'NONE',  ( 1.017060367454068803, -0.2845877964562159024, 0.3641732283464567677 ) ) ;
#32513 = CARTESIAN_POINT ( 'NONE',  ( -1.476377952755905110, 0.1660481256975885056, 0.3530559997133364547 ) ) ;
#32514 = CARTESIAN_POINT ( 'NONE',  ( -0.3996062992125986590, 0.1070741851644051723, -1.054461942257217899 ) ) ;
#32515 = CARTESIAN_POINT ( 'NONE',  ( 0.9711286089238851948, -0.6046776061558809534, -0.2411417322834644161 ) ) ;
#32516 = CARTESIAN_POINT ( 'NONE',  ( 0.1049643490035303689, 0.3917322834645670104, -0.7729658792650916377 ) ) ;
#32518 = CARTESIAN_POINT ( 'NONE',  ( -0.4724409448818898682, -8.678599364036362592E-17, -1.141732283464566899 ) ) ;
#32517 = CARTESIAN_POINT ( 'NONE',  ( 0.6627296587926517768, -0.6692913385826773087, -0.1292274648535924053 ) ) ;
#32519 = CARTESIAN_POINT ( 'NONE',  ( -1.581364829396324945, -0.2845877964562159024, 0.3641732283464567677 ) ) ;
#32520 = CARTESIAN_POINT ( 'NONE',  ( 0.5774278215223103139, -0.5023911411419708095, -0.1820866141732282451 ) ) ;
#32521 = CARTESIAN_POINT ( 'NONE',  ( 0.5052493438320218022, -0.6692913385826773087, -0.1292274648535924053 ) ) ;
#32522 = CARTESIAN_POINT ( 'NONE',  ( -0.4359958488159792478, 1.724409448818897683, 2.094141031014984389 ) ) ;
#32523 = CARTESIAN_POINT ( 'NONE',  ( -0.8792650918635160906, -0.004921259842519870586, -0.3153832671262229437 ) ) ;
#32524 = CARTESIAN_POINT ( 'NONE',  ( -1.194225721784776262, 0.05413385826771626580, -0.4176697321401330321 ) ) ;
#32525 = CARTESIAN_POINT ( 'NONE',  ( 1.522309711286089939, 0.2306618581243848609, 0.2411417322834645549 ) ) ;
#32526 = CARTESIAN_POINT ( 'NONE',  ( -1.272965879265091305, -0.4281496062992124485, 0.4176697321401328655 ) ) ;
#32527 = CARTESIAN_POINT ( 'NONE',  ( 0.7874015748031503170, -0.1870078740157480879, -0.4822834645669291653 ) ) ;
#32528 = CARTESIAN_POINT ( 'NONE',  ( -1.253280839895012377, -0.2845877964562161244, -0.3641732283464567121 ) ) ;
#32529 = LINE ( 'NONE', #53127, #51758 ) ;
#32530 = CARTESIAN_POINT ( 'NONE',  ( 1.154855643044620184, 0.2306618581243847221, -0.2411417322834647770 ) ) ;
#32531 = CARTESIAN_POINT ( 'NONE',  ( -1.157146581871515012E-16, 0.4724409448818898682, -2.596456692913385655 ) ) ;
#32532 = CARTESIAN_POINT ( 'NONE',  ( -1.430446194225721390, -0.4281496062992124485, 0.4176697321401328655 ) ) ;
#32533 = CARTESIAN_POINT ( 'NONE',  ( 1.220472440944882608, 0.2952755905511811885, 0.000000000000000000 ) ) ;
#32534 = CARTESIAN_POINT ( 'NONE',  ( -0.8727034120734901146, -0.08942795157528024563, -0.3641732283464568787 ) ) ;
#32535 = CARTESIAN_POINT ( 'NONE',  ( 1.482939632545932307, -0.3690944881889763329, 0.3153832671262228327 ) ) ;
#32536 = CARTESIAN_POINT ( 'NONE',  ( -1.207349081364828436, -0.5023911411419708095, 0.1820866141732285504 ) ) ;
#32537 = CARTESIAN_POINT ( 'NONE',  ( -0.4986876640419939388, 0.1283753931104746893, -0.1820866141732285504 ) ) ;
#32538 = CARTESIAN_POINT ( 'NONE',  ( -1.469816272965878357, -0.5023911411419708095, -0.1820866141732282451 ) ) ;
#32539 = CARTESIAN_POINT ( 'NONE',  ( 0.8464566929133865436, 0.07958543189024071263, -0.2665933059059888421 ) ) ;
#32540 = CARTESIAN_POINT ( 'NONE',  ( 0.3412073490813655186, -0.6046776061558809534, -0.2411417322834644161 ) ) ;
#32541 = DIRECTION ( 'NONE',  ( 0.000000000000000000, 0.000000000000000000, -1.000000000000000000 ) ) ;
#32542 = CARTESIAN_POINT ( 'NONE',  ( -0.1443569553805765515, -0.4281496062992127816, -0.4176697321401328100 ) ) ;
#32543 = EDGE_CURVE ( 'NONE', #76877, #72166, #55997, .T. ) ;
#32544 = CARTESIAN_POINT ( 'NONE',  ( 0.5839895013123367340, -0.5511811023622048555, -0.09757992244046775898 ) ) ;
#32545 = CARTESIAN_POINT ( 'NONE',  ( -1.620734908136482577, 0.2952755905511811885, 0.1292274648535926551 ) ) ;
#32546 = EDGE_CURVE ( 'NONE', #47373, #38086, #82215, .T. ) ;
#32547 = CARTESIAN_POINT ( 'NONE',  ( -1.384514435695537005, -0.6692913385826773087, -0.1292274648535924053 ) ) ;
#32548 = CARTESIAN_POINT ( 'NONE',  ( -0.3477690288713905509, -0.6692913385826771977, 0.1292274648535927661 ) ) ;
#32549 = CARTESIAN_POINT ( 'NONE',  ( -0.3460692066303960868, 0.1998031496062990242, -0.4986876640419947715 ) ) ;
#32550 = CARTESIAN_POINT ( 'NONE',  ( 0.2925321140481932369, -0.2925321140481931814, -2.852362204724409711 ) ) ;
#32551 = CARTESIAN_POINT ( 'NONE',  ( -0.08530183727034056085, -0.05778040916215560624, -0.4822834645669293319 ) ) ;
#32552 = CARTESIAN_POINT ( 'NONE',  ( 1.082677165354331228, -0.4536011799217367080, 0.2665933059059888421 ) ) ;
#32553 = CARTESIAN_POINT ( 'NONE',  ( -0.3149606299212590610, -0.1870078740157480879, -0.4822834645669291653 ) ) ;
#32554 = CARTESIAN_POINT ( 'NONE',  ( 0.2099737532808405305, 0.2306618581243847221, -0.2411417322834647770 ) ) ;
#32555 = CARTESIAN_POINT ( 'NONE',  ( 0.1070741851644054915, -0.3996062992125986035, -2.604986876640420057 ) ) ;
#32556 = CARTESIAN_POINT ( 'NONE',  ( -0.3420746716998661618, 0.1974969037888702206, -2.073490813648294129 ) ) ;
#32557 = CARTESIAN_POINT ( 'NONE',  ( 0.3392501089628018884, -0.1958661417322834220, -0.5695538057742781657 ) ) ;
#32558 = LINE ( 'NONE', #70875, #31800 ) ;
#32559 = CARTESIAN_POINT ( 'NONE',  ( 0.3917322834645670104, 2.398668435337828261E-17, -1.055118110236220375 ) ) ;
#32560 = CARTESIAN_POINT ( 'NONE',  ( -1.154855643044618851, -0.5023911411419708095, -0.1820866141732282451 ) ) ;
#32561 = CARTESIAN_POINT ( 'NONE',  ( 0.3392501089628018884, -0.1958661417322834220, -1.199475065616797842 ) ) ;
#32562 = CARTESIAN_POINT ( 'NONE',  ( -0.9580052493438311334, -0.4281496062992124485, 0.4176697321401328655 ) ) ;
#32563 = AXIS2_PLACEMENT_3D ( 'NONE', #27070, #46419, #72111 ) ;
#32564 = CARTESIAN_POINT ( 'NONE',  ( 0.2867679344610365999, 0.2867679344610365999, 0.09713217667422754942 ) ) ;
#32565 = CARTESIAN_POINT ( 'NONE',  ( 0.5380577427821529035, -0.4281496062992124485, 0.4176697321401328655 ) ) ;
#32566 = EDGE_CURVE ( 'NONE', #14206, #15218, #40961, .T. ) ;
#32567 = CARTESIAN_POINT ( 'NONE',  ( 1.213910761154856299, -0.6692913385826773087, -0.1292274648535924053 ) ) ;
#32568 = CARTESIAN_POINT ( 'NONE',  ( 0.5774278215223103139, -0.6046776061558809534, -0.2411417322834644161 ) ) ;
#32569 = CARTESIAN_POINT ( 'NONE',  ( -0.3458507752293906723, -0.3458507752293910609, -2.736220472440944018 ) ) ;
#32570 = CARTESIAN_POINT ( 'NONE',  ( -9.787531504996567848E-17, 0.3996062992125986035, -2.519685039370078705 ) ) ;
#32571 = CARTESIAN_POINT ( 'NONE',  ( 0.3917322834645670659, 2.398668435337828261E-17, -1.217210916831708012 ) ) ;
#32572 = CARTESIAN_POINT ( 'NONE',  ( 1.154855643044620184, -0.6046776061558807314, 0.2411417322834647770 ) ) ;
#32573 = CARTESIAN_POINT ( 'NONE',  ( 0.3740157480314966754, 0.1660481256975883668, -0.3530559997133364547 ) ) ;
#32574 = CARTESIAN_POINT ( 'NONE',  ( 0.09186351706036799403, -0.4281496062992127816, -0.4176697321401328100 ) ) ;
#32575 = CARTESIAN_POINT ( 'NONE',  ( 0.6233595800524939223, -0.2845877964562159024, 0.3641732283464567677 ) ) ;
#32576 = CARTESIAN_POINT ( 'NONE',  ( 1.141732283464567788, -0.6692913385826771977, 8.415575281601705876E-17 ) ) ;
#32577 = APPLICATION_CONTEXT ( 'automotive_design' ) ;
#32578 = CARTESIAN_POINT ( 'NONE',  ( 0.2867679344610365999, -0.2867679344610365444, -0.02559055118110245899 ) ) ;
#32579 = CARTESIAN_POINT ( 'NONE',  ( -0.07874015748031421014, -0.1870078740157480879, -0.4822834645669291653 ) ) ;
#32580 = CARTESIAN_POINT ( 'NONE',  ( 0.8792650918635177559, 0.05413385826771666132, 0.4176697321401328100 ) ) ;
#32581 = CARTESIAN_POINT ( 'NONE',  ( 0.4724409448818904789, -0.1870078740157480879, -0.4822834645669291653 ) ) ;
#32582 = CARTESIAN_POINT ( 'NONE',  ( 1.266404199475066328, -0.2845877964562161244, -0.3641732283464567121 ) ) ;
#32583 = CARTESIAN_POINT ( 'NONE',  ( -0.8202099737532801971, -0.6692913385826771977, 0.1292274648535927661 ) ) ;
#32584 = CARTESIAN_POINT ( 'NONE',  ( -0.8333333333333323711, -0.6692913385826773087, -0.1292274648535924053 ) ) ;
#32585 = CARTESIAN_POINT ( 'NONE',  ( 1.148293963254593653, 0.2952755905511810774, -0.1292274648535930714 ) ) ;
#32586 = CARTESIAN_POINT ( 'NONE',  ( -0.1504864506472308738, -0.3622863298698439927, -1.929133858267717549 ) ) ;
#32587 = CARTESIAN_POINT ( 'NONE',  ( -0.3917322834645670104, -7.196005306013484475E-17, -1.921259842519684957 ) ) ;
#32588 = CARTESIAN_POINT ( 'NONE',  ( -0.2867679344610365999, 0.2867679344610364889, -2.846456692913385655 ) ) ;
#32589 = VERTEX_POINT ( 'NONE', #19978 ) ;
#32590 = CARTESIAN_POINT ( 'NONE',  ( 4.893765752498283924E-17, -0.3996062992125986035, 0.07874015748031494566 ) ) ;
#32591 = ORIENTED_EDGE ( 'NONE', *, *, #13980, .T. ) ;
#32592 = CARTESIAN_POINT ( 'NONE',  ( 1.587926509186352586, -0.4281496062992127816, -0.4176697321401328100 ) ) ;
#32593 = CARTESIAN_POINT ( 'NONE',  ( 0.9448818897637802916, -0.1870078740157479769, 0.3641732283464567677 ) ) ;
#32594 = CARTESIAN_POINT ( 'NONE',  ( 0.1998031496062994405, -0.3460692066303958092, -1.981627296587926690 ) ) ;
#32595 = DIRECTION ( 'NONE',  ( 1.000000000000000000, -0.000000000000000000, -0.000000000000000000 ) ) ;
#32596 = CARTESIAN_POINT ( 'NONE',  ( -0.01711285633636233997, 1.063222675620814073, 2.873802023517004312 ) ) ;
#32597 = DIRECTION ( 'NONE',  ( 0.000000000000000000, 0.000000000000000000, -1.000000000000000000 ) ) ;
#32598 = CARTESIAN_POINT ( 'NONE',  ( 0.1958661417322836440, -0.3392501089628017219, -0.9639107611548557442 ) ) ;
#32599 = CARTESIAN_POINT ( 'NONE',  ( -1.233595800524933894, -0.5023911411419708095, -0.1820866141732282451 ) ) ;
#32600 = CARTESIAN_POINT ( 'NONE',  ( -1.515748031496062076, 0.07958543189024071263, -0.2665933059059888421 ) ) ;
#32601 = CARTESIAN_POINT ( 'NONE',  ( -1.253280839895012377, -0.3162353388693409650, -0.4822834645669289433 ) ) ;
#32602 = CARTESIAN_POINT ( 'NONE',  ( -0.4265091863517051496, 0.2952755905511810774, -0.1292274648535930714 ) ) ;
#32603 = CARTESIAN_POINT ( 'NONE',  ( -1.646981627296586703, -0.05778040916215522460, 0.4822834645669289988 ) ) ;
#32604 = ORIENTED_EDGE ( 'NONE', *, *, #19758, .F. ) ;
#32605 = CARTESIAN_POINT ( 'NONE',  ( 0.3499960723095488224, 0.3045081538226084295, -0.01928741089222631502 ) ) ;
#32606 = DIRECTION ( 'NONE',  ( -1.000000000000000000, 0.000000000000000000, -6.982962677686266711E-15 ) ) ;
#32607 = B_SPLINE_CURVE_WITH_KNOTS ( 'NONE', 3,
 ( #27497, #59483, #35063, #34656 ),
 .UNSPECIFIED., .F., .F.,
 ( 4, 4 ),
 ( 0.01019635767495674639, 0.01088423237384165791 ),
 .UNSPECIFIED. ) ;
#32608 = CARTESIAN_POINT ( 'NONE',  ( -0.1265901696524993347, 0.4724409448818896462, -2.683727034120734878 ) ) ;
#32609 = CARTESIAN_POINT ( 'NONE',  ( -1.614173228346457378, 1.543375672658094944, 0.1372047244094476981 ) ) ;
#32610 = CARTESIAN_POINT ( 'NONE',  ( -0.9186351706036736120, -0.5023911411419708095, -0.1820866141732282451 ) ) ;
#32611 = CARTESIAN_POINT ( 'NONE',  ( 0.9186351706036752773, 0.1539470093639521697, -0.1968503937007875793 ) ) ;
#32612 = CARTESIAN_POINT ( 'NONE',  ( 0.5446194225721792126, -0.3162353388693405765, 0.4822834645669290543 ) ) ;
#32613 = ORIENTED_EDGE ( 'NONE', *, *, #54463, .T. ) ;
#32615 = CARTESIAN_POINT ( 'NONE',  ( -0.1265901696524986964, -0.4724409448818899238, -2.668635170603674833 ) ) ;
#32614 = CARTESIAN_POINT ( 'NONE',  ( -0.3307086614173228023, 0.3647102339900947787, 0.000000000000000000 ) ) ;
#32616 = CARTESIAN_POINT ( 'NONE',  ( 1.279527559055118724, -0.5400638737290845981, -0.3530559997133363437 ) ) ;
#32617 = CARTESIAN_POINT ( 'NONE',  ( -1.561679790026246017, 0.05413385826771666132, 0.4176697321401328100 ) ) ;
#32618 = CARTESIAN_POINT ( 'NONE',  ( -0.1958661417322836440, 0.3392501089628016664, -0.8805581120396831496 ) ) ;
#32619 = CARTESIAN_POINT ( 'NONE',  ( -0.4396325459317579898, 0.1771653543307087630, 0.09757992244046791164 ) ) ;
#32620 = CARTESIAN_POINT ( 'NONE',  ( -1.627296587926508442, 0.1283753931104748280, 0.1820866141732283561 ) ) ;
#32621 = CARTESIAN_POINT ( 'NONE',  ( -0.2867679344610366554, 0.2867679344610365444, -1.206692913385826849 ) ) ;
#32622 = CARTESIAN_POINT ( 'NONE',  ( -0.3805774278215216522, -0.004921259842519576551, 0.3153832671262227771 ) ) ;
#32623 = CARTESIAN_POINT ( 'NONE',  ( 0.1968503937007881344, 0.1771653543307087630, 0.000000000000000000 ) ) ;
#32624 = CARTESIAN_POINT ( 'NONE',  ( -0.07874015748031421014, -0.1870078740157480879, -0.4822834645669291653 ) ) ;
#32625 = CARTESIAN_POINT ( 'NONE',  ( -1.148293963254592542, 0.1771653543307087630, 0.09757992244046791164 ) ) ;
#32626 = CARTESIAN_POINT ( 'NONE',  ( -0.1958661417322834220, -0.3392501089628018884, -2.577427821522309426 ) ) ;
#32627 = CARTESIAN_POINT ( 'NONE',  ( 1.187664041994751285, -0.3162353388693409650, -0.4822834645669289433 ) ) ;
#32628 = EDGE_CURVE ( 'NONE', #51375, #41668, #32183, .T. ) ;
#32629 = CARTESIAN_POINT ( 'NONE',  ( -1.515748031496062076, -0.5400638737290844871, 0.3530559997133364547 ) ) ;
#32630 = CARTESIAN_POINT ( 'NONE',  ( -0.1265901696524993347, 0.4724409448818895907, -1.185695538057742526 ) ) ;
#32631 = CARTESIAN_POINT ( 'NONE',  ( -0.3412073490813641308, -0.6046776061558807314, 0.2411417322834647770 ) ) ;
#32632 = CARTESIAN_POINT ( 'NONE',  ( 0.2230971128608929543, -0.004921259842519870586, -0.3153832671262229437 ) ) ;
#32633 = CARTESIAN_POINT ( 'NONE',  ( -0.7939632545931750718, -0.05778040916215560624, -0.4822834645669293319 ) ) ;
#32634 = CARTESIAN_POINT ( 'NONE',  ( 0.8202099737532814183, -0.5511811023622048555, -0.09757992244046775898 ) ) ;
#32635 = CARTESIAN_POINT ( 'NONE',  ( -0.4461942257217840213, 0.1283753931104748280, 0.1820866141732283561 ) ) ;
#32636 = CARTESIAN_POINT ( 'NONE',  ( -0.8333333333333323711, -0.6692913385826773087, -0.1292274648535924053 ) ) ;
#32637 = CARTESIAN_POINT ( 'NONE',  ( -1.496062992125983815, -0.1870078740157479769, 0.4822834645669291653 ) ) ;
#32638 = DIRECTION ( 'NONE',  ( -0.7119855458575206075, 0.7021941202331221099, 0.000000000000000000 ) ) ;
#32639 = CARTESIAN_POINT ( 'NONE',  ( 1.351706036745407680, -0.004921259842519576551, 0.3153832671262227771 ) ) ;
#32640 = CARTESIAN_POINT ( 'NONE',  ( -1.528871391076114250, -0.6692913385826771977, 0.1292274648535927661 ) ) ;
#32641 = CARTESIAN_POINT ( 'NONE',  ( -1.640419947506561060, -0.4281496062992127816, -0.4176697321401328100 ) ) ;
#32642 = ORIENTED_EDGE ( 'NONE', *, *, #4112, .T. ) ;
#32643 = CARTESIAN_POINT ( 'NONE',  ( 0.3460692066303959202, -0.1998031496062991630, -2.386482939632545985 ) ) ;
#32644 = CARTESIAN_POINT ( 'NONE',  ( -0.7152230971128602510, -0.2845877964562159024, 0.3641732283464567677 ) ) ;
#32645 = CARTESIAN_POINT ( 'NONE',  ( 0.7283464566929140904, -0.5400638737290845981, -0.3530559997133363437 ) ) ;
#32646 = CARTESIAN_POINT ( 'NONE',  ( -0.9251968503937002541, 0.07958543189024085140, 0.2665933059059887866 ) ) ;
#32647 = CARTESIAN_POINT ( 'NONE',  ( 0.2925321140481932369, -0.2925321140481931814, -1.907480314960629642 ) ) ;
#32648 = CARTESIAN_POINT ( 'NONE',  ( -1.167979002624671470, -0.4281496062992127816, -0.4176697321401328100 ) ) ;
#32649 = CARTESIAN_POINT ( 'NONE',  ( 0.6561679790026253567, -0.6046776061558809534, -0.2411417322834644161 ) ) ;
#32650 = CARTESIAN_POINT ( 'NONE',  ( 0.3805774278215230400, -0.4281496062992124485, 0.4176697321401328655 ) ) ;
#32651 = CARTESIAN_POINT ( 'NONE',  ( 1.614173228346457378, 0.2952755905511811885, 0.000000000000000000 ) ) ;
#32652 = CARTESIAN_POINT ( 'NONE',  ( -1.660104986876639543, -0.08942795157528024563, -0.3641732283464568787 ) ) ;
#32653 = CARTESIAN_POINT ( 'NONE',  ( -0.3460692066303957537, -0.1998031496062994405, -1.074146981627296604 ) ) ;
#32654 = CARTESIAN_POINT ( 'NONE',  ( -0.2925321140481930704, -0.2925321140481933480, -1.003937007874015741 ) ) ;
#32655 = CARTESIAN_POINT ( 'NONE',  ( -0.3949938075777409963, -7.255918531996591613E-17, -0.5118110236220473341 ) ) ;
#32656 = CARTESIAN_POINT ( 'NONE',  ( 1.028546380722451081, 1.694949792723957183, 0.4486317206264757718 ) ) ;
#32657 = CARTESIAN_POINT ( 'NONE',  ( 0.8858267716535438430, 0.07958543189024085140, 0.2665933059059887866 ) ) ;
#32658 = CARTESIAN_POINT ( 'NONE',  ( 0.4790026246719167324, -0.08942795157527998196, 0.3641732283464567121 ) ) ;
#32659 = CARTESIAN_POINT ( 'NONE',  ( -0.03937007874015669567, -0.6692913385826771977, 8.415575281601705876E-17 ) ) ;
#32660 = CARTESIAN_POINT ( 'NONE',  ( 1.351706036745407458, -0.4281496062992127816, -0.4176697321401328100 ) ) ;
#32661 = CARTESIAN_POINT ( 'NONE',  ( -0.2891555358219909388, -0.2891555358219912164, -1.395669291338582418 ) ) ;
#32662 = CARTESIAN_POINT ( 'NONE',  ( 0.4855643044619430415, -0.3690944881889765550, -0.3153832671262227771 ) ) ;
#32663 = CARTESIAN_POINT ( 'NONE',  ( -0.7480314960629914633, -0.6692913385826771977, 8.415575281601705876E-17 ) ) ;
#32664 = CARTESIAN_POINT ( 'NONE',  ( -1.135170603674539924, 0.2952755905511810774, -0.1292274648535930714 ) ) ;
#32665 = CARTESIAN_POINT ( 'NONE',  ( 0.9055118110236227702, 0.2952755905511811885, 0.000000000000000000 ) ) ;
#32666 = CARTESIAN_POINT ( 'NONE',  ( -0.1265901696524993347, 0.4724409448818895907, -1.738845144356955696 ) ) ;
#32667 = CARTESIAN_POINT ( 'NONE',  ( 0.1998031496062994405, -0.3460692066303958092, -2.611548556430446144 ) ) ;
#32668 = ORIENTED_EDGE ( 'NONE', *, *, #73267, .F. ) ;
#32669 = ORIENTED_EDGE ( 'NONE', *, *, #72215, .T. ) ;
#32670 = VECTOR ( 'NONE', #82149, 39.37007874015748143 ) ;
#32671 = CARTESIAN_POINT ( 'NONE',  ( -1.345144356955379816, -0.05778040916215560624, -0.4822834645669293319 ) ) ;
#32672 = CARTESIAN_POINT ( 'NONE',  ( -0.5511811023622038563, -0.1870078740157479769, 0.4822834645669291653 ) ) ;
#32674 = CARTESIAN_POINT ( 'NONE',  ( -0.8267716535433065062, 0.2952755905511811885, 0.000000000000000000 ) ) ;
#32673 = CARTESIAN_POINT ( 'NONE',  ( -0.9055118110236215490, -0.5511811023622047445, 6.969142054262312111E-17 ) ) ;
#32675 = CARTESIAN_POINT ( 'NONE',  ( 0.3917322834645669549, 2.398668435337827645E-17, -1.930426878443882943 ) ) ;
#32676 = CARTESIAN_POINT ( 'NONE',  ( -0.3996062992125985480, -7.340648628747423112E-17, -2.793307086614173151 ) ) ;
#32677 = CARTESIAN_POINT ( 'NONE',  ( -1.509186351706035767, -0.3690944881889763329, 0.3153832671262228327 ) ) ;
#32678 = CARTESIAN_POINT ( 'NONE',  ( -1.036745406824146176, 0.05413385826771626580, -0.4176697321401330321 ) ) ;
#32679 = CARTESIAN_POINT ( 'NONE',  ( 0.3871391076115492380, -0.05778040916215560624, -0.4822834645669293319 ) ) ;
#32680 = CARTESIAN_POINT ( 'NONE',  ( -0.7808398950131222316, -0.3162353388693409650, -0.4822834645669289433 ) ) ;
#32681 = CARTESIAN_POINT ( 'NONE',  ( 0.6496062992125991586, 0.1660481256975885056, 0.3530559997133364547 ) ) ;
#32682 = CARTESIAN_POINT ( 'NONE',  ( 0.3917322834645670104, -0.1049643490035303411, -1.363517060367453793 ) ) ;
#32683 = CARTESIAN_POINT ( 'NONE',  ( -1.030183727034119867, -0.2845877964562159024, 0.3641732283464567677 ) ) ;
#32684 = EDGE_LOOP ( 'NONE', ( #62214, #76697, #72568, #37421 ) ) ;
#32685 = CARTESIAN_POINT ( 'NONE',  ( 0.3420746716998660508, -0.1974969037888703871, -1.679790026246719359 ) ) ;
#32686 = ORIENTED_EDGE ( 'NONE', *, *, #32099, .T. ) ;
#32687 = CARTESIAN_POINT ( 'NONE',  ( -0.3149606299212553973, -5.463695987328517809E-17, -1.076935383196058860 ) ) ;
#32688 = CARTESIAN_POINT ( 'NONE',  ( -1.253280839895012377, -0.05778040916215522460, 0.4822834645669289988 ) ) ;
#32689 = CARTESIAN_POINT ( 'NONE',  ( -1.286089238845143479, 0.2306618581243847221, -0.2411417322834647770 ) ) ;
#32690 = CARTESIAN_POINT ( 'NONE',  ( 0.3460692066303959202, 0.1998031496062993295, -0.1312335958005249603 ) ) ;
#32691 = CARTESIAN_POINT ( 'NONE',  ( -1.259842519685038686, -0.1870078740157479769, 0.4822834645669291653 ) ) ;
#32692 = CARTESIAN_POINT ( 'NONE',  ( -1.194225721784776262, 0.05413385826771626580, -0.4176697321401330321 ) ) ;
#32693 = CARTESIAN_POINT ( 'NONE',  ( -1.371391076115484609, -0.6692913385826771977, 0.1292274648535927661 ) ) ;
#32694 = FILL_AREA_STYLE ('',( #59617 ) ) ;
#32695 = EDGE_CURVE ( 'NONE', #22673, #48423, #7345, .T. ) ;
#32696 = CARTESIAN_POINT ( 'NONE',  ( -0.3392501089628019995, 0.1958661417322832277, 0.2040682414698161695 ) ) ;
#32697 = CARTESIAN_POINT ( 'NONE',  ( 0.07217847769028949700, -0.2845877964562159024, 0.3641732283464567677 ) ) ;
#32698 = DIRECTION ( 'NONE',  ( -0.000000000000000000, -1.000000000000000000, -0.000000000000000000 ) ) ;
#32699 = CARTESIAN_POINT ( 'NONE',  ( -0.1049643490035307020, 0.3917322834645669549, -0.4061679790026246351 ) ) ;
#32700 = CARTESIAN_POINT ( 'NONE',  ( -0.3937007874015740483, -0.1870078740157480601, -0.3641732283464567677 ) ) ;
#32701 = CARTESIAN_POINT ( 'NONE',  ( -0.9186351706036736120, -0.6046776061558809534, -0.2411417322834644161 ) ) ;
#32702 = EDGE_CURVE ( 'NONE', #56386, #20489, #67439, .T. ) ;
#32703 = CARTESIAN_POINT ( 'NONE',  ( 1.213910761154856299, -0.6692913385826773087, -0.1292274648535924053 ) ) ;
#32704 = CARTESIAN_POINT ( 'NONE',  ( -0.6955380577427815458, 0.05413385826771666132, 0.4176697321401328100 ) ) ;
#32705 = ORIENTED_EDGE ( 'NONE', *, *, #48920, .F. ) ;
#32706 = ORIENTED_EDGE ( 'NONE', *, *, #71071, .F. ) ;
#32707 = CARTESIAN_POINT ( 'NONE',  ( 0.3996062992125984925, 0.1070741851644054637, -1.933727034120735100 ) ) ;
#32708 = CARTESIAN_POINT ( 'NONE',  ( -0.9776902887139098386, 0.2952755905511810774, -0.1292274648535930714 ) ) ;
#32709 = CARTESIAN_POINT ( 'NONE',  ( 1.364829396325459854, -0.6046776061558809534, -0.2411417322834644161 ) ) ;
#32710 = CARTESIAN_POINT ( 'NONE',  ( -1.568241469816272105, -0.08942795157527998196, 0.3641732283464567121 ) ) ;
#32711 = CARTESIAN_POINT ( 'NONE',  ( -1.345144356955379816, -0.05778040916215560624, -0.4822834645669293319 ) ) ;
#32712 = CARTESIAN_POINT ( 'NONE',  ( -0.4724409448818899238, 0.1265901696524986686, -0.6627296587926508886 ) ) ;
#32713 = CARTESIAN_POINT ( 'NONE',  ( -2.130163876374039589, 1.668131542012053048, 0.4562955581495582447 ) ) ;
#32714 = CARTESIAN_POINT ( 'NONE',  ( 4.797336870675656522E-17, -0.3917322834645670104, -0.2283464566929133410 ) ) ;
#32715 = CARTESIAN_POINT ( 'NONE',  ( 0.3917322834645669549, 0.1049643490035304660, -1.941601049868766582 ) ) ;
#32716 = CARTESIAN_POINT ( 'NONE',  ( 0.2165354330708668673, -0.5400638737290844871, 0.3530559997133364547 ) ) ;
#32717 = CARTESIAN_POINT ( 'NONE',  ( -1.299212598425196097, 0.1771653543307087630, 0.000000000000000000 ) ) ;
#32718 = CARTESIAN_POINT ( 'NONE',  ( -0.8661417322834640276, -0.1870078740157480879, -0.4822834645669291653 ) ) ;
#32719 = CARTESIAN_POINT ( 'NONE',  ( 0.4724409448818896462, 0.1265901696524990294, -2.563648293963254776 ) ) ;
#32721 = CARTESIAN_POINT ( 'NONE',  ( 0.4724409448818898682, 2.892866454678787531E-17, -1.139763779527559029 ) ) ;
#32720 = CARTESIAN_POINT ( 'NONE',  ( -1.443569553805773564, -0.6046776061558807314, 0.2411417322834647770 ) ) ;
#32722 = CARTESIAN_POINT ( 'NONE',  ( -0.9186351706036736120, 0.2306618581243848609, 0.2411417322834645549 ) ) ;
#32723 = CARTESIAN_POINT ( 'NONE',  ( -0.5314960629921254842, -0.5400638737290845981, -0.3530559997133363437 ) ) ;
#32724 = CARTESIAN_POINT ( 'NONE',  ( -0.1974969037888704149, -0.3420746716998661063, -2.662073490813648746 ) ) ;
#32725 = CARTESIAN_POINT ( 'NONE',  ( 1.069553805774278610, -0.5511811023622046335, 0.09757992244046803654 ) ) ;
#32726 = CARTESIAN_POINT ( 'NONE',  ( 4.797336870675656522E-17, -0.3917322834645670104, -0.1633858267716536417 ) ) ;
#32727 = AXIS2_PLACEMENT_3D ( 'NONE', #27782, #47128, #16004 ) ;
#32728 = CARTESIAN_POINT ( 'NONE',  ( 0.6364829396325465405, -0.2845877964562161244, -0.3641732283464567121 ) ) ;
#32729 = CARTESIAN_POINT ( 'NONE',  ( 1.404199475065617264, -0.3690944881889763329, 0.3153832671262228327 ) ) ;
#32730 = CARTESIAN_POINT ( 'NONE',  ( 1.450131233595801428, 0.2952755905511811885, 0.1292274648535926551 ) ) ;
#32731 = CARTESIAN_POINT ( 'NONE',  ( 0.2362204724409456558, -0.1870078740157479769, 0.3641732283464567677 ) ) ;
#32732 = CARTESIAN_POINT ( 'NONE',  ( -0.1958661417322836718, 0.3392501089628017219, -1.580052493438320216 ) ) ;
#32733 = CARTESIAN_POINT ( 'NONE',  ( -0.8792650918635160906, -0.4281496062992124485, 0.4176697321401328655 ) ) ;
#32734 = CARTESIAN_POINT ( 'NONE',  ( 1.174540682414699111, -0.05778040916215560624, -0.4822834645669293319 ) ) ;
#32735 = CARTESIAN_POINT ( 'NONE',  ( 0.2362204724409449064, 0.4091458600556404646, -0.06364829396325459576 ) ) ;
#32736 = CARTESIAN_POINT ( 'NONE',  ( -0.3543307086614165824, 0.1771653543307087630, 0.000000000000000000 ) ) ;
#32737 = CARTESIAN_POINT ( 'NONE',  ( -0.4724409448818908119, 0.1265901696524971698, -1.054461942257217899 ) ) ;
#32738 = CARTESIAN_POINT ( 'NONE',  ( 0.2099737532808405305, -0.6046776061558807314, 0.2411417322834647770 ) ) ;
#32739 = CARTESIAN_POINT ( 'NONE',  ( -1.018733685929528399, 1.601836984657050378, -0.4702924666327328307 ) ) ;
#32740 = CIRCLE ( 'NONE', #71742, 3.543307086614173151 ) ;
#32741 = CARTESIAN_POINT ( 'NONE',  ( 1.089238845144357537, -0.3690944881889763329, 0.3153832671262228327 ) ) ;
#32742 = CARTESIAN_POINT ( 'NONE',  ( -0.01968503937007793844, -0.4536011799217367080, 0.2665933059059888421 ) ) ;
#32743 = CARTESIAN_POINT ( 'NONE',  ( -0.2493438320209966919, -0.4281496062992124485, 0.4176697321401328655 ) ) ;
#32744 = CARTESIAN_POINT ( 'NONE',  ( -1.286089238845143479, -0.6046776061558807314, 0.2411417322834647770 ) ) ;
#32745 = CARTESIAN_POINT ( 'NONE',  ( -0.7545931758530176614, -0.5511811023622048555, -0.09757992244046775898 ) ) ;
#32746 = DIRECTION ( 'NONE',  ( 0.000000000000000000, -1.000000000000000000, 0.000000000000000000 ) ) ;
#32747 = CARTESIAN_POINT ( 'NONE',  ( 0.7086614173228353852, -0.1870078740157479769, 0.4822834645669291653 ) ) ;
#32748 = CARTESIAN_POINT ( 'NONE',  ( -0.9120734908136475250, -0.6692913385826773087, -0.1292274648535924053 ) ) ;
#32749 = CARTESIAN_POINT ( 'NONE',  ( -0.2925321140481930149, -0.2925321140481933480, -1.080708661417322691 ) ) ;
#32750 = CARTESIAN_POINT ( 'NONE',  ( -0.1049643490035307020, 0.3917322834645669549, -2.610892388451443225 ) ) ;
#32751 = CARTESIAN_POINT ( 'NONE',  ( 0.3018372703412079971, -0.3690944881889763329, 0.3153832671262228327 ) ) ;
#32752 = CARTESIAN_POINT ( 'NONE',  ( -0.5905511811023613777, -0.6692913385826771977, 8.415575281601705876E-17 ) ) ;
#32753 = CARTESIAN_POINT ( 'NONE',  ( -1.194225721784776262, -0.4281496062992124485, 0.4176697321401328655 ) ) ;
#32754 = CARTESIAN_POINT ( 'NONE',  ( -1.423884514435694859, -0.08942795157528024563, -0.3641732283464568787 ) ) ;
#32755 = LINE ( 'NONE', #27693, #81755 ) ;
#32756 = CARTESIAN_POINT ( 'NONE',  ( -0.8595800524934373854, -0.08942795157527998196, 0.3641732283464567121 ) ) ;
#32757 = CARTESIAN_POINT ( 'NONE',  ( -1.509186351706035767, -0.004921259842519870586, -0.3153832671262229437 ) ) ;
#32758 = CARTESIAN_POINT ( 'NONE',  ( 1.115485564304462551, 0.05413385826771666132, 0.4176697321401328100 ) ) ;
#32759 = CARTESIAN_POINT ( 'NONE',  ( -9.787531504996567848E-17, 0.3996062992125986035, 0.1574803149606299191 ) ) ;
#32760 = CARTESIAN_POINT ( 'NONE',  ( -0.2867679344610367109, 0.2867679344610365444, -2.536108554626983480 ) ) ;
#32761 = ORIENTED_EDGE ( 'NONE', *, *, #44453, .T. ) ;
#32762 = DIRECTION ( 'NONE',  ( 0.000000000000000000, -1.000000000000000000, 0.000000000000000000 ) ) ;
#32763 = CARTESIAN_POINT ( 'NONE',  ( 1.594488188976378673, 0.07958543189024085140, 0.2665933059059887866 ) ) ;
#32764 = CARTESIAN_POINT ( 'NONE',  ( -1.482939632545930975, -0.4281496062992127816, -0.4176697321401328100 ) ) ;
#32765 = CARTESIAN_POINT ( 'NONE',  ( 1.259842519685040019, -0.1870078740157479769, 0.4822834645669291653 ) ) ;
#32766 = CARTESIAN_POINT ( 'NONE',  ( 0.1049643490035304938, -0.3917322834645669549, -1.902230971128608727 ) ) ;
#32767 = DIRECTION ( 'NONE',  ( 1.445602896647338917E-16, 1.000000000000000000, 0.000000000000000000 ) ) ;
#32768 = CARTESIAN_POINT ( 'NONE',  ( 0.7217847769028878924, 0.05413385826771666132, 0.4176697321401328100 ) ) ;
#32769 = CARTESIAN_POINT ( 'NONE',  ( 0.01312335958005323398, -0.4281496062992127816, -0.4176697321401328100 ) ) ;
#32770 = CARTESIAN_POINT ( 'NONE',  ( -0.6971652711706680661, 5.991678263669262536E-15, 0.3791483426435162674 ) ) ;
#32771 = CARTESIAN_POINT ( 'NONE',  ( -0.6824146981627288167, 0.2306618581243848609, 0.2411417322834645549 ) ) ;
#32772 = CARTESIAN_POINT ( 'NONE',  ( 0.8202099737532813073, 0.1771653543307087630, 0.09757992244046791164 ) ) ;
#32773 = CARTESIAN_POINT ( 'NONE',  ( -0.1070741851644051862, -0.3996062992125987146, -1.332020997375328086 ) ) ;
#32774 = ORIENTED_EDGE ( 'NONE', *, *, #82598, .T. ) ;
#32775 = CARTESIAN_POINT ( 'NONE',  ( -0.1958661417322834220, -0.3392501089628018884, -2.892388451443569153 ) ) ;
#32776 = ORIENTED_EDGE ( 'NONE', *, *, #2252, .T. ) ;
#32777 = CARTESIAN_POINT ( 'NONE',  ( -0.2230971128608915943, -0.4281496062992127816, -0.4176697321401328100 ) ) ;
#32778 = CARTESIAN_POINT ( 'NONE',  ( 1.587926509186352142, 0.05413385826771666132, 0.4176697321401328100 ) ) ;
#32779 = CARTESIAN_POINT ( 'NONE',  ( 0.6036745406824154392, 0.2306618581243847221, -0.2411417322834647770 ) ) ;
#32780 = VECTOR ( 'NONE', #83209, 39.37007874015748143 ) ;
#32781 = CARTESIAN_POINT ( 'NONE',  ( 1.259842519685040019, -0.1870078740157480879, -0.4822834645669291653 ) ) ;
#32782 = CARTESIAN_POINT ( 'NONE',  ( 1.601049868766404982, 0.2306618581243848609, 0.2411417322834645549 ) ) ;
#32783 = CARTESIAN_POINT ( 'NONE',  ( -0.4593175853018364174, -0.4281496062992127816, -0.4176697321401328100 ) ) ;
#32784 = CARTESIAN_POINT ( 'NONE',  ( 0.1902887139107617975, 0.2952755905511811885, 0.1292274648535926551 ) ) ;
#32785 = CARTESIAN_POINT ( 'NONE',  ( -1.620734908136482577, 0.2952755905511811885, 0.1292274648535926551 ) ) ;
#32786 = CARTESIAN_POINT ( 'NONE',  ( 1.371391076115485719, -0.6692913385826773087, -0.1292274648535924053 ) ) ;
#32787 = CARTESIAN_POINT ( 'NONE',  ( 1.266404199475066328, -0.3162353388693409650, -0.4822834645669289433 ) ) ;
#32788 = CARTESIAN_POINT ( 'NONE',  ( -0.2230971128608915943, -0.4281496062992127816, -0.4176697321401328100 ) ) ;
#32789 = CARTESIAN_POINT ( 'NONE',  ( -0.1049643490035302024, -0.3917322834645671215, -0.3792650918635169233 ) ) ;
#32790 = CARTESIAN_POINT ( 'NONE',  ( 0.3608923884514443348, -0.5511811023622046335, 0.09757992244046803654 ) ) ;
#32791 = VERTEX_POINT ( 'NONE', #77646 ) ;
#32792 = CARTESIAN_POINT ( 'NONE',  ( 0.3949938075777409408, 0.1058382717557500574, -0.7545931758530185496 ) ) ;
#32793 = ORIENTED_EDGE ( 'NONE', *, *, #13910, .T. ) ;
#32794 = CARTESIAN_POINT ( 'NONE',  ( -0.2362204724409442680, -0.1870078740157480601, -0.3641732283464567677 ) ) ;
#32795 = CARTESIAN_POINT ( 'NONE',  ( 0.03937007874015833325, -0.6692913385826771977, 8.415575281601705876E-17 ) ) ;
#32796 = DIRECTION ( 'NONE',  ( 3.491481338843132961E-15, 0.000000000000000000, -1.000000000000000000 ) ) ;
#32797 = CARTESIAN_POINT ( 'NONE',  ( 0.03280839895013198948, 0.2952755905511811885, 0.1292274648535926551 ) ) ;
#32798 = CARTESIAN_POINT ( 'NONE',  ( -0.01968503937007793844, -0.5400638737290844871, 0.3530559997133364547 ) ) ;
#32799 = EDGE_CURVE ( 'NONE', #57471, #50964, #37851, .T. ) ;
#32800 = CARTESIAN_POINT ( 'NONE',  ( -1.089238845144356427, 0.05413385826771666132, 0.4176697321401328100 ) ) ;
#32801 = CIRCLE ( 'NONE', #7273, 1.929133858267716661 ) ;
#32802 = CARTESIAN_POINT ( 'NONE',  ( 1.469816272965879911, -0.5023911411419708095, 0.1820866141732285504 ) ) ;
#32803 = CARTESIAN_POINT ( 'NONE',  ( -1.482939632545930975, 0.05413385826771666132, 0.4176697321401328100 ) ) ;
#32804 = CARTESIAN_POINT ( 'NONE',  ( 0.3917322834645670104, -0.1049643490035303411, -2.873359580052493811 ) ) ;
#32805 = CARTESIAN_POINT ( 'NONE',  ( 0.7349081364829402885, -0.5023911411419708095, -0.1820866141732282451 ) ) ;
#32806 = CARTESIAN_POINT ( 'NONE',  ( 0.5839895013123367340, 0.2952755905511811885, 0.1292274648535926551 ) ) ;
#32807 = CARTESIAN_POINT ( 'NONE',  ( 0.7677165354330716118, 0.1660481256975883668, -0.3530559997133364547 ) ) ;
#32808 = CARTESIAN_POINT ( 'NONE',  ( 0.1998031496062994405, -0.3460692066303958092, -1.194225721784776928 ) ) ;
#32809 = CARTESIAN_POINT ( 'NONE',  ( -1.666666666666665853, 0.05413385826771626580, -0.4176697321401330321 ) ) ;
#32810 = CARTESIAN_POINT ( 'NONE',  ( -0.1070741851644051862, -0.3996062992125986590, -0.7788713910761155823 ) ) ;
#32811 = CARTESIAN_POINT ( 'NONE',  ( -0.3996062992125986590, 0.1070741851644051723, -0.1095800524934383291 ) ) ;
#32812 = CARTESIAN_POINT ( 'NONE',  ( 0.05249343832021075018, 0.2306618581243847221, -0.2411417322834647770 ) ) ;
#32813 = CARTESIAN_POINT ( 'NONE',  ( -0.3996062992125986035, -7.340648628747425578E-17, -2.716535433070865757 ) ) ;
#32814 = CARTESIAN_POINT ( 'NONE',  ( -0.1049643490035302024, -0.3917322834645671215, -2.046587926509185973 ) ) ;
#32815 = CARTESIAN_POINT ( 'NONE',  ( -1.082677165354329896, -0.4536011799217368745, -0.2665933059059886201 ) ) ;
#32816 = CARTESIAN_POINT ( 'NONE',  ( 1.443569553805774897, 0.2306618581243848609, 0.2411417322834645549 ) ) ;
#32817 = CARTESIAN_POINT ( 'NONE',  ( 1.220472440944882608, 0.2952755905511811885, 0.000000000000000000 ) ) ;
#32818 = CARTESIAN_POINT ( 'NONE',  ( -0.4133858267716528645, -0.4536011799217367080, 0.2665933059059888421 ) ) ;
#32819 = CARTESIAN_POINT ( 'NONE',  ( 0.3215223097112867578, -0.05778040916215522460, 0.4822834645669289988 ) ) ;
#32820 = CARTESIAN_POINT ( 'NONE',  ( 0.4091458600556404646, -0.2362204724409448231, -1.599081364829396223 ) ) ;
#32821 = CARTESIAN_POINT ( 'NONE',  ( 0.2755905511811031494, 0.1771653543307087630, 0.000000000000000000 ) ) ;
#32822 = CARTESIAN_POINT ( 'NONE',  ( -0.03280839895013062252, -0.6692913385826771977, 0.1292274648535927661 ) ) ;
#32823 = CARTESIAN_POINT ( 'NONE',  ( -0.1058382717557503072, 0.3949938075777408852, -1.500656167979002253 ) ) ;
#32824 = CARTESIAN_POINT ( 'NONE',  ( -1.227034120734907585, 0.2952755905511811885, 0.1292274648535926551 ) ) ;
#32825 = CARTESIAN_POINT ( 'NONE',  ( 0.3740157480314966754, 0.07958543189024071263, -0.2665933059059888421 ) ) ;
#32826 = CARTESIAN_POINT ( 'NONE',  ( 0.3809280630633196107, 0.004960608223778500969, -0.3437734562760191848 ) ) ;
#32827 = CARTESIAN_POINT ( 'NONE',  ( -0.6758530183727028406, -0.6692913385826773087, -0.1292274648535924053 ) ) ;
#32828 = CARTESIAN_POINT ( 'NONE',  ( -0.2690288713910754526, -0.5511811023622046335, 0.09757992244046803654 ) ) ;
#32829 = CARTESIAN_POINT ( 'NONE',  ( -2.554262525012343854, 1.528780496884629025, -0.4744094488188976277 ) ) ;
#32830 = CARTESIAN_POINT ( 'NONE',  ( -0.8070866141732276899, -0.5400638737290844871, 0.3530559997133364547 ) ) ;
#32831 = CARTESIAN_POINT ( 'NONE',  ( -0.09842519685039295696, -0.5400638737290844871, 0.3530559997133364547 ) ) ;
#32832 = CARTESIAN_POINT ( 'NONE',  ( 0.3937007874015754361, -0.1870078740157480601, -0.3641732283464567677 ) ) ;
#32833 = CARTESIAN_POINT ( 'NONE',  ( -0.1998031496062991630, -0.3460692066303959202, -2.032152230971128848 ) ) ;
#32834 = CARTESIAN_POINT ( 'NONE',  ( -0.08530183727034056085, -0.3162353388693405765, 0.4822834645669290543 ) ) ;
#32835 = CARTESIAN_POINT ( 'NONE',  ( 0.1958661417322836162, -0.3392501089628018329, -1.904180159283777485 ) ) ;
#32836 = LINE ( 'NONE', #71562, #22053 ) ;
#32837 = CARTESIAN_POINT ( 'NONE',  ( 0.6627296587926517768, -0.5511811023622048555, -0.09757992244046775898 ) ) ;
#32838 = CARTESIAN_POINT ( 'NONE',  ( 1.489501312335958172, -0.05778040916215560624, -0.4822834645669293319 ) ) ;
#32839 = CARTESIAN_POINT ( 'NONE',  ( -1.010498687664041384, -0.3690944881889765550, -0.3153832671262227771 ) ) ;
#32840 = CARTESIAN_POINT ( 'NONE',  ( -1.227034120734907585, 0.1771653543307087630, 0.09757992244046791164 ) ) ;
#32841 = CARTESIAN_POINT ( 'NONE',  ( -0.5643044619422565855, -0.4281496062992124485, 0.4176697321401328655 ) ) ;
#32842 = CARTESIAN_POINT ( 'NONE',  ( 0.03937007874015806264, 0.2952755905511811885, 0.000000000000000000 ) ) ;
#32843 = CARTESIAN_POINT ( 'NONE',  ( 0.5577427821522316087, -0.08942795157527998196, 0.3641732283464567121 ) ) ;
#32844 = CARTESIAN_POINT ( 'NONE',  ( -0.2710150415003134139, 0.1175404812240907898, 5.835005246025586345 ) ) ;
#32845 = CARTESIAN_POINT ( 'NONE',  ( 0.9776902887139113929, 0.1771653543307087630, 0.09757992244046791164 ) ) ;
#32846 = CARTESIAN_POINT ( 'NONE',  ( 0.4527559055118117182, 0.1660481256975883668, -0.3530559997133364547 ) ) ;
#32847 = CARTESIAN_POINT ( 'NONE',  ( -0.3996062992125984925, -0.1070741851644056858, 0.03477690288713909672 ) ) ;
#32848 = CARTESIAN_POINT ( 'NONE',  ( -0.3740157480314953431, -0.5400638737290845981, -0.3530559997133363437 ) ) ;
#32849 = CARTESIAN_POINT ( 'NONE',  ( 0.1958661417322834775, 0.3392501089628018884, -1.488845144356955252 ) ) ;
#32850 = CARTESIAN_POINT ( 'NONE',  ( 1.541994750656168645, -0.5511811023622046335, 0.09757992244046803654 ) ) ;
#32851 = CARTESIAN_POINT ( 'NONE',  ( 0.6758530183727039509, -0.6692913385826771977, 0.1292274648535927661 ) ) ;
#32852 = CARTESIAN_POINT ( 'NONE',  ( 0.1771653543307093182, -0.5400638737290845981, -0.3530559997133363437 ) ) ;
#32853 = CARTESIAN_POINT ( 'NONE',  ( 1.112701331685804984, -9.595573933774993207E-16, 0.4281989832122458095 ) ) ;
#32854 = CARTESIAN_POINT ( 'NONE',  ( -0.1181102362204717315, -0.5511811023622047445, 6.969142054262312111E-17 ) ) ;
#32855 = CARTESIAN_POINT ( 'NONE',  ( 0.7545931758530189937, 0.2952755905511810774, -0.1292274648535930714 ) ) ;
#32856 = CARTESIAN_POINT ( 'NONE',  ( -0.4724409448818890911, -0.1870078740157479769, 0.3641732283464567677 ) ) ;
#32857 = AXIS2_PLACEMENT_3D ( 'NONE', #53071, #77097, #7656 ) ;
#32858 = CARTESIAN_POINT ( 'NONE',  ( -0.5183727034120726440, 0.2952755905511811885, 0.1292274648535926551 ) ) ;
#32859 = CARTESIAN_POINT ( 'NONE',  ( 1.204164820379010070, 1.535433070866141447, 0.4915354330708652242 ) ) ;
#32860 = CARTESIAN_POINT ( 'NONE',  ( -0.3215223097112853146, -0.3162353388693405765, 0.4822834645669290543 ) ) ;
#32861 = VERTEX_POINT ( 'NONE', #57838 ) ;
#32862 = CARTESIAN_POINT ( 'NONE',  ( -1.174540682414697335, -0.05778040916215522460, 0.4822834645669289988 ) ) ;
#32863 = CARTESIAN_POINT ( 'NONE',  ( -0.8727034120734901146, -0.08942795157528024563, -0.3641732283464568787 ) ) ;
#32864 = CARTESIAN_POINT ( 'NONE',  ( -0.006561679790025524116, -0.3162353388693405765, 0.4822834645669290543 ) ) ;
#32865 = CARTESIAN_POINT ( 'NONE',  ( -1.450131233595799651, -0.6692913385826771977, 0.1292274648535927661 ) ) ;
#32866 = CARTESIAN_POINT ( 'NONE',  ( -0.6758530183727028406, 0.2952755905511811885, 0.1292274648535926551 ) ) ;
#32867 = CARTESIAN_POINT ( 'NONE',  ( -1.895394334970792016, 2.755905511811024056, 0.5314960629921260393 ) ) ;
#32869 = CARTESIAN_POINT ( 'NONE',  ( 1.240157480314961314, -0.5400638737290844871, 0.3530559997133364547 ) ) ;
#32868 = CARTESIAN_POINT ( 'NONE',  ( -0.9348729704079935532, -2.191421614605370878E-15, 0.4445507791589071167 ) ) ;
#32870 = CARTESIAN_POINT ( 'NONE',  ( 1.115485564304462551, -0.4281496062992127816, -0.4176697321401328100 ) ) ;
#32871 = CARTESIAN_POINT ( 'NONE',  ( 0.2867679344610366554, 0.2867679344610366554, -2.649606299212598604 ) ) ;
#32872 = LINE ( 'NONE', #51794, #14003 ) ;
#32873 = CARTESIAN_POINT ( 'NONE',  ( -1.423884514435694859, -0.3162353388693405765, 0.4822834645669290543 ) ) ;
#32874 = CARTESIAN_POINT ( 'NONE',  ( -0.4091458600556402980, -0.2362204724409451284, -0.6824146981627295938 ) ) ;
#32875 = CARTESIAN_POINT ( 'NONE',  ( 4.893765752498283924E-17, -0.3996062992125986035, -0.07874015748031498729 ) ) ;
#32876 = ORIENTED_EDGE ( 'NONE', *, *, #42409, .F. ) ;
#32877 = CARTESIAN_POINT ( 'NONE',  ( -0.2230971128608915943, -0.004921259842519576551, 0.3153832671262227771 ) ) ;
#32878 = CARTESIAN_POINT ( 'NONE',  ( 0.2867679344610365999, -0.2867679344610365444, -1.980314960629921073 ) ) ;
#32879 = EDGE_LOOP ( 'NONE', ( #29562, #57097, #2280, #37741, #33457, #71924, #60757, #11681, #60029, #50591, #73924, #53904, #503, #46141 ) ) ;
#32880 = CARTESIAN_POINT ( 'NONE',  ( 0.2165354330708668673, 0.1660481256975883668, -0.3530559997133364547 ) ) ;
#32881 = CARTESIAN_POINT ( 'NONE',  ( 0.3937007874015754361, -0.1870078740157480879, -0.4822834645669291653 ) ) ;
#32882 = CARTESIAN_POINT ( 'NONE',  ( -0.006307039255731988932, 0.3948371832379762858, -2.755905511811026720 ) ) ;
#32883 = PLANE ( 'NONE',  #23817 ) ;
#32884 = CARTESIAN_POINT ( 'NONE',  ( -0.8464566929133852113, 0.07958543189024085140, 0.2665933059059887866 ) ) ;
#32885 = CARTESIAN_POINT ( 'NONE',  ( -0.2142011206082509722, -0.2032823926810629067, 0.1316721176867485243 ) ) ;
#32886 = CARTESIAN_POINT ( 'NONE',  ( 0.7742782152230979209, 0.05413385826771626580, -0.4176697321401330321 ) ) ;
#32887 = CARTESIAN_POINT ( 'NONE',  ( 0.8661417322834652488, -0.1870078740157480601, -0.3641732283464567677 ) ) ;
#32888 = CARTESIAN_POINT ( 'NONE',  ( -0.3215223097112853146, -0.05778040916215560624, -0.4822834645669293319 ) ) ;
#32889 = CARTESIAN_POINT ( 'NONE',  ( -0.1049643490035301746, -0.3917322834645670659, -0.9396132301499194872 ) ) ;
#32890 = CARTESIAN_POINT ( 'NONE',  ( -0.7874015748031489847, -0.1870078740157480879, -0.4822834645669291653 ) ) ;
#32891 = CARTESIAN_POINT ( 'NONE',  ( -1.692913385826770645, 0.1771653543307087630, 0.000000000000000000 ) ) ;
#32892 = EDGE_CURVE ( 'NONE', #5361, #4140, #52432, .T. ) ;
#32893 = CARTESIAN_POINT ( 'NONE',  ( -0.8727034120734901146, -0.05778040916215560624, -0.4822834645669293319 ) ) ;
#32894 = CARTESIAN_POINT ( 'NONE',  ( 1.213910761154856299, 0.2952755905511811885, 0.1292274648535926551 ) ) ;
#32895 = FACE_OUTER_BOUND ( 'NONE', #54214, .T. ) ;
#32896 = EDGE_LOOP ( 'NONE', ( #34570, #6178, #73289, #7016 ) ) ;
#32897 = CARTESIAN_POINT ( 'NONE',  ( -0.1958661417322833942, -0.3392501089628018884, -2.582040313157166977 ) ) ;
#32898 = CARTESIAN_POINT ( 'NONE',  ( -0.1181102362204717315, -0.6692913385826771977, 8.415575281601705876E-17 ) ) ;
#32899 = VERTEX_POINT ( 'NONE', #33443 ) ;
#32900 = CARTESIAN_POINT ( 'NONE',  ( -0.8202099737532801971, -0.6692913385826771977, 0.1292274648535927661 ) ) ;
#32901 = CARTESIAN_POINT ( 'NONE',  ( 1.246719160104987623, -0.4281496062992124485, 0.4176697321401328655 ) ) ;
#32902 = CARTESIAN_POINT ( 'NONE',  ( 1.089238845144357537, -0.4281496062992124485, 0.4176697321401328655 ) ) ;
#32903 = CARTESIAN_POINT ( 'NONE',  ( 0.4527559055118117182, -0.5400638737290844871, 0.3530559997133364547 ) ) ;
#32904 = EDGE_CURVE ( 'NONE', #62516, #25432, #16239, .T. ) ;
#32905 = CARTESIAN_POINT ( 'NONE',  ( -0.3477690288713902178, 0.2952755905511810774, -0.1292274648535930714 ) ) ;
#32906 = CARTESIAN_POINT ( 'NONE',  ( 0.1049643490035303689, 0.3917322834645670104, -1.652887139107611425 ) ) ;
#32907 = CARTESIAN_POINT ( 'NONE',  ( -1.286089238845143479, -0.6046776061558807314, 0.2411417322834647770 ) ) ;
#32908 = CARTESIAN_POINT ( 'NONE',  ( -0.07874015748031421014, -0.1870078740157479769, 0.4822834645669291653 ) ) ;
#32909 = AXIS2_PLACEMENT_3D ( 'NONE', #14525, #14104, #40177 ) ;
#32910 = CARTESIAN_POINT ( 'NONE',  ( -0.1837270341207340729, 0.1283753931104746893, -0.1820866141732285504 ) ) ;
#32911 = CARTESIAN_POINT ( 'NONE',  ( 1.574803149606299746, -0.1870078740157480879, -0.4822834645669291653 ) ) ;
#32912 = CARTESIAN_POINT ( 'NONE',  ( 1.371391076115485941, 0.2952755905511811885, 0.1292274648535926551 ) ) ;
#32913 = CARTESIAN_POINT ( 'NONE',  ( -0.4002624671916004129, -0.05778040916215560624, -0.4822834645669293319 ) ) ;
#32914 = CARTESIAN_POINT ( 'NONE',  ( -0.5314960629921393620, 2.755400581649068315, 3.831845081856512181 ) ) ;
#32915 = CARTESIAN_POINT ( 'NONE',  ( 1.325459317585302665, 0.05413385826771626580, -0.4176697321401330321 ) ) ;
#32916 = CARTESIAN_POINT ( 'NONE',  ( 0.4986876640419954376, 0.1539470093639523085, 0.1968503937007873850 ) ) ;
#32917 = VERTEX_POINT ( 'NONE', #52357 ) ;
#32918 = CARTESIAN_POINT ( 'NONE',  ( 0.3412073490813655186, -0.6046776061558809534, -0.2411417322834644161 ) ) ;
#32919 = CARTESIAN_POINT ( 'NONE',  ( -0.4461942257217840213, 0.1283753931104748280, 0.1820866141732283561 ) ) ;
#32921 = CARTESIAN_POINT ( 'NONE',  ( -1.614173228346456712, 0.4410134679336886188, -0.1372047244094478091 ) ) ;
#32920 = CARTESIAN_POINT ( 'NONE',  ( 1.555118110236221041, 0.07958543189024071263, -0.2665933059059888421 ) ) ;
#32922 = CARTESIAN_POINT ( 'NONE',  ( -0.3458507752293909498, 0.3458507752293907833, -0.09645669291338582196 ) ) ;
#32923 = CARTESIAN_POINT ( 'NONE',  ( 1.568241469816273659, -0.08942795157528024563, -0.3641732283464568787 ) ) ;
#32924 = CARTESIAN_POINT ( 'NONE',  ( 1.259842519685040019, -0.1870078740157479769, 0.4822834645669291653 ) ) ;
#32925 = AXIS2_PLACEMENT_3D ( 'NONE', #41412, #46878, #21635 ) ;
#32926 = CARTESIAN_POINT ( 'NONE',  ( -0.2891555358219909388, -0.2891555358219912164, 0.02165354330708659999 ) ) ;
#32927 = CARTESIAN_POINT ( 'NONE',  ( -0.1115485564304456306, 0.2952755905511810774, -0.1292274648535930714 ) ) ;
#32928 = CARTESIAN_POINT ( 'NONE',  ( -1.633858267716534529, 0.1660481256975885056, 0.3530559997133364547 ) ) ;
#32929 = CARTESIAN_POINT ( 'NONE',  ( -1.732283464566928277, -0.1870078740157479769, 0.4822834645669291653 ) ) ;
#32930 = CARTESIAN_POINT ( 'NONE',  ( -0.3412073490813641308, -0.6046776061558807314, 0.2411417322834647770 ) ) ;
#32931 = CARTESIAN_POINT ( 'NONE',  ( -0.2891555358219911054, 0.2891555358219909388, 0.06102362204724409017 ) ) ;
#32932 = CARTESIAN_POINT ( 'NONE',  ( 1.620734908136483465, -0.6692913385826771977, 0.1292274648535927661 ) ) ;
#32933 = CARTESIAN_POINT ( 'NONE',  ( 0.6758530183727039509, 0.2952755905511810774, -0.1292274648535930714 ) ) ;
#32934 = CARTESIAN_POINT ( 'NONE',  ( 1.043307086614173818, 0.07958543189024085140, 0.2665933059059887866 ) ) ;
#32935 = DIRECTION ( 'NONE',  ( 0.000000000000000000, 1.000000000000000000, -0.000000000000000000 ) ) ;
#32936 = CARTESIAN_POINT ( 'NONE',  ( 0.8136482939632553313, -0.5023911411419708095, -0.1820866141732282451 ) ) ;
#32937 = CARTESIAN_POINT ( 'NONE',  ( -1.358267716535432434, -0.5400638737290844871, 0.3530559997133364547 ) ) ;
#32938 = CARTESIAN_POINT ( 'NONE',  ( -0.3460692066303960313, 0.1998031496062989965, -0.7329396325459317518 ) ) ;
#32939 = CARTESIAN_POINT ( 'NONE',  ( 1.141732283464567788, -0.6692913385826771977, 8.415575281601705876E-17 ) ) ;
#32940 = CARTESIAN_POINT ( 'NONE',  ( 4.797336870675656522E-17, -0.3917322834645670104, -0.7007874015748030150 ) ) ;
#32942 = CARTESIAN_POINT ( 'NONE',  ( -0.4091458600556402980, -0.2362204724409451284, -0.4442257217847768724 ) ) ;
#32941 = CARTESIAN_POINT ( 'NONE',  ( 0.6561679790026253567, -0.6046776061558809534, -0.2411417322834644161 ) ) ;
#32943 = DIRECTION ( 'NONE',  ( -3.096699300667737957E-16, 1.000000000000000000, -0.000000000000000000 ) ) ;
#32944 = CARTESIAN_POINT ( 'NONE',  ( 0.2362204724409456558, -0.1870078740157480601, -0.3641732283464567677 ) ) ;
#32945 = CARTESIAN_POINT ( 'NONE',  ( 0.4921259842519691285, -0.5400638737290845981, -0.3530559997133363437 ) ) ;
#32946 = CARTESIAN_POINT ( 'NONE',  ( 1.686351706036745890, 0.1771653543307087630, 0.09757992244046791164 ) ) ;
#32947 = CARTESIAN_POINT ( 'NONE',  ( -0.9776902887139098386, -0.5511811023622046335, 0.09757992244046803654 ) ) ;
#32948 = CARTESIAN_POINT ( 'NONE',  ( -0.8202099737532801971, -0.6692913385826771977, 0.1292274648535927661 ) ) ;
#32949 = CARTESIAN_POINT ( 'NONE',  ( -1.627296587926508442, -0.6046776061558809534, -0.2411417322834644161 ) ) ;
#32950 = CARTESIAN_POINT ( 'NONE',  ( 1.082677165354331228, 0.1660481256975883668, -0.3530559997133364547 ) ) ;
#32951 = CARTESIAN_POINT ( 'NONE',  ( 1.646981627296588035, -0.3162353388693405765, 0.4822834645669290543 ) ) ;
#32952 = CARTESIAN_POINT ( 'NONE',  ( 1.084078074602846664, 1.161389122953379260, -0.2896872109502376391 ) ) ;
#32953 = CARTESIAN_POINT ( 'NONE',  ( 0.9120734908136489683, -0.6692913385826771977, 0.1292274648535927661 ) ) ;
#32954 = CARTESIAN_POINT ( 'NONE',  ( -0.1265901696524986964, -0.4724409448818899238, -2.668635170603674833 ) ) ;
#32955 = CARTESIAN_POINT ( 'NONE',  ( 0.1527192119523664293, 1.087977008489718012, 3.934072827720677790 ) ) ;
#32956 = CARTESIAN_POINT ( 'NONE',  ( 1.568241469816273659, -0.05778040916215560624, -0.4822834645669293319 ) ) ;
#32957 = CARTESIAN_POINT ( 'NONE',  ( -1.633858267716534529, -0.4536011799217368745, -0.2665933059059886201 ) ) ;
#32958 = CARTESIAN_POINT ( 'NONE',  ( 1.069553805774278832, 0.1771653543307087075, -0.09757992244046823083 ) ) ;
#32959 = CARTESIAN_POINT ( 'NONE',  ( -1.443569553805773564, 0.1283753931104746893, -0.1820866141732285504 ) ) ;
#32960 = CARTESIAN_POINT ( 'NONE',  ( -0.5774278215223089816, -0.5023911411419708095, 0.1820866141732285504 ) ) ;
#32961 = CARTESIAN_POINT ( 'NONE',  ( -1.594488188976377563, -0.4536011799217367080, 0.2665933059059888421 ) ) ;
#32962 = CARTESIAN_POINT ( 'NONE',  ( 1.003937007874016185, 0.07958543189024071263, -0.2665933059059888421 ) ) ;
#32963 = CARTESIAN_POINT ( 'NONE',  ( 0.5446194225721792126, -0.3162353388693405765, 0.4822834645669290543 ) ) ;
#32964 = CARTESIAN_POINT ( 'NONE',  ( 1.003937007874016185, 0.1660481256975883668, -0.3530559997133364547 ) ) ;
#32965 = CARTESIAN_POINT ( 'NONE',  ( 0.09842519685039434474, 0.1660481256975885056, 0.3530559997133364547 ) ) ;
#32966 = CARTESIAN_POINT ( 'NONE',  ( 0.7480314960629927956, -0.5511811023622047445, 6.969142054262312111E-17 ) ) ;
#32967 = CARTESIAN_POINT ( 'NONE',  ( 1.614173228346457378, 0.2952755905511811885, 0.000000000000000000 ) ) ;
#32968 = CARTESIAN_POINT ( 'NONE',  ( 1.141392835773559211, 1.299212598425196985, 1.141392835773562764 ) ) ;
#32969 = CARTESIAN_POINT ( 'NONE',  ( -0.6824146981627291497, -0.6046776061558809534, -0.2411417322834644161 ) ) ;
#32970 = CARTESIAN_POINT ( 'NONE',  ( -0.2925321140481932369, 0.2925321140481931814, -0.3346456692913385433 ) ) ;
#32971 = CARTESIAN_POINT ( 'NONE',  ( -0.3129921259842520787, 1.496062992125984259, 2.300774849103979725E-17 ) ) ;
#32972 = CARTESIAN_POINT ( 'NONE',  ( 0.07874015748031558404, -0.1870078740157480879, -0.4822834645669291653 ) ) ;
#32974 = VECTOR ( 'NONE', #21571, 39.37007874015748143 ) ;
#32973 = CARTESIAN_POINT ( 'NONE',  ( -0.3805774278215216522, 0.05413385826771666132, 0.4176697321401328100 ) ) ;
#32975 = CARTESIAN_POINT ( 'NONE',  ( -0.1837270341207343505, -0.6046776061558807314, 0.2411417322834647770 ) ) ;
#32976 = CARTESIAN_POINT ( 'NONE',  ( 0.3460692066303959202, 0.1998031496062993295, -2.650918635170603554 ) ) ;
#32977 = CARTESIAN_POINT ( 'NONE',  ( -0.1058382717557503211, 0.3949938075777409408, -2.053805774278215868 ) ) ;
#32978 = CARTESIAN_POINT ( 'NONE',  ( 0.1958661417322834775, 0.3392501089628018884, -0.4514435695538057125 ) ) ;
#32979 = CARTESIAN_POINT ( 'NONE',  ( 0.2917607380149856433, -0.04688787658492848953, 5.873221924710890107 ) ) ;
#32980 = CARTESIAN_POINT ( 'NONE',  ( -0.3392501089628017219, -0.1958661417322836718, -0.9895013123359579499 ) ) ;
#32981 = CARTESIAN_POINT ( 'NONE',  ( -1.049868766404198794, 0.1283753931104746893, -0.1820866141732285504 ) ) ;
#32982 = CARTESIAN_POINT ( 'NONE',  ( 0.1049643490035304938, -0.3917322834645669549, -1.179790026246718915 ) ) ;
#32983 = CARTESIAN_POINT ( 'NONE',  ( -1.240157480314959759, 0.1660481256975885056, 0.3530559997133364547 ) ) ;
#32984 = CARTESIAN_POINT ( 'NONE',  ( 0.3949938075777409408, -0.1058382717557499186, -2.865485564304462329 ) ) ;
#32985 = CARTESIAN_POINT ( 'NONE',  ( 0.5446194225721792126, -0.3162353388693405765, 0.4822834645669290543 ) ) ;
#32986 = CARTESIAN_POINT ( 'NONE',  ( -0.07874015748031421014, -0.1870078740157480601, -0.3641732283464567677 ) ) ;
#32987 = CARTESIAN_POINT ( 'NONE',  ( 1.259842519685040019, -0.1870078740157479769, 0.4822834645669291653 ) ) ;
#32988 = CARTESIAN_POINT ( 'NONE',  ( 0.4199475065616803948, -0.6046776061558809534, -0.2411417322834644161 ) ) ;
#32989 = CARTESIAN_POINT ( 'NONE',  ( -0.4470386624395519815, 1.696927142811738287, -2.112798853176812042 ) ) ;
#32990 = CARTESIAN_POINT ( 'NONE',  ( -0.3996062992125987146, 0.1070741851644051862, -2.709973753280840114 ) ) ;
#32991 = CARTESIAN_POINT ( 'NONE',  ( -0.1049643490035302301, -0.3917322834645671770, -1.171279158301524292 ) ) ;
#32992 = CARTESIAN_POINT ( 'NONE',  ( 1.076115485564305141, 0.2306618581243847221, -0.2411417322834647770 ) ) ;
#32993 = CARTESIAN_POINT ( 'NONE',  ( 0.3018372703412079971, -0.4281496062992124485, 0.4176697321401328655 ) ) ;
#32994 = CARTESIAN_POINT ( 'NONE',  ( 0.3412073490813655186, 0.2306618581243848609, 0.2411417322834645549 ) ) ;
#32995 = CARTESIAN_POINT ( 'NONE',  ( 1.417322834645670104, -0.1870078740157480879, -0.4822834645669291653 ) ) ;
#32996 = CARTESIAN_POINT ( 'NONE',  ( -0.3392501089628017219, -0.1958661417322836718, -0.4520997375328084655 ) ) ;
#32997 = CARTESIAN_POINT ( 'NONE',  ( -0.09842519685039295696, 0.1660481256975883668, -0.3530559997133364547 ) ) ;
#32998 = CARTESIAN_POINT ( 'NONE',  ( 1.141732283464567788, -0.6692913385826771977, 8.415575281601705876E-17 ) ) ;
#32999 = CARTESIAN_POINT ( 'NONE',  ( 0.4921259842519691285, -0.5400638737290845981, -0.3530559997133363437 ) ) ;
#33000 = CARTESIAN_POINT ( 'NONE',  ( 1.122047244094488860, -0.4536011799217368745, -0.2665933059059886201 ) ) ;
#33001 = CARTESIAN_POINT ( 'NONE',  ( -1.089238845144356427, 0.05413385826771666132, 0.4176697321401328100 ) ) ;
#33002 = CARTESIAN_POINT ( 'NONE',  ( -1.528871391076114250, 0.2952755905511810774, -0.1292274648535930714 ) ) ;
#33003 = CARTESIAN_POINT ( 'NONE',  ( 0.7349081364829402885, -0.6046776061558809534, -0.2411417322834644161 ) ) ;
#33004 = CARTESIAN_POINT ( 'NONE',  ( 0.2316922116746869542, -0.3165741174733261998, -1.929133858267716439 ) ) ;
#33005 = CARTESIAN_POINT ( 'NONE',  ( -0.2867679344610365999, 0.2867679344610364889, -1.744094488188976610 ) ) ;
#33006 = ORIENTED_EDGE ( 'NONE', *, *, #50269, .T. ) ;
#33007 = CARTESIAN_POINT ( 'NONE',  ( 0.1070741851644054915, -0.3996062992125986035, 0.07217847769028869209 ) ) ;
#33008 = EDGE_LOOP ( 'NONE', ( #63631, #79786 ) ) ;
#33009 = CARTESIAN_POINT ( 'NONE',  ( 1.351706036745407680, 0.05413385826771666132, 0.4176697321401328100 ) ) ;
#33010 = CARTESIAN_POINT ( 'NONE',  ( 1.043307086614173818, -0.4536011799217368745, -0.2665933059059886201 ) ) ;
#33011 = CARTESIAN_POINT ( 'NONE',  ( -0.4724409448818898682, -8.678599364036362592E-17, -1.929133858267716439 ) ) ;
#33012 = CARTESIAN_POINT ( 'NONE',  ( 1.530808498934191571E-16, 0.000000000000000000, 1.250000000000000000 ) ) ;
#33013 = CARTESIAN_POINT ( 'NONE',  ( 0.000000000000000000, -0.09842519685039369248, 5.158493410915829266E-18 ) ) ;
#33014 = CARTESIAN_POINT ( 'NONE',  ( -0.1958661417322834220, -0.3392501089628018884, -0.9376640419947508409 ) ) ;
#33015 = CARTESIAN_POINT ( 'NONE',  ( -1.253280839895012377, -0.2845877964562161244, -0.3641732283464567121 ) ) ;
#33016 = CARTESIAN_POINT ( 'NONE',  ( -1.653543307086613234, -0.1870078740157480601, -0.3641732283464567677 ) ) ;
#33017 = CARTESIAN_POINT ( 'NONE',  ( -0.3996062992125986035, -1.273259842764937629E-12, -1.929133858267794599 ) ) ;
#33018 = CARTESIAN_POINT ( 'NONE',  ( -0.2296587926509179312, -0.3162353388693409650, -0.4822834645669289433 ) ) ;
#33019 = CARTESIAN_POINT ( 'NONE',  ( 1.292650918635171564, 0.2952755905511811885, 0.1292274648535926551 ) ) ;
#33020 = ORIENTED_EDGE ( 'NONE', *, *, #51302, .F. ) ;
#33021 = EDGE_CURVE ( 'NONE', #12829, #59707, #8125, .T. ) ;
#33022 = CARTESIAN_POINT ( 'NONE',  ( -1.482939632545930975, -0.4281496062992127816, -0.4176697321401328100 ) ) ;
#33023 = CARTESIAN_POINT ( 'NONE',  ( -0.7201575634749992627, -5.642773921931522838E-15, -0.3791483426435192094 ) ) ;
#33024 = DIRECTION ( 'NONE',  ( -1.000000000000000000, -6.123233995736767268E-17, -6.982962677686266711E-15 ) ) ;
#33025 = CARTESIAN_POINT ( 'NONE',  ( 0.3458507752293908943, 0.3458507752293908943, -2.657480314960630086 ) ) ;
#33026 = FACE_OUTER_BOUND ( 'NONE', #64, .T. ) ;
#33027 = CARTESIAN_POINT ( 'NONE',  ( -0.8070866141732276899, 0.07958543189024071263, -0.2665933059059888421 ) ) ;
#33028 = CARTESIAN_POINT ( 'NONE',  ( -1.377952755905511140, -0.6692913385826771977, 8.415575281601705876E-17 ) ) ;
#33029 = CARTESIAN_POINT ( 'NONE',  ( 0.6167979002624679463, 0.05413385826771626580, -0.4176697321401330321 ) ) ;
#33030 = AXIS2_PLACEMENT_3D ( 'NONE', #13259, #12418, #25439 ) ;
#33031 = ORIENTED_EDGE ( 'NONE', *, *, #60488, .F. ) ;
#33033 = FACE_OUTER_BOUND ( 'NONE', #13035, .T. ) ;
#33032 = CARTESIAN_POINT ( 'NONE',  ( 0.000000000000000000, 2.559055118110236560, 0.000000000000000000 ) ) ;
#33034 = CARTESIAN_POINT ( 'NONE',  ( 1.364829396325460076, 0.2306618581243848609, 0.2411417322834645549 ) ) ;
#33035 = CARTESIAN_POINT ( 'NONE',  ( 1.528871391076116026, -0.5511811023622048555, -0.09757992244046775898 ) ) ;
#33036 = CARTESIAN_POINT ( 'NONE',  ( -0.3917322834645669549, -7.196005306013483243E-17, -0.9068048311997882749 ) ) ;
#33037 = CARTESIAN_POINT ( 'NONE',  ( -0.4068241469816267775, -0.004921259842519870586, -0.3153832671262229437 ) ) ;
#33038 = CARTESIAN_POINT ( 'NONE',  ( -1.358267716535432434, -0.4536011799217367080, 0.2665933059059888421 ) ) ;
#33039 = CARTESIAN_POINT ( 'NONE',  ( 0.2867679344610366554, 0.2867679344610366554, -1.167322834645669438 ) ) ;
#33040 = CARTESIAN_POINT ( 'NONE',  ( 0.4724409448818904789, -0.1870078740157479769, 0.4822834645669291653 ) ) ;
#33041 = CARTESIAN_POINT ( 'NONE',  ( -0.9580052493438311334, -0.004921259842519870586, -0.3153832671262229437 ) ) ;
#33042 = CARTESIAN_POINT ( 'NONE',  ( 0.2493438320209980519, -0.3690944881889765550, -0.3153832671262227771 ) ) ;
#33043 = CARTESIAN_POINT ( 'NONE',  ( 0.1640419947506569498, -0.05778040916215522460, 0.4822834645669289988 ) ) ;
#33044 = CARTESIAN_POINT ( 'NONE',  ( -0.9514435695538050464, -0.08942795157528024563, -0.3641732283464568787 ) ) ;
#33045 = CARTESIAN_POINT ( 'NONE',  ( 0.1958661417322836718, -0.3392501089628017219, 0.06887832201343642435 ) ) ;
#33046 = CARTESIAN_POINT ( 'NONE',  ( 0.9317585301837276734, -0.4281496062992124485, 0.4176697321401328655 ) ) ;
#33047 = ADVANCED_FACE ( 'NONE', ( #1048 ), #26702, .F. ) ;
#33048 = CARTESIAN_POINT ( 'NONE',  ( -1.253280839895012377, -0.3162353388693409650, -0.4822834645669289433 ) ) ;
#33049 = CARTESIAN_POINT ( 'NONE',  ( 0.2362204724409449064, 0.4091458600556404646, -1.323490813648294129 ) ) ;
#33050 = CARTESIAN_POINT ( 'NONE',  ( -0.7677165354330699465, 0.1660481256975885056, 0.3530559997133364547 ) ) ;
#33051 = CARTESIAN_POINT ( 'NONE',  ( -0.3149606299212590610, -0.1870078740157479769, 0.3641732283464567677 ) ) ;
#33052 = CARTESIAN_POINT ( 'NONE',  ( -1.095800524934382292, -0.3162353388693409650, -0.4822834645669289433 ) ) ;
#33053 = CARTESIAN_POINT ( 'NONE',  ( 0.8661417322834653598, -0.1870078740157479769, 0.3641732283464567677 ) ) ;
#33054 = CARTESIAN_POINT ( 'NONE',  ( -0.2755905511811018171, 0.1771653543307087630, 0.000000000000000000 ) ) ;
#33055 = CARTESIAN_POINT ( 'NONE',  ( -0.6233595800524928121, -0.05778040916215522460, 0.4822834645669289988 ) ) ;
#33057 = B_SPLINE_CURVE_WITH_KNOTS ( 'NONE', 3,
 ( #67128, #9458, #16202, #46497, #46913, #59966, #65885 ),
 .UNSPECIFIED., .F., .F.,
 ( 4, 3, 4 ),
 ( 3.469446951953614189E-17, 0.001246232571205268744, 0.002492492258783275856 ),
 .UNSPECIFIED. ) ;
#33056 = CARTESIAN_POINT ( 'NONE',  ( -1.325459317585300889, -0.4281496062992127816, -0.4176697321401328100 ) ) ;
#33058 = CARTESIAN_POINT ( 'NONE',  ( -1.581364829396324945, -0.05778040916215560624, -0.4822834645669293319 ) ) ;
#33059 = CARTESIAN_POINT ( 'NONE',  ( 0.4724409448818898682, 2.892866454678787531E-17, -2.084645669291338432 ) ) ;
#33060 = CARTESIAN_POINT ( 'NONE',  ( 1.384514435695538559, 0.1771653543307087075, -0.09757992244046823083 ) ) ;
#33061 = CARTESIAN_POINT ( 'NONE',  ( 0.4396325459317593221, 0.2952755905511810774, -0.1292274648535930714 ) ) ;
#33062 = CARTESIAN_POINT ( 'NONE',  ( 1.220472440944882386, 0.2952755905511811885, 0.000000000000000000 ) ) ;
#33063 = CARTESIAN_POINT ( 'NONE',  ( -1.653543307086613234, -0.1870078740157480879, -0.4822834645669291653 ) ) ;
#33064 = ORIENTED_EDGE ( 'NONE', *, *, #70713, .T. ) ;
#33065 = EDGE_CURVE ( 'NONE', #67145, #81967, #56647, .T. ) ;
#33066 = CARTESIAN_POINT ( 'NONE',  ( -0.1998031496062994405, 0.3460692066303957537, -2.609580052493438274 ) ) ;
#33067 = CARTESIAN_POINT ( 'NONE',  ( -1.062992125984250968, -0.5511811023622047445, 6.969142054262312111E-17 ) ) ;
#33068 = CARTESIAN_POINT ( 'NONE',  ( 0.9383202099737536495, -0.3162353388693405765, 0.4822834645669290543 ) ) ;
#33069 = AXIS2_PLACEMENT_3D ( 'NONE', #62960, #12856, #25458 ) ;
#33070 = CARTESIAN_POINT ( 'NONE',  ( -1.069553805774277722, 0.1771653543307087630, 0.09757992244046791164 ) ) ;
#33071 = CARTESIAN_POINT ( 'NONE',  ( 0.3460692066303958092, 0.1998031496062993018, -1.940288713910761409 ) ) ;
#33072 = CARTESIAN_POINT ( 'NONE',  ( -1.095800524934382292, -0.05778040916215522460, 0.4822834645669289988 ) ) ;
#33073 = CIRCLE ( 'NONE', #38469, 0.4923228346456693938 ) ;
#33074 = VECTOR ( 'NONE', #66390, 39.37007874015748143 ) ;
#33075 = CARTESIAN_POINT ( 'NONE',  ( 0.8530183727034128527, -0.4281496062992124485, 0.4176697321401328655 ) ) ;
#33076 = CARTESIAN_POINT ( 'NONE',  ( 0.3018372703412079971, 0.05413385826771626580, -0.4176697321401330321 ) ) ;
#33077 = CARTESIAN_POINT ( 'NONE',  ( 0.9973753280839902091, 0.2306618581243847221, -0.2411417322834647770 ) ) ;
#33078 = CARTESIAN_POINT ( 'NONE',  ( -1.725721784776902190, -0.08942795157527998196, 0.3641732283464567121 ) ) ;
#33079 = CARTESIAN_POINT ( 'NONE',  ( -0.2925321140481932369, 0.2925321140481930704, -1.041338582677165281 ) ) ;
#33080 = CARTESIAN_POINT ( 'NONE',  ( 0.1998031496062994405, -0.3460692066303958092, -1.194225721784776928 ) ) ;
#33081 = CARTESIAN_POINT ( 'NONE',  ( -0.3420746716998659953, -0.1974969037888706647, -0.6824146981627297048 ) ) ;
#33082 = CARTESIAN_POINT ( 'NONE',  ( 0.4469586986358917158, 1.697151583350163806, 2.611754389584974856 ) ) ;
#33083 = CARTESIAN_POINT ( 'NONE',  ( 0.9580052493438327987, -0.3690944881889765550, -0.3153832671262227771 ) ) ;
#33084 = CARTESIAN_POINT ( 'NONE',  ( 0.1837270341207354329, 0.1283753931104748280, 0.1820866141732283561 ) ) ;
#33085 = CARTESIAN_POINT ( 'NONE',  ( 0.1246719160104994284, -0.6692913385826771977, 0.1292274648535927661 ) ) ;
#33086 = CARTESIAN_POINT ( 'NONE',  ( 1.423884514435696191, -0.05778040916215522460, 0.4822834645669289988 ) ) ;
#33087 = CARTESIAN_POINT ( 'NONE',  ( 0.1058382717557500852, -0.3949938075777408852, -1.894356955380577245 ) ) ;
#33088 = CARTESIAN_POINT ( 'NONE',  ( 0.3608923884514443348, -0.5511811023622046335, 0.09757992244046803654 ) ) ;
#33089 = CARTESIAN_POINT ( 'NONE',  ( -0.9383202099737524282, -0.3162353388693409650, -0.4822834645669289433 ) ) ;
#33090 = CARTESIAN_POINT ( 'NONE',  ( 1.423884514435696191, -0.05778040916215522460, 0.4822834645669289988 ) ) ;
#33091 = CARTESIAN_POINT ( 'NONE',  ( 0.9645669291338591078, -0.5400638737290845981, -0.3530559997133363437 ) ) ;
#33092 = CARTESIAN_POINT ( 'NONE',  ( 0.3458507752293908943, 0.3458507752293908943, -2.027559055118109743 ) ) ;
#33093 = CARTESIAN_POINT ( 'NONE',  ( 1.614173228346457378, 1.330640075373405118, -0.1372047244094476148 ) ) ;
#33094 = VECTOR ( 'NONE', #47723, 39.37007874015748143 ) ;
#33095 = ORIENTED_EDGE ( 'NONE', *, *, #49331, .T. ) ;
#33096 = ORIENTED_EDGE ( 'NONE', *, *, #19297, .T. ) ;
#33097 = CARTESIAN_POINT ( 'NONE',  ( -1.437007874015747477, -0.5400638737290844871, 0.3530559997133364547 ) ) ;
#33099 = CARTESIAN_POINT ( 'NONE',  ( -0.5511811023622038563, -0.1870078740157479769, 0.4822834645669291653 ) ) ;
#33098 = CARTESIAN_POINT ( 'NONE',  ( -0.6758530183727028406, 0.1771653543307087630, 0.09757992244046791164 ) ) ;
#33100 = CARTESIAN_POINT ( 'NONE',  ( 0.1049643490035304522, -0.3917322834645668994, -2.370059424375641211 ) ) ;
#33101 = CARTESIAN_POINT ( 'NONE',  ( 0.1502491711592395529, -0.2549859370038549122, 0.1564451348283543985 ) ) ;
#33102 = CARTESIAN_POINT ( 'NONE',  ( -1.601049868766403650, 0.1283753931104746893, -0.1820866141732285504 ) ) ;
#33103 = CARTESIAN_POINT ( 'NONE',  ( -1.220472440944881054, 0.2952755905511811885, 0.000000000000000000 ) ) ;
#33104 = CARTESIAN_POINT ( 'NONE',  ( 0.1377952755905518800, -0.5400638737290844871, 0.3530559997133364547 ) ) ;
#33105 = CARTESIAN_POINT ( 'NONE',  ( -1.410761154855641575, -0.3162353388693409650, -0.4822834645669289433 ) ) ;
#33106 = CARTESIAN_POINT ( 'NONE',  ( 0.2867679344610365999, 0.2867679344610365999, 0.09251968503937001154 ) ) ;
#33107 = SHAPE_REPRESENTATION ( 'Independent Actuating Lead Screws', ( #22098 ), #649 ) ;
#33108 = CARTESIAN_POINT ( 'NONE',  ( 0.4593175853018379162, -0.4281496062992124485, 0.4176697321401328655 ) ) ;
#33109 = CARTESIAN_POINT ( 'NONE',  ( 0.3392501089628018329, 0.1958661417322835607, -1.698162729658792891 ) ) ;
#33110 = CARTESIAN_POINT ( 'NONE',  ( -0.8333333333333323711, 0.1771653543307087630, 0.09757992244046791164 ) ) ;
#33111 = VERTEX_POINT ( 'NONE', #206 ) ;
#33112 = CARTESIAN_POINT ( 'NONE',  ( -0.1058382717557503211, 0.3949938075777409408, -1.738845144356955696 ) ) ;
#33113 = EDGE_LOOP ( 'NONE', ( #51123, #17614, #26039, #75865, #6701, #22047, #75320, #9211, #79948, #26468 ) ) ;
#33114 = DIRECTION ( 'NONE',  ( 1.000000000000000000, 0.000000000000000000, 0.000000000000000000 ) ) ;
#33115 = CARTESIAN_POINT ( 'NONE',  ( -1.167979002624671470, -0.4281496062992127816, -0.4176697321401328100 ) ) ;
#33116 = CARTESIAN_POINT ( 'NONE',  ( -1.443569553805773564, 0.2306618581243847221, -0.2411417322834647770 ) ) ;
#33117 = CARTESIAN_POINT ( 'NONE',  ( -0.1070741851644051862, -0.3996062992125987146, -0.7020997375328084100 ) ) ;
#33118 = CARTESIAN_POINT ( 'NONE',  ( -1.089238845144356427, 0.05413385826771666132, 0.4176697321401328100 ) ) ;
#33119 = CARTESIAN_POINT ( 'NONE',  ( -1.358267716535432434, 0.1660481256975883668, -0.3530559997133364547 ) ) ;
#33120 = CARTESIAN_POINT ( 'NONE',  ( -1.286089238845143479, 0.2306618581243847221, -0.2411417322834647770 ) ) ;
#33121 = CARTESIAN_POINT ( 'NONE',  ( -1.604771003085129655, 1.829390573268580455, 0.1466069496707748387 ) ) ;
#33122 = CARTESIAN_POINT ( 'NONE',  ( -0.03443470937339728616, 1.062992125984252079, -1.635441089090149402 ) ) ;
#33123 = CARTESIAN_POINT ( 'NONE',  ( 0.1706036745406830368, -0.3690944881889765550, -0.3153832671262227771 ) ) ;
#33124 = CARTESIAN_POINT ( 'NONE',  ( -0.03443470937343537375, 1.064243487142137568, -1.440673310089392478 ) ) ;
#33125 = CARTESIAN_POINT ( 'NONE',  ( 0.1958661417322834775, 0.3392501089628018884, -0.5439632545931759600 ) ) ;
#33126 = CARTESIAN_POINT ( 'NONE',  ( -0.2624671916010490880, 0.1283753931104746893, -0.1820866141732285504 ) ) ;
#33127 = CARTESIAN_POINT ( 'NONE',  ( -0.7020997375328074108, -0.05778040916215522460, 0.4822834645669289988 ) ) ;
#33128 = CARTESIAN_POINT ( 'NONE',  ( 1.148293963254593653, 0.2952755905511810774, -0.1292274648535930714 ) ) ;
#33129 = CARTESIAN_POINT ( 'NONE',  ( -0.5577427821522301654, -0.3162353388693405765, 0.4822834645669290543 ) ) ;
#33130 = ORIENTED_EDGE ( 'NONE', *, *, #52141, .T. ) ;
#33131 = ORIENTED_EDGE ( 'NONE', *, *, #57575, .F. ) ;
#33132 = CARTESIAN_POINT ( 'NONE',  ( -0.3996062992125986590, 0.1070741851644051723, -2.156824146981627166 ) ) ;
#33133 = CARTESIAN_POINT ( 'NONE',  ( -0.9711286089238838626, 0.2306618581243847221, -0.2411417322834647770 ) ) ;
#33134 = CARTESIAN_POINT ( 'NONE',  ( 0.7349081364829402885, -0.6046776061558809534, -0.2411417322834644161 ) ) ;
#33135 = CARTESIAN_POINT ( 'NONE',  ( -1.692913385826770645, 0.1771653543307087630, 0.000000000000000000 ) ) ;
#33136 = CARTESIAN_POINT ( 'NONE',  ( 0.2362204724409449064, 0.4091458600556404646, -1.404199475065616820 ) ) ;
#33137 = CARTESIAN_POINT ( 'NONE',  ( 0.5314960629920917334, 2.755905511811024056, 3.264097702071378393 ) ) ;
#33138 = CARTESIAN_POINT ( 'NONE',  ( 0.2867679344610365999, 0.2867679344610365999, -0.4448818897637794589 ) ) ;
#33139 = AXIS2_PLACEMENT_3D ( 'NONE', #77981, #7695, #64502 ) ;
#33140 = CARTESIAN_POINT ( 'NONE',  ( 0.1958661417322836440, -0.3392501089628017219, -2.066272965879265122 ) ) ;
#33141 = CARTESIAN_POINT ( 'NONE',  ( -0.1246719160104980823, -0.6692913385826773087, -0.1292274648535924053 ) ) ;
#33142 = CARTESIAN_POINT ( 'NONE',  ( 1.679790026246720025, 0.2306618581243848609, 0.2411417322834645549 ) ) ;
#33143 = AXIS2_PLACEMENT_3D ( 'NONE', #21373, #47857, #35244 ) ;
#33144 = AXIS2_PLACEMENT_3D ( 'NONE', #38052, #70041, #25002 ) ;
#33145 = CARTESIAN_POINT ( 'NONE',  ( -0.7808398950131225646, -0.05778040916215522460, 0.4822834645669289988 ) ) ;
#33146 = CARTESIAN_POINT ( 'NONE',  ( -0.3460692066303957537, -0.1998031496062994405, 0.02821522309711283621 ) ) ;
#33148 = CARTESIAN_POINT ( 'NONE',  ( -1.076935383196057527, 2.559055118110236560, 0.3149606299212596716 ) ) ;
#33147 = CARTESIAN_POINT ( 'NONE',  ( -1.246719160104986512, 0.05413385826771666132, 0.4176697321401328100 ) ) ;
#33149 = CARTESIAN_POINT ( 'NONE',  ( -0.8792650918635160906, 0.05413385826771626580, -0.4176697321401330321 ) ) ;
#33150 = CARTESIAN_POINT ( 'NONE',  ( -0.5905511811023615998, 0.2952755905511811885, 0.000000000000000000 ) ) ;
#33151 = CARTESIAN_POINT ( 'NONE',  ( -0.3949938075777408852, -0.1058382717557502933, -2.642388451443569597 ) ) ;
#33152 = CARTESIAN_POINT ( 'NONE',  ( 0.8202099737532813073, 0.1771653543307087630, 0.09757992244046791164 ) ) ;
#33153 = CARTESIAN_POINT ( 'NONE',  ( 4.797336870675656522E-17, -0.3917322834645670104, -0.005905511811023714773 ) ) ;
#33154 = CARTESIAN_POINT ( 'NONE',  ( 0.5446194225721792126, -0.2845877964562159024, 0.3641732283464567677 ) ) ;
#33155 = CARTESIAN_POINT ( 'NONE',  ( 1.207349081364829990, -0.5023911411419708095, -0.1820866141732282451 ) ) ;
#33156 = CARTESIAN_POINT ( 'NONE',  ( 1.489501312335958172, -0.05778040916215560624, -0.4822834645669293319 ) ) ;
#33157 = CARTESIAN_POINT ( 'NONE',  ( 0.02624671916010564918, -0.5023911411419708095, -0.1820866141732282451 ) ) ;
#33158 = CARTESIAN_POINT ( 'NONE',  ( -0.3392501089628019995, 0.1958661417322832277, -1.750656167979002698 ) ) ;
#33159 = CARTESIAN_POINT ( 'NONE',  ( -1.404199475065615932, -0.4281496062992127816, -0.4176697321401328100 ) ) ;
#33160 = CARTESIAN_POINT ( 'NONE',  ( 1.351706036745407458, -0.4281496062992127816, -0.4176697321401328100 ) ) ;
#33161 = VECTOR ( 'NONE', #36122, 39.37007874015748143 ) ;
#33162 = CARTESIAN_POINT ( 'NONE',  ( -0.4091458600556405756, 0.2362204724409446288, 0.05446194225721784354 ) ) ;
#33163 = CARTESIAN_POINT ( 'NONE',  ( -0.5774278215223089816, -0.5023911411419708095, 0.1820866141732285504 ) ) ;
#33164 = CARTESIAN_POINT ( 'NONE',  ( 1.614173228346457156, 1.929133858267716661, 0.5309055118110233007 ) ) ;
#33165 = CARTESIAN_POINT ( 'NONE',  ( 0.2427821522309719648, -0.05778040916215522460, 0.4822834645669289988 ) ) ;
#33166 = LINE ( 'NONE', #6646, #73406 ) ;
#33167 = CARTESIAN_POINT ( 'NONE',  ( 0.7545931758530188826, -0.5511811023622046335, 0.09757992244046803654 ) ) ;
#33168 = CARTESIAN_POINT ( 'NONE',  ( 0.09186351706036799403, -0.3690944881889765550, -0.3153832671262227771 ) ) ;
#33169 = CARTESIAN_POINT ( 'NONE',  ( -0.2230971128608915943, 0.05413385826771666132, 0.4176697321401328100 ) ) ;
#33170 = CARTESIAN_POINT ( 'NONE',  ( -1.371391076115484831, 0.2952755905511810774, -0.1292274648535930714 ) ) ;
#33171 = CARTESIAN_POINT ( 'NONE',  ( -0.6824146981627288167, 0.1283753931104748280, 0.1820866141732283561 ) ) ;
#33172 = DIRECTION ( 'NONE',  ( -0.000000000000000000, -1.000000000000000000, -0.000000000000000000 ) ) ;
#33173 = CARTESIAN_POINT ( 'NONE',  ( 0.4199475065616805614, 0.2306618581243848609, 0.2411417322834645549 ) ) ;
#33174 = CARTESIAN_POINT ( 'NONE',  ( -0.9186351706036736120, -0.6046776061558809534, -0.2411417322834644161 ) ) ;
#33175 = CARTESIAN_POINT ( 'NONE',  ( -0.1070741851644056997, 0.3996062992125984925, -1.185695538057742526 ) ) ;
#33176 = CARTESIAN_POINT ( 'NONE',  ( 0.3917322834645670104, 2.398668435337828261E-17, -2.879921259842519454 ) ) ;
#33177 = CARTESIAN_POINT ( 'NONE',  ( 0.2952755905511816326, -0.4536011799217367080, 0.2665933059059888421 ) ) ;
#33178 = CARTESIAN_POINT ( 'NONE',  ( -0.9973753280839886548, 0.2306618581243848609, 0.2411417322834645549 ) ) ;
#33179 = CARTESIAN_POINT ( 'NONE',  ( -1.213910761154854745, -0.6692913385826771977, 0.1292274648535927661 ) ) ;
#33180 = CARTESIAN_POINT ( 'NONE',  ( -1.305774278215222184, 0.1771653543307087630, 0.09757992244046791164 ) ) ;
#33181 = CARTESIAN_POINT ( 'NONE',  ( 1.581364829396326277, -0.3162353388693409650, -0.4822834645669289433 ) ) ;
#33182 = EDGE_CURVE ( 'NONE', #5038, #51414, #33851, .T. ) ;
#33183 = CARTESIAN_POINT ( 'NONE',  ( -0.9317585301837263412, -0.3690944881889765550, -0.3153832671262227771 ) ) ;
#33184 = CARTESIAN_POINT ( 'NONE',  ( 1.227034120734908917, -0.6692913385826771977, 0.1292274648535927661 ) ) ;
#33185 = CARTESIAN_POINT ( 'NONE',  ( 0.1070741851644053527, 0.3996062992125986590, 0.006561679790026237087 ) ) ;
#33186 = CARTESIAN_POINT ( 'NONE',  ( -0.3917322834645671770, 0.1049643490035302024, -2.549231914207035654 ) ) ;
#33187 = VERTEX_POINT ( 'NONE', #71740 ) ;
#33188 = EDGE_CURVE ( 'NONE', #45259, #9709, #52628, .T. ) ;
#33189 = CARTESIAN_POINT ( 'NONE',  ( 0.4697243008124812880, 1.606021484273581823, -2.565507813389724223 ) ) ;
#33190 = CARTESIAN_POINT ( 'NONE',  ( -1.660104986876639543, -0.05778040916215560624, -0.4822834645669293319 ) ) ;
#33191 = CARTESIAN_POINT ( 'NONE',  ( -1.292650918635170010, -0.6692913385826771977, 0.1292274648535927661 ) ) ;
#33192 = VECTOR ( 'NONE', #54607, 39.37007874015748143 ) ;
#33193 = CARTESIAN_POINT ( 'NONE',  ( 1.095800524934383846, -0.3162353388693405765, 0.4822834645669290543 ) ) ;
#33194 = CARTESIAN_POINT ( 'NONE',  ( -0.1958661417322834220, -0.3392501089628018884, -2.197506561679789971 ) ) ;
#33195 = LINE ( 'NONE', #45381, #52524 ) ;
#33196 = CARTESIAN_POINT ( 'NONE',  ( 0.4527559055118117182, 0.1660481256975883668, -0.3530559997133364547 ) ) ;
#33197 = CARTESIAN_POINT ( 'NONE',  ( -0.2099737532808391705, 0.2306618581243848609, 0.2411417322834645549 ) ) ;
#33198 = CARTESIAN_POINT ( 'NONE',  ( 0.4441561269002810564, 1.369975275916394342, -3.911878359814730644 ) ) ;
#33199 = CIRCLE ( 'NONE', #30550, 0.09842519685039351207 ) ;
#33200 =( GEOMETRIC_REPRESENTATION_CONTEXT ( 3 ) GLOBAL_UNCERTAINTY_ASSIGNED_CONTEXT ( ( #28496 ) ) GLOBAL_UNIT_ASSIGNED_CONTEXT ( ( #81468, #30517, #17903 ) ) REPRESENTATION_CONTEXT ( 'NONE', 'WORKASPACE' ) );
#33202 = CARTESIAN_POINT ( 'NONE',  ( 0.06804098107080244762, 1.722984403643211298E-16, -0.4118484887281974594 ) ) ;
#33201 = CONICAL_SURFACE ( 'NONE', #25119, 2.637795275590551380, 0.7853981633974500554 ) ;
#33203 = CARTESIAN_POINT ( 'NONE',  ( 0.9776902887139113929, 0.1771653543307087630, 0.09757992244046791164 ) ) ;
#33204 = CARTESIAN_POINT ( 'NONE',  ( -0.3996062992125986035, -0.1070741851644056997, -1.463254593175853158 ) ) ;
#33205 = EDGE_LOOP ( 'NONE', ( #48733, #76091, #39632, #8564 ) ) ;
#33206 = CARTESIAN_POINT ( 'NONE',  ( 0.3392501089628018329, 0.1958661417322835607, -0.1279720716873509745 ) ) ;
#33207 = ORIENTED_EDGE ( 'NONE', *, *, #72797, .F. ) ;
#33208 = CARTESIAN_POINT ( 'NONE',  ( -0.03937007874015669567, -0.6692913385826771977, 8.415575281601705876E-17 ) ) ;
#33209 = PRODUCT_DEFINITION_SHAPE ( 'NONE', 'NONE',  #83324 ) ;
#33210 = CARTESIAN_POINT ( 'NONE',  ( 1.437007874015748810, 0.1660481256975885056, 0.3530559997133364547 ) ) ;
#33211 = CARTESIAN_POINT ( 'NONE',  ( 0.1312335958005257930, 0.2306618581243847221, -0.2411417322834647770 ) ) ;
#33212 = CARTESIAN_POINT ( 'NONE',  ( 1.351706036745407680, 0.05413385826771666132, 0.4176697321401328100 ) ) ;
#33213 = CARTESIAN_POINT ( 'NONE',  ( -0.3083989501312330295, -0.3162353388693409650, -0.4822834645669289433 ) ) ;
#33214 = CARTESIAN_POINT ( 'NONE',  ( -0.05249343832020938322, -0.6046776061558809534, -0.2411417322834644161 ) ) ;
#33215 = CARTESIAN_POINT ( 'NONE',  ( 1.568241469816273437, -0.3162353388693405765, 0.4822834645669290543 ) ) ;
#33216 = CARTESIAN_POINT ( 'NONE',  ( 1.266404199475066328, -0.05778040916215522460, 0.4822834645669289988 ) ) ;
#33217 = EDGE_CURVE ( 'NONE', #18027, #2500, #22920, .T. ) ;
#33218 = CARTESIAN_POINT ( 'NONE',  ( 1.161417322834646493, -0.5400638737290844871, 0.3530559997133364547 ) ) ;
#33219 = CARTESIAN_POINT ( 'NONE',  ( 0.2867679344610365999, 0.2867679344610365999, -0.2874015748031494843 ) ) ;
#33220 = CARTESIAN_POINT ( 'NONE',  ( 0.2362204724409456558, -0.1870078740157479769, 0.3641732283464567677 ) ) ;
#33221 = VERTEX_POINT ( 'NONE', #79317 ) ;
#33222 = CARTESIAN_POINT ( 'NONE',  ( -0.1058382717557497937, -0.3949938075777411628, -0.5446194225721784354 ) ) ;
#33223 = ORIENTED_EDGE ( 'NONE', *, *, #28501, .T. ) ;
#33224 = CARTESIAN_POINT ( 'NONE',  ( -0.5249343832020990641, -0.5023911411419708095, -0.1820866141732282451 ) ) ;
#33225 = CARTESIAN_POINT ( 'NONE',  ( -0.1837270341207340729, 0.2306618581243847221, -0.2411417322834647770 ) ) ;
#33226 = CARTESIAN_POINT ( 'NONE',  ( 2.571257611060531190, 1.453715418023198591, 0.4672341690643353473 ) ) ;
#33227 = CARTESIAN_POINT ( 'NONE',  ( 0.2296587926509192634, -0.05778040916215560624, -0.4822834645669293319 ) ) ;
#33228 = CARTESIAN_POINT ( 'NONE',  ( 0.1246719160104994284, -0.6692913385826771977, 0.1292274648535927661 ) ) ;
#33229 = CARTESIAN_POINT ( 'NONE',  ( -0.7677165354330699465, -0.5400638737290845981, -0.3530559997133363437 ) ) ;
#33230 = CARTESIAN_POINT ( 'NONE',  ( -1.174540682414697335, -0.3162353388693409650, -0.4822834645669289433 ) ) ;
#33231 = EDGE_CURVE ( 'NONE', #63414, #37754, #44558, .T. ) ;
#33232 = CARTESIAN_POINT ( 'NONE',  ( 1.568241469816273659, -0.08942795157528024563, -0.3641732283464568787 ) ) ;
#33233 = CARTESIAN_POINT ( 'NONE',  ( 1.595398199321655497, 0.4619154201552252981, 0.1559797534342493852 ) ) ;
#33234 = LINE ( 'NONE', #39536, #62542 ) ;
#33235 = CARTESIAN_POINT ( 'NONE',  ( 0.8727034120734912248, -0.2845877964562161244, -0.3641732283464567121 ) ) ;
#33236 = CARTESIAN_POINT ( 'NONE',  ( 0.6036745406824154392, 0.2306618581243847221, -0.2411417322834647770 ) ) ;
#33237 = CARTESIAN_POINT ( 'NONE',  ( 0.8136482939632553313, -0.6046776061558809534, -0.2411417322834644161 ) ) ;
#33238 = CARTESIAN_POINT ( 'NONE',  ( -0.1998031496062991907, -0.3460692066303959757, -1.482939632545931863 ) ) ;
#33239 = DIRECTION ( 'NONE',  ( 0.000000000000000000, 0.000000000000000000, 1.000000000000000000 ) ) ;
#33240 = CARTESIAN_POINT ( 'NONE',  ( -0.3460692066303957537, -0.1998031496062994405, -0.6017060367454067915 ) ) ;
#33241 = CARTESIAN_POINT ( 'NONE',  ( 0.1070741851644053388, 0.3996062992125986035, -0.07020997375328086321 ) ) ;
#33242 = CARTESIAN_POINT ( 'NONE',  ( -0.4658792650918627265, -0.05778040916215522460, 0.4822834645669289988 ) ) ;
#33243 = CARTESIAN_POINT ( 'NONE',  ( 0.3996062992125986035, 2.446882876249141962E-17, -2.795275590551181022 ) ) ;
#33244 = EDGE_CURVE ( 'NONE', #11621, #15186, #16376, .T. ) ;
#33245 = CARTESIAN_POINT ( 'NONE',  ( -9.594673741351313045E-17, 0.3917322834645670104, -2.289370078740157410 ) ) ;
#33246 = CARTESIAN_POINT ( 'NONE',  ( -1.010498687664041384, -0.004921259842519576551, 0.3153832671262227771 ) ) ;
#33247 = CARTESIAN_POINT ( 'NONE',  ( 1.286089238845145033, 0.2306618581243848609, 0.2411417322834645549 ) ) ;
#33248 = CARTESIAN_POINT ( 'NONE',  ( 0.9448818897637802916, -0.1870078740157480879, -0.4822834645669291653 ) ) ;
#33249 = CARTESIAN_POINT ( 'NONE',  ( -0.3346456692913377662, 0.07958543189024071263, -0.2665933059059888421 ) ) ;
#33250 = CARTESIAN_POINT ( 'NONE',  ( 0.3280839895013130669, 0.05413385826771666132, 0.4176697321401328100 ) ) ;
#33251 = CARTESIAN_POINT ( 'NONE',  ( 0.4724409448818896462, 0.1265901696524990294, -1.303805774278215202 ) ) ;
#33252 = CARTESIAN_POINT ( 'NONE',  ( 0.2034120734908144990, -0.5511811023622046335, 0.09757992244046803654 ) ) ;
#33253 = CARTESIAN_POINT ( 'NONE',  ( -0.2034120734908131112, -0.6692913385826773087, -0.1292274648535924053 ) ) ;
#33254 = CARTESIAN_POINT ( 'NONE',  ( 0.1058382717557499880, 0.3949938075777409408, -1.330052493438319994 ) ) ;
#33255 = CARTESIAN_POINT ( 'NONE',  ( -1.207349081364828880, 0.2306618581243847221, -0.2411417322834647770 ) ) ;
#33256 = CARTESIAN_POINT ( 'NONE',  ( 0.6955380577427828781, -0.004921259842519870586, -0.3153832671262229437 ) ) ;
#33257 = CARTESIAN_POINT ( 'NONE',  ( -2.611722799339339485, 1.697109554835841472, -0.4469779880792068005 ) ) ;
#33258 = CARTESIAN_POINT ( 'NONE',  ( -0.6036745406824141069, 0.2306618581243848609, 0.2411417322834645549 ) ) ;
#33259 = CARTESIAN_POINT ( 'NONE',  ( -0.3543307086614165824, 0.1771653543307087630, 0.000000000000000000 ) ) ;
#33260 = CARTESIAN_POINT ( 'NONE',  ( 3.900966923095589678, 2.677165354330708791, 0.5314960629921260393 ) ) ;
#33261 = CARTESIAN_POINT ( 'NONE',  ( -0.8202099737532801971, -0.6692913385826771977, 0.1292274648535927661 ) ) ;
#33262 = CARTESIAN_POINT ( 'NONE',  ( -0.7808398950131222316, -0.3162353388693409650, -0.4822834645669289433 ) ) ;
#33263 = CARTESIAN_POINT ( 'NONE',  ( -0.08530183727034056085, -0.3162353388693405765, 0.4822834645669290543 ) ) ;
#33264 = CARTESIAN_POINT ( 'NONE',  ( -0.2925321140481930149, -0.2925321140481933480, -2.340551181102362488 ) ) ;
#33265 = CARTESIAN_POINT ( 'NONE',  ( -0.1706036745406816491, 0.05413385826771626580, -0.4176697321401330321 ) ) ;
#33266 = AXIS2_PLACEMENT_3D ( 'NONE', #30048, #75101, #42259 ) ;
#33268 = CARTESIAN_POINT ( 'NONE',  ( 0.1049643490035303689, 0.3917322834645668994, -2.120715592354644130 ) ) ;
#33267 = CIRCLE ( 'NONE', #80325, 0.1978346456692914035 ) ;
#33269 = CARTESIAN_POINT ( 'NONE',  ( 3.937007874015748143, 1.537401574803149984, 2.901595197523589142E-16 ) ) ;
#33270 = CARTESIAN_POINT ( 'NONE',  ( 0.7086614173228353852, -0.1870078740157479769, 0.3641732283464567677 ) ) ;
#33271 = CARTESIAN_POINT ( 'NONE',  ( 1.246719160104987623, -0.4281496062992124485, 0.4176697321401328655 ) ) ;
#33272 = CARTESIAN_POINT ( 'NONE',  ( -0.8267716535433065062, -0.5511811023622047445, 6.969142054262312111E-17 ) ) ;
#33273 = CARTESIAN_POINT ( 'NONE',  ( -0.9973753280839886548, -0.5023911411419708095, -0.1820866141732282451 ) ) ;
#33274 = CARTESIAN_POINT ( 'NONE',  ( -0.6758530183727028406, 0.2952755905511811885, 0.1292274648535926551 ) ) ;
#33275 = CARTESIAN_POINT ( 'NONE',  ( -0.1377952755905504645, 0.1660481256975885056, 0.3530559997133364547 ) ) ;
#33276 = CARTESIAN_POINT ( 'NONE',  ( 0.4330708661417329575, 0.1771653543307087630, 0.000000000000000000 ) ) ;
#33277 = LINE ( 'NONE', #51344, #38061 ) ;
#33278 = CARTESIAN_POINT ( 'NONE',  ( 0.8661417322834652488, -0.1870078740157480601, -0.3641732283464567677 ) ) ;
#33279 = CARTESIAN_POINT ( 'NONE',  ( 0.3805774278215230400, -0.4281496062992124485, 0.4176697321401328655 ) ) ;
#33280 = CARTESIAN_POINT ( 'NONE',  ( 0.3460692066303958092, 0.1998031496062993018, 0.1069553805774278027 ) ) ;
#33281 = CARTESIAN_POINT ( 'NONE',  ( -0.7742782152230965886, 0.05413385826771666132, 0.4176697321401328100 ) ) ;
#33282 = CARTESIAN_POINT ( 'NONE',  ( -0.3392501089628019995, 0.1958661417322832277, -1.213254593175852936 ) ) ;
#33283 = CARTESIAN_POINT ( 'NONE',  ( 1.279527559055118724, 0.07958543189024085140, 0.2665933059059887866 ) ) ;
#33284 = CARTESIAN_POINT ( 'NONE',  ( 0.4724409448818904789, -0.1870078740157480879, -0.4822834645669291653 ) ) ;
#33285 = CARTESIAN_POINT ( 'NONE',  ( 0.2755905511811031494, 0.2952755905511811885, 0.000000000000000000 ) ) ;
#33286 = CARTESIAN_POINT ( 'NONE',  ( 0.2034120734908144990, -0.5511811023622046335, 0.09757992244046803654 ) ) ;
#33287 = CARTESIAN_POINT ( 'NONE',  ( 0.6175017169405826456, 2.784432375088962958E-17, -0.3464511005275205946 ) ) ;
#33288 = CARTESIAN_POINT ( 'NONE',  ( -0.1574803149606292529, -0.1870078740157480601, -0.3641732283464567677 ) ) ;
#33289 = CARTESIAN_POINT ( 'NONE',  ( 0.8530183727034128527, -0.4281496062992124485, 0.4176697321401328655 ) ) ;
#33290 = EDGE_CURVE ( 'NONE', #56483, #42415, #29197, .T. ) ;
#33291 = CARTESIAN_POINT ( 'NONE',  ( -0.7480314960629914633, 0.1771653543307087630, 0.000000000000000000 ) ) ;
#33292 = CARTESIAN_POINT ( 'NONE',  ( -0.7545931758530176614, -0.6692913385826773087, -0.1292274648535924053 ) ) ;
#33293 = CARTESIAN_POINT ( 'NONE',  ( -0.4724409448818898682, -8.678599364036362592E-17, -2.559055118110236560 ) ) ;
#33294 = ORIENTED_EDGE ( 'NONE', *, *, #12532, .F. ) ;
#33295 = CARTESIAN_POINT ( 'NONE',  ( -1.292650918635170010, 0.2952755905511810774, -0.1292274648535930714 ) ) ;
#33296 = CARTESIAN_POINT ( 'NONE',  ( -1.292650918635170010, -0.5511811023622046335, 0.09757992244046803654 ) ) ;
#33297 = CARTESIAN_POINT ( 'NONE',  ( 0.08530183727034192087, -0.3162353388693409650, -0.4822834645669289433 ) ) ;
#33298 = CARTESIAN_POINT ( 'NONE',  ( -1.496062992125983815, -0.1870078740157480879, -0.4822834645669291653 ) ) ;
#33299 = CARTESIAN_POINT ( 'NONE',  ( -0.6233595800524928121, -0.3162353388693409650, -0.4822834645669289433 ) ) ;
#33300 = DIRECTION ( 'NONE',  ( -1.000000000000000000, -3.412570772413389987E-16, 0.000000000000000000 ) ) ;
#33302 = CARTESIAN_POINT ( 'NONE',  ( 0.9973753280839902091, 0.2306618581243847221, -0.2411417322834647770 ) ) ;
#33301 = CARTESIAN_POINT ( 'NONE',  ( 1.076115485564305141, 0.2306618581243847221, -0.2411417322834647770 ) ) ;
#33303 = CARTESIAN_POINT ( 'NONE',  ( 1.430446194225722500, -0.4281496062992127816, -0.4176697321401328100 ) ) ;
#33304 = CARTESIAN_POINT ( 'NONE',  ( 0.3917322834645670104, -0.1049643490035303273, -2.465879265091862838 ) ) ;
#33305 = CARTESIAN_POINT ( 'NONE',  ( 1.548556430446194954, -0.6046776061558807314, 0.2411417322834647770 ) ) ;
#33306 = CARTESIAN_POINT ( 'NONE',  ( -1.194225721784776262, 0.05413385826771626580, -0.4176697321401330321 ) ) ;
#33307 = CARTESIAN_POINT ( 'NONE',  ( -0.4091458600556402980, -0.2362204724409451284, -0.8398950131233595684 ) ) ;
#33308 = CARTESIAN_POINT ( 'NONE',  ( 0.2925321140481932369, -0.2925321140481932369, -0.09842519685039373412 ) ) ;
#33309 = VERTEX_POINT ( 'NONE', #21636 ) ;
#33310 = CARTESIAN_POINT ( 'NONE',  ( -0.1968503937007867743, 0.1771653543307087630, 0.000000000000000000 ) ) ;
#33311 = CARTESIAN_POINT ( 'NONE',  ( 0.2867679344610365999, 0.2867679344610365999, -1.704724409448818978 ) ) ;
#33312 = ORIENTED_EDGE ( 'NONE', *, *, #34017, .F. ) ;
#33313 = CARTESIAN_POINT ( 'NONE',  ( 0.06561679790026316017, 0.05413385826771626580, -0.4176697321401330321 ) ) ;
#33314 = CARTESIAN_POINT ( 'NONE',  ( 0.2296587926509192634, -0.05778040916215560624, -0.4822834645669293319 ) ) ;
#33315 = CARTESIAN_POINT ( 'NONE',  ( -0.6167979002624665030, -0.4281496062992127816, -0.4176697321401328100 ) ) ;
#33316 = CARTESIAN_POINT ( 'NONE',  ( -0.06463254593175619955, 0.06463254593175608853, -0.5032808398950130435 ) ) ;
#33317 = CARTESIAN_POINT ( 'NONE',  ( -0.8070866141732276899, 0.07958543189024071263, -0.2665933059059888421 ) ) ;
#33318 = DIRECTION ( 'NONE',  ( -0.000000000000000000, -1.000000000000000000, -0.000000000000000000 ) ) ;
#33319 = CARTESIAN_POINT ( 'NONE',  ( 0.8005249343832028242, -0.4281496062992127816, -0.4176697321401328100 ) ) ;
#33320 = CARTESIAN_POINT ( 'NONE',  ( 0.4790026246719167324, -0.08942795157527998196, 0.3641732283464567121 ) ) ;
#33321 = CARTESIAN_POINT ( 'NONE',  ( -0.3412073490813641308, 0.2306618581243847221, -0.2411417322834647770 ) ) ;
#33322 = CARTESIAN_POINT ( 'NONE',  ( -0.2867679344610364334, -0.2867679344610368219, -1.083970185530496844 ) ) ;
#33323 = CARTESIAN_POINT ( 'NONE',  ( -0.6430446194225712953, 0.05413385826771626580, -0.4176697321401330321 ) ) ;
#33324 = CARTESIAN_POINT ( 'NONE',  ( -1.574803149606298636, -0.1870078740157479769, 0.3641732283464567677 ) ) ;
#33325 = CARTESIAN_POINT ( 'NONE',  ( 1.167979002624672580, -0.4281496062992124485, 0.4176697321401328655 ) ) ;
#33326 = CARTESIAN_POINT ( 'NONE',  ( 1.660104986876641320, -0.08942795157527998196, 0.3641732283464567121 ) ) ;
#33327 = VERTEX_POINT ( 'NONE', #54864 ) ;
#33328 = CARTESIAN_POINT ( 'NONE',  ( 0.3917322834645670659, 2.398668435337828261E-17, -2.319573121556117279 ) ) ;
#33329 = CARTESIAN_POINT ( 'NONE',  ( -0.1377952755905504645, -0.5400638737290845981, -0.3530559997133363437 ) ) ;
#33330 = ORIENTED_EDGE ( 'NONE', *, *, #43286, .T. ) ;
#33331 = CONICAL_SURFACE ( 'NONE', #83055, 0.1978346456692914035, 0.8726646259971700959 ) ;
#33332 = CARTESIAN_POINT ( 'NONE',  ( -0.8595800524934373854, -0.3162353388693409650, -0.4822834645669289433 ) ) ;
#33333 = CARTESIAN_POINT ( 'NONE',  ( 1.548556430446194954, -0.6046776061558807314, 0.2411417322834647770 ) ) ;
#33334 = CARTESIAN_POINT ( 'NONE',  ( 1.233595800524935227, -0.6046776061558807314, 0.2411417322834647770 ) ) ;
#33335 = CARTESIAN_POINT ( 'NONE',  ( 0.1312335958005255154, -0.6046776061558807314, 0.2411417322834647770 ) ) ;
#33336 = CARTESIAN_POINT ( 'NONE',  ( -0.2690288713910754526, -0.6692913385826771977, 0.1292274648535927661 ) ) ;
#33337 = CARTESIAN_POINT ( 'NONE',  ( 0.3392501089628018884, -0.1958661417322834220, -1.764435695538057791 ) ) ;
#33338 = CARTESIAN_POINT ( 'NONE',  ( -1.207349081364828880, 0.2306618581243847221, -0.2411417322834647770 ) ) ;
#33339 = CARTESIAN_POINT ( 'NONE',  ( -0.07217847769028787330, -0.05778040916215522460, 0.4822834645669289988 ) ) ;
#33340 = CARTESIAN_POINT ( 'NONE',  ( 0.06561679790026316017, -0.3690944881889763329, 0.3153832671262228327 ) ) ;
#33341 = DIRECTION ( 'NONE',  ( 0.000000000000000000, 0.000000000000000000, 1.000000000000000000 ) ) ;
#33342 = CARTESIAN_POINT ( 'NONE',  ( -0.3937007874015740483, -0.1870078740157480879, -0.4822834645669291653 ) ) ;
#33343 = DIRECTION ( 'NONE',  ( -1.000000000000000000, 1.445602896647338917E-16, -0.000000000000000000 ) ) ;
#33344 = CARTESIAN_POINT ( 'NONE',  ( 1.318897637795276356, 0.1660481256975883668, -0.3530559997133364547 ) ) ;
#33345 = DIRECTION ( 'NONE',  ( 3.491481338843132961E-15, 0.000000000000000000, -1.000000000000000000 ) ) ;
#33346 = VERTEX_POINT ( 'NONE', #67506 ) ;
#33347 = CARTESIAN_POINT ( 'NONE',  ( -0.1115485564304453947, -0.6692913385826771977, 0.1292274648535927661 ) ) ;
#33348 = CARTESIAN_POINT ( 'NONE',  ( -0.1574803149606292529, -0.1870078740157479769, 0.3641732283464567677 ) ) ;
#33349 = CARTESIAN_POINT ( 'NONE',  ( 0.9251968503937015864, 0.07958543189024071263, -0.2665933059059888421 ) ) ;
#33350 = CARTESIAN_POINT ( 'NONE',  ( -0.4091458600556402980, -0.2362204724409451284, -0.1292650918635170620 ) ) ;
#33351 = CARTESIAN_POINT ( 'NONE',  ( 1.220472440944882386, 0.000000000000000000, 0.4445507791589061175 ) ) ;
#33352 = CARTESIAN_POINT ( 'NONE',  ( 1.299212598425197429, 0.2952755905511811885, 0.000000000000000000 ) ) ;
#33353 = CARTESIAN_POINT ( 'NONE',  ( 0.1058382717557500852, -0.3949938075777408852, -0.1620734908136483021 ) ) ;
#33354 = CARTESIAN_POINT ( 'NONE',  ( 0.1968503937007881344, 0.2952755905511811885, 0.000000000000000000 ) ) ;
#33355 = LINE ( 'NONE', #33765, #20343 ) ;
#33356 = CARTESIAN_POINT ( 'NONE',  ( -1.522309711286088607, 0.2306618581243847221, -0.2411417322834647770 ) ) ;
#33357 = CARTESIAN_POINT ( 'NONE',  ( 0.02624671916010564918, 0.2306618581243848609, 0.2411417322834645549 ) ) ;
#33358 = CARTESIAN_POINT ( 'NONE',  ( 0.1974969037888704704, 0.3420746716998660508, -0.06364829396325460964 ) ) ;
#33359 = CARTESIAN_POINT ( 'NONE',  ( -1.587926509186350810, -0.004921259842519870586, -0.3153832671262229437 ) ) ;
#33360 = CARTESIAN_POINT ( 'NONE',  ( 0.5380577427821529035, 0.05413385826771626580, -0.4176697321401330321 ) ) ;
#33361 = CARTESIAN_POINT ( 'NONE',  ( 1.030183727034121421, -0.08942795157527998196, 0.3641732283464567121 ) ) ;
#33362 = CARTESIAN_POINT ( 'NONE',  ( 0.2314737228097724919, 1.092014648053644565, 0.2109979669470876118 ) ) ;
#33363 = CARTESIAN_POINT ( 'NONE',  ( 0.5446194225721792126, -0.2845877964562159024, 0.3641732283464567677 ) ) ;
#33364 = CARTESIAN_POINT ( 'NONE',  ( -1.069553805774277722, -0.6692913385826773087, -0.1292274648535924053 ) ) ;
#33365 = CARTESIAN_POINT ( 'NONE',  ( 0.1070741851644054776, -0.3996062992125984925, -0.9494750656167976199 ) ) ;
#33366 = CARTESIAN_POINT ( 'NONE',  ( 1.338582677165355062, -0.1870078740157479769, 0.4822834645669291653 ) ) ;
#33367 = CARTESIAN_POINT ( 'NONE',  ( 4.797336870675656522E-17, -0.3917322834645670104, -0.5433070866141732624 ) ) ;
#33369 = CARTESIAN_POINT ( 'NONE',  ( -0.6299212598425059095, 2.165354330708661568, -3.937007874015764131 ) ) ;
#33368 = CARTESIAN_POINT ( 'NONE',  ( 0.5971128608923891301, 0.2952755905511810774, -0.1292274648535930714 ) ) ;
#33370 = CARTESIAN_POINT ( 'NONE',  ( -0.7993346172249354842, -1.308147748527373767E-15, -0.3627985898453525704 ) ) ;
#33371 = CARTESIAN_POINT ( 'NONE',  ( 0.3412073490813655186, 0.1283753931104748280, 0.1820866141732283561 ) ) ;
#33372 = CARTESIAN_POINT ( 'NONE',  ( 0.6824146981627303710, -0.6046776061558807314, 0.2411417322834647770 ) ) ;
#33373 = CARTESIAN_POINT ( 'NONE',  ( 1.646981627296588035, -0.2845877964562159024, 0.3641732283464567677 ) ) ;
#33374 = CARTESIAN_POINT ( 'NONE',  ( -0.9120734908136475250, 0.1771653543307087630, 0.09757992244046791164 ) ) ;
#33375 = CARTESIAN_POINT ( 'NONE',  ( -0.9580052493438311334, -0.4281496062992124485, 0.4176697321401328655 ) ) ;
#33376 = CARTESIAN_POINT ( 'NONE',  ( -1.601049868766403650, -0.6046776061558807314, 0.2411417322834647770 ) ) ;
#33377 = CARTESIAN_POINT ( 'NONE',  ( 1.108923884514436686, -0.3162353388693409650, -0.4822834645669289433 ) ) ;
#33378 = CARTESIAN_POINT ( 'NONE',  ( 1.541994750656168645, 0.2952755905511810774, -0.1292274648535930714 ) ) ;
#33379 = DIRECTION ( 'NONE',  ( -0.000000000000000000, -1.000000000000000000, -0.000000000000000000 ) ) ;
#33380 = CARTESIAN_POINT ( 'NONE',  ( 0.7480314960629927956, -0.6692913385826771977, 8.415575281601705876E-17 ) ) ;
#33381 = CIRCLE ( 'NONE', #73714, 1.178877988035069047 ) ;
#33382 = CARTESIAN_POINT ( 'NONE',  ( 0.1265901696524989462, 0.4724409448818897572, -2.747375328083988766 ) ) ;
#33383 = CARTESIAN_POINT ( 'NONE',  ( 1.646981627296588035, -0.3162353388693405765, 0.4822834645669290543 ) ) ;
#33384 = CARTESIAN_POINT ( 'NONE',  ( 1.535433070866142558, 0.2952755905511811885, 0.000000000000000000 ) ) ;
#33385 = CARTESIAN_POINT ( 'NONE',  ( -1.358267716535432434, 0.07958543189024071263, -0.2665933059059888421 ) ) ;
#33386 = CARTESIAN_POINT ( 'NONE',  ( 1.266404199475066328, -0.2845877964562161244, -0.3641732283464567121 ) ) ;
#33387 = CARTESIAN_POINT ( 'NONE',  ( -1.115485564304461219, -0.004921259842519870586, -0.3153832671262229437 ) ) ;
#33388 = CARTESIAN_POINT ( 'NONE',  ( -0.5249343832020990641, 0.1283753931104748280, 0.1820866141732283561 ) ) ;
#33389 = ADVANCED_FACE ( 'NONE', ( #80569 ), #74172, .F. ) ;
#33390 = FACE_OUTER_BOUND ( 'NONE', #41093, .T. ) ;
#33391 = CARTESIAN_POINT ( 'NONE',  ( 1.069553805774278610, -0.5511811023622046335, 0.09757992244046803654 ) ) ;
#33392 = CARTESIAN_POINT ( 'NONE',  ( 0.7086614173228353852, -0.1870078740157479769, 0.4822834645669291653 ) ) ;
#33393 = CARTESIAN_POINT ( 'NONE',  ( 1.089238845144357537, -0.4281496062992124485, 0.4176697321401328655 ) ) ;
#33394 = CARTESIAN_POINT ( 'NONE',  ( -0.01312335958005186876, 0.05413385826771626580, -0.4176697321401330321 ) ) ;
#33395 = CARTESIAN_POINT ( 'NONE',  ( 0.4921259842519691285, 0.07958543189024085140, 0.2665933059059887866 ) ) ;
#33396 = CARTESIAN_POINT ( 'NONE',  ( 1.305774278215223960, 0.2952755905511810774, -0.1292274648535930714 ) ) ;
#33397 = CARTESIAN_POINT ( 'NONE',  ( -1.555118110236219930, -0.5400638737290845981, -0.3530559997133363437 ) ) ;
#33398 = CARTESIAN_POINT ( 'NONE',  ( -0.4199475065616791736, 0.2306618581243847221, -0.2411417322834647770 ) ) ;
#33399 = CARTESIAN_POINT ( 'NONE',  ( -0.1998031496062994683, 0.3460692066303958092, -0.8005249343832020470 ) ) ;
#33400 = CARTESIAN_POINT ( 'NONE',  ( -0.3128565372736722416, 1.393882159635214890, 0.01004378685656346325 ) ) ;
#33401 = CARTESIAN_POINT ( 'NONE',  ( 0.2230971128608929543, 0.05413385826771626580, -0.4176697321401330321 ) ) ;
#33402 = CARTESIAN_POINT ( 'NONE',  ( -0.6364829396325453192, -0.05778040916215560624, -0.4822834645669293319 ) ) ;
#33403 = CARTESIAN_POINT ( 'NONE',  ( -0.09842519685039295696, 0.1660481256975883668, -0.3530559997133364547 ) ) ;
#33404 = CARTESIAN_POINT ( 'NONE',  ( -0.2925321140481930704, -0.2925321140481933480, -2.421259842519684735 ) ) ;
#33405 = CARTESIAN_POINT ( 'NONE',  ( 0.2891555358219910499, 0.2891555358219910499, -1.870078740157480324 ) ) ;
#33406 = CARTESIAN_POINT ( 'NONE',  ( 4.797336870675656522E-17, -0.3917322834645670104, -0.7007874015748030150 ) ) ;
#33407 = CARTESIAN_POINT ( 'NONE',  ( -0.2867679344610366554, 0.2867679344610365444, -0.9566929133858265155 ) ) ;
#33408 = CARTESIAN_POINT ( 'NONE',  ( -1.003937007874015297, -0.4536011799217368745, -0.2665933059059886201 ) ) ;
#33409 = CARTESIAN_POINT ( 'NONE',  ( -0.1958661417322836718, 0.3392501089628017219, -0.9501312335958004285 ) ) ;
#33410 = CARTESIAN_POINT ( 'NONE',  ( -1.148293963254592542, -0.6692913385826773087, -0.1292274648535924053 ) ) ;
#33411 = CARTESIAN_POINT ( 'NONE',  ( -0.1958661417322836440, 0.3392501089628016664, 0.06432377772409630934 ) ) ;
#33412 = CARTESIAN_POINT ( 'NONE',  ( 0.5643044619422579178, 0.05413385826771666132, 0.4176697321401328100 ) ) ;
#33413 = CARTESIAN_POINT ( 'NONE',  ( -0.5446194225721777693, -0.2845877964562161244, -0.3641732283464567121 ) ) ;
#33414 = CARTESIAN_POINT ( 'NONE',  ( 1.423884514435696191, -0.05778040916215522460, 0.4822834645669289988 ) ) ;
#33415 = CARTESIAN_POINT ( 'NONE',  ( 0.1706036745406830368, 0.05413385826771666132, 0.4176697321401328100 ) ) ;
#33416 = CARTESIAN_POINT ( 'NONE',  ( 0.3250094633868885197, 1.191472453874008020, 1.074005115865686477 ) ) ;
#33417 = CARTESIAN_POINT ( 'NONE',  ( 0.1070741851644053527, 0.3996062992125986590, -2.513123359580052174 ) ) ;
#33418 = CARTESIAN_POINT ( 'NONE',  ( -9.594673741351313045E-17, 0.3917322834645670659, -1.414061310532495286 ) ) ;
#33419 = CARTESIAN_POINT ( 'NONE',  ( 1.049868766404200349, 0.2306618581243848609, 0.2411417322834645549 ) ) ;
#33420 = CARTESIAN_POINT ( 'NONE',  ( 0.6758530183727039509, 0.2952755905511810774, -0.1292274648535930714 ) ) ;
#33421 = MANIFOLD_SOLID_BREP ( 'Cut-Revolve1', #344 ) ;
#33422 = CARTESIAN_POINT ( 'NONE',  ( 0.2952755905511816326, -0.5400638737290844871, 0.3530559997133364547 ) ) ;
#33423 = CARTESIAN_POINT ( 'NONE',  ( 1.450131233595801428, 0.2952755905511811885, 0.1292274648535926551 ) ) ;
#33424 = CARTESIAN_POINT ( 'NONE',  ( 1.017060367454068803, -0.3162353388693405765, 0.4822834645669290543 ) ) ;
#33425 = CARTESIAN_POINT ( 'NONE',  ( 0.3917322834645670104, -0.1049643490035303411, -0.3536745406824148286 ) ) ;
#33426 = CARTESIAN_POINT ( 'NONE',  ( -0.1443569553805768291, 0.05413385826771666132, 0.4176697321401328100 ) ) ;
#33427 = CARTESIAN_POINT ( 'NONE',  ( 0.8923884514435703741, 0.2306618581243848609, 0.2411417322834645549 ) ) ;
#33428 = CARTESIAN_POINT ( 'NONE',  ( 0.4658792650918641698, -0.05778040916215560624, -0.4822834645669293319 ) ) ;
#33429 = CARTESIAN_POINT ( 'NONE',  ( 1.141732283464567788, -0.5511811023622047445, 6.969142054262312111E-17 ) ) ;
#33430 = CARTESIAN_POINT ( 'NONE',  ( -0.7742782152230965886, 0.05413385826771666132, 0.4176697321401328100 ) ) ;
#33431 = CARTESIAN_POINT ( 'NONE',  ( -1.456692913385826182, -0.6692913385826771977, 8.415575281601705876E-17 ) ) ;
#33432 = CARTESIAN_POINT ( 'NONE',  ( 0.5971128608923890191, -0.6692913385826771977, 0.1292274648535927661 ) ) ;
#33433 = CARTESIAN_POINT ( 'NONE',  ( -0.3726288332202236653, -0.1208384647423932784, -1.929133858267952473 ) ) ;
#33434 = CARTESIAN_POINT ( 'NONE',  ( 0.1958661417322836440, -0.3392501089628017219, -2.131233595800524849 ) ) ;
#33435 =( BOUNDED_CURVE ( )  B_SPLINE_CURVE ( 1, ( #65951, #39003 ),
 .UNSPECIFIED., .F., .F. ) 
 B_SPLINE_CURVE_WITH_KNOTS ( ( 2, 2 ),
 ( 1.387778780781445676E-17, 0.001999999999999991368 ),
 .UNSPECIFIED. ) 
 CURVE ( )  GEOMETRIC_REPRESENTATION_ITEM ( )  RATIONAL_B_SPLINE_CURVE ( ( 0.9875488213027535656, 0.9875488213027535656 ) ) 
 REPRESENTATION_ITEM ( '' )  );
#33436 = EDGE_LOOP ( 'NONE', ( #82901, #40573, #71620, #26355 ) ) ;
#33437 = CARTESIAN_POINT ( 'NONE',  ( 0.3996062992125986590, -0.1070741851644053111, -0.4265091863517060933 ) ) ;
#33438 = ORIENTED_EDGE ( 'NONE', *, *, #47097, .F. ) ;
#33439 = CARTESIAN_POINT ( 'NONE',  ( 1.522309711286089939, 0.2306618581243848609, 0.2411417322834645549 ) ) ;
#33440 = CARTESIAN_POINT ( 'NONE',  ( 1.017060367454068581, -0.08942795157528024563, -0.3641732283464568787 ) ) ;
#33441 = CARTESIAN_POINT ( 'NONE',  ( 0.000000000000000000, -0.09842519685039369248, 5.158493410915829266E-18 ) ) ;
#33442 = DIRECTION ( 'NONE',  ( 0.000000000000000000, 0.000000000000000000, 1.000000000000000000 ) ) ;
#33443 = CARTESIAN_POINT ( 'NONE',  ( 0.4724409448818898682, 2.892866454678787531E-17, -2.714566929133858331 ) ) ;
#33444 = CARTESIAN_POINT ( 'NONE',  ( 0.2867679344610365999, 0.2867679344610365999, -1.009842519685039353 ) ) ;
#33445 = CARTESIAN_POINT ( 'NONE',  ( 1.115485564304462551, 0.05413385826771666132, 0.4176697321401328100 ) ) ;
#33446 = CARTESIAN_POINT ( 'NONE',  ( -0.3790285851608742318, -0.1011035889004742866, -1.929133858267716439 ) ) ;
#33447 = CARTESIAN_POINT ( 'NONE',  ( -0.4724409448818890911, -0.1870078740157479769, 0.4822834645669291653 ) ) ;
#33448 = CARTESIAN_POINT ( 'NONE',  ( 0.9908136482939640111, 0.2952755905511810774, -0.1292274648535930714 ) ) ;
#33449 = ORIENTED_EDGE ( 'NONE', *, *, #19165, .T. ) ;
#33450 = CARTESIAN_POINT ( 'NONE',  ( -1.640419947506561060, -0.4281496062992127816, -0.4176697321401328100 ) ) ;
#33451 = CARTESIAN_POINT ( 'NONE',  ( -1.038399629478160113, 1.326389387685770638, -0.4251810372651388392 ) ) ;
#33452 = DIRECTION ( 'NONE',  ( -1.000000000000000000, -3.096699300667737464E-16, 1.692413147294446216E-16 ) ) ;
#33453 = CARTESIAN_POINT ( 'NONE',  ( 2.795275590551181910, 1.726086921369709426, 0.000000000000000000 ) ) ;
#33454 = CARTESIAN_POINT ( 'NONE',  ( -0.9251968503937002541, -0.4536011799217368745, -0.2665933059059886201 ) ) ;
#33455 = CARTESIAN_POINT ( 'NONE',  ( 0.8989501312335963501, 0.2066929133858267931, 0.1054918080437490802 ) ) ;
#33456 = CARTESIAN_POINT ( 'NONE',  ( 0.4068241469816281097, 0.05413385826771666132, 0.4176697321401328100 ) ) ;
#33457 = ORIENTED_EDGE ( 'NONE', *, *, #82059, .T. ) ;
#33459 = CARTESIAN_POINT ( 'NONE',  ( -1.614173228346456712, 1.543375672658095610, -0.1372047244094478091 ) ) ;
#33458 = CARTESIAN_POINT ( 'NONE',  ( -0.5314960629921194890, 2.729653112167212736, -1.868118600003770391 ) ) ;
#33460 = CARTESIAN_POINT ( 'NONE',  ( 1.003937007874016407, -0.5400638737290844871, 0.3530559997133364547 ) ) ;
#33461 = CARTESIAN_POINT ( 'NONE',  ( -1.725721784776902190, -0.05778040916215522460, 0.4822834645669289988 ) ) ;
#33462 = CARTESIAN_POINT ( 'NONE',  ( 0.2867679344610365999, -0.2867679344610365999, -0.9658599493100242794 ) ) ;
#33463 = CARTESIAN_POINT ( 'NONE',  ( -0.7742782152230965886, -0.004921259842519576551, 0.3153832671262227771 ) ) ;
#33464 = CARTESIAN_POINT ( 'NONE',  ( 1.666666666666667185, 0.05413385826771666132, 0.4176697321401328100 ) ) ;
#33465 = CARTESIAN_POINT ( 'NONE',  ( -0.3392501089628019995, 0.1958661417322832277, -1.213254593175852936 ) ) ;
#33466 = CARTESIAN_POINT ( 'NONE',  ( 0.2624671916010504757, -0.6046776061558809534, -0.2411417322834644161 ) ) ;
#33467 = CARTESIAN_POINT ( 'NONE',  ( -0.8595800524934373854, -0.08942795157527998196, 0.3641732283464567121 ) ) ;
#33468 = CARTESIAN_POINT ( 'NONE',  ( 0.1181102362204730916, -0.5511811023622047445, 6.969142054262312111E-17 ) ) ;
#33469 = CARTESIAN_POINT ( 'NONE',  ( -0.3805774278215216522, -0.4281496062992127816, -0.4176697321401328100 ) ) ;
#33470 = CARTESIAN_POINT ( 'NONE',  ( -1.108923884514435132, -0.08942795157528024563, -0.3641732283464568787 ) ) ;
#33471 = CARTESIAN_POINT ( 'NONE',  ( 0.2867679344610366554, -0.2867679344610365999, 0.06231664222341019160 ) ) ;
#33472 = CARTESIAN_POINT ( 'NONE',  ( 0.6233595800524939223, -0.3162353388693405765, 0.4822834645669290543 ) ) ;
#33473 = ADVANCED_FACE ( 'NONE', ( #2702 ), #41413, .F. ) ;
#33474 = CARTESIAN_POINT ( 'NONE',  ( -1.627296587926508442, 0.2306618581243848609, 0.2411417322834645549 ) ) ;
#33475 = CARTESIAN_POINT ( 'NONE',  ( 0.3458507752293908943, -0.3458507752293908943, -1.435039370078740051 ) ) ;
#33476 = CARTESIAN_POINT ( 'NONE',  ( -0.7480314960629914633, 0.2952755905511811885, 0.000000000000000000 ) ) ;
#33477 = CARTESIAN_POINT ( 'NONE',  ( -0.02624671916010428221, -0.5023911411419708095, 0.1820866141732285504 ) ) ;
#33478 = CARTESIAN_POINT ( 'NONE',  ( -1.194225721784776262, -0.4281496062992124485, 0.4176697321401328655 ) ) ;
#33479 = CARTESIAN_POINT ( 'NONE',  ( 1.023622047244095334, -0.1870078740157479769, 0.3641732283464567677 ) ) ;
#33480 = CARTESIAN_POINT ( 'NONE',  ( -0.6102362204724400829, 0.07958543189024085140, 0.2665933059059887866 ) ) ;
#33481 = CARTESIAN_POINT ( 'NONE',  ( -0.9514435695538050464, -0.3162353388693405765, 0.4822834645669290543 ) ) ;
#33482 = CARTESIAN_POINT ( 'NONE',  ( -1.089238845144356427, 0.05413385826771666132, 0.4176697321401328100 ) ) ;
#33483 = CARTESIAN_POINT ( 'NONE',  ( -1.601049868766403650, 0.2306618581243847221, -0.2411417322834647770 ) ) ;
#33485 = EDGE_CURVE ( 'NONE', #37547, #63414, #54024, .T. ) ;
#33484 = CYLINDRICAL_SURFACE ( 'NONE', #58187, 0.4744094488188972947 ) ;
#33486 = CARTESIAN_POINT ( 'NONE',  ( 0.9514435695538062676, -0.2845877964562161244, -0.3641732283464567121 ) ) ;
#33487 = CARTESIAN_POINT ( 'NONE',  ( 0.4790026246719168435, -0.3162353388693409650, -0.4822834645669289433 ) ) ;
#33488 = CARTESIAN_POINT ( 'NONE',  ( -1.332020997375327642, -0.05778040916215522460, 0.4822834645669289988 ) ) ;
#33489 = CARTESIAN_POINT ( 'NONE',  ( -1.476377952755905110, -0.5400638737290845981, -0.3530559997133363437 ) ) ;
#33490 = ORIENTED_EDGE ( 'NONE', *, *, #48506, .T. ) ;
#33491 = CARTESIAN_POINT ( 'NONE',  ( -0.2891555358219911054, 0.2891555358219909388, 0.2185039370078739884 ) ) ;
#33492 = CARTESIAN_POINT ( 'NONE',  ( -1.423884514435694859, -0.08942795157528024563, -0.3641732283464568787 ) ) ;
#33493 = CARTESIAN_POINT ( 'NONE',  ( 0.5511811023622054106, -0.1870078740157480879, -0.4822834645669291653 ) ) ;
#33494 = CARTESIAN_POINT ( 'NONE',  ( -1.266404199475064773, -0.2845877964562159024, 0.3641732283464567677 ) ) ;
#33495 = CARTESIAN_POINT ( 'NONE',  ( 0.3996062992125986035, -0.1070741851644052972, -1.763123359580052174 ) ) ;
#33496 = CARTESIAN_POINT ( 'NONE',  ( -1.404199475065615932, 0.05413385826771666132, 0.4176697321401328100 ) ) ;
#33497 = CARTESIAN_POINT ( 'NONE',  ( 0.8989501312335964611, 0.2952755905511811885, 0.1292274648535926551 ) ) ;
#33498 = CARTESIAN_POINT ( 'NONE',  ( 0.6496062992125991586, -0.5400638737290845981, -0.3530559997133363437 ) ) ;
#33499 = CARTESIAN_POINT ( 'NONE',  ( 1.358267716535433323, -0.5400638737290845981, -0.3530559997133363437 ) ) ;
#33500 = CARTESIAN_POINT ( 'NONE',  ( 0.2925321140481931814, 0.2925321140481931814, -1.001968503937007871 ) ) ;
#33501 = CARTESIAN_POINT ( 'NONE',  ( 0.2925321140481932369, 0.2925321140481932369, -1.397637795275590067 ) ) ;
#33502 = CARTESIAN_POINT ( 'NONE',  ( -0.3420746716998661618, 0.1974969037888702206, -0.6561679790026245795 ) ) ;
#33503 = DIRECTION ( 'NONE',  ( 0.000000000000000000, -0.7071067811865462405, -0.7071067811865486830 ) ) ;
#33504 = CARTESIAN_POINT ( 'NONE',  ( 0.5118110236220478892, 0.1771653543307087630, 0.000000000000000000 ) ) ;
#33505 = CARTESIAN_POINT ( 'NONE',  ( 0.1443569553805781891, -0.4281496062992124485, 0.4176697321401328655 ) ) ;
#33506 = CARTESIAN_POINT ( 'NONE',  ( 1.456692913385827515, 0.2952755905511811885, 0.000000000000000000 ) ) ;
#33507 = CARTESIAN_POINT ( 'NONE',  ( -0.2891555358219909388, -0.2891555358219912164, -1.553149606299212504 ) ) ;
#33508 = CARTESIAN_POINT ( 'NONE',  ( 0.1902887139107617975, -0.5511811023622048555, -0.09757992244046775898 ) ) ;
#33509 = CARTESIAN_POINT ( 'NONE',  ( -0.7283464566929126471, -0.5400638737290844871, 0.3530559997133364547 ) ) ;
#33510 = CARTESIAN_POINT ( 'NONE',  ( 1.607611548556431069, 0.2952755905511811885, 0.1292274648535926551 ) ) ;
#33511 = CARTESIAN_POINT ( 'NONE',  ( 0.3805774278215230400, -0.4281496062992124485, 0.4176697321401328655 ) ) ;
#33512 = CARTESIAN_POINT ( 'NONE',  ( -0.2362204724409447953, -0.4091458600556404646, -2.112860892388451539 ) ) ;
#33513 = CARTESIAN_POINT ( 'NONE',  ( 0.6299212598425337761, 2.755905511811024056, -3.886287458032460229 ) ) ;
#33514 = ORIENTED_EDGE ( 'NONE', *, *, #82040, .F. ) ;
#33515 = EDGE_LOOP ( 'NONE', ( #34985, #59531, #82567, #54018, #61967, #66798, #34882, #32270 ) ) ;
#33516 = CARTESIAN_POINT ( 'NONE',  ( -1.187664041994750175, -0.05778040916215560624, -0.4822834645669293319 ) ) ;
#33518 = CARTESIAN_POINT ( 'NONE',  ( -1.056430446194224881, -0.6692913385826771977, 0.1292274648535927661 ) ) ;
#33517 = CARTESIAN_POINT ( 'NONE',  ( -1.240157480314959759, -0.4536011799217368745, -0.2665933059059886201 ) ) ;
#33519 = CARTESIAN_POINT ( 'NONE',  ( 0.2867679344610365999, -0.2867679344610365999, -2.540663098916323914 ) ) ;
#33520 = CARTESIAN_POINT ( 'NONE',  ( -0.4621018179204942067, -4.378520898609941727E-15, 0.4281989832122470863 ) ) ;
#33521 = CARTESIAN_POINT ( 'NONE',  ( 1.574803149606299746, -0.1870078740157480879, -0.4822834645669291653 ) ) ;
#33522 = CARTESIAN_POINT ( 'NONE',  ( -1.227034120734907585, 0.2952755905511811885, 0.1292274648535926551 ) ) ;
#33523 = CARTESIAN_POINT ( 'NONE',  ( 0.4199475065616803948, -0.6046776061558809534, -0.2411417322834644161 ) ) ;
#33524 = CARTESIAN_POINT ( 'NONE',  ( -1.325459317585300889, 0.05413385826771666132, 0.4176697321401328100 ) ) ;
#33525 = CARTESIAN_POINT ( 'NONE',  ( -0.2867679344610365999, 0.2867679344610364889, 0.2106299212598424508 ) ) ;
#33526 = CARTESIAN_POINT ( 'NONE',  ( 0.8267716535433077274, 0.2952755905511811885, 0.000000000000000000 ) ) ;
#33527 = CARTESIAN_POINT ( 'NONE',  ( 0.1958661417322836440, -0.3392501089628017219, -1.973753280839895208 ) ) ;
#33528 = CARTESIAN_POINT ( 'NONE',  ( -1.135170603674539924, 0.1771653543307087075, -0.09757992244046823083 ) ) ;
#33529 = EDGE_LOOP ( 'NONE', ( #7953, #15431, #72647, #52365 ) ) ;
#33530 = CARTESIAN_POINT ( 'NONE',  ( 0.3420746716998659953, 0.1974969037888705536, -1.863517060367453793 ) ) ;
#33531 = ORIENTED_EDGE ( 'NONE', *, *, #70994, .T. ) ;
#33532 = CARTESIAN_POINT ( 'NONE',  ( -0.6402603868039137280, -5.134928753749862370E-15, -0.4281989832122467532 ) ) ;
#33533 = CARTESIAN_POINT ( 'NONE',  ( -0.9842519685039365918, -0.6692913385826771977, 8.415575281601705876E-17 ) ) ;
#33534 = CARTESIAN_POINT ( 'NONE',  ( -1.259842519685038686, -0.1870078740157480879, -0.4822834645669291653 ) ) ;
#33535 = CARTESIAN_POINT ( 'NONE',  ( 0.3460692066303959202, 0.1998031496062993295, -0.7611548556430446366 ) ) ;
#33536 = CARTESIAN_POINT ( 'NONE',  ( -1.469816272965878357, -0.6046776061558809534, -0.2411417322834644161 ) ) ;
#33537 = CARTESIAN_POINT ( 'NONE',  ( -1.699475065616797398, 0.2952755905511811885, 0.1292274648535926551 ) ) ;
#33538 = CARTESIAN_POINT ( 'NONE',  ( -1.404199475065615932, -0.4281496062992127816, -0.4176697321401328100 ) ) ;
#33539 = CARTESIAN_POINT ( 'NONE',  ( -1.586052503253846169, 1.850393700787402729, 0.1653254495020583248 ) ) ;
#33540 = LINE ( 'NONE', #33122, #14688 ) ;
#33541 = CARTESIAN_POINT ( 'NONE',  ( -0.03937007874015669567, 0.1771653543307087630, 0.000000000000000000 ) ) ;
#33542 = CARTESIAN_POINT ( 'NONE',  ( 0.4734416007054343400, 1.572145545125848587, 2.167714792466635565 ) ) ;
#33543 = CARTESIAN_POINT ( 'NONE',  ( -0.1958661417322834220, -0.3392501089628018884, -0.4652230971128609727 ) ) ;
#33544 = CARTESIAN_POINT ( 'NONE',  ( -0.2296587926509179312, -0.2845877964562161244, -0.3641732283464567121 ) ) ;
#33545 = CARTESIAN_POINT ( 'NONE',  ( -0.7874015748031489847, -0.1870078740157480879, -0.4822834645669291653 ) ) ;
#33546 = CARTESIAN_POINT ( 'NONE',  ( 1.128608923884514947, 0.2306618581243848609, 0.2411417322834645549 ) ) ;
#33547 = CARTESIAN_POINT ( 'NONE',  ( -0.8398950131233585692, 0.2306618581243848609, 0.2411417322834645549 ) ) ;
#33548 = ORIENTED_EDGE ( 'NONE', *, *, #405, .F. ) ;
#33549 = VERTEX_POINT ( 'NONE', #48132 ) ;
#33550 = CARTESIAN_POINT ( 'NONE',  ( -0.8267716535433065062, 0.2952755905511811885, 0.000000000000000000 ) ) ;
#33551 = CARTESIAN_POINT ( 'NONE',  ( 0.7020997375328090762, -0.05778040916215560624, -0.4822834645669293319 ) ) ;
#33552 = CARTESIAN_POINT ( 'NONE',  ( -1.535433070866141225, 0.1771653543307087630, 0.000000000000000000 ) ) ;
#33553 = CARTESIAN_POINT ( 'NONE',  ( 0.4724409448818898682, 2.892866454678787531E-17, -1.062992125984252079 ) ) ;
#33554 = CARTESIAN_POINT ( 'NONE',  ( -2.161121219943175742, 1.597527518877485786, 0.4706608522957222984 ) ) ;
#33555 = CARTESIAN_POINT ( 'NONE',  ( 0.2867679344610365999, 0.2867679344610365999, -0.2874015748031494843 ) ) ;
#33556 = CARTESIAN_POINT ( 'NONE',  ( 0.3917322834645670104, 2.398668435337828261E-17, -2.407480314960630086 ) ) ;
#33557 = CARTESIAN_POINT ( 'NONE',  ( -0.2821522309711278487, -0.6692913385826773087, -0.1292274648535924053 ) ) ;
#33558 = CARTESIAN_POINT ( 'NONE',  ( -1.286089238845143479, 0.1283753931104746893, -0.1820866141732285504 ) ) ;
#33559 = CARTESIAN_POINT ( 'NONE',  ( -0.8070866141732276899, -0.5400638737290844871, 0.3530559997133364547 ) ) ;
#33560 = CARTESIAN_POINT ( 'NONE',  ( -0.3996062992125986590, 0.1070741851644051723, -0.1095800524934383291 ) ) ;
#33562 = CARTESIAN_POINT ( 'NONE',  ( 0.4330708661417324024, 2.793565526369266028, 0.000000000000000000 ) ) ;
#33561 = CARTESIAN_POINT ( 'NONE',  ( -1.469816272965878357, -0.6046776061558809534, -0.2411417322834644161 ) ) ;
#33563 = CARTESIAN_POINT ( 'NONE',  ( -1.568241469816272105, -0.05778040916215522460, 0.4822834645669289988 ) ) ;
#33564 = CARTESIAN_POINT ( 'NONE',  ( -0.4396325459317579898, 0.2952755905511811885, 0.1292274648535926551 ) ) ;
#33565 = CARTESIAN_POINT ( 'NONE',  ( -0.3420746716998662729, 0.1974969037888702206, -2.780183727034121866 ) ) ;
#33566 = CARTESIAN_POINT ( 'NONE',  ( 0.5708661417322841158, -0.4536011799217368745, -0.2665933059059886201 ) ) ;
#33567 = FACE_OUTER_BOUND ( 'NONE', #34132, .T. ) ;
#33568 = CARTESIAN_POINT ( 'NONE',  ( 0.2624671916010504757, 0.1283753931104748280, 0.1820866141732283561 ) ) ;
#33569 = CARTESIAN_POINT ( 'NONE',  ( 1.253280839895013710, -0.2845877964562159024, 0.3641732283464567677 ) ) ;
#33570 = CARTESIAN_POINT ( 'NONE',  ( 1.141732283464567566, 0.2952755905511811885, 0.000000000000000000 ) ) ;
#33571 = CARTESIAN_POINT ( 'NONE',  ( 0.2559055118110243332, 0.07958543189024085140, 0.2665933059059887866 ) ) ;
#33572 = CARTESIAN_POINT ( 'NONE',  ( 0.3917322834645670104, 2.398668435337828261E-17, -1.842519685039370136 ) ) ;
#33573 = CARTESIAN_POINT ( 'NONE',  ( -1.463254593175852492, 0.2952755905511811885, 0.1292274648535926551 ) ) ;
#33574 = CARTESIAN_POINT ( 'NONE',  ( 0.01968503937007930540, 0.07958543189024085140, 0.2665933059059887866 ) ) ;
#33575 = CARTESIAN_POINT ( 'NONE',  ( -0.4724409448818898682, -8.678599364036362592E-17, -0.1161417322834645827 ) ) ;
#33576 = CARTESIAN_POINT ( 'NONE',  ( -0.5511811023622038563, -0.1870078740157479769, 0.3641732283464567677 ) ) ;
#33577 = CARTESIAN_POINT ( 'NONE',  ( -0.4485632242333278397, 1.695109487299527817, -1.028575266362750096 ) ) ;
#33578 = CARTESIAN_POINT ( 'NONE',  ( -0.3018372703412066094, -0.4281496062992127816, -0.4176697321401328100 ) ) ;
#33579 = DIRECTION ( 'NONE',  ( 0.000000000000000000, 0.000000000000000000, -1.000000000000000000 ) ) ;
#33580 = CARTESIAN_POINT ( 'NONE',  ( 1.056430446194226436, -0.5511811023622048555, -0.09757992244046775898 ) ) ;
#33581 = CARTESIAN_POINT ( 'NONE',  ( -0.2034120734908131112, -0.5511811023622048555, -0.09757992244046775898 ) ) ;
#33582 = CARTESIAN_POINT ( 'NONE',  ( -0.2559055118110227234, -0.5400638737290844871, 0.3530559997133364547 ) ) ;
#33583 = DIRECTION ( 'NONE',  ( 1.445602896647338917E-16, 1.000000000000000000, 0.000000000000000000 ) ) ;
#33584 = CARTESIAN_POINT ( 'NONE',  ( -0.9317585301837263412, -0.3690944881889765550, -0.3153832671262227771 ) ) ;
#33585 = PLANE ( 'NONE',  #42163 ) ;
#33586 = CARTESIAN_POINT ( 'NONE',  ( 0.7611548556430454138, 0.2306618581243847221, -0.2411417322834647770 ) ) ;
#33587 = CARTESIAN_POINT ( 'NONE',  ( -0.8989501312335946848, -0.6692913385826771977, 0.1292274648535927661 ) ) ;
#33588 = CARTESIAN_POINT ( 'NONE',  ( 4.893765752498283308E-17, -0.3996062992125985480, -0.9429133858267716439 ) ) ;
#33589 = CARTESIAN_POINT ( 'NONE',  ( 4.797336870675656522E-17, -0.3917322834645670104, -2.840551181102362044 ) ) ;
#33590 = CARTESIAN_POINT ( 'NONE',  ( 0.04593175853018440641, 0.1771653543307087075, -0.09757992244046823083 ) ) ;
#33591 = CARTESIAN_POINT ( 'NONE',  ( -0.7742782152230962556, -0.4281496062992127816, -0.4176697321401328100 ) ) ;
#33592 = CARTESIAN_POINT ( 'NONE',  ( -1.108923884514435132, -0.05778040916215560624, -0.4822834645669293319 ) ) ;
#33593 = CARTESIAN_POINT ( 'NONE',  ( -1.391076115485563314, -0.5023911411419708095, -0.1820866141732282451 ) ) ;
#33594 = CARTESIAN_POINT ( 'NONE',  ( 1.620734908136483465, -0.6692913385826771977, 0.1292274648535927661 ) ) ;
#33595 = CARTESIAN_POINT ( 'NONE',  ( -1.076115485564303809, -0.5023911411419708095, -0.1820866141732282451 ) ) ;
#33596 = CARTESIAN_POINT ( 'NONE',  ( -0.7217847769028863381, 0.009842519685039144428, -0.3409548833797004797 ) ) ;
#33597 = CARTESIAN_POINT ( 'NONE',  ( 0.7414698162729663755, -0.6692913385826773087, -0.1292274648535924053 ) ) ;
#33598 = CARTESIAN_POINT ( 'NONE',  ( 0.1998031496062992740, 0.3460692066303959757, -0.1443569553805774397 ) ) ;
#33599 = CARTESIAN_POINT ( 'NONE',  ( -9.594673741351313045E-17, 0.3917322834645670659, -2.673903830217533972 ) ) ;
#33600 = ORIENTED_EDGE ( 'NONE', *, *, #27842, .F. ) ;
#33601 = FACE_OUTER_BOUND ( 'NONE', #18834, .T. ) ;
#33602 = EDGE_CURVE ( 'NONE', #38567, #30834, #48611, .T. ) ;
#33603 = CARTESIAN_POINT ( 'NONE',  ( 1.489501312335958172, -0.08942795157528024563, -0.3641732283464568787 ) ) ;
#33604 = CARTESIAN_POINT ( 'NONE',  ( -1.305774278215222184, -0.6692913385826773087, -0.1292274648535924053 ) ) ;
#33605 = CARTESIAN_POINT ( 'NONE',  ( 1.174540682414699111, -0.05778040916215560624, -0.4822834645669293319 ) ) ;
#33606 = CARTESIAN_POINT ( 'NONE',  ( 0.3917322834645670104, 2.398668435337828261E-17, -2.564960629921259727 ) ) ;
#33607 = CARTESIAN_POINT ( 'NONE',  ( 1.515748031496063408, 0.07958543189024085140, 0.2665933059059887866 ) ) ;
#33608 = EDGE_CURVE ( 'NONE', #78998, #41007, #78903, .T. ) ;
#33609 = CARTESIAN_POINT ( 'NONE',  ( 0.7283464566929143125, 0.1660481256975885056, 0.3530559997133364547 ) ) ;
#33610 = CARTESIAN_POINT ( 'NONE',  ( -0.3608923884514428360, 0.2952755905511811885, 0.1292274648535926551 ) ) ;
#33611 = CARTESIAN_POINT ( 'NONE',  ( 0.1229985535008144004, 1.078950944086593200, -3.935114172421038337 ) ) ;
#33612 = CARTESIAN_POINT ( 'NONE',  ( 3.826707563893392283, 2.755905511811024500, 0.5314960629921261503 ) ) ;
#33613 = CARTESIAN_POINT ( 'NONE',  ( 0.6167979002624678353, -0.3690944881889763329, 0.3153832671262228327 ) ) ;
#33614 = CARTESIAN_POINT ( 'NONE',  ( -0.1070741851644056997, 0.3996062992125986035, -1.738845144356955696 ) ) ;
#33615 = ORIENTED_EDGE ( 'NONE', *, *, #54690, .T. ) ;
#33616 = CARTESIAN_POINT ( 'NONE',  ( -0.1958661417322833942, -0.3392501089628018884, -0.5347962186689783071 ) ) ;
#33617 = VERTEX_POINT ( 'NONE', #34272 ) ;
#33618 = CARTESIAN_POINT ( 'NONE',  ( 0.01312335958005323398, 0.05413385826771666132, 0.4176697321401328100 ) ) ;
#33619 = CARTESIAN_POINT ( 'NONE',  ( 1.253280839895013710, -0.3162353388693405765, 0.4822834645669290543 ) ) ;
#33620 = CARTESIAN_POINT ( 'NONE',  ( 0.2493438320209980519, 0.05413385826771666132, 0.4176697321401328100 ) ) ;
#33621 = CARTESIAN_POINT ( 'NONE',  ( -0.1640419947506553400, -0.08942795157528024563, -0.3641732283464568787 ) ) ;
#33622 = CARTESIAN_POINT ( 'NONE',  ( 1.220472440944882608, 0.2952755905511811885, 0.000000000000000000 ) ) ;
#33623 = CARTESIAN_POINT ( 'NONE',  ( -0.5971128608923877978, -0.6692913385826773087, -0.1292274648535924053 ) ) ;
#33624 = CARTESIAN_POINT ( 'NONE',  ( -0.1377952755905504645, 0.1660481256975885056, 0.3530559997133364547 ) ) ;
#33625 = CARTESIAN_POINT ( 'NONE',  ( -1.587926509186350810, 0.05413385826771626580, -0.4176697321401330321 ) ) ;
#33626 = CARTESIAN_POINT ( 'NONE',  ( 1.450131233595801428, 0.2952755905511811885, 0.1292274648535926551 ) ) ;
#33627 = CARTESIAN_POINT ( 'NONE',  ( 1.181102362204725198, -0.1870078740157479769, 0.4822834645669291653 ) ) ;
#33628 = EDGE_CURVE ( 'NONE', #2588, #19450, #72120, .T. ) ;
#33629 = CARTESIAN_POINT ( 'NONE',  ( -0.3917322834645671215, 0.1049643490035301469, -0.6548556430446192955 ) ) ;
#33630 = CARTESIAN_POINT ( 'NONE',  ( 0.4855643044619430415, -0.3690944881889765550, -0.3153832671262227771 ) ) ;
#33631 = ORIENTED_EDGE ( 'NONE', *, *, #18554, .T. ) ;
#33632 = CARTESIAN_POINT ( 'NONE',  ( -0.3949938075777411628, 0.1058382717557497937, -0.8202099737532810853 ) ) ;
#33633 = ORIENTED_EDGE ( 'NONE', *, *, #36412, .F. ) ;
#33634 = CARTESIAN_POINT ( 'NONE',  ( -0.5118110236220466680, -0.5511811023622047445, 6.969142054262312111E-17 ) ) ;
#33635 = CARTESIAN_POINT ( 'NONE',  ( -0.2427821522309703550, -0.3162353388693405765, 0.4822834645669290543 ) ) ;
#33636 = CARTESIAN_POINT ( 'NONE',  ( 2.777177547361622256, 1.169463170161816779, 0.3010181502270526388 ) ) ;
#33637 = CARTESIAN_POINT ( 'NONE',  ( -0.1443569553805768291, 0.05413385826771666132, 0.4176697321401328100 ) ) ;
#33638 = CARTESIAN_POINT ( 'NONE',  ( -0.06561679790026180015, -0.4281496062992127816, -0.4176697321401328100 ) ) ;
#33639 = EDGE_CURVE ( 'NONE', #28101, #65196, #80978, .T. ) ;
#33640 = CARTESIAN_POINT ( 'NONE',  ( -0.9251968503937002541, -0.5400638737290845981, -0.3530559997133363437 ) ) ;
#33641 = CARTESIAN_POINT ( 'NONE',  ( -0.9251968503937002541, 0.1660481256975885056, 0.3530559997133364547 ) ) ;
#33642 = CARTESIAN_POINT ( 'NONE',  ( 1.161417322834646493, -0.4536011799217367080, 0.2665933059059888421 ) ) ;
#33643 = CARTESIAN_POINT ( 'NONE',  ( -1.555118110236219930, -0.5400638737290845981, -0.3530559997133363437 ) ) ;
#33644 = CARTESIAN_POINT ( 'NONE',  ( -0.1467811222005243055, -2.624320362099288585E-15, 0.4118477457933001906 ) ) ;
#33645 = CARTESIAN_POINT ( 'NONE',  ( 0.8792650918635177559, -0.3690944881889765550, -0.3153832671262227771 ) ) ;
#33646 = CARTESIAN_POINT ( 'NONE',  ( 0.4986876640419954376, -0.6046776061558809534, -0.2411417322834644161 ) ) ;
#33647 = CARTESIAN_POINT ( 'NONE',  ( 0.3608923884514443348, -0.6692913385826771977, 0.1292274648535927661 ) ) ;
#33648 = CARTESIAN_POINT ( 'NONE',  ( -0.3996062992125986035, -0.1070741851644056997, -1.148293963254592986 ) ) ;
#33649 = CARTESIAN_POINT ( 'NONE',  ( -1.646981627296586703, -0.3162353388693409650, -0.4822834645669289433 ) ) ;
#33650 = CARTESIAN_POINT ( 'NONE',  ( -0.3996062992125984925, -0.1070741851644056858, -0.9101049868766404316 ) ) ;
#33651 = CARTESIAN_POINT ( 'NONE',  ( -0.3996062992125986590, 0.1070741851644051723, -0.5820209973753280863 ) ) ;
#33652 = CARTESIAN_POINT ( 'NONE',  ( -0.7152230971128602510, -0.05778040916215560624, -0.4822834645669293319 ) ) ;
#33653 = CARTESIAN_POINT ( 'NONE',  ( -1.157146581871515012E-16, 0.4724409448818898682, -0.1574803149606299191 ) ) ;
#33654 = CARTESIAN_POINT ( 'NONE',  ( -0.3917322834645670104, -7.196005306013484475E-17, -2.013779527559055094 ) ) ;
#33655 = CARTESIAN_POINT ( 'NONE',  ( -1.213910761154854745, -0.5511811023622046335, 0.09757992244046803654 ) ) ;
#33656 = CARTESIAN_POINT ( 'NONE',  ( 0.9711286089238851948, 0.2306618581243848609, 0.2411417322834645549 ) ) ;
#33657 = CARTESIAN_POINT ( 'NONE',  ( 0.9514435695538062676, -0.3162353388693409650, -0.4822834645669289433 ) ) ;
#33658 = CARTESIAN_POINT ( 'NONE',  ( -0.1246719160104980823, -0.5511811023622048555, -0.09757992244046775898 ) ) ;
#33659 = CARTESIAN_POINT ( 'NONE',  ( 0.5511811023622054106, -0.1870078740157480879, -0.4822834645669291653 ) ) ;
#33660 = CARTESIAN_POINT ( 'NONE',  ( -0.4724409448818895907, -0.1265901696524993070, -2.012467191601049699 ) ) ;
#33661 = CARTESIAN_POINT ( 'NONE',  ( 0.07874015748031558404, -0.1870078740157479769, 0.3641732283464567677 ) ) ;
#33662 = CARTESIAN_POINT ( 'NONE',  ( -0.05905511811023545637, -0.5400638737290845981, -0.3530559997133363437 ) ) ;
#33664 = CIRCLE ( 'NONE', #59179, 3.937007874015748143 ) ;
#33663 = CARTESIAN_POINT ( 'NONE',  ( -0.1974969037888704149, -0.3420746716998661063, -1.559711286089239035 ) ) ;
#33665 = CARTESIAN_POINT ( 'NONE',  ( -1.679790026246718693, 0.2306618581243847221, -0.2411417322834647770 ) ) ;
#33666 = CARTESIAN_POINT ( 'NONE',  ( 0.6167979002624678353, -0.3690944881889763329, 0.3153832671262228327 ) ) ;
#33667 = CARTESIAN_POINT ( 'NONE',  ( 1.568241469816273659, -0.08942795157528024563, -0.3641732283464568787 ) ) ;
#33668 = CARTESIAN_POINT ( 'NONE',  ( -0.5708661417322828946, 0.1660481256975883668, -0.3530559997133364547 ) ) ;
#33669 = CARTESIAN_POINT ( 'NONE',  ( -0.1902887139107604098, 0.1771653543307087075, -0.09757992244046823083 ) ) ;
#33670 = DIRECTION ( 'NONE',  ( 0.000000000000000000, 0.000000000000000000, -1.000000000000000000 ) ) ;
#33671 = CARTESIAN_POINT ( 'NONE',  ( -0.7677165354330699465, 0.1660481256975885056, 0.3530559997133364547 ) ) ;
#33672 = CARTESIAN_POINT ( 'NONE',  ( -0.8005249343832011588, 0.05413385826771626580, -0.4176697321401330321 ) ) ;
#33673 = CARTESIAN_POINT ( 'NONE',  ( -0.1312335958005241554, -0.6046776061558809534, -0.2411417322834644161 ) ) ;
#33674 = CARTESIAN_POINT ( 'NONE',  ( 0.2925321140481932369, -0.2925321140481931814, -2.379921259842520342 ) ) ;
#33675 = CARTESIAN_POINT ( 'NONE',  ( -0.1958661417322834497, -0.3392501089628018884, -2.035413755084302778 ) ) ;
#33676 = CARTESIAN_POINT ( 'NONE',  ( -1.666666666666665853, -0.004921259842519870586, -0.3153832671262229437 ) ) ;
#33677 = CARTESIAN_POINT ( 'NONE',  ( 0.5577427821522316087, -0.08942795157527998196, 0.3641732283464567121 ) ) ;
#33678 = CARTESIAN_POINT ( 'NONE',  ( 1.404199475065617264, -0.4281496062992124485, 0.4176697321401328655 ) ) ;
#33679 = CARTESIAN_POINT ( 'NONE',  ( -0.7020997375328076329, -0.2845877964562161244, -0.3641732283464567121 ) ) ;
#33680 = CARTESIAN_POINT ( 'NONE',  ( -1.135170603674539924, -0.5511811023622046335, 0.09757992244046803654 ) ) ;
#33681 = CARTESIAN_POINT ( 'NONE',  ( -0.8070866141732276899, 0.1660481256975883668, -0.3530559997133364547 ) ) ;
#33682 = CARTESIAN_POINT ( 'NONE',  ( -0.6758530183727028406, -0.6692913385826773087, -0.1292274648535924053 ) ) ;
#33683 = CARTESIAN_POINT ( 'NONE',  ( 0.4461942257217856311, 0.1283753931104746893, -0.1820866141732285504 ) ) ;
#33684 = CARTESIAN_POINT ( 'NONE',  ( -0.2396931915125568024, 0.1724440681141642395, 5.660914615074364775 ) ) ;
#33685 = CARTESIAN_POINT ( 'NONE',  ( 1.095800524934383846, -0.2845877964562159024, 0.3641732283464567677 ) ) ;
#33686 = EDGE_CURVE ( 'NONE', #30580, #81796, #43913, .T. ) ;
#33687 = CARTESIAN_POINT ( 'NONE',  ( 0.3412073490813655186, -0.6046776061558809534, -0.2411417322834644161 ) ) ;
#33688 = CARTESIAN_POINT ( 'NONE',  ( -0.1998031496062991630, -0.3460692066303959202, 0.01509186351706036204 ) ) ;
#33689 = CARTESIAN_POINT ( 'NONE',  ( -0.5380577427821514602, -0.4281496062992127816, -0.4176697321401328100 ) ) ;
#33690 = CARTESIAN_POINT ( 'NONE',  ( -0.1049643490035307020, 0.3917322834645669549, -1.351049868766404538 ) ) ;
#33691 = CARTESIAN_POINT ( 'NONE',  ( -1.706036745406823485, 0.2306618581243848609, 0.2411417322834645549 ) ) ;
#33692 = CARTESIAN_POINT ( 'NONE',  ( 0.5052493438320218022, -0.6692913385826773087, -0.1292274648535924053 ) ) ;
#33693 = CARTESIAN_POINT ( 'NONE',  ( 0.2559055118110243332, 0.1660481256975885056, 0.3530559997133364547 ) ) ;
#33694 = CARTESIAN_POINT ( 'NONE',  ( 0.1377952755905518800, 0.07958543189024071263, -0.2665933059059888421 ) ) ;
#33695 = CARTESIAN_POINT ( 'NONE',  ( -0.2952755905511810774, 3.616083068348483797E-17, -1.929133858267716661 ) ) ;
#33697 = MANIFOLD_SOLID_BREP ( 'Fillet2', #25857 ) ;
#33696 = CARTESIAN_POINT ( 'NONE',  ( -0.1377952755905504645, -0.4536011799217368745, -0.2665933059059886201 ) ) ;
#33698 = CARTESIAN_POINT ( 'NONE',  ( 0.8989501312335964611, 0.2952755905511811885, 0.1292274648535926551 ) ) ;
#33699 = CARTESIAN_POINT ( 'NONE',  ( -0.6167979002624665030, -0.004921259842519576551, 0.3153832671262227771 ) ) ;
#33700 = CARTESIAN_POINT ( 'NONE',  ( -1.069553805774277722, -0.6692913385826773087, -0.1292274648535924053 ) ) ;
#33701 = LINE ( 'NONE', #79583, #31349 ) ;
#33702 = ORIENTED_EDGE ( 'NONE', *, *, #18159, .F. ) ;
#33703 = CARTESIAN_POINT ( 'NONE',  ( -1.233595800524933894, -0.6046776061558809534, -0.2411417322834644161 ) ) ;
#33704 = CARTESIAN_POINT ( 'NONE',  ( -1.062992125984250968, 0.1771653543307087630, 0.000000000000000000 ) ) ;
#33705 = CARTESIAN_POINT ( 'NONE',  ( 0.01968503937007930540, 0.1660481256975885056, 0.3530559997133364547 ) ) ;
#33706 = CARTESIAN_POINT ( 'NONE',  ( -1.555118110236219930, 0.1660481256975885056, 0.3530559997133364547 ) ) ;
#33707 = CARTESIAN_POINT ( 'NONE',  ( -0.7611548556430438595, -0.6046776061558809534, -0.2411417322834644161 ) ) ;
#33708 = CARTESIAN_POINT ( 'NONE',  ( -1.868118687985136805, 2.729653196743539567, 0.5314960629921260393 ) ) ;
#33710 = CARTESIAN_POINT ( 'NONE',  ( 0.7939632545931766261, -0.05778040916215522460, 0.4822834645669289988 ) ) ;
#33709 = CARTESIAN_POINT ( 'NONE',  ( 1.686351706036745890, 0.2952755905511811885, 0.1292274648535926551 ) ) ;
#33711 = CARTESIAN_POINT ( 'NONE',  ( 0.7742782152230979209, 0.05413385826771626580, -0.4176697321401330321 ) ) ;
#33712 = CARTESIAN_POINT ( 'NONE',  ( -0.3917322834645670104, -7.196005306013484475E-17, -2.393700787401574992 ) ) ;
#33713 = CARTESIAN_POINT ( 'NONE',  ( -0.3808816823641234528, 0.09156050430092053938, -1.220472440944881942 ) ) ;
#33714 = CARTESIAN_POINT ( 'NONE',  ( -1.259842519685038686, -0.1870078740157479769, 0.4822834645669291653 ) ) ;
#33715 = CARTESIAN_POINT ( 'NONE',  ( 0.1070741851644054915, -0.3996062992125986035, -0.2427821522309711877 ) ) ;
#33716 = ORIENTED_EDGE ( 'NONE', *, *, #57864, .T. ) ;
#33717 = CARTESIAN_POINT ( 'NONE',  ( -0.3412073490813641308, 0.1283753931104746893, -0.1820866141732285504 ) ) ;
#33718 = CARTESIAN_POINT ( 'NONE',  ( -0.3392501089628017219, -0.1958661417322836718, -1.776902887139107490 ) ) ;
#33719 = ORIENTED_EDGE ( 'NONE', *, *, #82527, .T. ) ;
#33720 = CARTESIAN_POINT ( 'NONE',  ( 0.2362204724409456558, -0.1870078740157480879, -0.4822834645669291653 ) ) ;
#33721 = CARTESIAN_POINT ( 'NONE',  ( 0.06561679790026316017, 0.05413385826771626580, -0.4176697321401330321 ) ) ;
#33722 = CARTESIAN_POINT ( 'NONE',  ( -0.4921259842519677963, 0.1660481256975883668, -0.3530559997133364547 ) ) ;
#33723 = CARTESIAN_POINT ( 'NONE',  ( 1.489501312335958172, -0.3162353388693405765, 0.4822834645669290543 ) ) ;
#33724 = CARTESIAN_POINT ( 'NONE',  ( -1.017060367454067249, -0.08942795157527998196, 0.3641732283464567121 ) ) ;
#33725 = CARTESIAN_POINT ( 'NONE',  ( 0.008867907465126901798, 1.063056921846344371, -1.625415946341134399 ) ) ;
#33726 = CARTESIAN_POINT ( 'NONE',  ( 0.8989501312335964611, 0.2952755905511811885, 0.1292274648535926551 ) ) ;
#33727 = CARTESIAN_POINT ( 'NONE',  ( 0.6233595800524939223, -0.2845877964562159024, 0.3641732283464567677 ) ) ;
#33728 = VECTOR ( 'NONE', #7878, 39.37007874015748143 ) ;
#33729 = CARTESIAN_POINT ( 'NONE',  ( -0.2624671916010490880, -0.6046776061558807314, 0.2411417322834647770 ) ) ;
#33730 = CARTESIAN_POINT ( 'NONE',  ( -0.1958661417322836440, 0.3392501089628016664, -1.352999056921573295 ) ) ;
#33731 = CARTESIAN_POINT ( 'NONE',  ( -0.9514435695538050464, -0.05778040916215560624, -0.4822834645669293319 ) ) ;
#33732 = CARTESIAN_POINT ( 'NONE',  ( -1.719160104986876103, -0.004921259842519576551, 0.3153832671262227771 ) ) ;
#33733 = EDGE_CURVE ( 'NONE', #31638, #28541, #36477, .T. ) ;
#33734 = CARTESIAN_POINT ( 'NONE',  ( 1.266404199475066328, -0.3162353388693409650, -0.4822834645669289433 ) ) ;
#33735 = CARTESIAN_POINT ( 'NONE',  ( 1.627296587926509996, -0.5023911411419708095, 0.1820866141732285504 ) ) ;
#33736 = VERTEX_POINT ( 'NONE', #82209 ) ;
#33737 = CARTESIAN_POINT ( 'NONE',  ( 0.1958661417322836718, -0.3392501089628017219, -2.450806717356642128 ) ) ;
#33738 = CARTESIAN_POINT ( 'NONE',  ( -0.01312335958005186876, 0.05413385826771626580, -0.4176697321401330321 ) ) ;
#33739 = VERTEX_POINT ( 'NONE', #56507 ) ;
#33740 = CARTESIAN_POINT ( 'NONE',  ( -1.266404199475064773, -0.3162353388693405765, 0.4822834645669290543 ) ) ;
#33741 = CARTESIAN_POINT ( 'NONE',  ( 1.279527559055118724, 0.1660481256975885056, 0.3530559997133364547 ) ) ;
#33742 = CARTESIAN_POINT ( 'NONE',  ( 1.351706036745407458, -0.4281496062992127816, -0.4176697321401328100 ) ) ;
#33743 = CARTESIAN_POINT ( 'NONE',  ( 0.4658792650918640033, -0.3162353388693405765, 0.4822834645669290543 ) ) ;
#33744 = CARTESIAN_POINT ( 'NONE',  ( -0.5183727034120726440, 0.2952755905511811885, 0.1292274648535926551 ) ) ;
#33745 = CARTESIAN_POINT ( 'NONE',  ( -0.1049643490035302024, -0.3917322834645671215, -1.889107611548556109 ) ) ;
#33746 = CARTESIAN_POINT ( 'NONE',  ( -1.292650918635170010, -0.6692913385826771977, 0.1292274648535927661 ) ) ;
#33747 = CARTESIAN_POINT ( 'NONE',  ( -0.5708661417322825615, -0.5400638737290844871, 0.3530559997133364547 ) ) ;
#33748 = CARTESIAN_POINT ( 'NONE',  ( -0.5052493438320203589, 0.1771653543307087075, -0.09757992244046823083 ) ) ;
#33749 = CARTESIAN_POINT ( 'NONE',  ( -1.603475055217291612, 0.7166759647713523140, 0.04573490813648251746 ) ) ;
#33750 = AXIS2_PLACEMENT_3D ( 'NONE', #35780, #29460, #68195 ) ;
#33751 = CARTESIAN_POINT ( 'NONE',  ( -0.5839895013123351797, 0.2952755905511810774, -0.1292274648535930714 ) ) ;
#33752 = CARTESIAN_POINT ( 'NONE',  ( -0.5314960629921395840, 2.677165354330708791, 3.900966923095588346 ) ) ;
#33753 = CARTESIAN_POINT ( 'NONE',  ( 0.6627296587926515548, 0.2952755905511811885, 0.1292274648535926551 ) ) ;
#33754 = CARTESIAN_POINT ( 'NONE',  ( 3.911272252003783034, 1.384743710585661924, -0.4494451973059669370 ) ) ;
#33755 = CARTESIAN_POINT ( 'NONE',  ( -0.1443569553805765515, -0.4281496062992127816, -0.4176697321401328100 ) ) ;
#33756 = CARTESIAN_POINT ( 'NONE',  ( -0.4199475065616791736, 0.1283753931104746893, -0.1820866141732285504 ) ) ;
#33758 = CARTESIAN_POINT ( 'NONE',  ( -0.9251968503937002541, 0.1012011053420777407, 0.2882089793578257453 ) ) ;
#33757 = CARTESIAN_POINT ( 'NONE',  ( 0.9317585301837276734, -0.004921259842519870586, -0.3153832671262229437 ) ) ;
#33759 = CARTESIAN_POINT ( 'NONE',  ( 0.4724409448818896462, 0.1265901696524990294, -0.5164041994750655507 ) ) ;
#33760 = CARTESIAN_POINT ( 'NONE',  ( 1.345144356955381593, -0.08942795157527998196, 0.3641732283464567121 ) ) ;
#33761 = EDGE_CURVE ( 'NONE', #50299, #49469, #50599, .T. ) ;
#33762 = CARTESIAN_POINT ( 'NONE',  ( 1.423884514435696191, -0.05778040916215522460, 0.4822834645669289988 ) ) ;
#33763 = CARTESIAN_POINT ( 'NONE',  ( -0.1974969037888706924, 0.3420746716998658843, -0.2473753280839895707 ) ) ;
#33764 = CARTESIAN_POINT ( 'NONE',  ( 0.2034120734908142214, 0.2952755905511810774, -0.1292274648535930714 ) ) ;
#33765 = CARTESIAN_POINT ( 'NONE',  ( 3.924389226575468737, 2.755905511811024056, -0.3149606299212597271 ) ) ;
#33766 = CARTESIAN_POINT ( 'NONE',  ( -1.607611548556429737, -0.6692913385826771977, 0.1292274648535927661 ) ) ;
#33767 = CARTESIAN_POINT ( 'NONE',  ( -0.01968503937007793844, -0.5400638737290844871, 0.3530559997133364547 ) ) ;
#33768 = ADVANCED_FACE ( 'NONE', ( #50193 ), #43187, .T. ) ;
#33769 = CARTESIAN_POINT ( 'NONE',  ( 0.2891555358219910499, 0.2891555358219910499, -0.05708661417322836301 ) ) ;
#33770 = CARTESIAN_POINT ( 'NONE',  ( -1.561679790026246017, -0.3690944881889765550, -0.3153832671262227771 ) ) ;
#33771 = CARTESIAN_POINT ( 'NONE',  ( 0.4133858267716541968, -0.5400638737290845981, -0.3530559997133363437 ) ) ;
#33772 = CARTESIAN_POINT ( 'NONE',  ( 0.8267716535433078384, -0.5511811023622047445, 6.969142054262312111E-17 ) ) ;
#33773 = CARTESIAN_POINT ( 'NONE',  ( 0.3130111271098954262, 1.444537301488023839, 0.002033853763896861528 ) ) ;
#33774 = CARTESIAN_POINT ( 'NONE',  ( 0.4527559055118117182, 0.07958543189024071263, -0.2665933059059888421 ) ) ;
#33775 = CARTESIAN_POINT ( 'NONE',  ( -1.417322834645668772, -0.1870078740157480879, -0.4822834645669291653 ) ) ;
#33776 = CARTESIAN_POINT ( 'NONE',  ( 0.1998031496062994128, -0.3460692066303957537, -0.9560367454068241511 ) ) ;
#33777 = CARTESIAN_POINT ( 'NONE',  ( 1.181102362204725198, -0.1870078740157479769, 0.4822834645669291653 ) ) ;
#33778 = CARTESIAN_POINT ( 'NONE',  ( 0.3392501089628018884, -0.1958661417322834220, -0.5695538057742781657 ) ) ;
#33780 = CARTESIAN_POINT ( 'NONE',  ( 0.000000000000000000, 2.755905511811024056, 0.000000000000000000 ) ) ;
#33779 = CARTESIAN_POINT ( 'NONE',  ( 0.4724409448818904789, -0.1870078740157480879, -0.4822834645669291653 ) ) ;
#33781 = CARTESIAN_POINT ( 'NONE',  ( -0.3273801728231969244, -2.609869883881465018E-15, -0.3464511005275220379 ) ) ;
#33782 = CARTESIAN_POINT ( 'NONE',  ( 0.3674540682414705883, 0.1283753931104746893, -0.1820866141732285504 ) ) ;
#33783 = CARTESIAN_POINT ( 'NONE',  ( 0.4002624671916016896, -0.05778040916215522460, 0.4822834645669289988 ) ) ;
#33784 = DIRECTION ( 'NONE',  ( -0.000000000000000000, -1.000000000000000000, -0.000000000000000000 ) ) ;
#33785 = CARTESIAN_POINT ( 'NONE',  ( -1.082677165354329896, 0.07958543189024085140, 0.2665933059059887866 ) ) ;
#33786 = CARTESIAN_POINT ( 'NONE',  ( -0.8858267716535425107, 0.1660481256975883668, -0.3530559997133364547 ) ) ;
#33787 = CARTESIAN_POINT ( 'NONE',  ( 1.614173228346457378, 0.1771653543307087630, 0.000000000000000000 ) ) ;
#33788 = VECTOR ( 'NONE', #69414, 39.37007874015748143 ) ;
#33789 = CARTESIAN_POINT ( 'NONE',  ( 0.7414698162729663755, 0.2952755905511811885, 0.1292274648535926551 ) ) ;
#33790 = CARTESIAN_POINT ( 'NONE',  ( -1.633858267716534529, 0.07958543189024085140, 0.2665933059059887866 ) ) ;
#33791 = CARTESIAN_POINT ( 'NONE',  ( -0.3857547143408425749, 0.07128922432405607190, -1.220472440944881942 ) ) ;
#33792 = CARTESIAN_POINT ( 'NONE',  ( 0.6824146981627303710, 0.2306618581243847221, -0.2411417322834647770 ) ) ;
#33793 = CARTESIAN_POINT ( 'NONE',  ( -0.3458507752293906723, -0.3458507752293910609, -2.812992125984251857 ) ) ;
#33794 = CARTESIAN_POINT ( 'NONE',  ( 1.574803149606299746, -0.1870078740157480879, -0.4822834645669291653 ) ) ;
#33795 = CARTESIAN_POINT ( 'NONE',  ( 1.528871391076116026, 0.2952755905511811885, 0.1292274648535926551 ) ) ;
#33796 = CARTESIAN_POINT ( 'NONE',  ( -1.653543307086613234, -0.1870078740157480601, -0.3641732283464567677 ) ) ;
#33797 = CARTESIAN_POINT ( 'NONE',  ( 1.017060367454068803, -0.2845877964562159024, 0.3641732283464567677 ) ) ;
#33798 = CARTESIAN_POINT ( 'NONE',  ( -1.351706036745406347, -0.3690944881889763329, 0.3153832671262228327 ) ) ;
#33799 = CARTESIAN_POINT ( 'NONE',  ( -0.6692913385826764205, 0.1771653543307087630, 0.000000000000000000 ) ) ;
#33800 = CARTESIAN_POINT ( 'NONE',  ( -0.03443470937339819515, 1.064243487142144673, -1.633358474390059989 ) ) ;
#33801 = CARTESIAN_POINT ( 'NONE',  ( 0.4527559055118117182, -0.4536011799217367080, 0.2665933059059888421 ) ) ;
#33802 = CARTESIAN_POINT ( 'NONE',  ( 0.4527559055118117182, 0.1660481256975883668, -0.3530559997133364547 ) ) ;
#33803 = CARTESIAN_POINT ( 'NONE',  ( 1.174540682414699111, -0.05778040916215560624, -0.4822834645669293319 ) ) ;
#33804 = CARTESIAN_POINT ( 'NONE',  ( -0.1246719160104980823, -0.6692913385826773087, -0.1292274648535924053 ) ) ;
#33805 = CARTESIAN_POINT ( 'NONE',  ( 0.2034120734908142214, 0.1771653543307087075, -0.09757992244046823083 ) ) ;
#33806 = CARTESIAN_POINT ( 'NONE',  ( 1.299212598425197429, 0.2952755905511811885, 0.000000000000000000 ) ) ;
#33807 = DIRECTION ( 'NONE',  ( -3.491481338843133355E-15, -0.000000000000000000, 1.000000000000000000 ) ) ;
#33808 = CARTESIAN_POINT ( 'NONE',  ( -0.7742782152230965886, 0.05413385826771666132, 0.4176697321401328100 ) ) ;
#33809 = CARTESIAN_POINT ( 'NONE',  ( 0.3996062992125986035, 2.446882876249141962E-17, -0.5905511811023621549 ) ) ;
#33810 = CARTESIAN_POINT ( 'NONE',  ( 0.02624671916010564918, 0.1539470093639523085, 0.1968503937007873850 ) ) ;
#33811 = CARTESIAN_POINT ( 'NONE',  ( -0.02624671916010428221, -0.6046776061558807314, 0.2411417322834647770 ) ) ;
#33812 = CARTESIAN_POINT ( 'NONE',  ( -0.9580052493438311334, 0.05413385826771626580, -0.4176697321401330321 ) ) ;
#33813 = CARTESIAN_POINT ( 'NONE',  ( -0.1049868766404193215, 0.2306618581243847221, -0.2411417322834647770 ) ) ;
#33814 = CARTESIAN_POINT ( 'NONE',  ( 0.3460692066303959757, -0.1998031496062991907, -2.624671916010498762 ) ) ;
#33815 = CARTESIAN_POINT ( 'NONE',  ( 0.3949938075777409408, 0.1058382717557500574, -2.014435695538057569 ) ) ;
#33816 = CARTESIAN_POINT ( 'NONE',  ( 0.2867679344610365999, 0.2867679344610365999, -0.6023622047244093780 ) ) ;
#33817 = CARTESIAN_POINT ( 'NONE',  ( -3.184294706754630777, 2.755905511811024056, -0.5314960629921260393 ) ) ;
#33818 = CARTESIAN_POINT ( 'NONE',  ( -1.017060367454067249, -0.2845877964562161244, -0.3641732283464567121 ) ) ;
#33819 = CARTESIAN_POINT ( 'NONE',  ( -0.1958661417322836718, 0.3392501089628017219, -1.107611548556430403 ) ) ;
#33820 = CARTESIAN_POINT ( 'NONE',  ( -1.633858267716534529, -0.5400638737290845981, -0.3530559997133363437 ) ) ;
#33821 = CARTESIAN_POINT ( 'NONE',  ( -0.2867679344610364334, -0.2867679344610368219, 0.1758723341545424812 ) ) ;
#33822 = CARTESIAN_POINT ( 'NONE',  ( 0.6102362204724416372, 0.1660481256975883668, -0.3530559997133364547 ) ) ;
#33823 = CARTESIAN_POINT ( 'NONE',  ( -0.4593175853018366950, -0.004921259842519576551, 0.3153832671262227771 ) ) ;
#33824 = CARTESIAN_POINT ( 'NONE',  ( 0.7545931758530188826, -0.6692913385826771977, 0.1292274648535927661 ) ) ;
#33825 = CARTESIAN_POINT ( 'NONE',  ( 0.4396325459317590445, -0.6692913385826771977, 0.1292274648535927661 ) ) ;
#33826 = CARTESIAN_POINT ( 'NONE',  ( 0.000000000000000000, -0.04921259842519688094, 0.08523872084492505052 ) ) ;
#33827 = CARTESIAN_POINT ( 'NONE',  ( -0.1998031496062991907, -0.3460692066303959757, -2.742782152230971437 ) ) ;
#33828 = CARTESIAN_POINT ( 'NONE',  ( 0.2867679344610366554, -0.2867679344610365999, -1.040045562500999443 ) ) ;
#33829 = CARTESIAN_POINT ( 'NONE',  ( 1.174540682414699111, -0.3162353388693405765, 0.4822834645669290543 ) ) ;
#33830 = CARTESIAN_POINT ( 'NONE',  ( 0.006561679790026889343, -0.05778040916215522460, 0.4822834645669289988 ) ) ;
#33831 = CARTESIAN_POINT ( 'NONE',  ( 1.430446194225722500, 0.05413385826771666132, 0.4176697321401328100 ) ) ;
#33832 = CARTESIAN_POINT ( 'NONE',  ( 0.7020997375328090762, -0.3162353388693405765, 0.4822834645669290543 ) ) ;
#33833 = CARTESIAN_POINT ( 'NONE',  ( 0.3392501089628018884, -0.1958661417322834220, -0.6620734908136483021 ) ) ;
#33834 = CARTESIAN_POINT ( 'NONE',  ( -0.05249343832020938322, -0.6046776061558809534, -0.2411417322834644161 ) ) ;
#33835 = CARTESIAN_POINT ( 'NONE',  ( 0.5643044619422579178, 0.05413385826771666132, 0.4176697321401328100 ) ) ;
#33836 = CARTESIAN_POINT ( 'NONE',  ( -0.2099737532808391705, 0.2306618581243848609, 0.2411417322834645549 ) ) ;
#33837 = CARTESIAN_POINT ( 'NONE',  ( 1.154855643044620184, -0.5023911411419708095, 0.1820866141732285504 ) ) ;
#33838 = CARTESIAN_POINT ( 'NONE',  ( -1.253280839895012377, -0.05778040916215522460, 0.4822834645669289988 ) ) ;
#33839 = CARTESIAN_POINT ( 'NONE',  ( -1.502624671916009680, -0.05778040916215560624, -0.4822834645669293319 ) ) ;
#33840 = AXIS2_PLACEMENT_3D ( 'NONE', #37266, #24625, #75170 ) ;
#33841 = CARTESIAN_POINT ( 'NONE',  ( 0.6758530183727039509, 0.2952755905511810774, -0.1292274648535930714 ) ) ;
#33842 = CARTESIAN_POINT ( 'NONE',  ( 0.3758920641862648626, -0.1123167701215118386, -1.929133858267716883 ) ) ;
#33843 = CARTESIAN_POINT ( 'NONE',  ( -0.3917322834645671215, 0.1049643490035301469, -1.757217847769028340 ) ) ;
#33844 = ORIENTED_EDGE ( 'NONE', *, *, #63059, .T. ) ;
#33845 = CARTESIAN_POINT ( 'NONE',  ( -0.1070741851644051862, -0.3996062992125987146, -0.2296587926509186528 ) ) ;
#33846 = ORIENTED_EDGE ( 'NONE', *, *, #37456, .F. ) ;
#33847 = CARTESIAN_POINT ( 'NONE',  ( 1.286089238845145033, -0.6046776061558809534, -0.2411417322834644161 ) ) ;
#33848 = CARTESIAN_POINT ( 'NONE',  ( 0.9973753280839902091, 0.1283753931104746893, -0.1820866141732285504 ) ) ;
#33849 = CARTESIAN_POINT ( 'NONE',  ( -0.3149606299212458493, 2.165354330708661568, -3.937007874015763242 ) ) ;
#33850 = CARTESIAN_POINT ( 'NONE',  ( 0.3307086614173228023, 0.3242060844882008741, 0.000000000000000000 ) ) ;
#33851 = LINE ( 'NONE', #46047, #12331 ) ;
#33852 = CARTESIAN_POINT ( 'NONE',  ( -0.3917322834645670104, -7.196005306013484475E-17, -1.068897637795275690 ) ) ;
#33853 = EDGE_CURVE ( 'NONE', #57422, #75161, #192, .T. ) ;
#33854 = CARTESIAN_POINT ( 'NONE',  ( 1.371391076115485719, -0.6692913385826773087, -0.1292274648535924053 ) ) ;
#33855 = CARTESIAN_POINT ( 'NONE',  ( -1.574803149606298192, -0.1870078740157480879, -0.4822834645669291653 ) ) ;
#33856 = CARTESIAN_POINT ( 'NONE',  ( -0.5052493438320203589, -0.6692913385826771977, 0.1292274648535927661 ) ) ;
#33857 = CARTESIAN_POINT ( 'NONE',  ( 0.9317585301837276734, -0.4281496062992124485, 0.4176697321401328655 ) ) ;
#33858 = ORIENTED_EDGE ( 'NONE', *, *, #63918, .T. ) ;
#33859 = CARTESIAN_POINT ( 'NONE',  ( -1.561679790026246017, 0.05413385826771666132, 0.4176697321401328100 ) ) ;
#33860 = CARTESIAN_POINT ( 'NONE',  ( -0.09115970038225217065, 2.409604939980833412E-17, -0.3464511005275205946 ) ) ;
#33861 = SHAPE_DEFINITION_REPRESENTATION ( #71506, #79348 ) ;
#33862 = CARTESIAN_POINT ( 'NONE',  ( 1.686351706036745890, 0.1771653543307087630, 0.09757992244046791164 ) ) ;
#33863 = CARTESIAN_POINT ( 'NONE',  ( -1.614173228346457378, 1.881821177735609085, 0.1372047244094476981 ) ) ;
#33864 = CARTESIAN_POINT ( 'NONE',  ( -0.9908136482939626788, 0.1771653543307087630, 0.09757992244046791164 ) ) ;
#33865 = CARTESIAN_POINT ( 'NONE',  ( -1.587926509186350810, 0.05413385826771626580, -0.4176697321401330321 ) ) ;
#33866 = CARTESIAN_POINT ( 'NONE',  ( 0.8005249343832028242, -0.4281496062992127816, -0.4176697321401328100 ) ) ;
#33867 = ORIENTED_EDGE ( 'NONE', *, *, #78524, .T. ) ;
#33869 = CARTESIAN_POINT ( 'NONE',  ( -0.4068241469816267775, 0.009842519685039144428, -0.3409548833797004797 ) ) ;
#33868 = CARTESIAN_POINT ( 'NONE',  ( 1.509186351706037543, 0.05413385826771666132, 0.4176697321401328100 ) ) ;
#33870 = CARTESIAN_POINT ( 'NONE',  ( -0.5446194225721777693, -0.2845877964562161244, -0.3641732283464567121 ) ) ;
#33871 = CARTESIAN_POINT ( 'NONE',  ( 0.6430446194225729606, -0.4281496062992127816, -0.4176697321401328100 ) ) ;
#33872 = CARTESIAN_POINT ( 'NONE',  ( -1.614173228346456268, -0.6692913385826771977, 8.415575281601705876E-17 ) ) ;
#33873 = CARTESIAN_POINT ( 'NONE',  ( 0.1958661417322836162, -0.3392501089628018329, -1.116778584480628389 ) ) ;
#33874 = CARTESIAN_POINT ( 'NONE',  ( -0.7283464566929126471, 0.07958543189024071263, -0.2665933059059888421 ) ) ;
#33875 = CARTESIAN_POINT ( 'NONE',  ( 1.587926509186352586, -0.4281496062992127816, -0.4176697321401328100 ) ) ;
#33876 = LINE ( 'NONE', #20001, #8872 ) ;
#33877 = CARTESIAN_POINT ( 'NONE',  ( 0.6692913385826777528, 0.2952755905511811885, 0.000000000000000000 ) ) ;
#33878 = CARTESIAN_POINT ( 'NONE',  ( -0.7611548556430438595, -0.5023911411419708095, -0.1820866141732282451 ) ) ;
#33879 = CARTESIAN_POINT ( 'NONE',  ( -0.4199475065616791736, 0.1283753931104746893, -0.1820866141732285504 ) ) ;
#33880 = CARTESIAN_POINT ( 'NONE',  ( -0.1902887139107604098, -0.6692913385826771977, 0.1292274648535927661 ) ) ;
#33881 = CARTESIAN_POINT ( 'NONE',  ( -1.266404199475064773, -0.08942795157528024563, -0.3641732283464568787 ) ) ;
#33882 = CARTESIAN_POINT ( 'NONE',  ( 0.3392501089628018329, 0.1958661417322835607, 0.02950824327327895152 ) ) ;
#33883 = CARTESIAN_POINT ( 'NONE',  ( 0.6627296587926515548, 0.2952755905511811885, 0.1292274648535926551 ) ) ;
#33884 = CARTESIAN_POINT ( 'NONE',  ( 2.543486866223389153, 2.716535433070866645, 0.5314960629921260393 ) ) ;
#33885 = CARTESIAN_POINT ( 'NONE',  ( -0.3458507752293906723, -0.3458507752293910609, -1.710629921259842812 ) ) ;
#33886 = CARTESIAN_POINT ( 'NONE',  ( -0.9383202099737524282, -0.05778040916215522460, 0.4822834645669289988 ) ) ;
#33887 = CARTESIAN_POINT ( 'NONE',  ( -0.2034120734908131112, -0.5511811023622048555, -0.09757992244046775898 ) ) ;
#33888 = CARTESIAN_POINT ( 'NONE',  ( -1.397637795275589623, -0.5400638737290845981, -0.3530559997133363437 ) ) ;
#33889 = CARTESIAN_POINT ( 'NONE',  ( 0.6627296587926517768, -0.5511811023622048555, -0.09757992244046775898 ) ) ;
#33890 = CARTESIAN_POINT ( 'NONE',  ( -0.9317585301837263412, -0.004921259842519576551, 0.3153832671262227771 ) ) ;
#33891 = CARTESIAN_POINT ( 'NONE',  ( -0.8858267716535425107, 0.1660481256975883668, -0.3530559997133364547 ) ) ;
#33892 = CARTESIAN_POINT ( 'NONE',  ( -1.679790026246718693, 0.2306618581243847221, -0.2411417322834647770 ) ) ;
#33893 = CARTESIAN_POINT ( 'NONE',  ( -1.541994750656167090, -0.6692913385826773087, -0.1292274648535924053 ) ) ;
#33894 = CARTESIAN_POINT ( 'NONE',  ( -0.6743677364976040645, 1.919528099548696076, 0.5309055118110236338 ) ) ;
#33895 = CARTESIAN_POINT ( 'NONE',  ( 0.9711286089238851948, -0.5023911411419708095, -0.1820866141732282451 ) ) ;
#33896 = PRODUCT_DEFINITION_SHAPE ( 'NONE', 'NONE',  #83320 ) ;
#33897 = CARTESIAN_POINT ( 'NONE',  ( 0.6036745406824154392, 0.2306618581243847221, -0.2411417322834647770 ) ) ;
#33898 = CARTESIAN_POINT ( 'NONE',  ( -1.456692913385826182, 0.2952755905511811885, 0.000000000000000000 ) ) ;
#33899 = CARTESIAN_POINT ( 'NONE',  ( 1.548556430446194954, -0.5023911411419708095, 0.1820866141732285504 ) ) ;
#33900 = CONICAL_SURFACE ( 'NONE', #59433, 2.559055118110236560, 0.7853981633974500554 ) ;
#33901 = ORIENTED_EDGE ( 'NONE', *, *, #61940, .F. ) ;
#33902 = CARTESIAN_POINT ( 'NONE',  ( 0.2925321140481932369, -0.2925321140481931814, -2.852362204724409711 ) ) ;
#33903 = CARTESIAN_POINT ( 'NONE',  ( -1.167979002624671470, -0.004921259842519576551, 0.3153832671262227771 ) ) ;
#33904 = CARTESIAN_POINT ( 'NONE',  ( -0.6758530183727028406, 0.2952755905511811885, 0.1292274648535926551 ) ) ;
#33905 = CARTESIAN_POINT ( 'NONE',  ( 0.2230971128608929543, 0.05413385826771626580, -0.4176697321401330321 ) ) ;
#33906 = CARTESIAN_POINT ( 'NONE',  ( -1.633858267716534529, -0.4536011799217368745, -0.2665933059059886201 ) ) ;
#33907 = CARTESIAN_POINT ( 'NONE',  ( -0.3460692066303960313, 0.1998031496062989965, -1.835301837270341352 ) ) ;
#33908 = CARTESIAN_POINT ( 'NONE',  ( -1.292650918635170010, -0.6692913385826771977, 0.1292274648535927661 ) ) ;
#33909 = CARTESIAN_POINT ( 'NONE',  ( 0.4461942257217856311, 0.2306618581243847221, -0.2411417322834647770 ) ) ;
#33910 = CARTESIAN_POINT ( 'NONE',  ( 0.3083989501312343062, -0.05778040916215560624, -0.4822834645669293319 ) ) ;
#33911 = CARTESIAN_POINT ( 'NONE',  ( 1.213910761154856299, -0.6692913385826773087, -0.1292274648535924053 ) ) ;
#33912 = CARTESIAN_POINT ( 'NONE',  ( -0.3996062992125986035, 0.1070741851644051584, -1.054461942257217899 ) ) ;
#33913 = CARTESIAN_POINT ( 'NONE',  ( 0.1070741851644054915, -0.3996062992125986035, -1.502624671916010346 ) ) ;
#33914 = CARTESIAN_POINT ( 'NONE',  ( -0.2891555358219908833, -0.2891555358219912164, -0.6889763779527559029 ) ) ;
#33915 = DIRECTION ( 'NONE',  ( -1.000000000000000000, -0.000000000000000000, -0.000000000000000000 ) ) ;
#33916 = CARTESIAN_POINT ( 'NONE',  ( 0.5183727034120741983, 0.1771653543307087075, -0.09757992244046823083 ) ) ;
#33917 = CARTESIAN_POINT ( 'NONE',  ( -0.4527559055118102749, 0.1660481256975885056, 0.3530559997133364547 ) ) ;
#33918 = CARTESIAN_POINT ( 'NONE',  ( 1.246719160104987623, -0.4281496062992124485, 0.4176697321401328655 ) ) ;
#33919 = CARTESIAN_POINT ( 'NONE',  ( 0.1058382717557500852, -0.3949938075777408852, -1.579396325459317740 ) ) ;
#33920 = CARTESIAN_POINT ( 'NONE',  ( 0.006561679790026889343, -0.2845877964562161244, -0.3641732283464567121 ) ) ;
#33921 =( BOUNDED_CURVE ( )  B_SPLINE_CURVE ( 2, ( #51591, #38151, #70981, #19205, #82373, #18401, #31418, #13325, #58334, #7000, #696, #57082, #63823 ),
 .UNSPECIFIED., .F., .F. ) 
 B_SPLINE_CURVE_WITH_KNOTS ( ( 3, 2, 2, 2, 2, 2, 3 ),
 ( 0.6733310946348007864, 0.6742424242424241987, 0.6780303030303029832, 0.6818181818181817677, 0.6856060606060605522, 0.6893939393939394478, 0.6903052690015629711 ),
 .UNSPECIFIED. ) 
 CURVE ( )  GEOMETRIC_REPRESENTATION_ITEM ( )  RATIONAL_B_SPLINE_CURVE ( ( 0.9875488213027523443, 0.9918020599134680371, 1.000000000000000000, 0.9659258262890683122, 1.000000000000000000, 0.9659258262890683122, 1.000000000000000000, 0.9659258262890683122, 1.000000000000000000, 0.9659258262890683122, 1.000000000000000000, 0.9918020599134671489, 0.9875488213027514561 ) ) 
 REPRESENTATION_ITEM ( '' )  );
#33922 = CARTESIAN_POINT ( 'NONE',  ( -1.095800524934382292, -0.3162353388693409650, -0.4822834645669289433 ) ) ;
#33923 = CARTESIAN_POINT ( 'NONE',  ( 1.502624671916010790, -0.3162353388693409650, -0.4822834645669289433 ) ) ;
#33924 = CARTESIAN_POINT ( 'NONE',  ( 0.3149606299212606708, -0.1870078740157480879, -0.4822834645669291653 ) ) ;
#33925 = CARTESIAN_POINT ( 'NONE',  ( -0.2362204724409451284, 0.4091458600556402425, -2.217847769028871596 ) ) ;
#33926 = CARTESIAN_POINT ( 'NONE',  ( 0.2955417804206911248, -0.2579773093944459084, -2.755905511811021835 ) ) ;
#33927 = EDGE_LOOP ( 'NONE', ( #62718, #32793, #34538 ) ) ;
#33928 = EDGE_LOOP ( 'NONE', ( #74235, #36716, #1721, #17508 ) ) ;
#33929 = CARTESIAN_POINT ( 'NONE',  ( 1.568241469816273437, -0.2845877964562159024, 0.3641732283464567677 ) ) ;
#33931 = CARTESIAN_POINT ( 'NONE',  ( -1.325459317585300889, 0.05413385826771666132, 0.4176697321401328100 ) ) ;
#33930 = CARTESIAN_POINT ( 'NONE',  ( -1.286089238845143479, 0.1283753931104746893, -0.1820866141732285504 ) ) ;
#33932 = CARTESIAN_POINT ( 'NONE',  ( -0.1049643490035301746, -0.3917322834645670659, -2.199455749834958951 ) ) ;
#33933 = CARTESIAN_POINT ( 'NONE',  ( 0.4848604877838280647, 0.000000000000000000, 0.3464511005275205946 ) ) ;
#33934 = CARTESIAN_POINT ( 'NONE',  ( 1.194225721784777594, 0.05413385826771666132, 0.4176697321401328100 ) ) ;
#33935 = CARTESIAN_POINT ( 'NONE',  ( -1.338582677165353729, -0.1870078740157480879, -0.4822834645669291653 ) ) ;
#33936 = CARTESIAN_POINT ( 'NONE',  ( 0.01968503937007930540, 0.1660481256975885056, 0.3530559997133364547 ) ) ;
#33937 = CARTESIAN_POINT ( 'NONE',  ( -1.253280839895012377, -0.3162353388693409650, -0.4822834645669289433 ) ) ;
#33938 = CARTESIAN_POINT ( 'NONE',  ( -0.3392501089628019995, 0.1958661417322832277, 0.2040682414698161695 ) ) ;
#33939 = ADVANCED_FACE ( 'NONE', ( #56917 ), #44280, .F. ) ;
#33940 = CARTESIAN_POINT ( 'NONE',  ( 0.4658792650918640033, -0.3162353388693405765, 0.4822834645669290543 ) ) ;
#33941 = CARTESIAN_POINT ( 'NONE',  ( -0.1958661417322836718, 0.3392501089628017219, -1.895013123359580165 ) ) ;
#33942 = CARTESIAN_POINT ( 'NONE',  ( -1.253280839895012377, -0.2845877964562161244, -0.3641732283464567121 ) ) ;
#33943 = ORIENTED_EDGE ( 'NONE', *, *, #55305, .T. ) ;
#33944 = CARTESIAN_POINT ( 'NONE',  ( -0.3420746716998661618, 0.1974969037888702206, -2.388451443569553856 ) ) ;
#33945 = VERTEX_POINT ( 'NONE', #23290 ) ;
#33946 = LINE ( 'NONE', #73925, #16712 ) ;
#33947 = CARTESIAN_POINT ( 'NONE',  ( -1.043307086614172707, 0.1660481256975883668, -0.3530559997133364547 ) ) ;
#33948 = CARTESIAN_POINT ( 'NONE',  ( -1.187664041994749731, -0.3162353388693405765, 0.4822834645669290543 ) ) ;
#33949 = CARTESIAN_POINT ( 'NONE',  ( 0.3996062992125986590, -0.1070741851644053111, -0.4265091863517060933 ) ) ;
#33950 = CARTESIAN_POINT ( 'NONE',  ( -1.443569553805773564, -0.6046776061558807314, 0.2411417322834647770 ) ) ;
#33951 = CARTESIAN_POINT ( 'NONE',  ( -1.541994750656167090, 0.2952755905511811885, 0.1292274648535926551 ) ) ;
#33952 = CARTESIAN_POINT ( 'NONE',  ( -1.535433070866141225, -0.6692913385826771977, 8.415575281601705876E-17 ) ) ;
#33953 = LINE ( 'NONE', #27635, #17637 ) ;
#33954 = CARTESIAN_POINT ( 'NONE',  ( -0.2867679344610364334, -0.2867679344610367109, 0.1712598425196849850 ) ) ;
#33955 = AXIS2_PLACEMENT_3D ( 'NONE', #30545, #19144, #30948 ) ;
#33956 = EDGE_CURVE ( 'NONE', #39102, #11296, #79151, .T. ) ;
#33957 = CARTESIAN_POINT ( 'NONE',  ( 0.2493438320209980519, -0.004921259842519576551, 0.3153832671262227771 ) ) ;
#33958 = CARTESIAN_POINT ( 'NONE',  ( 0.2867679344610365999, -0.2867679344610365444, -0.8129921259842518566 ) ) ;
#33959 = CARTESIAN_POINT ( 'NONE',  ( -0.6824146981627291497, -0.5023911411419708095, -0.1820866141732282451 ) ) ;
#33960 = CARTESIAN_POINT ( 'NONE',  ( -1.272965879265091305, 0.05413385826771626580, -0.4176697321401330321 ) ) ;
#33961 = CARTESIAN_POINT ( 'NONE',  ( 1.017060367454068581, -0.05778040916215560624, -0.4822834645669293319 ) ) ;
#33962 = CARTESIAN_POINT ( 'NONE',  ( -0.9580052493438311334, 0.05413385826771626580, -0.4176697321401330321 ) ) ;
#33963 = CARTESIAN_POINT ( 'NONE',  ( -0.1049643490035302024, -0.3917322834645671215, 0.09317585301837272294 ) ) ;
#33964 = EDGE_LOOP ( 'NONE', ( #41073, #27528, #54516, #53287, #35377, #82605, #68537, #41174 ) ) ;
#33965 = CARTESIAN_POINT ( 'NONE',  ( -0.7742782152230962556, -0.4281496062992127816, -0.4176697321401328100 ) ) ;
#33966 = CARTESIAN_POINT ( 'NONE',  ( 0.7152230971128614723, -0.3162353388693409650, -0.4822834645669289433 ) ) ;
#33967 = CARTESIAN_POINT ( 'NONE',  ( -1.706036745406823485, 0.1283753931104748280, 0.1820866141732283561 ) ) ;
#33968 = CARTESIAN_POINT ( 'NONE',  ( 0.000000000000000000, 0.03937007874015747977, -3.405511811023621771 ) ) ;
#33969 = CARTESIAN_POINT ( 'NONE',  ( -0.4724409448818898682, -8.678599364036362592E-17, -1.299212598425196985 ) ) ;
#33970 = CARTESIAN_POINT ( 'NONE',  ( 2.000606668791046427, 1.230840736494993815, -0.3632157284009380760 ) ) ;
#33971 = CARTESIAN_POINT ( 'NONE',  ( -0.3917322834645671215, 0.1049643490035301469, -0.4973753280839895430 ) ) ;
#33972 = CARTESIAN_POINT ( 'NONE',  ( -0.3392501089628017219, -0.1958661417322836718, -2.499343832020997080 ) ) ;
#33973 = CARTESIAN_POINT ( 'NONE',  ( -0.5052493438320203589, 0.2952755905511810774, -0.1292274648535930714 ) ) ;
#33974 = CARTESIAN_POINT ( 'NONE',  ( 1.686351706036745890, 0.2952755905511811885, 0.1292274648535926551 ) ) ;
#33975 = CARTESIAN_POINT ( 'NONE',  ( 0.3460692066303958092, 0.1998031496062993018, -0.05052493438320212332 ) ) ;
#33977 = CARTESIAN_POINT ( 'NONE',  ( -0.5314960629921373636, 2.729657682812315134, 3.237502084714954709 ) ) ;
#33976 = CARTESIAN_POINT ( 'NONE',  ( -1.325459317585300889, -0.4281496062992127816, -0.4176697321401328100 ) ) ;
#33978 = CARTESIAN_POINT ( 'NONE',  ( -1.417322834645668772, -0.1870078740157479769, 0.4822834645669291653 ) ) ;
#33979 = CARTESIAN_POINT ( 'NONE',  ( -0.3280839895013117347, -0.4281496062992124485, 0.4176697321401328655 ) ) ;
#33980 = CARTESIAN_POINT ( 'NONE',  ( -0.3949938075777409963, -7.255918531996591613E-17, -2.478346456692914312 ) ) ;
#33981 = CARTESIAN_POINT ( 'NONE',  ( 0.5774278215223103139, -0.5023911411419708095, -0.1820866141732282451 ) ) ;
#33982 = CARTESIAN_POINT ( 'NONE',  ( 0.3392501089628018329, 0.1958661417322835607, -0.05839895013123368173 ) ) ;
#33983 = CARTESIAN_POINT ( 'NONE',  ( 0.2887139107611556010, 0.1283753931104746893, -0.1820866141732285504 ) ) ;
#33984 = CARTESIAN_POINT ( 'NONE',  ( 1.410761154855643795, -0.2845877964562159024, 0.3641732283464567677 ) ) ;
#33985 = CARTESIAN_POINT ( 'NONE',  ( 0.9580052493438326877, 0.05413385826771666132, 0.4176697321401328100 ) ) ;
#33986 = CARTESIAN_POINT ( 'NONE',  ( 0.2230971128608932319, -0.3690944881889763329, 0.3153832671262228327 ) ) ;
#33987 = CARTESIAN_POINT ( 'NONE',  ( -0.3917322834645671215, 0.1049643490035301469, -2.072178477690288734 ) ) ;
#33988 = CARTESIAN_POINT ( 'NONE',  ( -1.240157480314959759, -0.5400638737290845981, -0.3530559997133363437 ) ) ;
#33989 = CARTESIAN_POINT ( 'NONE',  ( 0.006561679790026889343, -0.08942795157527998196, 0.3641732283464567121 ) ) ;
#33990 = CARTESIAN_POINT ( 'NONE',  ( -1.161417322834644716, 0.07958543189024085140, 0.2665933059059887866 ) ) ;
#33991 = CARTESIAN_POINT ( 'NONE',  ( -0.4724409448818899238, 0.1265901696524986686, -0.2670603674540683037 ) ) ;
#33992 = CARTESIAN_POINT ( 'NONE',  ( -0.6299212598425188991, -0.1870078740157480601, -0.3641732283464567677 ) ) ;
#33993 = CARTESIAN_POINT ( 'NONE',  ( 0.4478265126066724999, 1.380810887145295096, -1.530100757606696060 ) ) ;
#33994 = CARTESIAN_POINT ( 'NONE',  ( -0.2362204724409440182, -0.1870078740157479769, 0.4822834645669291653 ) ) ;
#33995 = CARTESIAN_POINT ( 'NONE',  ( -1.614173228346456712, 2.401574803149606474, 0.1372047244094477536 ) ) ;
#33996 = CARTESIAN_POINT ( 'NONE',  ( 0.3805774278215230400, -0.004921259842519870586, -0.3153832671262229437 ) ) ;
#33997 = CARTESIAN_POINT ( 'NONE',  ( -0.1312335958005241554, 0.1283753931104748280, 0.1820866141732283561 ) ) ;
#33998 = CARTESIAN_POINT ( 'NONE',  ( -0.1443569553805765515, -0.4281496062992127816, -0.4176697321401328100 ) ) ;
#33999 = PLANE ( 'NONE',  #7611 ) ;
#34000 = CARTESIAN_POINT ( 'NONE',  ( -1.076115485564303809, -0.5023911411419708095, -0.1820866141732282451 ) ) ;
#34001 = DIRECTION ( 'NONE',  ( -0.000000000000000000, -1.000000000000000000, -0.000000000000000000 ) ) ;
#34002 = CONICAL_SURFACE ( 'NONE', #71673, 3.307086614173228689, 0.7853981633974500554 ) ;
#34003 = CARTESIAN_POINT ( 'NONE',  ( 0.5052493438320218022, -0.6692913385826773087, -0.1292274648535924053 ) ) ;
#34004 = CARTESIAN_POINT ( 'NONE',  ( -0.9514435695538050464, -0.05778040916215560624, -0.4822834645669293319 ) ) ;
#34005 = CARTESIAN_POINT ( 'NONE',  ( 0.1070741851644054776, -0.3996062992125984925, -1.421916010498687877 ) ) ;
#34006 = CARTESIAN_POINT ( 'NONE',  ( 0.3917322834645669549, 0.1049643490035304660, -2.571522309711286258 ) ) ;
#34007 = CARTESIAN_POINT ( 'NONE',  ( -0.1837270341207343505, -0.5023911411419708095, 0.1820866141732285504 ) ) ;
#34008 = CARTESIAN_POINT ( 'NONE',  ( -1.364829396325458521, -0.6046776061558807314, 0.2411417322834647770 ) ) ;
#34009 = CARTESIAN_POINT ( 'NONE',  ( 1.515748031496063408, 0.1660481256975885056, 0.3530559997133364547 ) ) ;
#34010 = DIRECTION ( 'NONE',  ( -0.000000000000000000, -1.000000000000000000, -0.000000000000000000 ) ) ;
#34011 = CARTESIAN_POINT ( 'NONE',  ( -0.5577427821522301654, -0.08942795157528024563, -0.3641732283464568787 ) ) ;
#34012 = DIRECTION ( 'NONE',  ( 0.000000000000000000, 0.000000000000000000, -1.000000000000000000 ) ) ;
#34013 = CARTESIAN_POINT ( 'NONE',  ( 0.6955380577427828781, 0.05413385826771626580, -0.4176697321401330321 ) ) ;
#34014 = CARTESIAN_POINT ( 'NONE',  ( 0.3996062992125986035, 2.446882876249141962E-17, -0.1181102362204724671 ) ) ;
#34015 = VECTOR ( 'NONE', #61649, 39.37007874015748854 ) ;
#34016 = CARTESIAN_POINT ( 'NONE',  ( -0.3917322834645670659, -7.196005306013484475E-17, -2.398313279036432100 ) ) ;
#34017 = EDGE_CURVE ( 'NONE', #4461, #23692, #28430, .T. ) ;
#34018 = CARTESIAN_POINT ( 'NONE',  ( -3.841955293929017135, 2.753420937170568461, -0.5314960629921260393 ) ) ;
#34019 = CARTESIAN_POINT ( 'NONE',  ( 1.535433070866142335, -0.5511811023622047445, 6.969142054262312111E-17 ) ) ;
#34020 = CARTESIAN_POINT ( 'NONE',  ( -1.187664041994750175, -0.05778040916215560624, -0.4822834645669293319 ) ) ;
#34021 = CARTESIAN_POINT ( 'NONE',  ( 1.364829396325459854, -0.6046776061558809534, -0.2411417322834644161 ) ) ;
#34022 = CARTESIAN_POINT ( 'NONE',  ( -0.1049643490035302024, -0.3917322834645671215, -2.519028871391075786 ) ) ;
#34023 = CARTESIAN_POINT ( 'NONE',  ( 1.640419947506562393, -0.3690944881889763329, 0.3153832671262228327 ) ) ;
#34024 = CARTESIAN_POINT ( 'NONE',  ( 0.6430446194225729606, -0.4281496062992127816, -0.4176697321401328100 ) ) ;
#34025 = CARTESIAN_POINT ( 'NONE',  ( -0.5511811023622038563, -0.1870078740157479769, 0.4822834645669291653 ) ) ;
#34026 = FACE_OUTER_BOUND ( 'NONE', #62373, .T. ) ;
#34027 = CARTESIAN_POINT ( 'NONE',  ( 3.900966923095589678, 2.687614851728675092, 0.5314960629921259283 ) ) ;
#34028 = CARTESIAN_POINT ( 'NONE',  ( 0.7677165354330716118, -0.4536011799217367080, 0.2665933059059888421 ) ) ;
#34029 = ORIENTED_EDGE ( 'NONE', *, *, #16635, .T. ) ;
#34030 = CARTESIAN_POINT ( 'NONE',  ( -0.3917322834645670104, -0.1049643490035307020, -0.3576308643382697383 ) ) ;
#34031 = EDGE_LOOP ( 'NONE', ( #28828, #16777, #485, #61884, #19716, #2779 ) ) ;
#34032 = CARTESIAN_POINT ( 'NONE',  ( -0.4658792650918627265, -0.05778040916215522460, 0.4822834645669289988 ) ) ;
#34033 = CARTESIAN_POINT ( 'NONE',  ( 1.194225721784777594, -0.4281496062992127816, -0.4176697321401328100 ) ) ;
#34034 = CARTESIAN_POINT ( 'NONE',  ( 0.1640419947506569498, -0.3162353388693409650, -0.4822834645669289433 ) ) ;
#34035 = CARTESIAN_POINT ( 'NONE',  ( -0.2099737532808391705, 0.1283753931104748280, 0.1820866141732283561 ) ) ;
#34036 = CARTESIAN_POINT ( 'NONE',  ( 1.154855643044620184, -0.6046776061558807314, 0.2411417322834647770 ) ) ;
#34037 = CARTESIAN_POINT ( 'NONE',  ( -0.8398950131233585692, 0.2306618581243848609, 0.2411417322834645549 ) ) ;
#34038 = CARTESIAN_POINT ( 'NONE',  ( 0.006561679790026889343, -0.05778040916215522460, 0.4822834645669289988 ) ) ;
#34039 = CARTESIAN_POINT ( 'NONE',  ( 1.135170603674541256, 0.2952755905511811885, 0.1292274648535926551 ) ) ;
#34040 = CARTESIAN_POINT ( 'NONE',  ( 0.9317585301837276734, -0.4281496062992124485, 0.4176697321401328655 ) ) ;
#34041 = CARTESIAN_POINT ( 'NONE',  ( 1.246719160104987623, 0.05413385826771626580, -0.4176697321401330321 ) ) ;
#34042 = CARTESIAN_POINT ( 'NONE',  ( -0.3917322834645670104, -7.196005306013484475E-17, -0.5039370078740157410 ) ) ;
#34043 = CARTESIAN_POINT ( 'NONE',  ( 0.05249343832021075018, -0.5023911411419708095, 0.1820866141732285504 ) ) ;
#34044 = VERTEX_POINT ( 'NONE', #71647 ) ;
#34045 = CARTESIAN_POINT ( 'NONE',  ( 0.3420746716998660508, -0.1974969037888703871, -1.049868766404199460 ) ) ;
#34046 = ORIENTED_EDGE ( 'NONE', *, *, #59684, .F. ) ;
#34047 = CARTESIAN_POINT ( 'NONE',  ( -0.2690288713910754526, 0.1771653543307087075, -0.09757992244046823083 ) ) ;
#34048 = CARTESIAN_POINT ( 'NONE',  ( -0.05249343832020911260, 0.2306618581243848609, 0.2411417322834645549 ) ) ;
#34049 = CARTESIAN_POINT ( 'NONE',  ( -1.467262695449858212, 1.144328835045041570, 0.2657261524766077465 ) ) ;
#34050 = CARTESIAN_POINT ( 'NONE',  ( -0.2624671916010490880, 0.2306618581243847221, -0.2411417322834647770 ) ) ;
#34051 = CARTESIAN_POINT ( 'NONE',  ( -0.3083989501312330295, -0.05778040916215522460, 0.4822834645669289988 ) ) ;
#34052 = CARTESIAN_POINT ( 'NONE',  ( -0.9186351706036736120, -0.6046776061558809534, -0.2411417322834644161 ) ) ;
#34053 = CARTESIAN_POINT ( 'NONE',  ( -0.9842519685039365918, -0.6692913385826771977, 8.415575281601705876E-17 ) ) ;
#34054 = CARTESIAN_POINT ( 'NONE',  ( 1.561679790026247350, -0.004921259842519870586, -0.3153832671262229437 ) ) ;
#34055 = DIRECTION ( 'NONE',  ( 0.000000000000000000, 1.000000000000000000, 8.673617379884024625E-16 ) ) ;
#34056 = CARTESIAN_POINT ( 'NONE',  ( -0.3458507752293906723, -0.3458507752293910609, -2.736220472440943574 ) ) ;
#34057 = CARTESIAN_POINT ( 'NONE',  ( 0.4790026246719167324, -0.08942795157527998196, 0.3641732283464567121 ) ) ;
#34058 = AXIS2_PLACEMENT_3D ( 'NONE', #59248, #70207, #6235 ) ;
#34059 = CARTESIAN_POINT ( 'NONE',  ( 0.5118110236220480003, -0.6692913385826771977, 8.415575281601705876E-17 ) ) ;
#34060 = CARTESIAN_POINT ( 'NONE',  ( 0.5446194225721792126, -0.3162353388693405765, 0.4822834645669290543 ) ) ;
#34061 = ORIENTED_EDGE ( 'NONE', *, *, #20875, .F. ) ;
#34062 = CARTESIAN_POINT ( 'NONE',  ( -0.3460692066303960868, 0.1998031496062990242, -1.286089238845144367 ) ) ;
#34063 = CARTESIAN_POINT ( 'NONE',  ( -1.601049868766403650, -0.6046776061558807314, 0.2411417322834647770 ) ) ;
#34064 = CARTESIAN_POINT ( 'NONE',  ( 0.3996062992125986035, -0.1070741851644052972, -1.133202099737532720 ) ) ;
#34065 = CARTESIAN_POINT ( 'NONE',  ( 0.3460692066303958092, 0.1998031496062993018, -0.6804461942257218343 ) ) ;
#34066 = CARTESIAN_POINT ( 'NONE',  ( -0.5643044619422565855, 0.05413385826771626580, -0.4176697321401330321 ) ) ;
#34067 = CARTESIAN_POINT ( 'NONE',  ( 0.2362204724409449064, 0.4091458600556404646, 0.01312335958005249326 ) ) ;
#34068 = CARTESIAN_POINT ( 'NONE',  ( -0.2867679344610364334, -0.2867679344610367109, -2.190944881889763440 ) ) ;
#34069 = CARTESIAN_POINT ( 'NONE',  ( -1.568241469816272105, -0.2845877964562161244, -0.3641732283464567121 ) ) ;
#34070 = CARTESIAN_POINT ( 'NONE',  ( 0.7874015748031503170, -0.1870078740157479769, 0.4822834645669291653 ) ) ;
#34071 = CARTESIAN_POINT ( 'NONE',  ( 1.122047244094488860, -0.5400638737290845981, -0.3530559997133363437 ) ) ;
#34072 = CARTESIAN_POINT ( 'NONE',  ( -0.3937007874015740483, -0.1870078740157479769, 0.3641732283464567677 ) ) ;
#34073 = CARTESIAN_POINT ( 'NONE',  ( 0.4396325459317590445, -0.6692913385826771977, 0.1292274648535927661 ) ) ;
#34074 = CARTESIAN_POINT ( 'NONE',  ( -0.3458507752293909498, 0.3458507752293907833, -1.828740157480315265 ) ) ;
#34075 = CARTESIAN_POINT ( 'NONE',  ( 0.04593175853018440641, -0.5511811023622046335, 0.09757992244046803654 ) ) ;
#34076 = CARTESIAN_POINT ( 'NONE',  ( 0.02624671916010564918, 0.2306618581243848609, 0.2411417322834645549 ) ) ;
#34077 = AXIS2_PLACEMENT_3D ( 'NONE', #46441, #72131, #8993 ) ;
#34078 = CARTESIAN_POINT ( 'NONE',  ( 0.3949938075777409963, 2.418639510665530743E-17, -1.612204724409448842 ) ) ;
#34079 = CARTESIAN_POINT ( 'NONE',  ( 1.601049868766404982, 0.1283753931104748280, 0.1820866141732283561 ) ) ;
#34080 = CARTESIAN_POINT ( 'NONE',  ( 0.03280839895013198948, 0.1771653543307087630, 0.09757992244046791164 ) ) ;
#34082 = EDGE_CURVE ( 'NONE', #29058, #22351, #26941, .T. ) ;
#34081 = CARTESIAN_POINT ( 'NONE',  ( -0.8333333333333323711, -0.6692913385826773087, -0.1292274648535924053 ) ) ;
#34083 = CARTESIAN_POINT ( 'NONE',  ( -0.7217847769028863381, -0.3690944881889763329, 0.3153832671262228327 ) ) ;
#34084 = CARTESIAN_POINT ( 'NONE',  ( -0.4724409448818898682, -8.678599364036362592E-17, -2.320866141732283783 ) ) ;
#34085 = CARTESIAN_POINT ( 'NONE',  ( -0.7414698162729651543, 0.2952755905511810774, -0.1292274648535930714 ) ) ;
#34086 = CARTESIAN_POINT ( 'NONE',  ( -0.4855643044619415427, 0.05413385826771626580, -0.4176697321401330321 ) ) ;
#34087 = CARTESIAN_POINT ( 'NONE',  ( -0.1902887139107604098, 0.2952755905511810774, -0.1292274648535930714 ) ) ;
#34088 = CARTESIAN_POINT ( 'NONE',  ( 0.3996062992125984925, 0.1070741851644054637, -2.563648293963254776 ) ) ;
#34089 = CARTESIAN_POINT ( 'NONE',  ( -0.2867679344610366554, 0.2867679344610365444, -1.989481996554119059 ) ) ;
#34090 = CARTESIAN_POINT ( 'NONE',  ( -1.850381573804679824, 1.062979042929935281, 0.007789085821720239007 ) ) ;
#34091 = CARTESIAN_POINT ( 'NONE',  ( 0.8989501312335964611, 0.1771653543307087630, 0.09757992244046791164 ) ) ;
#34092 = CARTESIAN_POINT ( 'NONE',  ( 1.476377952755906220, 0.1660481256975883668, -0.3530559997133364547 ) ) ;
#34093 = CARTESIAN_POINT ( 'NONE',  ( -1.213910761154854745, 0.1771653543307087075, -0.09757992244046823083 ) ) ;
#34094 = CARTESIAN_POINT ( 'NONE',  ( 1.122047244094488860, -0.5400638737290845981, -0.3530559997133363437 ) ) ;
#34095 = CARTESIAN_POINT ( 'NONE',  ( -1.069553805774277722, 0.1771653543307087630, 0.09757992244046791164 ) ) ;
#34096 = CARTESIAN_POINT ( 'NONE',  ( -0.5118110236220466680, -0.6692913385826771977, 8.415575281601705876E-17 ) ) ;
#34097 = CARTESIAN_POINT ( 'NONE',  ( -0.05905511811023545637, 0.07958543189024085140, 0.2665933059059887866 ) ) ;
#34098 = CARTESIAN_POINT ( 'NONE',  ( -1.614173228346456712, 0.4410134679336886188, -0.1372047244094478091 ) ) ;
#34099 = CARTESIAN_POINT ( 'NONE',  ( 1.272965879265092637, -0.004921259842519576551, 0.3153832671262227771 ) ) ;
#34100 = EDGE_CURVE ( 'NONE', #7120, #73064, #72066, .T. ) ;
#34101 = B_SPLINE_CURVE_WITH_KNOTS ( 'NONE', 3,
 ( #36668, #24039, #49709, #72409, #20223, #71570, #21057, #53019, #32844, #1295, #19380, #52188, #13921, #77892, #14345, #32009, #65267, #20644, #14758, #33684, #1703, #8021, #7603, #57669, #63995, #31, #52606, #46297, #45872, #6336, #39577, #71992, #39150, #59346, #25684, #26945, #58513, #78313 ),
 .UNSPECIFIED., .F., .F.,
 ( 4, 2, 2, 2, 2, 2, 2, 2, 2, 2, 2, 2, 2, 2, 2, 2, 2, 2, 4 ),
 ( 7.825718265876660833E-19, 0.0009023223452592547779, 0.001804644690518508905, 0.002706967035777763791, 0.003609289381037018244, 0.004511611726296273564, 0.005413934071555528450, 0.006316256416814782469, 0.007218578762074037355, 0.008120901107333289640, 0.008572062279962877618, 0.009023223452592465596, 0.009925545797851638083, 0.01082786814311081230, 0.01173019048836998653, 0.01263251283362915901, 0.01353483517888833497, 0.01398599635151791254, 0.01443715752414749011 ),
 .UNSPECIFIED. ) ;
#34102 = CARTESIAN_POINT ( 'NONE',  ( 0.2362204724409456558, -0.1870078740157479769, 0.4822834645669291653 ) ) ;
#34103 = EDGE_CURVE ( 'NONE', #21631, #23049, #64914, .T. ) ;
#34104 = CARTESIAN_POINT ( 'NONE',  ( 0.1998031496062992463, 0.3460692066303959202, -0.3786089238845143923 ) ) ;
#34105 = CARTESIAN_POINT ( 'NONE',  ( -0.7545931758530177724, 0.2952755905511811885, 0.1292274648535926551 ) ) ;
#34106 = CARTESIAN_POINT ( 'NONE',  ( 0.2867679344610365999, 0.2867679344610365999, -1.482283464566929387 ) ) ;
#34107 = CARTESIAN_POINT ( 'NONE',  ( 0.8333333333333340365, 0.1771653543307087075, -0.09757992244046823083 ) ) ;
#34108 = CARTESIAN_POINT ( 'NONE',  ( 0.3346456692913393205, -0.5400638737290845981, -0.3530559997133363437 ) ) ;
#34109 = CARTESIAN_POINT ( 'NONE',  ( 0.06561679790026316017, -0.4281496062992124485, 0.4176697321401328655 ) ) ;
#34110 = CARTESIAN_POINT ( 'NONE',  ( -0.1640419947506553400, -0.08942795157528024563, -0.3641732283464568787 ) ) ;
#34111 = DIRECTION ( 'NONE',  ( -0.000000000000000000, 1.000000000000000000, -0.000000000000000000 ) ) ;
#34112 = CARTESIAN_POINT ( 'NONE',  ( -0.2230971128608915943, -0.004921259842519576551, 0.3153832671262227771 ) ) ;
#34113 = CARTESIAN_POINT ( 'NONE',  ( 0.6889763779527566800, -0.5400638737290844871, 0.3530559997133364547 ) ) ;
#34114 = CARTESIAN_POINT ( 'NONE',  ( -0.8661417322834640276, -0.1870078740157480601, -0.3641732283464567677 ) ) ;
#34115 = CARTESIAN_POINT ( 'NONE',  ( -0.3996062992125986590, 0.1070741851644051723, -1.054461942257217899 ) ) ;
#34116 = CARTESIAN_POINT ( 'NONE',  ( -0.9514435695538050464, -0.05778040916215560624, -0.4822834645669293319 ) ) ;
#34117 = DIRECTION ( 'NONE',  ( 0.7071067811865495711, -0.000000000000000000, -0.7071067811865454633 ) ) ;
#34118 = VERTEX_POINT ( 'NONE', #26612 ) ;
#34119 = AXIS2_PLACEMENT_3D ( 'NONE', #82038, #24352, #50842 ) ;
#34120 = CARTESIAN_POINT ( 'NONE',  ( -0.9055118110236215490, 0.1771653543307087630, 0.000000000000000000 ) ) ;
#34121 = CARTESIAN_POINT ( 'NONE',  ( -0.09186351706036689768, 0.05413385826771626580, -0.4176697321401330321 ) ) ;
#34122 = CARTESIAN_POINT ( 'NONE',  ( -1.509186351706035767, 0.05413385826771626580, -0.4176697321401330321 ) ) ;
#34123 = CARTESIAN_POINT ( 'NONE',  ( -0.9186351706036736120, -0.6046776061558809534, -0.2411417322834644161 ) ) ;
#34124 = DIRECTION ( 'NONE',  ( -0.000000000000000000, 1.000000000000000000, -0.000000000000000000 ) ) ;
#34126 = CARTESIAN_POINT ( 'NONE',  ( 1.082677165354331228, -0.5400638737290844871, 0.3530559997133364547 ) ) ;
#34125 = FACE_OUTER_BOUND ( 'NONE', #10458, .T. ) ;
#34127 = CARTESIAN_POINT ( 'NONE',  ( 0.8858267716535438430, 0.1660481256975885056, 0.3530559997133364547 ) ) ;
#34128 = CARTESIAN_POINT ( 'NONE',  ( -0.2690288713910753970, 0.2066929133858267098, -0.1054918080437494132 ) ) ;
#34129 = DIRECTION ( 'NONE',  ( 0.000000000000000000, 1.000000000000000000, -8.673617379884024625E-16 ) ) ;
#34130 = CARTESIAN_POINT ( 'NONE',  ( -1.325459317585300889, -0.4281496062992127816, -0.4176697321401328100 ) ) ;
#34131 = CARTESIAN_POINT ( 'NONE',  ( -0.1998031496062994683, 0.3460692066303958092, -0.4855643044619422644 ) ) ;
#34132 = EDGE_LOOP ( 'NONE', ( #10929, #66782, #82492, #27526 ) ) ;
#34133 = CARTESIAN_POINT ( 'NONE',  ( -0.7086614173228339419, -0.1870078740157479769, 0.3641732283464567677 ) ) ;
#34135 = CARTESIAN_POINT ( 'NONE',  ( -0.3392501089628017219, -0.1958661417322836718, -2.091863517060367439 ) ) ;
#34134 = AXIS2_PLACEMENT_3D ( 'NONE', #47155, #61037, #61452 ) ;
#34136 = VERTEX_POINT ( 'NONE', #45533 ) ;
#34137 = CARTESIAN_POINT ( 'NONE',  ( 0.8923884514435701520, -0.6046776061558809534, -0.2411417322834644161 ) ) ;
#34138 = CARTESIAN_POINT ( 'NONE',  ( 0.1968503937007881344, 0.2952755905511811885, 0.000000000000000000 ) ) ;
#34139 = CARTESIAN_POINT ( 'NONE',  ( -0.7480314960629914633, -0.6692913385826771977, 8.415575281601705876E-17 ) ) ;
#34140 = CARTESIAN_POINT ( 'NONE',  ( 1.509186351706037543, 0.05413385826771666132, 0.4176697321401328100 ) ) ;
#34141 = CARTESIAN_POINT ( 'NONE',  ( -1.062992125984250968, -0.5511811023622047445, 6.969142054262312111E-17 ) ) ;
#34142 = LINE ( 'NONE', #15628, #56073 ) ;
#34143 = CARTESIAN_POINT ( 'NONE',  ( 0.6364829396325465405, -0.3162353388693409650, -0.4822834645669289433 ) ) ;
#34144 = CARTESIAN_POINT ( 'NONE',  ( 0.3871391076115492380, -0.08942795157528024563, -0.3641732283464568787 ) ) ;
#34145 = CARTESIAN_POINT ( 'NONE',  ( -0.5380577427821514602, 0.05413385826771666132, 0.4176697321401328100 ) ) ;
#34146 = CARTESIAN_POINT ( 'NONE',  ( 0.3917322834645668994, -0.1049643490035303134, -0.9789833088900768976 ) ) ;
#34147 = CARTESIAN_POINT ( 'NONE',  ( -1.115485564304461219, 0.05413385826771626580, -0.4176697321401330321 ) ) ;
#34148 = CARTESIAN_POINT ( 'NONE',  ( -1.712598425196849572, 0.07958543189024085140, 0.2665933059059887866 ) ) ;
#34149 = CARTESIAN_POINT ( 'NONE',  ( 1.535433070866142558, 0.2952755905511811885, 0.000000000000000000 ) ) ;
#34150 = CARTESIAN_POINT ( 'NONE',  ( 1.299212598425197429, -0.5511811023622047445, 6.969142054262312111E-17 ) ) ;
#34151 = EDGE_LOOP ( 'NONE', ( #46461, #47788, #69413, #71087 ) ) ;
#34152 = CARTESIAN_POINT ( 'NONE',  ( -0.3392501089628017219, -0.1958661417322836995, -2.568916953577114359 ) ) ;
#34153 = CARTESIAN_POINT ( 'NONE',  ( 0.04593175853018440641, -0.6692913385826771977, 0.1292274648535927661 ) ) ;
#34154 = ORIENTED_EDGE ( 'NONE', *, *, #31271, .F. ) ;
#34155 = CARTESIAN_POINT ( 'NONE',  ( 0.8858267716535438430, -0.4536011799217368745, -0.2665933059059886201 ) ) ;
#34156 = CARTESIAN_POINT ( 'NONE',  ( -1.043307086614172707, 0.1660481256975883668, -0.3530559997133364547 ) ) ;
#34157 = CARTESIAN_POINT ( 'NONE',  ( 1.141732283464567566, 0.2952755905511811885, 0.000000000000000000 ) ) ;
#34158 = CARTESIAN_POINT ( 'NONE',  ( 0.6430446194225728496, 0.05413385826771666132, 0.4176697321401328100 ) ) ;
#34159 = CARTESIAN_POINT ( 'NONE',  ( 0.3412073490813655186, 0.2306618581243848609, 0.2411417322834645549 ) ) ;
#34160 = CARTESIAN_POINT ( 'NONE',  ( -0.4658792650918627265, -0.3162353388693409650, -0.4822834645669289433 ) ) ;
#34161 = CARTESIAN_POINT ( 'NONE',  ( -0.3917322834645669549, -0.1049643490035306603, -1.862860892388451761 ) ) ;
#34162 = CARTESIAN_POINT ( 'NONE',  ( -1.377952755905511140, 0.2952755905511811885, 0.000000000000000000 ) ) ;
#34163 = CARTESIAN_POINT ( 'NONE',  ( -0.5249343832020990641, 0.2306618581243848609, 0.2411417322834645549 ) ) ;
#34164 = CARTESIAN_POINT ( 'NONE',  ( -0.3608923884514428360, 0.1771653543307087630, 0.09757992244046791164 ) ) ;
#34165 = DIRECTION ( 'NONE',  ( 0.000000000000000000, 0.000000000000000000, -1.000000000000000000 ) ) ;
#34166 = CARTESIAN_POINT ( 'NONE',  ( 0.3917322834645670104, -0.1049643490035303411, -2.938320209973753538 ) ) ;
#34167 = CARTESIAN_POINT ( 'NONE',  ( -0.4133858267716528645, 0.1660481256975883668, -0.3530559997133364547 ) ) ;
#34168 = CARTESIAN_POINT ( 'NONE',  ( -2.362204724409448620, 0.03937007874015751446, -0.5118110236220719811 ) ) ;
#34169 = CARTESIAN_POINT ( 'NONE',  ( 0.7480314960629927956, -0.6692913385826771977, 8.415575281601705876E-17 ) ) ;
#34170 = CARTESIAN_POINT ( 'NONE',  ( -0.1070741851644056997, 0.3996062992125986035, -1.738845144356955696 ) ) ;
#34171 = CARTESIAN_POINT ( 'NONE',  ( 3.937005118394719005, 1.063014994214472431, -0.03171225910627740313 ) ) ;
#34172 = CARTESIAN_POINT ( 'NONE',  ( -0.3412073490813641308, 0.2306618581243847221, -0.2411417322834647770 ) ) ;
#34174 = LINE ( 'NONE', #16802, #50551 ) ;
#34173 = CARTESIAN_POINT ( 'NONE',  ( 1.082677165354331228, 0.07958543189024071263, -0.2665933059059888421 ) ) ;
#34175 = CARTESIAN_POINT ( 'NONE',  ( -0.3458507752293909498, 0.3458507752293907833, -0.5688976377952755792 ) ) ;
#34176 = CARTESIAN_POINT ( 'NONE',  ( 1.299212598425197429, -0.5511811023622047445, 6.969142054262312111E-17 ) ) ;
#34177 = CARTESIAN_POINT ( 'NONE',  ( 1.227034120734908917, -0.6692913385826771977, 0.1292274648535927661 ) ) ;
#34178 = CARTESIAN_POINT ( 'NONE',  ( -0.2891555358219911054, 0.2891555358219909388, -0.2539370078740157410 ) ) ;
#34179 = CARTESIAN_POINT ( 'NONE',  ( -0.3412073490813641308, -0.6046776061558807314, 0.2411417322834647770 ) ) ;
#34180 = CARTESIAN_POINT ( 'NONE',  ( -1.443569553805773564, 0.2306618581243847221, -0.2411417322834647770 ) ) ;
#34181 = AXIS2_PLACEMENT_3D ( 'NONE', #17509, #43141, #24206 ) ;
#34182 = CARTESIAN_POINT ( 'NONE',  ( -1.679790026246718693, 0.2306618581243847221, -0.2411417322834647770 ) ) ;
#34183 = CARTESIAN_POINT ( 'NONE',  ( -0.3280839895013117347, -0.4281496062992124485, 0.4176697321401328655 ) ) ;
#34184 = CARTESIAN_POINT ( 'NONE',  ( -0.1974969037888704149, -0.3420746716998661063, -0.2998687664041995715 ) ) ;
#34185 = CARTESIAN_POINT ( 'NONE',  ( 1.377952755905512472, 0.2952755905511811885, 0.000000000000000000 ) ) ;
#34186 = CARTESIAN_POINT ( 'NONE',  ( 0.5708661417322841158, -0.5400638737290845981, -0.3530559997133363437 ) ) ;
#34187 = CARTESIAN_POINT ( 'NONE',  ( 0.4790026246719168435, -0.2845877964562161244, -0.3641732283464567121 ) ) ;
#34188 = CARTESIAN_POINT ( 'NONE',  ( -0.4724409448818896462, -0.1265901696524993070, -0.1227034120734908362 ) ) ;
#34189 = CARTESIAN_POINT ( 'NONE',  ( 0.2887139107611556010, 0.1283753931104746893, -0.1820866141732285504 ) ) ;
#34190 = DIRECTION ( 'NONE',  ( 0.000000000000000000, 0.000000000000000000, -1.000000000000000000 ) ) ;
#34191 = CARTESIAN_POINT ( 'NONE',  ( 0.1998031496062992463, 0.3460692066303959202, -1.480971128608923992 ) ) ;
#34192 = CARTESIAN_POINT ( 'NONE',  ( 0.9645669291338591078, -0.5400638737290845981, -0.3530559997133363437 ) ) ;
#34193 = CARTESIAN_POINT ( 'NONE',  ( -0.1049643490035307020, 0.3917322834645669549, -0.6286089238845143923 ) ) ;
#34194 = CARTESIAN_POINT ( 'NONE',  ( 0.3503937007874015630, 0.3051181102362204856, -0.01968503937007903132 ) ) ;
#34195 = CARTESIAN_POINT ( 'NONE',  ( -0.3280839895013117347, 0.009842519685039147898, -0.3409548833797004797 ) ) ;
#34196 = CARTESIAN_POINT ( 'NONE',  ( -0.1049868766404193215, 0.1283753931104746893, -0.1820866141732285504 ) ) ;
#34197 = CIRCLE ( 'NONE', #77198, 3.582677165354330562 ) ;
#34198 = CARTESIAN_POINT ( 'NONE',  ( 0.3346456692913393205, -0.5400638737290845981, -0.3530559997133363437 ) ) ;
#34199 =( REPRESENTATION_RELATIONSHIP ('NONE','NONE', #79348, #82043 ) REPRESENTATION_RELATIONSHIP_WITH_TRANSFORMATION ( #24536 )SHAPE_REPRESENTATION_RELATIONSHIP( ) );
#34200 = CARTESIAN_POINT ( 'NONE',  ( 1.450131233595801428, -0.5511811023622048555, -0.09757992244046775898 ) ) ;
#34201 = CARTESIAN_POINT ( 'NONE',  ( -0.8136482939632537770, -0.5023911411419708095, 0.1820866141732285504 ) ) ;
#34202 = CARTESIAN_POINT ( 'NONE',  ( -0.9776902887139098386, -0.6692913385826771977, 0.1292274648535927661 ) ) ;
#34203 = CARTESIAN_POINT ( 'NONE',  ( -1.384514435695537005, 0.2952755905511811885, 0.1292274648535926551 ) ) ;
#34204 = CARTESIAN_POINT ( 'NONE',  ( 0.3346456692913393205, -0.5400638737290845981, -0.3530559997133363437 ) ) ;
#34205 = CARTESIAN_POINT ( 'NONE',  ( 1.423884514435696413, -0.3162353388693409650, -0.4822834645669289433 ) ) ;
#34206 = CARTESIAN_POINT ( 'NONE',  ( 1.035593395983585907, 1.340617077144278024, -0.4319465832450602449 ) ) ;
#34207 = CARTESIAN_POINT ( 'NONE',  ( 0.4133858267716541968, -0.5400638737290845981, -0.3530559997133363437 ) ) ;
#34208 = CARTESIAN_POINT ( 'NONE',  ( -0.2362204724409447953, -0.4091458600556404646, -2.819553805774277944 ) ) ;
#34209 = CARTESIAN_POINT ( 'NONE',  ( 1.640419947506562393, -0.4281496062992124485, 0.4176697321401328655 ) ) ;
#34210 = CARTESIAN_POINT ( 'NONE',  ( 1.318897637795276356, -0.5400638737290844871, 0.3530559997133364547 ) ) ;
#34211 = CARTESIAN_POINT ( 'NONE',  ( -1.423884514435694859, -0.2845877964562159024, 0.3641732283464567677 ) ) ;
#34212 = CARTESIAN_POINT ( 'NONE',  ( 1.148293963254593875, -0.5511811023622046335, 0.09757992244046803654 ) ) ;
#34213 = CARTESIAN_POINT ( 'NONE',  ( -1.167979002624671470, -0.004921259842519576551, 0.3153832671262227771 ) ) ;
#34214 = CARTESIAN_POINT ( 'NONE',  ( -0.8136482939632537770, 0.1283753931104746893, -0.1820866141732285504 ) ) ;
#34215 = FACE_OUTER_BOUND ( 'NONE', #26775, .T. ) ;
#34216 = CARTESIAN_POINT ( 'NONE',  ( 0.6299212598425204535, -0.1870078740157479769, 0.3641732283464567677 ) ) ;
#34217 = CARTESIAN_POINT ( 'NONE',  ( 0.3280839895013130669, -0.4281496062992127816, -0.4176697321401328100 ) ) ;
#34218 = CARTESIAN_POINT ( 'NONE',  ( 0.9383202099737536495, -0.3162353388693405765, 0.4822834645669290543 ) ) ;
#34219 = ADVANCED_FACE ( 'NONE', ( #44686 ), #16733, .F. ) ;
#34220 = CARTESIAN_POINT ( 'NONE',  ( 0.1115485564304470323, 0.2952755905511811885, 0.1292274648535926551 ) ) ;
#34221 = CARTESIAN_POINT ( 'NONE',  ( 0.01312335958005323398, -0.004921259842519576551, 0.3153832671262227771 ) ) ;
#34222 = B_SPLINE_CURVE_WITH_KNOTS ( 'NONE', 3,
 ( #43454, #23700, #68741, #69152 ),
 .UNSPECIFIED., .F., .F.,
 ( 4, 4 ),
 ( 3.210432057660995322E-07, 0.001287787053612077974 ),
 .UNSPECIFIED. ) ;
#34223 = CARTESIAN_POINT ( 'NONE',  ( 1.384514435695538337, -0.6692913385826771977, 0.1292274648535927661 ) ) ;
#34224 = DIRECTION ( 'NONE',  ( -1.000000000000000000, -3.469446951953613696E-16, 0.000000000000000000 ) ) ;
#34225 = CARTESIAN_POINT ( 'NONE',  ( -1.003937007874015297, -0.5400638737290845981, -0.3530559997133363437 ) ) ;
#34226 = CARTESIAN_POINT ( 'NONE',  ( 0.3460692066303959202, 0.1998031496062993295, -0.7611548556430446366 ) ) ;
#34227 = CARTESIAN_POINT ( 'NONE',  ( 0.2952755905511810774, 3.597759587968672259E-17, 5.524802951929911998 ) ) ;
#34228 = CARTESIAN_POINT ( 'NONE',  ( -0.8398950131233585692, 0.2306618581243848609, 0.2411417322834645549 ) ) ;
#34229 = CARTESIAN_POINT ( 'NONE',  ( -0.1706036745406816491, -0.4281496062992124485, 0.4176697321401328655 ) ) ;
#34230 = EDGE_CURVE ( 'NONE', #51195, #67389, #1410, .T. ) ;
#34231 = CARTESIAN_POINT ( 'NONE',  ( -0.3996062992125987146, 0.1070741851644051862, -2.709973753280840114 ) ) ;
#34232 = CARTESIAN_POINT ( 'NONE',  ( -0.3420746716998661618, 0.1974969037888702206, -2.230971128608923770 ) ) ;
#34233 = EDGE_LOOP ( 'NONE', ( #73083, #2368, #62949, #56776, #78783, #5722, #57735, #81684, #80032, #56599, #77117, #53494 ) ) ;
#34234 = CARTESIAN_POINT ( 'NONE',  ( 4.797336870675656522E-17, -0.3917322834645670104, -1.015748031496062964 ) ) ;
#34235 = CARTESIAN_POINT ( 'NONE',  ( 3.870235431238101764, 2.740199102106095186, -0.5314960629921260393 ) ) ;
#34236 = ADVANCED_FACE ( 'NONE', ( #42151 ), #2627, .F. ) ;
#34237 = CARTESIAN_POINT ( 'NONE',  ( -1.207349081364828880, 0.1283753931104746893, -0.1820866141732285504 ) ) ;
#34238 = CARTESIAN_POINT ( 'NONE',  ( 0.1049643490035303689, 0.3917322834645670104, -0.9304461942257216123 ) ) ;
#34239 = CARTESIAN_POINT ( 'NONE',  ( -1.581364829396324945, -0.3162353388693405765, 0.4822834645669290543 ) ) ;
#34240 = CARTESIAN_POINT ( 'NONE',  ( -0.3392501089628019439, 0.1958661417322832554, 0.2086807331046737768 ) ) ;
#34241 = CARTESIAN_POINT ( 'NONE',  ( 0.1377952755905518800, 0.1660481256975883668, -0.3530559997133364547 ) ) ;
#34242 = CARTESIAN_POINT ( 'NONE',  ( -0.3608923884514428360, -0.5511811023622048555, -0.09757992244046775898 ) ) ;
#34243 = CARTESIAN_POINT ( 'NONE',  ( 0.8661417322834652488, -0.1870078740157480879, -0.4822834645669291653 ) ) ;
#34244 = CARTESIAN_POINT ( 'NONE',  ( 0.3805774278215230400, 0.05413385826771626580, -0.4176697321401330321 ) ) ;
#34245 = CARTESIAN_POINT ( 'NONE',  ( 0.4259733500547865370, 1.326302081955849310, 1.038124814314992372 ) ) ;
#34246 = CARTESIAN_POINT ( 'NONE',  ( 0.3460692066303959757, -0.1998031496062991907, -2.467191601049868677 ) ) ;
#34247 = CARTESIAN_POINT ( 'NONE',  ( -0.2867679344610365444, -0.2867679344610367664, -1.315636113682101982 ) ) ;
#34248 = CARTESIAN_POINT ( 'NONE',  ( 1.102362204724410155, -0.1870078740157480879, -0.4822834645669291653 ) ) ;
#34249 = CARTESIAN_POINT ( 'NONE',  ( 0.1443569553805781891, -0.4281496062992124485, 0.4176697321401328655 ) ) ;
#34250 = CARTESIAN_POINT ( 'NONE',  ( -1.194225721784776262, -0.4281496062992124485, 0.4176697321401328655 ) ) ;
#34252 = CARTESIAN_POINT ( 'NONE',  ( 1.351706036745407458, -0.4281496062992127816, -0.4176697321401328100 ) ) ;
#34251 = VECTOR ( 'NONE', #1047, 39.37007874015748143 ) ;
#34253 = CARTESIAN_POINT ( 'NONE',  ( 1.089238845144357759, 0.05413385826771626580, -0.4176697321401330321 ) ) ;
#34254 = CARTESIAN_POINT ( 'NONE',  ( 0.2867679344610365999, 0.2867679344610365999, -0.5374015748031496509 ) ) ;
#34255 = CARTESIAN_POINT ( 'NONE',  ( 0.02624671916010564918, 0.2306618581243848609, 0.2411417322834645549 ) ) ;
#34256 = CARTESIAN_POINT ( 'NONE',  ( 0.6167979002624679463, 0.05413385826771626580, -0.4176697321401330321 ) ) ;
#34257 = CARTESIAN_POINT ( 'NONE',  ( 8.195543980992789655E-16, -0.1870078740157480879, -0.4822834645669291653 ) ) ;
#34258 = CARTESIAN_POINT ( 'NONE',  ( 0.5577427821522316087, -0.08942795157527998196, 0.3641732283464567121 ) ) ;
#34259 = CARTESIAN_POINT ( 'NONE',  ( -1.207349081364828880, 0.2306618581243847221, -0.2411417322834647770 ) ) ;
#34260 = CARTESIAN_POINT ( 'NONE',  ( -1.338582677165353729, -0.1870078740157480879, -0.4822834645669291653 ) ) ;
#34261 = CARTESIAN_POINT ( 'NONE',  ( 0.7742782152230978099, -0.4281496062992124485, 0.4176697321401328655 ) ) ;
#34262 = CARTESIAN_POINT ( 'NONE',  ( -0.3021538998208400661, -0.2502216998138593884, -1.929133858267717549 ) ) ;
#34263 = ADVANCED_FACE ( 'NONE', ( #53112 ), #79658, .F. ) ;
#34264 = CARTESIAN_POINT ( 'NONE',  ( 0.1049643490035304938, -0.3917322834645669549, -1.967191601049868899 ) ) ;
#34265 = ORIENTED_EDGE ( 'NONE', *, *, #31679, .T. ) ;
#34266 = CARTESIAN_POINT ( 'NONE',  ( 0.3460692066303959202, 0.1998031496062993295, -0.4461942257217847430 ) ) ;
#34267 = ORIENTED_EDGE ( 'NONE', *, *, #30068, .T. ) ;
#34268 = CARTESIAN_POINT ( 'NONE',  ( 1.128608923884515169, -0.6046776061558809534, -0.2411417322834644161 ) ) ;
#34269 = CARTESIAN_POINT ( 'NONE',  ( 0.4790026246719167324, -0.08942795157527998196, 0.3641732283464567121 ) ) ;
#34270 = CARTESIAN_POINT ( 'NONE',  ( -0.7763038905084325147, -3.623651218081290895E-15, 0.3954974714151467952 ) ) ;
#34271 = CARTESIAN_POINT ( 'NONE',  ( 0.4581548248993063122, 1.775897345035375441, -0.5309055118110237448 ) ) ;
#34272 = CARTESIAN_POINT ( 'NONE',  ( -1.614173228346457378, 0.5038684218300933937, -0.1372047244094477536 ) ) ;
#34273 = CARTESIAN_POINT ( 'NONE',  ( -0.1049643490035302024, -0.3917322834645671215, -1.416666666666666519 ) ) ;
#34274 = EDGE_CURVE ( 'NONE', #66374, #32472, #21150, .T. ) ;
#34275 = CARTESIAN_POINT ( 'NONE',  ( -0.3972027188793493813, -0.005815251566504483528, -1.929133858265299262 ) ) ;
#34276 = CARTESIAN_POINT ( 'NONE',  ( -0.2230971128608915943, -0.4281496062992127816, -0.4176697321401328100 ) ) ;
#34277 = CARTESIAN_POINT ( 'NONE',  ( 1.213910761154856299, -0.6692913385826773087, -0.1292274648535924053 ) ) ;
#34278 = EDGE_LOOP ( 'NONE', ( #32227, #22264, #54634, #50056 ) ) ;
#34279 = CARTESIAN_POINT ( 'NONE',  ( -1.371391076115484831, 0.2952755905511810774, -0.1292274648535930714 ) ) ;
#34280 = CARTESIAN_POINT ( 'NONE',  ( -1.024260578284143186, 1.413296633437248984, -0.4581541405492637331 ) ) ;
#34281 = DIRECTION ( 'NONE',  ( 3.876322972432713694E-31, 1.000000000000000000, -5.551115123125781470E-17 ) ) ;
#34282 = CARTESIAN_POINT ( 'NONE',  ( -9.787531504996566615E-17, 0.3996062992125985480, -2.124015748031496287 ) ) ;
#34283 = CARTESIAN_POINT ( 'NONE',  ( -1.423884514435694859, -0.08942795157528024563, -0.3641732283464568787 ) ) ;
#34284 = EDGE_CURVE ( 'NONE', #30161, #23065, #25288, .T. ) ;
#34285 = CARTESIAN_POINT ( 'NONE',  ( -1.561679790026246017, -0.4281496062992127816, -0.4176697321401328100 ) ) ;
#34286 = CARTESIAN_POINT ( 'NONE',  ( 0.2099737532808405305, -0.6046776061558807314, 0.2411417322834647770 ) ) ;
#34287 = ORIENTED_EDGE ( 'NONE', *, *, #39222, .T. ) ;
#34289 = CARTESIAN_POINT ( 'NONE',  ( -0.4527559055118102749, 0.1012011053420777407, 0.2882089793578257453 ) ) ;
#34288 = CARTESIAN_POINT ( 'NONE',  ( 1.640419947506562393, -0.4281496062992124485, 0.4176697321401328655 ) ) ;
#34290 = CARTESIAN_POINT ( 'NONE',  ( -0.5511811023622041894, -0.1870078740157480601, -0.3641732283464567677 ) ) ;
#34291 =( BOUNDED_CURVE ( )  B_SPLINE_CURVE ( 1, ( #65504, #26762 ),
 .UNSPECIFIED., .F., .F. ) 
 B_SPLINE_CURVE_WITH_KNOTS ( ( 2, 2 ),
 ( 0.000000000000000000, 0.002000000000000008715 ),
 .UNSPECIFIED. ) 
 CURVE ( )  GEOMETRIC_REPRESENTATION_ITEM ( )  RATIONAL_B_SPLINE_CURVE ( ( 0.9875488213027527884, 0.9875488213027527884 ) ) 
 REPRESENTATION_ITEM ( '' )  );
#34292 = CARTESIAN_POINT ( 'NONE',  ( 0.7939632545931766261, -0.3162353388693409650, -0.4822834645669289433 ) ) ;
#34293 = CARTESIAN_POINT ( 'NONE',  ( 1.574803149606299746, -0.1870078740157479769, 0.3641732283464567677 ) ) ;
#34294 = CARTESIAN_POINT ( 'NONE',  ( 0.3392501089628018329, 0.1958661417322835052, -1.313628978181415441 ) ) ;
#34295 = CARTESIAN_POINT ( 'NONE',  ( -0.8727034120734901146, -0.08942795157528024563, -0.3641732283464568787 ) ) ;
#34296 = CARTESIAN_POINT ( 'NONE',  ( -1.620734908136482577, 0.1771653543307087630, 0.09757992244046791164 ) ) ;
#34297 = CARTESIAN_POINT ( 'NONE',  ( 0.3917322834645669549, 0.1049643490035304660, -1.154199475065616820 ) ) ;
#34298 = CARTESIAN_POINT ( 'NONE',  ( 0.5511811023622054106, -0.1870078740157480879, -0.4822834645669291653 ) ) ;
#34299 = CARTESIAN_POINT ( 'NONE',  ( -0.7874015748031489847, -0.1870078740157480601, -0.3641732283464567677 ) ) ;
#34300 = CARTESIAN_POINT ( 'NONE',  ( -0.1246719160104980823, 0.1771653543307087630, 0.09757992244046791164 ) ) ;
#34301 = CARTESIAN_POINT ( 'NONE',  ( -0.1115485564304456306, 0.2952755905511810774, -0.1292274648535930714 ) ) ;
#34302 = CARTESIAN_POINT ( 'NONE',  ( -1.515748031496062076, -0.4536011799217367080, 0.2665933059059888421 ) ) ;
#34303 = CARTESIAN_POINT ( 'NONE',  ( 4.797336870675656522E-17, -0.3917322834645670659, 0.08200168159348891761 ) ) ;
#34304 = CARTESIAN_POINT ( 'NONE',  ( 0.5708661417322841158, -0.5400638737290845981, -0.3530559997133363437 ) ) ;
#34305 = CARTESIAN_POINT ( 'NONE',  ( -1.653543307086613234, -0.1870078740157479769, 0.4822834645669291653 ) ) ;
#34306 = CARTESIAN_POINT ( 'NONE',  ( 0.2362204724409449064, 0.4091458600556404646, -1.638451443569553634 ) ) ;
#34307 = CARTESIAN_POINT ( 'NONE',  ( -0.6889763779527552368, -0.5400638737290845981, -0.3530559997133363437 ) ) ;
#34308 = CARTESIAN_POINT ( 'NONE',  ( 0.01312335958005323398, -0.004921259842519576551, 0.3153832671262227771 ) ) ;
#34309 = CARTESIAN_POINT ( 'NONE',  ( -1.469816272965878357, 0.2306618581243848609, 0.2411417322834645549 ) ) ;
#34310 = CARTESIAN_POINT ( 'NONE',  ( 0.5708661417322842269, 0.07958543189024085140, 0.2665933059059887866 ) ) ;
#34311 = CONICAL_SURFACE ( 'NONE', #26240, 1.220472440944881942, 0.7853981633974621568 ) ;
#34312 = CARTESIAN_POINT ( 'NONE',  ( -0.7283464566929126471, 0.07958543189024071263, -0.2665933059059888421 ) ) ;
#34313 = CARTESIAN_POINT ( 'NONE',  ( -1.174540682414697335, -0.3162353388693409650, -0.4822834645669289433 ) ) ;
#34314 = CARTESIAN_POINT ( 'NONE',  ( -1.686351706036744558, 0.2952755905511810774, -0.1292274648535930714 ) ) ;
#34315 = CARTESIAN_POINT ( 'NONE',  ( 1.437007874015748810, -0.5400638737290845981, -0.3530559997133363437 ) ) ;
#34316 = DIRECTION ( 'NONE',  ( 0.000000000000000000, 0.000000000000000000, 1.000000000000000000 ) ) ;
#34317 = CARTESIAN_POINT ( 'NONE',  ( 0.8858267716535438430, 0.07958543189024085140, 0.2665933059059887866 ) ) ;
#34318 = CARTESIAN_POINT ( 'NONE',  ( 0.4068241469816281097, 0.05413385826771666132, 0.4176697321401328100 ) ) ;
#34319 = CARTESIAN_POINT ( 'NONE',  ( -1.437007874015747477, 0.1660481256975883668, -0.3530559997133364547 ) ) ;
#34320 = CARTESIAN_POINT ( 'NONE',  ( 1.364829396325459854, -0.5023911411419708095, -0.1820866141732282451 ) ) ;
#34321 = VERTEX_POINT ( 'NONE', #15677 ) ;
#34322 = CARTESIAN_POINT ( 'NONE',  ( -0.1070741851644056997, 0.3996062992125984925, -2.760498687664041384 ) ) ;
#34323 = CARTESIAN_POINT ( 'NONE',  ( -1.253280839895012377, -0.2845877964562161244, -0.3641732283464567121 ) ) ;
#34324 = CARTESIAN_POINT ( 'NONE',  ( -0.2887139107611542133, -0.6046776061558809534, -0.2411417322834644161 ) ) ;
#34325 = CARTESIAN_POINT ( 'NONE',  ( 0.4986876640419954376, 0.2306618581243848609, 0.2411417322834645549 ) ) ;
#34326 = CARTESIAN_POINT ( 'NONE',  ( -1.377952755905511140, 0.1771653543307087630, 0.000000000000000000 ) ) ;
#34327 = CARTESIAN_POINT ( 'NONE',  ( -0.3996062992125984925, -0.1070741851644056858, -1.697506561679790194 ) ) ;
#34328 = CARTESIAN_POINT ( 'NONE',  ( -1.227034120734907585, 0.2952755905511811885, 0.1292274648535926551 ) ) ;
#34329 = CARTESIAN_POINT ( 'NONE',  ( 0.3280839895013130669, -0.4281496062992127816, -0.4176697321401328100 ) ) ;
#34330 = CARTESIAN_POINT ( 'NONE',  ( 0.05905511811023709395, -0.5400638737290844871, 0.3530559997133364547 ) ) ;
#34331 = CARTESIAN_POINT ( 'NONE',  ( 1.384514435695538337, -0.6692913385826771977, 0.1292274648535927661 ) ) ;
#34333 = EDGE_CURVE ( 'NONE', #58442, #27207, #33664, .T. ) ;
#34332 = CARTESIAN_POINT ( 'NONE',  ( -0.3460692066303960313, 0.1998031496062989965, -1.047900262467191590 ) ) ;
#34334 = CARTESIAN_POINT ( 'NONE',  ( -0.3460692066303960868, 0.1998031496062990242, -1.286089238845144367 ) ) ;
#34335 = CARTESIAN_POINT ( 'NONE',  ( 0.2891555358219910499, 0.2891555358219910499, -0.7677165354330709457 ) ) ;
#34336 = CARTESIAN_POINT ( 'NONE',  ( -0.3392501089628017219, -0.1958661417322836718, -0.2020997375328083545 ) ) ;
#34337 = CARTESIAN_POINT ( 'NONE',  ( -0.3149606299212590610, -0.1870078740157479769, 0.3641732283464567677 ) ) ;
#34338 = CARTESIAN_POINT ( 'NONE',  ( -0.3937007874015740483, -0.1870078740157480879, -0.4822834645669291653 ) ) ;
#34339 = CARTESIAN_POINT ( 'NONE',  ( 1.036745406824147508, -0.4281496062992127816, -0.4176697321401328100 ) ) ;
#34340 = CARTESIAN_POINT ( 'NONE',  ( -0.3949938075777409963, -7.255918531996591613E-17, -1.848425196850393970 ) ) ;
#34341 = CARTESIAN_POINT ( 'NONE',  ( 0.09186351706036827158, -0.004921259842519576551, 0.3153832671262227771 ) ) ;
#34342 = CARTESIAN_POINT ( 'NONE',  ( -1.220472440944881054, -0.6692913385826771977, 8.415575281601705876E-17 ) ) ;
#34343 = CARTESIAN_POINT ( 'NONE',  ( 1.548556430446194954, -0.6046776061558807314, 0.2411417322834647770 ) ) ;
#34344 = CARTESIAN_POINT ( 'NONE',  ( -0.2362204724409447953, -0.4091458600556404646, -1.955380577427821454 ) ) ;
#34345 = CARTESIAN_POINT ( 'NONE',  ( 0.3486222174624411529, -0.1789624963018366099, -2.755905511811023612 ) ) ;
#34346 = ORIENTED_EDGE ( 'NONE', *, *, #3777, .T. ) ;
#34347 = ORIENTED_EDGE ( 'NONE', *, *, #51054, .F. ) ;
#34348 = CARTESIAN_POINT ( 'NONE',  ( 1.253280839895013710, -0.3162353388693405765, 0.4822834645669290543 ) ) ;
#34349 = CARTESIAN_POINT ( 'NONE',  ( 1.528871391076116026, -0.5511811023622048555, -0.09757992244046775898 ) ) ;
#34351 = CARTESIAN_POINT ( 'NONE',  ( -1.377952755905511140, -0.6692913385826771977, 8.415575281601705876E-17 ) ) ;
#34350 = CARTESIAN_POINT ( 'NONE',  ( -1.377952755905511140, -0.5511811023622047445, 6.969142054262312111E-17 ) ) ;
#34352 = CARTESIAN_POINT ( 'NONE',  ( 0.2867679344610365999, 0.2867679344610365999, -2.580033177656481325 ) ) ;
#34353 = DIRECTION ( 'NONE',  ( 1.000000000000000000, -0.000000000000000000, -0.000000000000000000 ) ) ;
#34354 = CARTESIAN_POINT ( 'NONE',  ( 1.128608923884515169, -0.6046776061558809534, -0.2411417322834644161 ) ) ;
#34355 = CARTESIAN_POINT ( 'NONE',  ( -1.502624671916009680, -0.05778040916215560624, -0.4822834645669293319 ) ) ;
#34356 = CARTESIAN_POINT ( 'NONE',  ( -0.2493438320209966919, 0.05413385826771626580, -0.4176697321401330321 ) ) ;
#34357 = CARTESIAN_POINT ( 'NONE',  ( -0.03280839895013062252, -0.6692913385826771977, 0.1292274648535927661 ) ) ;
#34358 = CARTESIAN_POINT ( 'NONE',  ( -1.240157480314959759, -0.5400638737290845981, -0.3530559997133363437 ) ) ;
#34359 = CARTESIAN_POINT ( 'NONE',  ( -0.2867679344610364334, -0.2867679344610368219, -2.658773335136795701 ) ) ;
#34360 = CARTESIAN_POINT ( 'NONE',  ( 0.4133858267716541968, -0.5400638737290845981, -0.3530559997133363437 ) ) ;
#34361 = CARTESIAN_POINT ( 'NONE',  ( 0.3917322834645669549, 0.1049643490035304660, -1.849081364829396223 ) ) ;
#34362 = CARTESIAN_POINT ( 'NONE',  ( -1.233595800524933894, -0.5023911411419708095, -0.1820866141732282451 ) ) ;
#34363 = VERTEX_POINT ( 'NONE', #15260 ) ;
#34364 = CARTESIAN_POINT ( 'NONE',  ( -0.3949938075777409408, -0.1058382717557502933, -2.408136482939633449 ) ) ;
#34365 = ORIENTED_EDGE ( 'NONE', *, *, #3552, .F. ) ;
#34366 = LINE ( 'NONE', #8696, #4545 ) ;
#34367 = AXIS2_PLACEMENT_3D ( 'NONE', #835, #1256, #6711 ) ;
#34368 = CARTESIAN_POINT ( 'NONE',  ( -1.102362204724408601, -0.1870078740157479769, 0.4822834645669291653 ) ) ;
#34369 = CARTESIAN_POINT ( 'NONE',  ( -1.292650918635170010, 0.2952755905511810774, -0.1292274648535930714 ) ) ;
#34370 = CARTESIAN_POINT ( 'NONE',  ( 0.1998031496062994405, -0.3460692066303958092, -0.4068241469816273326 ) ) ;
#34371 = CARTESIAN_POINT ( 'NONE',  ( -1.541994750656167090, 0.2952755905511811885, 0.1292274648535926551 ) ) ;
#34372 = DIRECTION ( 'NONE',  ( -1.000000000000000000, -0.000000000000000000, -0.000000000000000000 ) ) ;
#34373 = CARTESIAN_POINT ( 'NONE',  ( -3.937007874015748143, 1.724409448818898127, -0.6299212598425202314 ) ) ;
#34374 = CARTESIAN_POINT ( 'NONE',  ( -0.3265464962716608799, 0.02791078216816347476, -0.4328096321851898631 ) ) ;
#34375 = CARTESIAN_POINT ( 'NONE',  ( -0.1958661417322834220, -0.3392501089628018884, 0.007217847769028785422 ) ) ;
#34376 = CARTESIAN_POINT ( 'NONE',  ( -0.07874015748031421014, -0.1870078740157479769, 0.3641732283464567677 ) ) ;
#34377 = CARTESIAN_POINT ( 'NONE',  ( -0.7939632545931754048, -0.2845877964562159024, 0.3641732283464567677 ) ) ;
#34378 = CARTESIAN_POINT ( 'NONE',  ( -1.371391076115484609, -0.6692913385826771977, 0.1292274648535927661 ) ) ;
#34379 = CARTESIAN_POINT ( 'NONE',  ( 1.108923884514436242, -0.05778040916215522460, 0.4822834645669289988 ) ) ;
#34380 = CARTESIAN_POINT ( 'NONE',  ( -0.7283464566929126471, -0.5400638737290844871, 0.3530559997133364547 ) ) ;
#34381 = CARTESIAN_POINT ( 'NONE',  ( 0.5314960629921392510, 2.753420937170568461, -3.841955293929014026 ) ) ;
#34382 = ORIENTED_EDGE ( 'NONE', *, *, #76459, .F. ) ;
#34383 = CARTESIAN_POINT ( 'NONE',  ( -1.496062992125983815, -0.1870078740157479769, 0.4822834645669291653 ) ) ;
#34384 = CARTESIAN_POINT ( 'NONE',  ( -1.437007874015747477, -0.4536011799217367080, 0.2665933059059888421 ) ) ;
#34385 = CARTESIAN_POINT ( 'NONE',  ( -1.666666666666665853, 0.05413385826771626580, -0.4176697321401330321 ) ) ;
#34386 = CARTESIAN_POINT ( 'NONE',  ( -1.157146581871515012E-16, 0.4724409448818898682, -1.259842519685039353 ) ) ;
#34387 = CARTESIAN_POINT ( 'NONE',  ( -3.937007874015748143, 2.755905511811024056, 0.5314960629921260393 ) ) ;
#34388 = CARTESIAN_POINT ( 'NONE',  ( -0.2867679344610364334, -0.2867679344610367109, -0.6811023622047243098 ) ) ;
#34389 = CARTESIAN_POINT ( 'NONE',  ( 0.1958661417322834775, 0.3392501089628018884, -2.276246719160105236 ) ) ;
#34390 = CARTESIAN_POINT ( 'NONE',  ( -0.3083989501312330295, -0.3162353388693409650, -0.4822834645669289433 ) ) ;
#34391 = CARTESIAN_POINT ( 'NONE',  ( -1.456692913385826182, 0.1771653543307087630, 0.000000000000000000 ) ) ;
#34392 = CARTESIAN_POINT ( 'NONE',  ( -0.1998031496062994405, 0.3460692066303957537, 0.06758530183727032292 ) ) ;
#34394 = CARTESIAN_POINT ( 'NONE',  ( 0.000000000000000000, 2.755905511811024056, 0.000000000000000000 ) ) ;
#34393 = CARTESIAN_POINT ( 'NONE',  ( -1.620734908136482577, -0.6692913385826773087, -0.1292274648535924053 ) ) ;
#34395 = CARTESIAN_POINT ( 'NONE',  ( -1.502624671916009680, -0.05778040916215560624, -0.4822834645669293319 ) ) ;
#34396 = CARTESIAN_POINT ( 'NONE',  ( -0.5577427821522301654, -0.05778040916215560624, -0.4822834645669293319 ) ) ;
#34397 = CARTESIAN_POINT ( 'NONE',  ( -0.3917322834645669549, -7.196005306013483243E-17, 0.1955573735246212974 ) ) ;
#34398 = CARTESIAN_POINT ( 'NONE',  ( 0.6627296587926515548, 0.1771653543307087630, 0.09757992244046791164 ) ) ;
#34399 = CARTESIAN_POINT ( 'NONE',  ( -0.09156050430092219083, -0.3808816823641230087, -1.492482962822815952E-17 ) ) ;
#34400 = CARTESIAN_POINT ( 'NONE',  ( 0.5314960629921267055, -0.4536011799217367080, 0.2665933059059888421 ) ) ;
#34401 = CARTESIAN_POINT ( 'NONE',  ( 0.9776902887139113929, 0.1771653543307087630, 0.09757992244046791164 ) ) ;
#34402 = CARTESIAN_POINT ( 'NONE',  ( 1.062992125984252745, -0.6692913385826771977, 8.415575281601705876E-17 ) ) ;
#34403 = CARTESIAN_POINT ( 'NONE',  ( -0.4330708661417315697, -0.5511811023622047445, 6.969142054262312111E-17 ) ) ;
#34404 = CARTESIAN_POINT ( 'NONE',  ( -0.1958661417322834220, -0.3392501089628018884, -1.947506561679789971 ) ) ;
#34405 = CARTESIAN_POINT ( 'NONE',  ( -1.200787401574802349, -0.5400638737290844871, 0.3530559997133364547 ) ) ;
#34406 = CARTESIAN_POINT ( 'NONE',  ( 0.05905511811023681640, 0.07958543189024071263, -0.2665933059059888421 ) ) ;
#34407 = CARTESIAN_POINT ( 'NONE',  ( -1.253280839895012377, -0.2845877964562161244, -0.3641732283464567121 ) ) ;
#34408 = CARTESIAN_POINT ( 'NONE',  ( 5.785732909357575061E-17, -0.4724409448818898682, -0.4704724409448819422 ) ) ;
#34409 = VECTOR ( 'NONE', #44301, 39.37007874015748143 ) ;
#34410 = CARTESIAN_POINT ( 'NONE',  ( -1.128608923884513837, 0.1283753931104746893, -0.1820866141732285504 ) ) ;
#34411 = CARTESIAN_POINT ( 'NONE',  ( -1.220472440944882386, 0.000000000000000000, 0.000000000000000000 ) ) ;
#34412 = CARTESIAN_POINT ( 'NONE',  ( -0.2034120734908128059, 0.2952755905511811885, 0.1292274648535926551 ) ) ;
#34413 = CARTESIAN_POINT ( 'NONE',  ( 1.581364829396326277, -0.2845877964562161244, -0.3641732283464567121 ) ) ;
#34414 = CARTESIAN_POINT ( 'NONE',  ( 0.3871391076115492380, -0.08942795157528024563, -0.3641732283464568787 ) ) ;
#34415 = CARTESIAN_POINT ( 'NONE',  ( -0.2230971128608915943, -0.3690944881889765550, -0.3153832671262227771 ) ) ;
#34416 = CARTESIAN_POINT ( 'NONE',  ( -0.2296587926509179312, -0.05778040916215522460, 0.4822834645669289988 ) ) ;
#34417 = CARTESIAN_POINT ( 'NONE',  ( -1.646981627296586703, -0.3162353388693409650, -0.4822834645669289433 ) ) ;
#34418 = CARTESIAN_POINT ( 'NONE',  ( -1.010498687664041384, -0.004921259842519576551, 0.3153832671262227771 ) ) ;
#34419 = CARTESIAN_POINT ( 'NONE',  ( -3.937007874015748143, 1.537401574803149984, -0.4744094488188975722 ) ) ;
#34420 = CARTESIAN_POINT ( 'NONE',  ( 0.5249343832021005074, -0.6046776061558807314, 0.2411417322834647770 ) ) ;
#34421 = ORIENTED_EDGE ( 'NONE', *, *, #39648, .F. ) ;
#34422 = B_SPLINE_CURVE_WITH_KNOTS ( 'NONE', 3,
 ( #78181, #45743, #21748, #7890, #15036, #26815, #39443, #72688, #46995, #53721 ),
 .UNSPECIFIED., .F., .F.,
 ( 4, 2, 2, 2, 4 ),
 ( 0.005193997702760927253, 0.006123015815168760499, 0.007052033927576592878, 0.007981052039984426125, 0.008910070152392259371 ),
 .UNSPECIFIED. ) ;
#34423 = CARTESIAN_POINT ( 'NONE',  ( 0.1070741851644053388, 0.3996062992125986035, -1.645013123359579943 ) ) ;
#34424 =( BOUNDED_CURVE ( )  B_SPLINE_CURVE ( 2, ( #29521, #34188, #21972, #2204, #28281, #48875, #53532, #53943, #66185, #16087, #47216, #41732, #9760 ),
 .UNSPECIFIED., .F., .F. ) 
 B_SPLINE_CURVE_WITH_KNOTS ( ( 3, 2, 2, 2, 2, 2, 3 ),
 ( 0.1125000000000000028, 0.1166666666666666685, 0.1208333333333333343, 0.1250000000000000000, 0.1291666666666666796, 0.1333333333333333315, 0.1375000000000000111 ),
 .UNSPECIFIED. ) 
 CURVE ( )  GEOMETRIC_REPRESENTATION_ITEM ( )  RATIONAL_B_SPLINE_CURVE ( ( 1.000000000000000000, 0.9659258262890683122, 1.000000000000000000, 0.9659258262890683122, 1.000000000000000000, 0.9659258262890683122, 1.000000000000000000, 0.9659258262890683122, 1.000000000000000000, 0.9659258262890683122, 1.000000000000000000, 0.9659258262890683122, 1.000000000000000000 ) ) 
 REPRESENTATION_ITEM ( '' )  );
#34425 = CARTESIAN_POINT ( 'NONE',  ( 1.397637795275591177, -0.5400638737290844871, 0.3530559997133364547 ) ) ;
#34426 = CARTESIAN_POINT ( 'NONE',  ( -0.1771653543307080136, -0.4536011799217367080, 0.2665933059059888421 ) ) ;
#34427 = AXIS2_PLACEMENT_3D ( 'NONE', #67923, #80974, #30839 ) ;
#34428 = CARTESIAN_POINT ( 'NONE',  ( -0.04593175853018302557, -0.6692913385826773087, -0.1292274648535924053 ) ) ;
#34429 = CARTESIAN_POINT ( 'NONE',  ( -1.587926509186350810, 0.05413385826771626580, -0.4176697321401330321 ) ) ;
#34430 = CARTESIAN_POINT ( 'NONE',  ( -1.496062992125983815, -0.1870078740157479769, 0.3641732283464567677 ) ) ;
#34431 = CARTESIAN_POINT ( 'NONE',  ( 1.253280839895013710, -0.05778040916215560624, -0.4822834645669293319 ) ) ;
#34432 = CARTESIAN_POINT ( 'NONE',  ( -0.5511811023622041894, -0.1870078740157480601, -0.3641732283464567677 ) ) ;
#34433 = CARTESIAN_POINT ( 'NONE',  ( 0.4556365134843000653, 1.537493841523237759, 0.5309055118110234117 ) ) ;
#34434 = CARTESIAN_POINT ( 'NONE',  ( -0.1998031496062991907, -0.3460692066303959757, -0.06561679790026248016 ) ) ;
#34435 = CARTESIAN_POINT ( 'NONE',  ( 0.1958661417322836718, -0.3392501089628017219, -2.450806717356642128 ) ) ;
#34436 = CARTESIAN_POINT ( 'NONE',  ( 1.141392835773559211, 0.3937007874015748254, 1.456353465694822491 ) ) ;
#34437 = CARTESIAN_POINT ( 'NONE',  ( 0.9973753280839902091, 0.1283753931104746893, -0.1820866141732285504 ) ) ;
#34438 = CARTESIAN_POINT ( 'NONE',  ( -1.246719160104986512, 0.05413385826771666132, 0.4176697321401328100 ) ) ;
#34439 = CARTESIAN_POINT ( 'NONE',  ( 1.279527559055118724, 0.1660481256975885056, 0.3530559997133364547 ) ) ;
#34440 = CARTESIAN_POINT ( 'NONE',  ( -0.1958661417322834220, -0.3392501089628018884, -2.354986876640420057 ) ) ;
#34441 = CARTESIAN_POINT ( 'NONE',  ( 1.338582677165355062, -0.1870078740157479769, 0.3641732283464567677 ) ) ;
#34442 = CARTESIAN_POINT ( 'NONE',  ( -0.03280839895013062252, 0.2952755905511810774, -0.1292274648535930714 ) ) ;
#34443 = CARTESIAN_POINT ( 'NONE',  ( -0.3740157480314953431, 0.1660481256975885056, 0.3530559997133364547 ) ) ;
#34444 = CARTESIAN_POINT ( 'NONE',  ( 1.594488188976378673, -0.5400638737290845981, -0.3530559997133363437 ) ) ;
#34445 = CARTESIAN_POINT ( 'NONE',  ( -0.3460692066303958092, -0.1998031496062994683, -1.942257217847769057 ) ) ;
#34446 = CARTESIAN_POINT ( 'NONE',  ( 0.1837270341207354329, 0.1283753931104748280, 0.1820866141732283561 ) ) ;
#34447 = ORIENTED_EDGE ( 'NONE', *, *, #8767, .F. ) ;
#34448 = CARTESIAN_POINT ( 'NONE',  ( 4.797336870675656522E-17, -0.3917322834645670659, -0.5479195782490308142 ) ) ;
#34449 = EDGE_LOOP ( 'NONE', ( #76891, #33207, #69773, #77641 ) ) ;
#34450 = CARTESIAN_POINT ( 'NONE',  ( -0.3937007874015740483, -0.1870078740157480879, -0.4822834645669291653 ) ) ;
#34451 = CARTESIAN_POINT ( 'NONE',  ( 1.233595800524935227, -0.6046776061558807314, 0.2411417322834647770 ) ) ;
#34452 = CARTESIAN_POINT ( 'NONE',  ( 0.4133858267716541968, 0.1660481256975885056, 0.3530559997133364547 ) ) ;
#34453 = CARTESIAN_POINT ( 'NONE',  ( -0.3805774278215216522, -0.004921259842519576551, 0.3153832671262227771 ) ) ;
#34454 = CARTESIAN_POINT ( 'NONE',  ( 0.6889763779527566800, -0.5400638737290844871, 0.3530559997133364547 ) ) ;
#34455 = CARTESIAN_POINT ( 'NONE',  ( -0.8858267716535425107, -0.5400638737290844871, 0.3530559997133364547 ) ) ;
#34456 = CARTESIAN_POINT ( 'NONE',  ( -0.6036745406824141069, 0.2306618581243848609, 0.2411417322834645549 ) ) ;
#34457 = CARTESIAN_POINT ( 'NONE',  ( -0.6955380577427815458, -0.4281496062992127816, -0.4176697321401328100 ) ) ;
#34458 = CARTESIAN_POINT ( 'NONE',  ( 1.122047244094488860, 0.1660481256975885056, 0.3530559997133364547 ) ) ;
#34459 = CARTESIAN_POINT ( 'NONE',  ( 0.9251968503937015864, -0.5400638737290844871, 0.3530559997133364547 ) ) ;
#34460 = CARTESIAN_POINT ( 'NONE',  ( 1.240157480314961314, 0.1660481256975883668, -0.3530559997133364547 ) ) ;
#34461 = CARTESIAN_POINT ( 'NONE',  ( 0.3917322834645669549, 0.1049643490035304660, -0.5892388451443569819 ) ) ;
#34462 = CARTESIAN_POINT ( 'NONE',  ( 0.2230971128608932319, -0.3690944881889763329, 0.3153832671262228327 ) ) ;
#34463 = VERTEX_POINT ( 'NONE', #41734 ) ;
#34464 = CARTESIAN_POINT ( 'NONE',  ( -0.1974969037888703871, -0.3420746716998661063, -1.010498687664042050 ) ) ;
#34465 = CONICAL_SURFACE ( 'NONE', #45178, 3.582677165354331450, 0.5235987755982945968 ) ;
#34466 = ORIENTED_EDGE ( 'NONE', *, *, #81028, .T. ) ;
#34467 = CARTESIAN_POINT ( 'NONE',  ( -0.7742782152230965886, -0.004921259842519576551, 0.3153832671262227771 ) ) ;
#34468 = AXIS2_PLACEMENT_3D ( 'NONE', #27261, #78635, #20959 ) ;
#34469 = CIRCLE ( 'NONE', #10326, 0.1574803149606300579 ) ;
#34470 = CARTESIAN_POINT ( 'NONE',  ( -0.2230971128608915943, 0.05413385826771666132, 0.4176697321401328100 ) ) ;
#34471 = CARTESIAN_POINT ( 'NONE',  ( 2.557132292622070757, 1.503024749832830631, 0.4732391302016651369 ) ) ;
#34472 = CARTESIAN_POINT ( 'NONE',  ( -0.1837270341207343505, -0.6046776061558807314, 0.2411417322834647770 ) ) ;
#34473 = CARTESIAN_POINT ( 'NONE',  ( -0.2624671916010490880, 0.2306618581243847221, -0.2411417322834647770 ) ) ;
#34474 = CARTESIAN_POINT ( 'NONE',  ( -0.9580052493438311334, 0.05413385826771626580, -0.4176697321401330321 ) ) ;
#34475 = CARTESIAN_POINT ( 'NONE',  ( -1.404199475065615932, 0.05413385826771666132, 0.4176697321401328100 ) ) ;
#34476 = CARTESIAN_POINT ( 'NONE',  ( 1.358267716535433323, 0.07958543189024085140, 0.2665933059059887866 ) ) ;
#34477 = LINE ( 'NONE', #2494, #33161 ) ;
#34478 = CARTESIAN_POINT ( 'NONE',  ( 0.2362214119660041856, 0.1771641016305865735, 5.695982005544458993 ) ) ;
#34479 = CARTESIAN_POINT ( 'NONE',  ( 0.4330708661417329575, -0.5511811023622047445, 6.969142054262312111E-17 ) ) ;
#34480 = CARTESIAN_POINT ( 'NONE',  ( -0.07217847769028787330, -0.05778040916215522460, 0.4822834645669289988 ) ) ;
#34481 = CARTESIAN_POINT ( 'NONE',  ( 0.1640419947506569498, -0.3162353388693409650, -0.4822834645669289433 ) ) ;
#34482 = ORIENTED_EDGE ( 'NONE', *, *, #45967, .T. ) ;
#34483 = CARTESIAN_POINT ( 'NONE',  ( -0.1998031496062994683, 0.3460692066303958092, -1.587926509186351698 ) ) ;
#34484 = CARTESIAN_POINT ( 'NONE',  ( -0.5971128608923876868, 0.2066929133858267931, 0.1054918080437490802 ) ) ;
#34485 = CARTESIAN_POINT ( 'NONE',  ( 0.1070741851644054776, -0.3996062992125984925, -1.264435695538057569 ) ) ;
#34486 = CARTESIAN_POINT ( 'NONE',  ( -0.3996062992125985480, -7.340648628747423112E-17, -0.4311023622047244208 ) ) ;
#34487 = CARTESIAN_POINT ( 'NONE',  ( -0.7480314960629914633, 0.2952755905511811885, 0.000000000000000000 ) ) ;
#34488 = CARTESIAN_POINT ( 'NONE',  ( 0.1998031496062994405, -0.3460692066303958092, -2.926509186351706315 ) ) ;
#34489 = CARTESIAN_POINT ( 'NONE',  ( 0.3917322834645670104, 2.398668435337828261E-17, -2.564960629921259727 ) ) ;
#34490 = CARTESIAN_POINT ( 'NONE',  ( -1.450131233595799651, 0.1771653543307087075, -0.09757992244046823083 ) ) ;
#34491 = CARTESIAN_POINT ( 'NONE',  ( 0.8727034120734912248, -0.3162353388693409650, -0.4822834645669289433 ) ) ;
#34492 = CONICAL_SURFACE ( 'NONE', #80171, 3.228346456692913424, 0.7853981633974500554 ) ;
#34493 = CARTESIAN_POINT ( 'NONE',  ( 0.7742782152230979209, 0.05413385826771626580, -0.4176697321401330321 ) ) ;
#34494 = CARTESIAN_POINT ( 'NONE',  ( -0.3412073490813641308, 0.1283753931104746893, -0.1820866141732285504 ) ) ;
#34495 = CARTESIAN_POINT ( 'NONE',  ( 0.1049868766404206816, -0.6046776061558809534, -0.2411417322834644161 ) ) ;
#34496 = CARTESIAN_POINT ( 'NONE',  ( 5.785732909357575061E-17, -0.4724409448818898682, -2.045275590551181022 ) ) ;
#34497 = CARTESIAN_POINT ( 'NONE',  ( -0.1902887139107604098, 0.1771653543307087075, -0.09757992244046823083 ) ) ;
#34498 = CARTESIAN_POINT ( 'NONE',  ( -0.4068241469816267775, 0.05413385826771626580, -0.4176697321401330321 ) ) ;
#34499 = CARTESIAN_POINT ( 'NONE',  ( -0.3420746716998660508, -0.1974969037888706924, -2.019028871391076230 ) ) ;
#34500 = CARTESIAN_POINT ( 'NONE',  ( -1.627296587926508442, -0.6046776061558809534, -0.2411417322834644161 ) ) ;
#34501 = CARTESIAN_POINT ( 'NONE',  ( 0.3018372703412079971, -0.3690944881889763329, 0.3153832671262228327 ) ) ;
#34502 = CARTESIAN_POINT ( 'NONE',  ( 0.000000000000000000, 0.000000000000000000, -1.929133858267716661 ) ) ;
#34503 = CARTESIAN_POINT ( 'NONE',  ( -1.049868766404198794, 0.2306618581243847221, -0.2411417322834647770 ) ) ;
#34504 = CARTESIAN_POINT ( 'NONE',  ( -0.8595800524934373854, -0.08942795157527998196, 0.3641732283464567121 ) ) ;
#34505 = CARTESIAN_POINT ( 'NONE',  ( 0.4724409448818880919, 0.1265901696525020825, -2.248687664041995049 ) ) ;
#34506 = CARTESIAN_POINT ( 'NONE',  ( -0.8005249343832013809, -0.4281496062992124485, 0.4176697321401328655 ) ) ;
#34507 = CARTESIAN_POINT ( 'NONE',  ( -0.5905511811023613777, -0.6692913385826771977, 8.415575281601705876E-17 ) ) ;
#34508 = CARTESIAN_POINT ( 'NONE',  ( 0.006561679790026889343, -0.3162353388693409650, -0.4822834645669289433 ) ) ;
#34509 = CARTESIAN_POINT ( 'NONE',  ( 0.3460692066303959202, -0.1998031496062991630, -2.386482939632545985 ) ) ;
#34510 = CARTESIAN_POINT ( 'NONE',  ( 0.3392501089628018329, -0.1958661417322834497, -2.232264148785090274 ) ) ;
#34511 = CARTESIAN_POINT ( 'NONE',  ( -2.170146923806554273, 1.537401574803149984, -0.4744094488188975722 ) ) ;
#34512 = CARTESIAN_POINT ( 'NONE',  ( 0.4658792650918641698, -0.08942795157528024563, -0.3641732283464568787 ) ) ;
#34513 = CARTESIAN_POINT ( 'NONE',  ( 0.9317585301837276734, -0.4281496062992124485, 0.4176697321401328655 ) ) ;
#34514 = CARTESIAN_POINT ( 'NONE',  ( -1.325459317585300889, -0.3690944881889765550, -0.3153832671262227771 ) ) ;
#34515 = CARTESIAN_POINT ( 'NONE',  ( 1.345144356955381593, -0.05778040916215522460, 0.4822834645669289988 ) ) ;
#34516 = CARTESIAN_POINT ( 'NONE',  ( -1.056430446194224881, 0.1771653543307087075, -0.09757992244046823083 ) ) ;
#34517 = CARTESIAN_POINT ( 'NONE',  ( -0.7283464566929126471, 0.1660481256975883668, -0.3530559997133364547 ) ) ;
#34518 = CARTESIAN_POINT ( 'NONE',  ( 0.1706036745406830368, -0.3690944881889765550, -0.3153832671262227771 ) ) ;
#34519 = DIRECTION ( 'NONE',  ( 0.000000000000000000, 0.000000000000000000, 1.000000000000000000 ) ) ;
#34520 = CARTESIAN_POINT ( 'NONE',  ( 0.8267716535433077274, 0.1771653543307087630, 0.000000000000000000 ) ) ;
#34521 = CARTESIAN_POINT ( 'NONE',  ( 0.4790026246719168435, -0.3162353388693409650, -0.4822834645669289433 ) ) ;
#34522 = CARTESIAN_POINT ( 'NONE',  ( -0.3460692066303960313, 0.1998031496062989965, -0.2604986876640419946 ) ) ;
#34523 = EDGE_CURVE ( 'NONE', #82183, #25632, #26924, .T. ) ;
#34524 = CARTESIAN_POINT ( 'NONE',  ( -0.8398950131233589023, -0.6046776061558809534, -0.2411417322834644161 ) ) ;
#34525 = CIRCLE ( 'NONE', #18362, 0.2952755905511810774 ) ;
#34526 = CARTESIAN_POINT ( 'NONE',  ( -0.1958661417322834220, -0.3392501089628018884, -2.040026246719160330 ) ) ;
#34527 = CARTESIAN_POINT ( 'NONE',  ( 1.207349081364829990, -0.5023911411419708095, -0.1820866141732282451 ) ) ;
#34529 = CARTESIAN_POINT ( 'NONE',  ( -0.02624671916010428221, 0.2306618581243847221, -0.2411417322834647770 ) ) ;
#34528 = AXIS2_PLACEMENT_3D ( 'NONE', #80029, #81258, #16461 ) ;
#34530 = CARTESIAN_POINT ( 'NONE',  ( -0.1902887139107604098, 0.2952755905511810774, -0.1292274648535930714 ) ) ;
#34531 = CARTESIAN_POINT ( 'NONE',  ( -0.2296587926509179312, -0.08942795157527998196, 0.3641732283464567121 ) ) ;
#34532 = CARTESIAN_POINT ( 'NONE',  ( 0.1509186351706045259, -0.08942795157528024563, -0.3641732283464568787 ) ) ;
#34533 = CARTESIAN_POINT ( 'NONE',  ( 0.5643044619422579178, 0.05413385826771666132, 0.4176697321401328100 ) ) ;
#34534 = CARTESIAN_POINT ( 'NONE',  ( -0.5971128608923877978, 0.1771653543307087630, 0.09757992244046791164 ) ) ;
#34535 = CARTESIAN_POINT ( 'NONE',  ( 0.3996062992125985480, 2.446882876249141654E-17, -0.8248031496062991907 ) ) ;
#34536 = CARTESIAN_POINT ( 'NONE',  ( -1.036745406824146176, -0.4281496062992124485, 0.4176697321401328655 ) ) ;
#34537 = CARTESIAN_POINT ( 'NONE',  ( 0.4724409448818898682, 2.892866454678787531E-17, -2.637795275590551380 ) ) ;
#34538 = ORIENTED_EDGE ( 'NONE', *, *, #68721, .T. ) ;
#34539 = CARTESIAN_POINT ( 'NONE',  ( -1.122047244094487306, -0.4536011799217367080, 0.2665933059059888421 ) ) ;
#34540 = CARTESIAN_POINT ( 'NONE',  ( -0.2034120734908131112, -0.6692913385826773087, -0.1292274648535924053 ) ) ;
#34541 = PLANE ( 'NONE',  #10383 ) ;
#34542 = CARTESIAN_POINT ( 'NONE',  ( -0.6955380577427815458, 0.05413385826771666132, 0.4176697321401328100 ) ) ;
#34543 = CARTESIAN_POINT ( 'NONE',  ( 0.000000000000000000, 2.145669291338582418, 0.000000000000000000 ) ) ;
#34544 = CARTESIAN_POINT ( 'NONE',  ( 1.213910761154856299, 0.2952755905511811885, 0.1292274648535926551 ) ) ;
#34545 = CARTESIAN_POINT ( 'NONE',  ( 1.056430446194226658, 0.2952755905511811885, 0.1292274648535926551 ) ) ;
#34546 = DIRECTION ( 'NONE',  ( 0.000000000000000000, 0.000000000000000000, 1.000000000000000000 ) ) ;
#34547 = DIRECTION ( 'NONE',  ( -3.491481338843132961E-15, -0.000000000000000000, 1.000000000000000000 ) ) ;
#34548 = CARTESIAN_POINT ( 'NONE',  ( 0.2396931915125568024, -0.1724440681141642395, 5.660914615074363887 ) ) ;
#34549 = CARTESIAN_POINT ( 'NONE',  ( 1.443569553805774897, 0.1283753931104748280, 0.1820866141732283561 ) ) ;
#34550 = CARTESIAN_POINT ( 'NONE',  ( -0.1998031496062994683, 0.3460692066303958092, -0.3280839895013123453 ) ) ;
#34551 = ORIENTED_EDGE ( 'NONE', *, *, #78501, .T. ) ;
#34552 = CARTESIAN_POINT ( 'NONE',  ( -0.3608923884514428360, 0.1771653543307087630, 0.09757992244046791164 ) ) ;
#34553 = CARTESIAN_POINT ( 'NONE',  ( -0.3917322834645670104, -7.196005306013484475E-17, -2.078740157480314821 ) ) ;
#34554 = ORIENTED_EDGE ( 'NONE', *, *, #67320, .F. ) ;
#34555 = CARTESIAN_POINT ( 'NONE',  ( 0.7611548556430451917, -0.6046776061558807314, 0.2411417322834647770 ) ) ;
#34556 = CARTESIAN_POINT ( 'NONE',  ( 0.1574803149606306130, -0.1870078740157479769, 0.4822834645669291653 ) ) ;
#34557 = CARTESIAN_POINT ( 'NONE',  ( -0.8858267716535425107, -0.5400638737290844871, 0.3530559997133364547 ) ) ;
#34558 = CARTESIAN_POINT ( 'NONE',  ( 1.476377952755906442, -0.5400638737290844871, 0.3530559997133364547 ) ) ;
#34559 = CARTESIAN_POINT ( 'NONE',  ( -0.8005249343832011588, -0.004921259842519870586, -0.3153832671262229437 ) ) ;
#34560 = CARTESIAN_POINT ( 'NONE',  ( 0.004535564325209356581, 1.062992125984248748, -1.627527093699462135 ) ) ;
#34561 = CARTESIAN_POINT ( 'NONE',  ( 0.4068241469816281097, 0.05413385826771666132, 0.4176697321401328100 ) ) ;
#34562 = EDGE_CURVE ( 'NONE', #76682, #5541, #10600, .T. ) ;
#34563 = CARTESIAN_POINT ( 'NONE',  ( 0.4330708661417329575, -0.5511811023622047445, 6.969142054262312111E-17 ) ) ;
#34564 = CARTESIAN_POINT ( 'NONE',  ( -1.043307086614172041, -0.5400638737290844871, 0.3530559997133364547 ) ) ;
#34565 = CARTESIAN_POINT ( 'NONE',  ( 0.1958661417322836162, -0.3392501089628018329, -1.431739214401887894 ) ) ;
#34566 = CARTESIAN_POINT ( 'NONE',  ( -1.286089238845143479, 0.2306618581243847221, -0.2411417322834647770 ) ) ;
#34567 = CARTESIAN_POINT ( 'NONE',  ( -1.594488188976377563, -0.4536011799217367080, 0.2665933059059888421 ) ) ;
#34568 = CARTESIAN_POINT ( 'NONE',  ( 0.9645669291338591078, -0.5400638737290845981, -0.3530559997133363437 ) ) ;
#34569 = CARTESIAN_POINT ( 'NONE',  ( 1.450131233595801428, -0.5511811023622048555, -0.09757992244046775898 ) ) ;
#34570 = ORIENTED_EDGE ( 'NONE', *, *, #42480, .F. ) ;
#34571 = CARTESIAN_POINT ( 'NONE',  ( 0.1049643490035304799, -0.3917322834645670104, -2.916685982448506298 ) ) ;
#34572 = CARTESIAN_POINT ( 'NONE',  ( -0.3477690288713902178, 0.2952755905511810774, -0.1292274648535930714 ) ) ;
#34573 = VERTEX_POINT ( 'NONE', #82124 ) ;
#34574 = CARTESIAN_POINT ( 'NONE',  ( 0.5446194225721792126, -0.08942795157528024563, -0.3641732283464568787 ) ) ;
#34575 = CARTESIAN_POINT ( 'NONE',  ( -1.391076115485563758, 0.2306618581243848609, 0.2411417322834645549 ) ) ;
#34576 = CARTESIAN_POINT ( 'NONE',  ( 1.036745406824147508, -0.4281496062992127816, -0.4176697321401328100 ) ) ;
#34577 = CARTESIAN_POINT ( 'NONE',  ( 0.7283464566929140904, -0.5400638737290845981, -0.3530559997133363437 ) ) ;
#34578 = CARTESIAN_POINT ( 'NONE',  ( -0.3083989501312330295, -0.05778040916215522460, 0.4822834645669289988 ) ) ;
#34579 = CARTESIAN_POINT ( 'NONE',  ( -0.2230971128608915943, 0.05413385826771666132, 0.4176697321401328100 ) ) ;
#34580 = CARTESIAN_POINT ( 'NONE',  ( -0.3917322834645670104, -7.196005306013484475E-17, -2.328740157480315265 ) ) ;
#34581 = CARTESIAN_POINT ( 'NONE',  ( -1.699475065616797398, 0.2952755905511811885, 0.1292274648535926551 ) ) ;
#34582 = CARTESIAN_POINT ( 'NONE',  ( -0.8136482939632537770, 0.2306618581243847221, -0.2411417322834647770 ) ) ;
#34583 = CARTESIAN_POINT ( 'NONE',  ( -0.5118110236220466680, 0.1771653543307087630, 0.000000000000000000 ) ) ;
#34584 = CARTESIAN_POINT ( 'NONE',  ( 1.299212598425197429, -0.6692913385826771977, 8.415575281601705876E-17 ) ) ;
#34585 = FACE_OUTER_BOUND ( 'NONE', #40363, .T. ) ;
#34586 = CARTESIAN_POINT ( 'NONE',  ( -1.076115485564303809, 0.2306618581243848609, 0.2411417322834645549 ) ) ;
#34587 = CARTESIAN_POINT ( 'NONE',  ( 0.1998031496062994128, -0.3460692066303957537, -0.01115485564304462100 ) ) ;
#34588 = VECTOR ( 'NONE', #37121, 39.37007874015748143 ) ;
#34589 = CARTESIAN_POINT ( 'NONE',  ( 0.8464566929133865436, 0.1660481256975883668, -0.3530559997133364547 ) ) ;
#34590 = CARTESIAN_POINT ( 'NONE',  ( 0.1070741851644053527, 0.3996062992125986590, -1.883202099737532276 ) ) ;
#34591 = CARTESIAN_POINT ( 'NONE',  ( 3.918979230920996315, 1.247401896492644102, 0.3767456479477053755 ) ) ;
#34592 = EDGE_CURVE ( 'NONE', #43965, #66126, #82757, .T. ) ;
#34593 = CIRCLE ( 'NONE', #81638, 0.3149606299212597271 ) ;
#34594 = CARTESIAN_POINT ( 'NONE',  ( -0.2427821522309703550, -0.3162353388693405765, 0.4822834645669290543 ) ) ;
#34595 = CARTESIAN_POINT ( 'NONE',  ( -1.272965879265091305, -0.004921259842519870586, -0.3153832671262229437 ) ) ;
#34597 = CARTESIAN_POINT ( 'NONE',  ( 3.937007874015748143, 1.724409448818897905, -0.4359958488159719758 ) ) ;
#34596 = CARTESIAN_POINT ( 'NONE',  ( 1.227034120734908917, 0.1771653543307087075, -0.09757992244046823083 ) ) ;
#34598 = CARTESIAN_POINT ( 'NONE',  ( 0.2362204724409451007, -0.4091458600556402980, -0.4835958005249343938 ) ) ;
#34599 = CARTESIAN_POINT ( 'NONE',  ( 1.338582677165355062, -0.1870078740157479769, 0.3641732283464567677 ) ) ;
#34600 = CARTESIAN_POINT ( 'NONE',  ( 1.404199475065617264, -0.4281496062992124485, 0.4176697321401328655 ) ) ;
#34601 = CARTESIAN_POINT ( 'NONE',  ( -0.1058382717557497660, -0.3949938075777411073, -0.3064304461942257696 ) ) ;
#34602 = CARTESIAN_POINT ( 'NONE',  ( -0.1706036745406816491, -0.4281496062992124485, 0.4176697321401328655 ) ) ;
#34603 = DIRECTION ( 'NONE',  ( -3.491481338843132961E-15, 0.000000000000000000, 1.000000000000000000 ) ) ;
#34604 = CARTESIAN_POINT ( 'NONE',  ( 1.489501312335958172, -0.08942795157528024563, -0.3641732283464568787 ) ) ;
#34605 = CARTESIAN_POINT ( 'NONE',  ( 0.03280839895013198948, 0.2952755905511811885, 0.1292274648535926551 ) ) ;
#34606 = CARTESIAN_POINT ( 'NONE',  ( -0.3420746716998660508, -0.1974969037888706924, -0.2867454068241469534 ) ) ;
#34607 = CARTESIAN_POINT ( 'NONE',  ( 1.194225721784777594, 0.05413385826771666132, 0.4176697321401328100 ) ) ;
#34608 = CARTESIAN_POINT ( 'NONE',  ( 0.3608923884514443348, 0.2952755905511810774, -0.1292274648535930714 ) ) ;
#34609 = CARTESIAN_POINT ( 'NONE',  ( 0.5446194225721792126, -0.2845877964562159024, 0.3641732283464567677 ) ) ;
#34610 = DIRECTION ( 'NONE',  ( 0.000000000000000000, 0.000000000000000000, 1.000000000000000000 ) ) ;
#34611 = CARTESIAN_POINT ( 'NONE',  ( 0.2821522309711292364, 0.1771653543307087075, -0.09757992244046823083 ) ) ;
#34612 = DIRECTION ( 'NONE',  ( 0.000000000000000000, 0.000000000000000000, -1.000000000000000000 ) ) ;
#34613 = CARTESIAN_POINT ( 'NONE',  ( 0.3996062992125986035, -0.1070741851644052972, -1.133202099737532720 ) ) ;
#34614 = CARTESIAN_POINT ( 'NONE',  ( 0.8858267716535438430, 0.1660481256975885056, 0.3530559997133364547 ) ) ;
#34615 = CARTESIAN_POINT ( 'NONE',  ( -0.3392501089628019995, 0.1958661417322832277, -0.9632545931758529356 ) ) ;
#34616 = CARTESIAN_POINT ( 'NONE',  ( 0.5314960629920922885, 2.729659900128874828, 3.210901142567245348 ) ) ;
#34617 = DIRECTION ( 'NONE',  ( 0.000000000000000000, 0.000000000000000000, -1.000000000000000000 ) ) ;
#34618 = B_SPLINE_CURVE_WITH_KNOTS ( 'NONE', 3,
 ( #34667, #45603, #71297, #2678, #1433, #13645, #40143, #78038, #72960, #32989, #65828, #72549 ),
 .UNSPECIFIED., .F., .F.,
 ( 4, 2, 2, 2, 2, 4 ),
 ( 0.04729187226826467999, 0.04795755069747602989, 0.04862322912668737979, 0.04995458598511005877, 0.05128594284353273774, 0.05261729970195541672 ),
 .UNSPECIFIED. ) ;
#34619 = CARTESIAN_POINT ( 'NONE',  ( 0.05905511811023681640, 0.07958543189024071263, -0.2665933059059888421 ) ) ;
#34620 = CARTESIAN_POINT ( 'NONE',  ( 0.03937007874015833325, -0.6692913385826771977, 8.415575281601705876E-17 ) ) ;
#34621 = CARTESIAN_POINT ( 'NONE',  ( 1.535433070866142558, 0.1771653543307087630, 0.000000000000000000 ) ) ;
#34622 = CARTESIAN_POINT ( 'NONE',  ( -1.502624671916009680, -0.08942795157528024563, -0.3641732283464568787 ) ) ;
#34623 = CARTESIAN_POINT ( 'NONE',  ( -1.469816272965878357, -0.6046776061558809534, -0.2411417322834644161 ) ) ;
#34624 = CARTESIAN_POINT ( 'NONE',  ( 0.6758530183727039509, -0.6692913385826771977, 0.1292274648535927661 ) ) ;
#34625 = CARTESIAN_POINT ( 'NONE',  ( 1.574803149606299746, -0.1870078740157480879, -0.4822834645669291653 ) ) ;
#34626 = DIRECTION ( 'NONE',  ( 0.000000000000000000, -1.000000000000000000, 0.000000000000000000 ) ) ;
#34627 = CARTESIAN_POINT ( 'NONE',  ( 0.4921259842519691285, 0.1660481256975885056, 0.3530559997133364547 ) ) ;
#34628 = CARTESIAN_POINT ( 'NONE',  ( -0.3460692066303957537, -0.1998031496062994405, 0.1856955380577427484 ) ) ;
#34629 = CARTESIAN_POINT ( 'NONE',  ( 1.541994750656168645, 0.2952755905511810774, -0.1292274648535930714 ) ) ;
#34630 = CARTESIAN_POINT ( 'NONE',  ( 0.9317585301837276734, 0.05413385826771626580, -0.4176697321401330321 ) ) ;
#34631 = CARTESIAN_POINT ( 'NONE',  ( -1.417322834645668772, -0.1870078740157479769, 0.3641732283464567677 ) ) ;
#34632 = CARTESIAN_POINT ( 'NONE',  ( 1.286089238845145033, -0.5023911411419708095, -0.1820866141732282451 ) ) ;
#34633 = CARTESIAN_POINT ( 'NONE',  ( 1.509186351706037543, 0.05413385826771666132, 0.4176697321401328100 ) ) ;
#34634 = CARTESIAN_POINT ( 'NONE',  ( -0.9186351706036736120, -0.5023911411419708095, -0.1820866141732282451 ) ) ;
#34635 = CARTESIAN_POINT ( 'NONE',  ( 1.614173228346457378, 0.2952755905511811885, 0.000000000000000000 ) ) ;
#34636 = CARTESIAN_POINT ( 'NONE',  ( 0.5052493438320215802, 0.1771653543307087630, 0.09757992244046791164 ) ) ;
#34637 = CARTESIAN_POINT ( 'NONE',  ( 0.1706036745406830368, -0.4281496062992127816, -0.4176697321401328100 ) ) ;
#34638 = CARTESIAN_POINT ( 'NONE',  ( 1.135170603674541256, 0.2952755905511811885, 0.1292274648535926551 ) ) ;
#34639 = CARTESIAN_POINT ( 'NONE',  ( -0.3346456692913377662, 0.1660481256975883668, -0.3530559997133364547 ) ) ;
#34640 = CARTESIAN_POINT ( 'NONE',  ( 0.3083989501312343062, -0.2845877964562159024, 0.3641732283464567677 ) ) ;
#34641 = CARTESIAN_POINT ( 'NONE',  ( 1.279527559055118724, 0.1660481256975885056, 0.3530559997133364547 ) ) ;
#34642 = CARTESIAN_POINT ( 'NONE',  ( -1.528871391076114250, -0.6692913385826771977, 0.1292274648535927661 ) ) ;
#34643 = CARTESIAN_POINT ( 'NONE',  ( -0.9580052493438311334, -0.4281496062992124485, 0.4176697321401328655 ) ) ;
#34645 = CARTESIAN_POINT ( 'NONE',  ( 4.893765752498283924E-17, -0.3996062992125986035, -0.8661417322834645827 ) ) ;
#34644 = CARTESIAN_POINT ( 'NONE',  ( -1.502624671916009680, -0.08942795157528024563, -0.3641732283464568787 ) ) ;
#34646 = CARTESIAN_POINT ( 'NONE',  ( 1.012524390108117345, 2.412178165100495768E-16, -0.3954985857520057491 ) ) ;
#34647 = AXIS2_PLACEMENT_3D ( 'NONE', #32462, #44650, #77933 ) ;
#34648 = CARTESIAN_POINT ( 'NONE',  ( -0.9514435695538050464, -0.05778040916215560624, -0.4822834645669293319 ) ) ;
#34649 = CARTESIAN_POINT ( 'NONE',  ( 0.1443569553805781891, -0.4281496062992124485, 0.4176697321401328655 ) ) ;
#34650 = CARTESIAN_POINT ( 'NONE',  ( 0.3996062992125986590, -0.1070741851644053111, -2.946194225721785465 ) ) ;
#34651 = CARTESIAN_POINT ( 'NONE',  ( 0.3949938075777409963, 2.418639510665530435E-17, -2.165354330708661124 ) ) ;
#34652 = ORIENTED_EDGE ( 'NONE', *, *, #74631, .F. ) ;
#34653 = CARTESIAN_POINT ( 'NONE',  ( 0.6955380577427828781, -0.3690944881889763329, 0.3153832671262228327 ) ) ;
#34654 = CARTESIAN_POINT ( 'NONE',  ( 0.3917322834645670104, 2.398668435337828261E-17, -1.055118110236220375 ) ) ;
#34655 = CARTESIAN_POINT ( 'NONE',  ( 1.128608923884514947, 0.2306618581243848609, 0.2411417322834645549 ) ) ;
#34656 = CARTESIAN_POINT ( 'NONE',  ( 0.4102808022082889416, 1.299212598425196985, -1.382164990278189398 ) ) ;
#34657 = CARTESIAN_POINT ( 'NONE',  ( -1.391076115485563758, 0.1283753931104748280, 0.1820866141732283561 ) ) ;
#34658 = CARTESIAN_POINT ( 'NONE',  ( -0.2017716535433071445, 0.2017716535433070613, 0.000000000000000000 ) ) ;
#34659 = EDGE_CURVE ( 'NONE', #19542, #16864, #50913, .T. ) ;
#34660 = CARTESIAN_POINT ( 'NONE',  ( -1.404199475065615932, 0.05413385826771666132, 0.4176697321401328100 ) ) ;
#34661 = CARTESIAN_POINT ( 'NONE',  ( -0.3917322834645668994, -0.1049643490035306742, -0.1259649361866648498 ) ) ;
#34662 = CARTESIAN_POINT ( 'NONE',  ( 0.1902887139107617975, -0.6692913385826773087, -0.1292274648535924053 ) ) ;
#34663 = CARTESIAN_POINT ( 'NONE',  ( -0.5314960629921254842, -0.4536011799217368745, -0.2665933059059886201 ) ) ;
#34664 = CARTESIAN_POINT ( 'NONE',  ( 0.9186351706036751663, -0.6046776061558807314, 0.2411417322834647770 ) ) ;
#34666 = EDGE_CURVE ( 'NONE', #81967, #67145, #15616, .T. ) ;
#34665 = CARTESIAN_POINT ( 'NONE',  ( 0.05249343832021075018, 0.2306618581243847221, -0.2411417322834647770 ) ) ;
#34667 = CARTESIAN_POINT ( 'NONE',  ( -0.4744094488188894121, 1.537401574803149984, -2.170146923806595574 ) ) ;
#34668 = DIRECTION ( 'NONE',  ( -3.096699300667737957E-16, 1.000000000000000000, -0.000000000000000000 ) ) ;
#34669 = CARTESIAN_POINT ( 'NONE',  ( -0.2867679344610367109, 0.2867679344610365444, -1.433746349902574213 ) ) ;
#34670 = CARTESIAN_POINT ( 'NONE',  ( 0.8989501312335964611, 0.2952755905511811885, 0.1292274648535926551 ) ) ;
#34671 = CARTESIAN_POINT ( 'NONE',  ( 0.2165354330708668673, 0.1660481256975883668, -0.3530559997133364547 ) ) ;
#34672 = CARTESIAN_POINT ( 'NONE',  ( -1.227034120734907141, -0.6692913385826773087, -0.1292274648535924053 ) ) ;
#34673 = CARTESIAN_POINT ( 'NONE',  ( -1.568241469816272105, -0.3162353388693409650, -0.4822834645669289433 ) ) ;
#34674 = CARTESIAN_POINT ( 'NONE',  ( 0.9120734908136490793, 0.2952755905511810774, -0.1292274648535930714 ) ) ;
#34675 = CARTESIAN_POINT ( 'NONE',  ( 0.3917322834645669549, 0.1049643490035304660, -0.3667979002624672802 ) ) ;
#34676 = CARTESIAN_POINT ( 'NONE',  ( -0.2362204724409442680, -0.1870078740157480879, -0.4822834645669291653 ) ) ;
#34677 = CARTESIAN_POINT ( 'NONE',  ( 0.4986876640419954376, -0.6046776061558809534, -0.2411417322834644161 ) ) ;
#34678 = CARTESIAN_POINT ( 'NONE',  ( -0.09186351706036663400, -0.4281496062992124485, 0.4176697321401328655 ) ) ;
#34679 = CARTESIAN_POINT ( 'NONE',  ( 0.5446194225721792126, -0.2845877964562159024, 0.3641732283464567677 ) ) ;
#34680 = CARTESIAN_POINT ( 'NONE',  ( -1.384514435695537005, 0.2952755905511811885, 0.1292274648535926551 ) ) ;
#34681 = CARTESIAN_POINT ( 'NONE',  ( -1.371391076115484831, 0.2952755905511810774, -0.1292274648535930714 ) ) ;
#34682 = CARTESIAN_POINT ( 'NONE',  ( 0.7283464566929140904, -0.5400638737290845981, -0.3530559997133363437 ) ) ;
#34683 = CARTESIAN_POINT ( 'NONE',  ( 0.3503937007874015630, -0.3733313776025732333, -0.4921259842519685179 ) ) ;
#34684 = CARTESIAN_POINT ( 'NONE',  ( -0.2867679344610364334, -0.2867679344610367109, -2.413385826771653253 ) ) ;
#34685 = ORIENTED_EDGE ( 'NONE', *, *, #74375, .T. ) ;
#34686 = ADVANCED_FACE ( 'NONE', ( #61926 ), #49698, .F. ) ;
#34687 = EDGE_LOOP ( 'NONE', ( #42336, #29382, #18610, #30385 ) ) ;
#34688 = CARTESIAN_POINT ( 'NONE',  ( 1.187664041994751285, -0.05778040916215522460, 0.4822834645669289988 ) ) ;
#34689 = CARTESIAN_POINT ( 'NONE',  ( 0.6824146981627303710, 0.1283753931104746893, -0.1820866141732285504 ) ) ;
#34690 = CARTESIAN_POINT ( 'NONE',  ( 0.4849061582275022153, 1.726086921369708538, 0.4921425059946342717 ) ) ;
#34691 = ADVANCED_FACE ( 'NONE', ( #55186 ), #80894, .T. ) ;
#34692 = DIRECTION ( 'NONE',  ( -3.491481338843132961E-15, -0.000000000000000000, 1.000000000000000000 ) ) ;
#34693 = CARTESIAN_POINT ( 'NONE',  ( 0.3917322834645669549, 0.1049643490035304660, -1.154199475065616820 ) ) ;
#34694 = CARTESIAN_POINT ( 'NONE',  ( -0.3996062992125984925, -0.1070741851644056858, -2.169947506561679340 ) ) ;
#34695 = DIRECTION ( 'NONE',  ( 1.000000000000000000, 0.000000000000000000, 0.000000000000000000 ) ) ;
#34696 = CARTESIAN_POINT ( 'NONE',  ( -0.9448818897637790704, -0.1870078740157479769, 0.4822834645669291653 ) ) ;
#34697 = CARTESIAN_POINT ( 'NONE',  ( 1.017060367454068581, -0.05778040916215560624, -0.4822834645669293319 ) ) ;
#34698 = ORIENTED_EDGE ( 'NONE', *, *, #40133, .F. ) ;
#34699 = CARTESIAN_POINT ( 'NONE',  ( -1.601049868766403650, -0.6046776061558807314, 0.2411417322834647770 ) ) ;
#34700 = CARTESIAN_POINT ( 'NONE',  ( -1.102283499656470322, 1.111697496334393742, 0.2116636225555746376 ) ) ;
#34701 = ITEM_DEFINED_TRANSFORMATION ( 'NONE', 'NONE', #43631,  #22098 ) ;
#34702 = FACE_OUTER_BOUND ( 'NONE', #53871, .T. ) ;
#34703 = CARTESIAN_POINT ( 'NONE',  ( -0.3460692066303960313, 0.1998031496062989965, -1.992782152230971437 ) ) ;
#34704 = CARTESIAN_POINT ( 'NONE',  ( -1.528871391076114250, -0.5511811023622046335, 0.09757992244046803654 ) ) ;
#34705 = CARTESIAN_POINT ( 'NONE',  ( -0.3917322834645670104, -7.196005306013484475E-17, 0.1259842519685039908 ) ) ;
#34706 = CARTESIAN_POINT ( 'NONE',  ( 0.3543307086614181922, -0.6692913385826771977, 8.415575281601705876E-17 ) ) ;
#34707 = VECTOR ( 'NONE', #56349, 39.37007874015748143 ) ;
#34709 = CARTESIAN_POINT ( 'NONE',  ( -0.4461942257217840213, 0.1539470093639523085, 0.1968503937007873850 ) ) ;
#34708 = CARTESIAN_POINT ( 'NONE',  ( 1.423884514435696413, -0.3162353388693409650, -0.4822834645669289433 ) ) ;
#34710 = CARTESIAN_POINT ( 'NONE',  ( -0.8005249343832013809, -0.3690944881889763329, 0.3153832671262228327 ) ) ;
#34711 = CARTESIAN_POINT ( 'NONE',  ( 0.6233595800524942554, -0.05778040916215560624, -0.4822834645669293319 ) ) ;
#34712 = CARTESIAN_POINT ( 'NONE',  ( 1.364829396325459854, -0.5023911411419708095, -0.1820866141732282451 ) ) ;
#34713 = CARTESIAN_POINT ( 'NONE',  ( 0.1958661417322834497, 0.3392501089628018329, -1.169272022800837973 ) ) ;
#34714 = CARTESIAN_POINT ( 'NONE',  ( -0.6364829396325453192, -0.2845877964562159024, 0.3641732283464567677 ) ) ;
#34715 = CARTESIAN_POINT ( 'NONE',  ( 1.292650918635171564, -0.6692913385826773087, -0.1292274648535924053 ) ) ;
#34716 = CARTESIAN_POINT ( 'NONE',  ( 0.3129921259842522452, 1.527841585044882100, -3.001297844601851921E-19 ) ) ;
#34718 = EDGE_CURVE ( 'NONE', #33221, #9295, #53913, .T. ) ;
#34717 = CARTESIAN_POINT ( 'NONE',  ( 0.3608923884514443348, 0.2952755905511810774, -0.1292274648535930714 ) ) ;
#34719 = CARTESIAN_POINT ( 'NONE',  ( -0.9776902887139098386, 0.1771653543307087075, -0.09757992244046823083 ) ) ;
#34720 = CARTESIAN_POINT ( 'NONE',  ( -0.1312335958005241554, 0.1283753931104748280, 0.1820866141732283561 ) ) ;
#34721 = CARTESIAN_POINT ( 'NONE',  ( -0.3412073490813641308, -0.6046776061558807314, 0.2411417322834647770 ) ) ;
#34722 = CARTESIAN_POINT ( 'NONE',  ( 1.587926509186352586, -0.4281496062992127816, -0.4176697321401328100 ) ) ;
#34723 = CARTESIAN_POINT ( 'NONE',  ( 0.3392501089628018884, -0.1958661417322833942, 0.05575496243338393110 ) ) ;
#34724 = CARTESIAN_POINT ( 'NONE',  ( 0.2427821522309716595, -0.3162353388693409650, -0.4822834645669289433 ) ) ;
#34725 = B_SPLINE_CURVE_WITH_KNOTS ( 'NONE', 3,
 ( #76461, #57486, #67363, #69315, #30993, #11666, #24267, #25087, #61031, #9696, #3381, #62996, #56258, #29043, #80421, #22732, #48391, #82362, #81954, #75638, #50348, #43614, #5335, #46529, #1523, #20037, #1937, #19611, #77281, #59580, #19194, #46113, #20877, #65914, #25921, #78126, #51579, #20460, #45274, #59165 ),
 .UNSPECIFIED., .F., .F.,
 ( 4, 2, 2, 2, 2, 2, 2, 2, 2, 2, 2, 2, 2, 2, 2, 2, 2, 2, 2, 4 ),
 ( 0.000000000000000000, 0.002124304967526596203, 0.003186457451289890618, 0.003717533693171541295, 0.004248609935053191539, 0.005310762418816507638, 0.005841838660698156147, 0.006372914902579806390, 0.006903991144461454899, 0.007435067386343104275, 0.008497219870106381343, 0.009559372353869659278, 0.01009044859575129738, 0.01062152483763293374, 0.01168367732139621168, 0.01221475356327785672, 0.01274582980515950176, 0.01380798228892279184, 0.01487013477268608018, 0.01699443974021267595 ),
 .UNSPECIFIED. ) ;
#34726 = CARTESIAN_POINT ( 'NONE',  ( -1.646981627296586703, -0.05778040916215522460, 0.4822834645669289988 ) ) ;
#34727 = CARTESIAN_POINT ( 'NONE',  ( 5.785732909357575061E-17, -0.4724409448818898682, -1.572834645669291431 ) ) ;
#34728 = CARTESIAN_POINT ( 'NONE',  ( -0.9842519685039365918, -0.6692913385826771977, 8.415575281601705876E-17 ) ) ;
#34729 = CARTESIAN_POINT ( 'NONE',  ( -0.3083989501312330295, -0.08942795157527998196, 0.3641732283464567121 ) ) ;
#34730 = CARTESIAN_POINT ( 'NONE',  ( -1.200787401574802349, -0.5400638737290844871, 0.3530559997133364547 ) ) ;
#34731 = CARTESIAN_POINT ( 'NONE',  ( 0.3215223097112867578, -0.2845877964562161244, -0.3641732283464567121 ) ) ;
#34732 = CARTESIAN_POINT ( 'NONE',  ( -0.6233595800524928121, -0.08942795157527998196, 0.3641732283464567121 ) ) ;
#34733 = CARTESIAN_POINT ( 'NONE',  ( -0.8792650918635160906, 0.05413385826771626580, -0.4176697321401330321 ) ) ;
#34734 = CARTESIAN_POINT ( 'NONE',  ( -1.482939632545930975, -0.4281496062992127816, -0.4176697321401328100 ) ) ;
#34735 = CARTESIAN_POINT ( 'NONE',  ( 1.450131233595801428, -0.6692913385826773087, -0.1292274648535924053 ) ) ;
#34736 = DIRECTION ( 'NONE',  ( 1.000000000000000000, 0.000000000000000000, 3.455050906509825972E-15 ) ) ;
#34737 = CARTESIAN_POINT ( 'NONE',  ( 0.8202099737532814183, -0.5511811023622048555, -0.09757992244046775898 ) ) ;
#34738 = CARTESIAN_POINT ( 'NONE',  ( 0.5839895013123367340, 0.2952755905511811885, 0.1292274648535926551 ) ) ;
#34739 = DIRECTION ( 'NONE',  ( -3.491481338843133355E-15, -0.000000000000000000, 1.000000000000000000 ) ) ;
#34740 = CARTESIAN_POINT ( 'NONE',  ( 1.614173228346457378, 0.1771653543307087630, 0.000000000000000000 ) ) ;
#34741 = ORIENTED_EDGE ( 'NONE', *, *, #4418, .F. ) ;
#34742 = ADVANCED_FACE ( 'NONE', ( #69068 ), #51863, .T. ) ;
#34743 = CARTESIAN_POINT ( 'NONE',  ( 4.837279021331061486E-17, -0.3949938075777409963, 0.1594488188976377896 ) ) ;
#34744 = CARTESIAN_POINT ( 'NONE',  ( -1.240157480314959759, -0.4536011799217368745, -0.2665933059059886201 ) ) ;
#34745 = CARTESIAN_POINT ( 'NONE',  ( -0.4527559055118102749, -0.5400638737290845981, -0.3530559997133363437 ) ) ;
#34746 = CARTESIAN_POINT ( 'NONE',  ( 0.3280839895013130669, 0.05413385826771666132, 0.4176697321401328100 ) ) ;
#34747 = CARTESIAN_POINT ( 'NONE',  ( -1.646981627296586703, -0.2845877964562161244, -0.3641732283464567121 ) ) ;
#34748 = CARTESIAN_POINT ( 'NONE',  ( 0.1998031496062992463, 0.3460692066303959202, -2.268372703412073754 ) ) ;
#34749 = CARTESIAN_POINT ( 'NONE',  ( -1.437007874015747477, -0.5400638737290844871, 0.3530559997133364547 ) ) ;
#34750 = CARTESIAN_POINT ( 'NONE',  ( 0.6102362204724416372, 0.1660481256975883668, -0.3530559997133364547 ) ) ;
#34751 = CARTESIAN_POINT ( 'NONE',  ( 0.1181102362204730916, 0.2952755905511811885, 0.000000000000000000 ) ) ;
#34752 = CARTESIAN_POINT ( 'NONE',  ( 1.391076115485564868, -0.6046776061558807314, 0.2411417322834647770 ) ) ;
#34753 = CYLINDRICAL_SURFACE ( 'NONE', #35899, 0.5118110236220472231 ) ;
#34754 = CARTESIAN_POINT ( 'NONE',  ( -0.3460692066303958092, -0.1998031496062994683, -1.312335958005249381 ) ) ;
#34755 = CARTESIAN_POINT ( 'NONE',  ( -9.674558042662121740E-17, 0.3949938075777409963, -0.9448818897637795144 ) ) ;
#34756 = CARTESIAN_POINT ( 'NONE',  ( -0.2925321140481932924, 0.2925321140481931814, -2.381889763779527325 ) ) ;
#34757 = CARTESIAN_POINT ( 'NONE',  ( -0.7426113562972000981, 2.401574803149605586, -0.5309055118110235227 ) ) ;
#34758 = CARTESIAN_POINT ( 'NONE',  ( -0.3917322834645671215, 0.1049643490035301469, -0.3398950131233596239 ) ) ;
#34759 = CARTESIAN_POINT ( 'NONE',  ( 0.06561679790026316017, -0.004921259842519870586, -0.3153832671262229437 ) ) ;
#34760 = CARTESIAN_POINT ( 'NONE',  ( -0.5249343832020990641, -0.6046776061558809534, -0.2411417322834644161 ) ) ;
#34761 = CARTESIAN_POINT ( 'NONE',  ( 0.8858267716535438430, -0.5400638737290845981, -0.3530559997133363437 ) ) ;
#34762 = CARTESIAN_POINT ( 'NONE',  ( 0.3420746716998660508, 0.1974969037888705814, -2.097769028871391495 ) ) ;
#34763 = CARTESIAN_POINT ( 'NONE',  ( 0.09842519685039434474, 0.07958543189024085140, 0.2665933059059887866 ) ) ;
#34764 = EDGE_CURVE ( 'NONE', #25718, #23063, #10998, .T. ) ;
#34765 = CARTESIAN_POINT ( 'NONE',  ( -1.154855643044618851, 0.2306618581243848609, 0.2411417322834645549 ) ) ;
#34766 = CARTESIAN_POINT ( 'NONE',  ( -1.568241469816272105, -0.3162353388693409650, -0.4822834645669289433 ) ) ;
#34767 = CARTESIAN_POINT ( 'NONE',  ( 0.4091458600556403535, 0.2362204724409449896, -2.020997375328084100 ) ) ;
#34768 = CARTESIAN_POINT ( 'NONE',  ( 0.1906283239483269054, 0.3428707098288080735, -2.755905511811022279 ) ) ;
#34769 = ORIENTED_EDGE ( 'NONE', *, *, #18297, .F. ) ;
#34770 = EDGE_LOOP ( 'NONE', ( #13444, #80431, #73879, #26748 ) ) ;
#34771 = CARTESIAN_POINT ( 'NONE',  ( 1.017060367454068581, -0.05778040916215560624, -0.4822834645669293319 ) ) ;
#34772 = CARTESIAN_POINT ( 'NONE',  ( 1.541994750656168645, -0.5511811023622046335, 0.09757992244046803654 ) ) ;
#34774 = CARTESIAN_POINT ( 'NONE',  ( -1.076115485564303809, -0.6046776061558809534, -0.2411417322834644161 ) ) ;
#34773 = CARTESIAN_POINT ( 'NONE',  ( -1.102362204724408601, -0.1870078740157480601, -0.3641732283464567677 ) ) ;
#34775 = CARTESIAN_POINT ( 'NONE',  ( -0.3917322834645668994, -0.1049643490035306742, -2.488169660596113886 ) ) ;
#34776 = CARTESIAN_POINT ( 'NONE',  ( 0.4177787735907000366, 0.4110443821404751730, -1.559171609364239375 ) ) ;
#34777 = CARTESIAN_POINT ( 'NONE',  ( 1.358267716535433323, 0.1660481256975885056, 0.3530559997133364547 ) ) ;
#34778 = CARTESIAN_POINT ( 'NONE',  ( -1.660104986876639543, -0.05778040916215560624, -0.4822834645669293319 ) ) ;
#34779 = CARTESIAN_POINT ( 'NONE',  ( -0.06561679790026180015, -0.4281496062992127816, -0.4176697321401328100 ) ) ;
#34780 = CARTESIAN_POINT ( 'NONE',  ( -0.07217847769028813698, -0.3162353388693409650, -0.4822834645669289433 ) ) ;
#34781 = CARTESIAN_POINT ( 'NONE',  ( -1.358267716535432434, -0.5400638737290844871, 0.3530559997133364547 ) ) ;
#34782 = CARTESIAN_POINT ( 'NONE',  ( 0.1049643490035303689, 0.3917322834645670104, 0.07939632545931750440 ) ) ;
#34783 = CARTESIAN_POINT ( 'NONE',  ( 0.3215223097112867578, -0.05778040916215522460, 0.4822834645669289988 ) ) ;
#34784 = CARTESIAN_POINT ( 'NONE',  ( 0.3917322834645670104, 2.398668435337828261E-17, -1.685039370078740051 ) ) ;
#34785 = CARTESIAN_POINT ( 'NONE',  ( -1.305774278215222184, 0.1771653543307087630, 0.09757992244046791164 ) ) ;
#34786 = ORIENTED_EDGE ( 'NONE', *, *, #81347, .F. ) ;
#34787 = CARTESIAN_POINT ( 'NONE',  ( 0.3420746716998660508, -0.1974969037888703871, -2.467191601049868677 ) ) ;
#34788 = ORIENTED_EDGE ( 'NONE', *, *, #51075, .T. ) ;
#34789 = CARTESIAN_POINT ( 'NONE',  ( -1.622865925661502562, 1.365114174391409252, 0.4420857170566875327 ) ) ;
#34790 = CARTESIAN_POINT ( 'NONE',  ( -1.646981627296586703, -0.3162353388693409650, -0.4822834645669289433 ) ) ;
#34791 = CARTESIAN_POINT ( 'NONE',  ( -0.1998031496062991907, -0.3460692066303959757, -0.5380577427821522374 ) ) ;
#34792 = CARTESIAN_POINT ( 'NONE',  ( -1.332020997375327642, -0.3162353388693409650, -0.4822834645669289433 ) ) ;
#34793 = CARTESIAN_POINT ( 'NONE',  ( -0.3503937007874015630, 0.000000000000000000, 0.000000000000000000 ) ) ;
#34794 = CARTESIAN_POINT ( 'NONE',  ( 0.2017716535433070613, 0.2017716535433070613, -0.3937007874015748254 ) ) ;
#34795 = CARTESIAN_POINT ( 'NONE',  ( -0.3740157480314952876, 0.1660481256975885056, 0.3530559997133364547 ) ) ;
#34796 = CARTESIAN_POINT ( 'NONE',  ( -0.3392501089628017219, -0.1958661417322836718, -0.1371391076115486551 ) ) ;
#34797 =( BOUNDED_SURFACE ( )  B_SPLINE_SURFACE ( 1, 2, ( 
 ( #9082, #15824, #43813, #79798, #22530, #50142, #73888, #73475, #62793, #24880, #2764, #5535, #69104, #82561, #82160, #81753, #31200, #50548, #75839, #16228, #69518, #11452, #37109, #5127, #41875, #62367, #76252, #30792, #28423, #54083, #24476, #58109, #51369, #64021, #39604, #19832, #77072, #13109, #77496, #38762, #33303, #63608, #7632, #1321, #65293, #58964, #7198, #18988, #19406, #58538, #12273, #77918, #70758, #32447, #64439, #25709, #904, #5945, #37931, #45481, #6775, #57693, #26970, #31614, #57275, #82973, #475, #12688, #52215, #26130, #51792, #45057, #25292, #71178, #13520, #52635, #78340, #44229, #64860, #50958, #76655, #39176, #6362, #70332, #44635, #55, #38347, #32034, #32870, #26561, #69919, #20249, #45898, #71595, #13947, #72435, #28639, #34545, #66536, #2142, #59372, #79180, #47570, #9701, #67367, #35371, #41271, #27387, #1731, #8867, #66121, #46743, #21084, #59788, #40030, #53048, #14373, #54297, #80011, #22326, #61036, #34960, #40441, #34127, #8457, #21495, #73688, #47989, #21908, #40851, #20671, #73264, #60211, #65718, #72017, #78759, #3386, #79593, #29048, #8049, #33711, #27810, #53470, #53878, #16028, #15612, #66957, #41675, #14785, #47154, #9289, #2561, #46324, #72845, #15193, #28219, #54720, #60623, #2973, #10120, #42493, #62691, #16858, #3799, #75329, #37429, #22737, #75743, #4608, #69421, #69004, #42901, #50049, #24377, #5033, #80829, #30701, #55943, #36593, #62271, #55120, #74511, #11776, #68596, #31102, #80426, #56365, #10936, #4203, #68197, #18084, #81658, #29867, #49222, #30280, #74928, #63102, #16442, #43719, #5441, #48396, #74096, #43306, #23143, #55529, #11355, #42087, #82064, #23554, #23969, #17273, #61862, #37013, #67782, #35782, #49636, #17676, #61451, #29462, #48812, #10535, #81238, #36191, #76154, #24784, #58011, #83287, #70233, #71497, #50453, #18494, #44137, #44957, #25199, #64760, #70653, #19305, #38246, #12178, #31936, #376, #45800, #20150, #13845, #77394, #63514, #37836, #13009, #18893, #82876, #57177, #12588, #69829, #5844, #31520, #7099, #32769, #58436, #39503, #71080, #76565, #63924, #44542, #57597, #26459, #798, #26031, #76975, #56769, #51691, #38664, #50865, #6258, #25610, #65191, #32350, #7527, #51273, #64342, #6678, #19726, #45384, #52112, #13423, #39079, #77820, #82469, #66022, #8769, #53369, #33197, #7948, #71919, #52532, #67266, #65617, #9188, #46223, #78660, #15508, #52946, #39928, #28121, #73584, #58865, #28534, #40750, #22223, #21803, #79080, #2871, #60522, #41167, #33610, #66856, #34443, #72744, #15092, #59273, #27288, #47879, #21397, #1223, #26872, #34860, #47052, #40341, #20981, #54191, #60110, #8358, #2041, #66433, #27706, #15929, #78240, #79907, #41576, #20572, #14269, #79488, #1629, #34025, #47467, #46641, #72336, #59686, #14684, #2463, #53776, #73159, #35679, #41984, #16341, #67678, #23870, #74826, #10838, #81552, #10014, #75232, #29362, #61345, #4512, #49948, #35267, #4932, #17170, #81962, #49537, #55431, #62590, #36914, #17575, #3697, #43208, #68498, #49120, #42804, #55022, #80730, #24277, #81140, #43622, #9599, #68904, #23455, #16753, #23044, #30600, #36498, #42392, #61764, #62173, #4104, #75646, #28947, #56266, #17986, #60932, #3282, #55843, #48711, #68091, #11256, #54612, #80321, #36093, #30181, #29770, #74409, #22637, #48297, #73994, #10436, #12484, #82774, #693, #63004, #37331, #5343, #57495, #37735, #77289, #83186, #31834, #50768, #24689, #44440, #12904, #58331, #32664, #26349, #6578, #76054, #50357, #25509, #31415, #12077, #69733, #25096, #31002, #18398, #56670, #19620, #45282, #70977, #52010, #274, #5744, #76469, #57079, #70133, #38975, #13322, #70549, #6159, #69324, #38563, #51174, #82370, #44040, #63409, #77715, #44851, #20045, #18796, #38148, #63820, #76870, #19202, #64658, #6997, #51588, #64243, #11674, #32249, #57910, #25929, #45697, #72643, #47370, #9093, #52425, #21298, #78135, #46951, #46121, #2364, #71816, #20468, #14993, #79810, #39823, #14166, #65511, #15410, #34766, #40650, #78977, #60425, #66334, #2776, #54095, #52848, #20885, #40238, #59587, #8672, #71393, #28020 ),
 ( #7843, #33510, #60008, #27606, #53267, #59172, #7420, #1530, #53679, #8258, #34343, #79387, #27184, #21706, #73060, #41070, #1944, #33923, #78559, #66759, #46536, #14585, #72236, #28436, #65921, #13742, #1119, #39399, #65082, #33090, #58757, #26770, #54931, #80638, #23776, #43117, #54512, #22542, #30088, #22950, #4013, #42713, #49447, #68814, #3186, #17076, #17486, #10749, #36819, #68409, #62494, #30507, #75141, #11160, #28850, #16658, #61672, #41485, #67171, #9500, #48617, #81459, #55751, #36406, #74311, #42298, #80226, #29677, #4829, #56169, #35173, #60834, #48205, #41888, #73900, #22127, #62081, #16241, #29267, #4421, #73487, #47785, #67995, #10341, #36002, #3602, #15837, #67581, #9913, #23360, #55340, #35585, #61248, #81048, #49031, #74727, #70038, #50264, #6483, #12392, #44347, #63315, #37235, #56984, #25413, #70882, #45176, #13231, #19107, #5246, #62913, #38049, #43944, #24596, #82278, #37638, #17892, #30910, #75553, #32153, #57809, #176, #38881, #12809, #18300, #11984, #69639, #82681, #51488, #25829, #83092, #18706, #81872, #51077, #63725, #43529, #49853, #56577, #64560, #57401, #6897, #69228, #11575, #5653, #31319, #31736, #77191, #76775, #44755, #19523, #75962, #24998, #70451, #6065, #24184, #50673, #76372, #38463, #32568, #64149, #46019, #40973, #597, #40555, #78037, #64984, #53163, #15310, #26253, #53582, #65827, #47269, #46854, #20784, #27924, #2258, #66236, #58656, #8574, #33825, #14489, #40142, #32988, #52331, #72959, #46440, #8992, #58230, #34244, #72130, #65413, #20367, #79292, #59491, #7750, #27088, #8160, #52751, #66655, #77619, #21609, #51912, #19952, #72548, #45602, #21199, #71296, #13644, #59906, #39297, #7319, #78459, #1845, #1023, #26676, #71713, #1432, #14068, #39721, #78875, #33415, #27506, #59077, #14895, #68315, #68714, #79710, #53998, #47686, #54415, #60738, #61983, #16975, #35485, #17389, #35071, #9401, #75043, #34665, #61573, #36307, #81359, #41387, #10237, #67068, #35904, #3089, #74632, #28753, #80126, #3916, #60329, #22445, #48106, #73804, #4320, #23672, #29577, #67899, #49343, #55240, #43020, #2677, #41787, #9814, #29167, #48513, #80946, #28337, #42615, #29985, #74214, #23262, #22026, #73381, #15731, #16140, #61149, #67479, #3501, #54836, #80541, #22853, #16559, #42204, #48931, #10652, #55649, #76273, #69124, #56066, #30812, #76676, #56888, #57295, #37951, #62814, #69940, #82993, #44657, #50569, #82581, #37130, #70353, #75859, #63216, #11888, #63628, #18201, #5965, #49754, #5148, #37541, #24900, #69538, #5556, #43836, #31220, #12708, #32054, #43427, #11473, #19009, #18607, #44250, #31635, #38367, #57714, #75454, #25314, #6382, #51391, #11055, #50978, #64043, #77, #17792, #12295, #56477, #25730, #82180, #77095, #24497, #50163, #19427, #45079, #36713, #62388, #4726, #30400, #81774, #24084, #34457, #54207, #60126, #47894, #73602, #59701, #27720, #21413, #40763, #79503, #15944, #15525, #60537, #66448, #2477, #70782, #13133, #6798, #45503, #79094, #38784, #19854, #71200, #39199, #64882, #13543, #7221, #32893, #66873, #28136, #53792, #2056, #499, #53387, #34876, #8784, #41183, #21819, #47066, #47482, #9203, #2888, #73175, #28550, #72758, #79923, #15107, #22239, #64461, #32469, #58131, #26153, #51814, #77519, #25704, #56860, #18983, #39599, #39171, #19401, #12683, #25286, #899, #64435, #38341, #57688, #38758, #50, #77913, #24875, #52209, #45893, #26556, #20244, #51787, #63603, #64016, #19826, #82557, #64855, #32029, #77068, #51364, #70327, #45476, #50543, #76247, #6770, #45052, #44631, #71590, #18581, #44224, #69914, #70753, #57270, #13514, #13104, #32442, #6357, #12268, #58104, #470, #13942, #5530, #31194, #26126, #37926, #5939, #31609, #77491, #82968, #71173, #7193, #50954, #32865, #58533, #76651, #8451, #46738, #21904, #1316, #33298, #66532, #34122, #78755, #80008, #58959, #26965, #52630, #53465, #33706, #73259, #79174, #27805, #72430, #20666, #40436, #8863, #54293, #28635, #22321, #2557, #72012, #46319, #21490, #27382, #8044, #65713, #21080, #78335, #14368, #40025, #15608, #41267, #66953, #47985, #79589, #1725 ) ),
 .UNSPECIFIED., .F., .F., .F. ) 
 B_SPLINE_SURFACE_WITH_KNOTS ( ( 2, 2 ),
 ( 3, 2, 2, 2, 2, 2, 2, 2, 2, 2, 2, 2, 2, 2, 2, 2, 2, 2, 2, 2, 2, 2, 2, 2, 2, 2, 2, 2, 2, 2, 2, 2, 2, 2, 2, 2, 2, 2, 2, 2, 2, 2, 2, 2, 2, 2, 2, 2, 2, 2, 2, 2, 2, 2, 2, 2, 2, 2, 2, 2, 2, 2, 2, 2, 2, 2, 2, 2, 2, 2, 2, 2, 2, 2, 2, 2, 2, 2, 2, 2, 2, 2, 2, 2, 2, 2, 2, 2, 2, 2, 2, 2, 2, 2, 2, 2, 2, 2, 2, 2, 2, 2, 2, 2, 2, 2, 2, 2, 2, 2, 2, 2, 2, 2, 2, 2, 2, 2, 2, 2, 2, 2, 2, 2, 2, 2, 2, 2, 2, 2, 2, 2, 2, 2, 2, 2, 2, 2, 2, 2, 2, 2, 2, 2, 2, 2, 2, 2, 2, 2, 2, 2, 2, 2, 2, 2, 2, 2, 2, 2, 2, 2, 2, 2, 2, 2, 2, 2, 2, 2, 2, 2, 2, 2, 2, 2, 2, 2, 2, 2, 2, 2, 2, 2, 2, 2, 2, 2, 2, 2, 2, 2, 2, 2, 2, 2, 2, 2, 2, 2, 2, 2, 2, 2, 2, 2, 2, 2, 2, 2, 2, 2, 2, 2, 2, 2, 2, 2, 2, 2, 2, 2, 2, 2, 2, 2, 2, 2, 2, 2, 2, 2, 2, 2, 2, 2, 2, 2, 2, 2, 2, 2, 2, 2, 2, 2, 2, 2, 2, 2, 2, 2, 2, 2, 2, 3 ),
 ( 0.000000000000000000, 1.000000000000000000 ),
 ( 0.000000000000000000, 0.003787878787878787984, 0.007575757575757575968, 0.01136363636363636395, 0.01515151515151515194, 0.01893939393939393992, 0.02272727272727272790, 0.02651515151515151589, 0.03030303030303030387, 0.03409090909090908839, 0.03787878787878787984, 0.04166666666666666435, 0.04545454545454545581, 0.04924242424242424032, 0.05303030303030303177, 0.05681818181818181629, 0.06060606060606060774, 0.06439393939393939226, 0.06818181818181817677, 0.07196969696969697516, 0.07575757575757575968, 0.07954545454545454419, 0.08333333333333332871, 0.08712121212121212710, 0.09090909090909091161, 0.09469696969696969613, 0.09848484848484848064, 0.1022727272727272790, 0.1060606060606060635, 0.1098484848484848481, 0.1136363636363636326, 0.1174242424242424310, 0.1212121212121212155, 0.1250000000000000000, 0.1287878787878787845, 0.1325757575757575690, 0.1363636363636363535, 0.1401515151515151381, 0.1439393939393939503, 0.1477272727272727348, 0.1515151515151515194, 0.1553030303030303039, 0.1590909090909090884, 0.1628787878787878729, 0.1666666666666666574, 0.1704545454545454419, 0.1742424242424242542, 0.1780303030303030387, 0.1818181818181818232, 0.1856060606060606077, 0.1893939393939393923, 0.1931818181818181768, 0.1969696969696969613, 0.2007575757575757458, 0.2045454545454545581, 0.2083333333333333426, 0.2121212121212121271, 0.2159090909090909116, 0.2196969696969696961, 0.2234848484848484806, 0.2272727272727272652, 0.2310606060606060497, 0.2348484848484848619, 0.2386363636363636465, 0.2424242424242424310, 0.2462121212121212155, 0.2500000000000000000, 0.2537878787878787845, 0.2575757575757575690, 0.2613636363636363535, 0.2651515151515151381, 0.2689393939393939226, 0.2727272727272727071, 0.2765151515151514916, 0.2803030303030302761, 0.2840909090909091161, 0.2878787878787879007, 0.2916666666666666852, 0.2954545454545454697, 0.2992424242424242542, 0.3030303030303030387, 0.3068181818181818232, 0.3106060606060606077, 0.3143939393939393923, 0.3181818181818181768, 0.3219696969696969613, 0.3257575757575757458, 0.3295454545454545303, 0.3333333333333333148, 0.3371212121212120993, 0.3409090909090908839, 0.3446969696969697239, 0.3484848484848485084, 0.3522727272727272929, 0.3560606060606060774, 0.3598484848484848619, 0.3636363636363636465, 0.3674242424242424310, 0.3712121212121212155, 0.3750000000000000000, 0.3787878787878787845, 0.3825757575757575690, 0.3863636363636363535, 0.3901515151515151381, 0.3939393939393939226, 0.3977272727272727071, 0.4015151515151514916, 0.4053030303030302761, 0.4090909090909091161, 0.4128787878787879007, 0.4166666666666666852, 0.4204545454545454697, 0.4242424242424242542, 0.4280303030303030387, 0.4318181818181818232, 0.4356060606060606077, 0.4393939393939393923, 0.4431818181818181768, 0.4469696969696969613, 0.4507575757575757458, 0.4545454545454545303, 0.4583333333333333148, 0.4621212121212120993, 0.4659090909090908839, 0.4696969696969697239, 0.4734848484848485084, 0.4772727272727272929, 0.4810606060606060774, 0.4848484848484848619, 0.4886363636363636465, 0.4924242424242424310, 0.4962121212121212155, 0.5000000000000000000, 0.5037878787878787845, 0.5075757575757575690, 0.5113636363636363535, 0.5151515151515151381, 0.5189393939393939226, 0.5227272727272727071, 0.5265151515151514916, 0.5303030303030302761, 0.5340909090909090606, 0.5378787878787878451, 0.5416666666666666297, 0.5454545454545454142, 0.5492424242424241987, 0.5530303030303029832, 0.5568181818181817677, 0.5606060606060605522, 0.5643939393939394478, 0.5681818181818182323, 0.5719696969696970168, 0.5757575757575758013, 0.5795454545454545858, 0.5833333333333333703, 0.5871212121212121549, 0.5909090909090909394, 0.5946969696969697239, 0.5984848484848485084, 0.6022727272727272929, 0.6060606060606060774, 0.6098484848484848619, 0.6136363636363636465, 0.6174242424242424310, 0.6212121212121212155, 0.6250000000000000000, 0.6287878787878787845, 0.6325757575757575690, 0.6363636363636363535, 0.6401515151515151381, 0.6439393939393939226, 0.6477272727272727071, 0.6515151515151514916, 0.6553030303030302761, 0.6590909090909090606, 0.6628787878787878451, 0.6666666666666666297, 0.6704545454545454142, 0.6742424242424241987, 0.6780303030303029832, 0.6818181818181817677, 0.6856060606060605522, 0.6893939393939394478, 0.6931818181818182323, 0.6969696969696970168, 0.7007575757575758013, 0.7045454545454545858, 0.7083333333333333703, 0.7121212121212121549, 0.7159090909090909394, 0.7196969696969697239, 0.7234848484848485084, 0.7272727272727272929, 0.7310606060606060774, 0.7348484848484848619, 0.7386363636363636465, 0.7424242424242424310, 0.7462121212121212155, 0.7500000000000000000, 0.7537878787878787845, 0.7575757575757575690, 0.7613636363636363535, 0.7651515151515151381, 0.7689393939393939226, 0.7727272727272727071, 0.7765151515151514916, 0.7803030303030302761, 0.7840909090909090606, 0.7878787878787878451, 0.7916666666666666297, 0.7954545454545454142, 0.7992424242424241987, 0.8030303030303029832, 0.8068181818181817677, 0.8106060606060605522, 0.8143939393939394478, 0.8181818181818182323, 0.8219696969696970168, 0.8257575757575758013, 0.8295454545454545858, 0.8333333333333333703, 0.8371212121212121549, 0.8409090909090909394, 0.8446969696969697239, 0.8484848484848485084, 0.8522727272727272929, 0.8560606060606060774, 0.8598484848484848619, 0.8636363636363636465, 0.8674242424242424310, 0.8712121212121212155, 0.8750000000000000000, 0.8787878787878787845, 0.8825757575757575690, 0.8863636363636363535, 0.8901515151515151381, 0.8939393939393939226, 0.8977272727272727071, 0.9015151515151514916, 0.9053030303030302761, 0.9090909090909090606, 0.9128787878787878451, 0.9166666666666666297, 0.9204545454545454142, 0.9242424242424241987, 0.9280303030303029832, 0.9318181818181817677, 0.9356060606060605522, 0.9393939393939394478, 0.9431818181818182323, 0.9469696969696970168, 0.9507575757575758013, 0.9545454545454545858, 0.9583333333333333703, 0.9621212121212121549, 0.9659090909090909394 ),
 .UNSPECIFIED. ) 
 GEOMETRIC_REPRESENTATION_ITEM ( )  RATIONAL_B_SPLINE_SURFACE ( (
 ( 1.000000000000000000, 0.9659258262890683122, 1.000000000000000000, 0.9659258262890683122, 1.000000000000000000, 0.9659258262890683122, 1.000000000000000000, 0.9659258262890683122, 1.000000000000000000, 0.9659258262890683122, 1.000000000000000000, 0.9659258262890683122, 1.000000000000000000, 0.9659258262890683122, 1.000000000000000000, 0.9659258262890683122, 1.000000000000000000, 0.9659258262890683122, 1.000000000000000000, 0.9659258262890683122, 1.000000000000000000, 0.9659258262890683122, 1.000000000000000000, 0.9659258262890683122, 1.000000000000000000, 0.9659258262890683122, 1.000000000000000000, 0.9659258262890683122, 1.000000000000000000, 0.9659258262890683122, 1.000000000000000000, 0.9659258262890683122, 1.000000000000000000, 0.9659258262890683122, 1.000000000000000000, 0.9659258262890683122, 1.000000000000000000, 0.9659258262890683122, 1.000000000000000000, 0.9659258262890683122, 1.000000000000000000, 0.9659258262890683122, 1.000000000000000000, 0.9659258262890683122, 1.000000000000000000, 0.9659258262890683122, 1.000000000000000000, 0.9659258262890683122, 1.000000000000000000, 0.9659258262890683122, 1.000000000000000000, 0.9659258262890683122, 1.000000000000000000, 0.9659258262890683122, 1.000000000000000000, 0.9659258262890683122, 1.000000000000000000, 0.9659258262890683122, 1.000000000000000000, 0.9659258262890683122, 1.000000000000000000, 0.9659258262890683122, 1.000000000000000000, 0.9659258262890683122, 1.000000000000000000, 0.9659258262890683122, 1.000000000000000000, 0.9659258262890683122, 1.000000000000000000, 0.9659258262890683122, 1.000000000000000000, 0.9659258262890683122, 1.000000000000000000, 0.9659258262890683122, 1.000000000000000000, 0.9659258262890683122, 1.000000000000000000, 0.9659258262890683122, 1.000000000000000000, 0.9659258262890683122, 1.000000000000000000, 0.9659258262890683122, 1.000000000000000000, 0.9659258262890683122, 1.000000000000000000, 0.9659258262890683122, 1.000000000000000000, 0.9659258262890683122, 1.000000000000000000, 0.9659258262890683122, 1.000000000000000000, 0.9659258262890683122, 1.000000000000000000, 0.9659258262890683122, 1.000000000000000000, 0.9659258262890683122, 1.000000000000000000, 0.9659258262890683122, 1.000000000000000000, 0.9659258262890683122, 1.000000000000000000, 0.9659258262890683122, 1.000000000000000000, 0.9659258262890683122, 1.000000000000000000, 0.9659258262890683122, 1.000000000000000000, 0.9659258262890683122, 1.000000000000000000, 0.9659258262890683122, 1.000000000000000000, 0.9659258262890683122, 1.000000000000000000, 0.9659258262890683122, 1.000000000000000000, 0.9659258262890683122, 1.000000000000000000, 0.9659258262890683122, 1.000000000000000000, 0.9659258262890683122, 1.000000000000000000, 0.9659258262890683122, 1.000000000000000000, 0.9659258262890683122, 1.000000000000000000, 0.9659258262890683122, 1.000000000000000000, 0.9659258262890683122, 1.000000000000000000, 0.9659258262890683122, 1.000000000000000000, 0.9659258262890683122, 1.000000000000000000, 0.9659258262890683122, 1.000000000000000000, 0.9659258262890683122, 1.000000000000000000, 0.9659258262890683122, 1.000000000000000000, 0.9659258262890683122, 1.000000000000000000, 0.9659258262890683122, 1.000000000000000000, 0.9659258262890683122, 1.000000000000000000, 0.9659258262890683122, 1.000000000000000000, 0.9659258262890683122, 1.000000000000000000, 0.9659258262890683122, 1.000000000000000000, 0.9659258262890683122, 1.000000000000000000, 0.9659258262890683122, 1.000000000000000000, 0.9659258262890683122, 1.000000000000000000, 0.9659258262890683122, 1.000000000000000000, 0.9659258262890683122, 1.000000000000000000, 0.9659258262890683122, 1.000000000000000000, 0.9659258262890683122, 1.000000000000000000, 0.9659258262890683122, 1.000000000000000000, 0.9659258262890683122, 1.000000000000000000, 0.9659258262890683122, 1.000000000000000000, 0.9659258262890683122, 1.000000000000000000, 0.9659258262890683122, 1.000000000000000000, 0.9659258262890683122, 1.000000000000000000, 0.9659258262890683122, 1.000000000000000000, 0.9659258262890683122, 1.000000000000000000, 0.9659258262890683122, 1.000000000000000000, 0.9659258262890683122, 1.000000000000000000, 0.9659258262890683122, 1.000000000000000000, 0.9659258262890683122, 1.000000000000000000, 0.9659258262890683122, 1.000000000000000000, 0.9659258262890683122, 1.000000000000000000, 0.9659258262890683122, 1.000000000000000000, 0.9659258262890683122, 1.000000000000000000, 0.9659258262890683122, 1.000000000000000000, 0.9659258262890683122, 1.000000000000000000, 0.9659258262890683122, 1.000000000000000000, 0.9659258262890683122, 1.000000000000000000, 0.9659258262890683122, 1.000000000000000000, 0.9659258262890683122, 1.000000000000000000, 0.9659258262890683122, 1.000000000000000000, 0.9659258262890683122, 1.000000000000000000, 0.9659258262890683122, 1.000000000000000000, 0.9659258262890683122, 1.000000000000000000, 0.9659258262890683122, 1.000000000000000000, 0.9659258262890683122, 1.000000000000000000, 0.9659258262890683122, 1.000000000000000000, 0.9659258262890683122, 1.000000000000000000, 0.9659258262890683122, 1.000000000000000000, 0.9659258262890683122, 1.000000000000000000, 0.9659258262890683122, 1.000000000000000000, 0.9659258262890683122, 1.000000000000000000, 0.9659258262890683122, 1.000000000000000000, 0.9659258262890683122, 1.000000000000000000, 0.9659258262890683122, 1.000000000000000000, 0.9659258262890683122, 1.000000000000000000, 0.9659258262890683122, 1.000000000000000000, 0.9659258262890683122, 1.000000000000000000, 0.9659258262890683122, 1.000000000000000000, 0.9659258262890683122, 1.000000000000000000, 0.9659258262890683122, 1.000000000000000000, 0.9659258262890683122, 1.000000000000000000, 0.9659258262890683122, 1.000000000000000000, 0.9659258262890683122, 1.000000000000000000, 0.9659258262890683122, 1.000000000000000000, 0.9659258262890683122, 1.000000000000000000, 0.9659258262890683122, 1.000000000000000000, 0.9659258262890683122, 1.000000000000000000, 0.9659258262890683122, 1.000000000000000000, 0.9659258262890683122, 1.000000000000000000, 0.9659258262890683122, 1.000000000000000000, 0.9659258262890683122, 1.000000000000000000, 0.9659258262890683122, 1.000000000000000000, 0.9659258262890683122, 1.000000000000000000, 0.9659258262890683122, 1.000000000000000000, 0.9659258262890683122, 1.000000000000000000, 0.9659258262890683122, 1.000000000000000000, 0.9659258262890683122, 1.000000000000000000, 0.9659258262890683122, 1.000000000000000000, 0.9659258262890683122, 1.000000000000000000, 0.9659258262890683122, 1.000000000000000000, 0.9659258262890683122, 1.000000000000000000, 0.9659258262890683122, 1.000000000000000000, 0.9659258262890683122, 1.000000000000000000, 0.9659258262890683122, 1.000000000000000000, 0.9659258262890683122, 1.000000000000000000, 0.9659258262890683122, 1.000000000000000000, 0.9659258262890683122, 1.000000000000000000, 0.9659258262890683122, 1.000000000000000000, 0.9659258262890683122, 1.000000000000000000, 0.9659258262890683122, 1.000000000000000000, 0.9659258262890683122, 1.000000000000000000, 0.9659258262890683122, 1.000000000000000000, 0.9659258262890683122, 1.000000000000000000, 0.9659258262890683122, 1.000000000000000000, 0.9659258262890683122, 1.000000000000000000, 0.9659258262890683122, 1.000000000000000000, 0.9659258262890683122, 1.000000000000000000, 0.9659258262890683122, 1.000000000000000000, 0.9659258262890683122, 1.000000000000000000, 0.9659258262890683122, 1.000000000000000000, 0.9659258262890683122, 1.000000000000000000, 0.9659258262890683122, 1.000000000000000000, 0.9659258262890683122, 1.000000000000000000, 0.9659258262890683122, 1.000000000000000000, 0.9659258262890683122, 1.000000000000000000, 0.9659258262890683122, 1.000000000000000000, 0.9659258262890683122, 1.000000000000000000, 0.9659258262890683122, 1.000000000000000000, 0.9659258262890683122, 1.000000000000000000, 0.9659258262890683122, 1.000000000000000000, 0.9659258262890683122, 1.000000000000000000, 0.9659258262890683122, 1.000000000000000000, 0.9659258262890683122, 1.000000000000000000, 0.9659258262890683122, 1.000000000000000000, 0.9659258262890683122, 1.000000000000000000, 0.9659258262890683122, 1.000000000000000000, 0.9659258262890683122, 1.000000000000000000, 0.9659258262890683122, 1.000000000000000000, 0.9659258262890683122, 1.000000000000000000, 0.9659258262890683122, 1.000000000000000000, 0.9659258262890683122, 1.000000000000000000, 0.9659258262890683122, 1.000000000000000000, 0.9659258262890683122, 1.000000000000000000, 0.9659258262890683122, 1.000000000000000000, 0.9659258262890683122, 1.000000000000000000, 0.9659258262890683122, 1.000000000000000000, 0.9659258262890683122, 1.000000000000000000, 0.9659258262890683122, 1.000000000000000000, 0.9659258262890683122, 1.000000000000000000, 0.9659258262890683122, 1.000000000000000000, 0.9659258262890683122, 1.000000000000000000, 0.9659258262890683122, 1.000000000000000000, 0.9659258262890683122, 1.000000000000000000, 0.9659258262890683122, 1.000000000000000000, 0.9659258262890683122, 1.000000000000000000, 0.9659258262890683122, 1.000000000000000000, 0.9659258262890683122, 1.000000000000000000, 0.9659258262890683122, 1.000000000000000000, 0.9659258262890683122, 1.000000000000000000, 0.9659258262890683122, 1.000000000000000000, 0.9659258262890683122, 1.000000000000000000, 0.9659258262890683122, 1.000000000000000000, 0.9659258262890683122, 1.000000000000000000, 0.9659258262890683122, 1.000000000000000000, 0.9659258262890683122, 1.000000000000000000, 0.9659258262890683122, 1.000000000000000000, 0.9659258262890683122, 1.000000000000000000, 0.9659258262890683122, 1.000000000000000000, 0.9659258262890683122, 1.000000000000000000, 0.9659258262890683122, 1.000000000000000000, 0.9659258262890683122, 1.000000000000000000, 0.9659258262890683122, 1.000000000000000000, 0.9659258262890683122, 1.000000000000000000, 0.9659258262890683122, 1.000000000000000000, 0.9659258262890683122, 1.000000000000000000, 0.9659258262890683122, 1.000000000000000000, 0.9659258262890683122, 1.000000000000000000, 0.9659258262890683122, 1.000000000000000000, 0.9659258262890683122, 1.000000000000000000, 0.9659258262890683122, 1.000000000000000000, 0.9659258262890683122, 1.000000000000000000, 0.9659258262890683122, 1.000000000000000000, 0.9659258262890683122, 1.000000000000000000, 0.9659258262890683122, 1.000000000000000000, 0.9659258262890683122, 1.000000000000000000, 0.9659258262890683122, 1.000000000000000000, 0.9659258262890683122, 1.000000000000000000, 0.9659258262890683122, 1.000000000000000000, 0.9659258262890683122, 1.000000000000000000, 0.9659258262890683122, 1.000000000000000000, 0.9659258262890683122, 1.000000000000000000, 0.9659258262890683122, 1.000000000000000000, 0.9659258262890683122, 1.000000000000000000, 0.9659258262890683122, 1.000000000000000000, 0.9659258262890683122, 1.000000000000000000, 0.9659258262890683122, 1.000000000000000000, 0.9659258262890683122, 1.000000000000000000, 0.9659258262890683122, 1.000000000000000000, 0.9659258262890683122, 1.000000000000000000, 0.9659258262890683122, 1.000000000000000000, 0.9659258262890683122, 1.000000000000000000, 0.9659258262890683122, 1.000000000000000000, 0.9659258262890683122, 1.000000000000000000, 0.9659258262890683122, 1.000000000000000000, 0.9659258262890683122, 1.000000000000000000, 0.9659258262890683122, 1.000000000000000000, 0.9659258262890683122, 1.000000000000000000, 0.9659258262890683122, 1.000000000000000000, 0.9659258262890683122, 1.000000000000000000, 0.9659258262890683122, 1.000000000000000000),
 ( 1.000000000000000000, 0.9659258262890683122, 1.000000000000000000, 0.9659258262890683122, 1.000000000000000000, 0.9659258262890683122, 1.000000000000000000, 0.9659258262890683122, 1.000000000000000000, 0.9659258262890683122, 1.000000000000000000, 0.9659258262890683122, 1.000000000000000000, 0.9659258262890683122, 1.000000000000000000, 0.9659258262890683122, 1.000000000000000000, 0.9659258262890683122, 1.000000000000000000, 0.9659258262890683122, 1.000000000000000000, 0.9659258262890683122, 1.000000000000000000, 0.9659258262890683122, 1.000000000000000000, 0.9659258262890683122, 1.000000000000000000, 0.9659258262890683122, 1.000000000000000000, 0.9659258262890683122, 1.000000000000000000, 0.9659258262890683122, 1.000000000000000000, 0.9659258262890683122, 1.000000000000000000, 0.9659258262890683122, 1.000000000000000000, 0.9659258262890683122, 1.000000000000000000, 0.9659258262890683122, 1.000000000000000000, 0.9659258262890683122, 1.000000000000000000, 0.9659258262890683122, 1.000000000000000000, 0.9659258262890683122, 1.000000000000000000, 0.9659258262890683122, 1.000000000000000000, 0.9659258262890683122, 1.000000000000000000, 0.9659258262890683122, 1.000000000000000000, 0.9659258262890683122, 1.000000000000000000, 0.9659258262890683122, 1.000000000000000000, 0.9659258262890683122, 1.000000000000000000, 0.9659258262890683122, 1.000000000000000000, 0.9659258262890683122, 1.000000000000000000, 0.9659258262890683122, 1.000000000000000000, 0.9659258262890683122, 1.000000000000000000, 0.9659258262890683122, 1.000000000000000000, 0.9659258262890683122, 1.000000000000000000, 0.9659258262890683122, 1.000000000000000000, 0.9659258262890683122, 1.000000000000000000, 0.9659258262890683122, 1.000000000000000000, 0.9659258262890683122, 1.000000000000000000, 0.9659258262890683122, 1.000000000000000000, 0.9659258262890683122, 1.000000000000000000, 0.9659258262890683122, 1.000000000000000000, 0.9659258262890683122, 1.000000000000000000, 0.9659258262890683122, 1.000000000000000000, 0.9659258262890683122, 1.000000000000000000, 0.9659258262890683122, 1.000000000000000000, 0.9659258262890683122, 1.000000000000000000, 0.9659258262890683122, 1.000000000000000000, 0.9659258262890683122, 1.000000000000000000, 0.9659258262890683122, 1.000000000000000000, 0.9659258262890683122, 1.000000000000000000, 0.9659258262890683122, 1.000000000000000000, 0.9659258262890683122, 1.000000000000000000, 0.9659258262890683122, 1.000000000000000000, 0.9659258262890683122, 1.000000000000000000, 0.9659258262890683122, 1.000000000000000000, 0.9659258262890683122, 1.000000000000000000, 0.9659258262890683122, 1.000000000000000000, 0.9659258262890683122, 1.000000000000000000, 0.9659258262890683122, 1.000000000000000000, 0.9659258262890683122, 1.000000000000000000, 0.9659258262890683122, 1.000000000000000000, 0.9659258262890683122, 1.000000000000000000, 0.9659258262890683122, 1.000000000000000000, 0.9659258262890683122, 1.000000000000000000, 0.9659258262890683122, 1.000000000000000000, 0.9659258262890683122, 1.000000000000000000, 0.9659258262890683122, 1.000000000000000000, 0.9659258262890683122, 1.000000000000000000, 0.9659258262890683122, 1.000000000000000000, 0.9659258262890683122, 1.000000000000000000, 0.9659258262890683122, 1.000000000000000000, 0.9659258262890683122, 1.000000000000000000, 0.9659258262890683122, 1.000000000000000000, 0.9659258262890683122, 1.000000000000000000, 0.9659258262890683122, 1.000000000000000000, 0.9659258262890683122, 1.000000000000000000, 0.9659258262890683122, 1.000000000000000000, 0.9659258262890683122, 1.000000000000000000, 0.9659258262890683122, 1.000000000000000000, 0.9659258262890683122, 1.000000000000000000, 0.9659258262890683122, 1.000000000000000000, 0.9659258262890683122, 1.000000000000000000, 0.9659258262890683122, 1.000000000000000000, 0.9659258262890683122, 1.000000000000000000, 0.9659258262890683122, 1.000000000000000000, 0.9659258262890683122, 1.000000000000000000, 0.9659258262890683122, 1.000000000000000000, 0.9659258262890683122, 1.000000000000000000, 0.9659258262890683122, 1.000000000000000000, 0.9659258262890683122, 1.000000000000000000, 0.9659258262890683122, 1.000000000000000000, 0.9659258262890683122, 1.000000000000000000, 0.9659258262890683122, 1.000000000000000000, 0.9659258262890683122, 1.000000000000000000, 0.9659258262890683122, 1.000000000000000000, 0.9659258262890683122, 1.000000000000000000, 0.9659258262890683122, 1.000000000000000000, 0.9659258262890683122, 1.000000000000000000, 0.9659258262890683122, 1.000000000000000000, 0.9659258262890683122, 1.000000000000000000, 0.9659258262890683122, 1.000000000000000000, 0.9659258262890683122, 1.000000000000000000, 0.9659258262890683122, 1.000000000000000000, 0.9659258262890683122, 1.000000000000000000, 0.9659258262890683122, 1.000000000000000000, 0.9659258262890683122, 1.000000000000000000, 0.9659258262890683122, 1.000000000000000000, 0.9659258262890683122, 1.000000000000000000, 0.9659258262890683122, 1.000000000000000000, 0.9659258262890683122, 1.000000000000000000, 0.9659258262890683122, 1.000000000000000000, 0.9659258262890683122, 1.000000000000000000, 0.9659258262890683122, 1.000000000000000000, 0.9659258262890683122, 1.000000000000000000, 0.9659258262890683122, 1.000000000000000000, 0.9659258262890683122, 1.000000000000000000, 0.9659258262890683122, 1.000000000000000000, 0.9659258262890683122, 1.000000000000000000, 0.9659258262890683122, 1.000000000000000000, 0.9659258262890683122, 1.000000000000000000, 0.9659258262890683122, 1.000000000000000000, 0.9659258262890683122, 1.000000000000000000, 0.9659258262890683122, 1.000000000000000000, 0.9659258262890683122, 1.000000000000000000, 0.9659258262890683122, 1.000000000000000000, 0.9659258262890683122, 1.000000000000000000, 0.9659258262890683122, 1.000000000000000000, 0.9659258262890683122, 1.000000000000000000, 0.9659258262890683122, 1.000000000000000000, 0.9659258262890683122, 1.000000000000000000, 0.9659258262890683122, 1.000000000000000000, 0.9659258262890683122, 1.000000000000000000, 0.9659258262890683122, 1.000000000000000000, 0.9659258262890683122, 1.000000000000000000, 0.9659258262890683122, 1.000000000000000000, 0.9659258262890683122, 1.000000000000000000, 0.9659258262890683122, 1.000000000000000000, 0.9659258262890683122, 1.000000000000000000, 0.9659258262890683122, 1.000000000000000000, 0.9659258262890683122, 1.000000000000000000, 0.9659258262890683122, 1.000000000000000000, 0.9659258262890683122, 1.000000000000000000, 0.9659258262890683122, 1.000000000000000000, 0.9659258262890683122, 1.000000000000000000, 0.9659258262890683122, 1.000000000000000000, 0.9659258262890683122, 1.000000000000000000, 0.9659258262890683122, 1.000000000000000000, 0.9659258262890683122, 1.000000000000000000, 0.9659258262890683122, 1.000000000000000000, 0.9659258262890683122, 1.000000000000000000, 0.9659258262890683122, 1.000000000000000000, 0.9659258262890683122, 1.000000000000000000, 0.9659258262890683122, 1.000000000000000000, 0.9659258262890683122, 1.000000000000000000, 0.9659258262890683122, 1.000000000000000000, 0.9659258262890683122, 1.000000000000000000, 0.9659258262890683122, 1.000000000000000000, 0.9659258262890683122, 1.000000000000000000, 0.9659258262890683122, 1.000000000000000000, 0.9659258262890683122, 1.000000000000000000, 0.9659258262890683122, 1.000000000000000000, 0.9659258262890683122, 1.000000000000000000, 0.9659258262890683122, 1.000000000000000000, 0.9659258262890683122, 1.000000000000000000, 0.9659258262890683122, 1.000000000000000000, 0.9659258262890683122, 1.000000000000000000, 0.9659258262890683122, 1.000000000000000000, 0.9659258262890683122, 1.000000000000000000, 0.9659258262890683122, 1.000000000000000000, 0.9659258262890683122, 1.000000000000000000, 0.9659258262890683122, 1.000000000000000000, 0.9659258262890683122, 1.000000000000000000, 0.9659258262890683122, 1.000000000000000000, 0.9659258262890683122, 1.000000000000000000, 0.9659258262890683122, 1.000000000000000000, 0.9659258262890683122, 1.000000000000000000, 0.9659258262890683122, 1.000000000000000000, 0.9659258262890683122, 1.000000000000000000, 0.9659258262890683122, 1.000000000000000000, 0.9659258262890683122, 1.000000000000000000, 0.9659258262890683122, 1.000000000000000000, 0.9659258262890683122, 1.000000000000000000, 0.9659258262890683122, 1.000000000000000000, 0.9659258262890683122, 1.000000000000000000, 0.9659258262890683122, 1.000000000000000000, 0.9659258262890683122, 1.000000000000000000, 0.9659258262890683122, 1.000000000000000000, 0.9659258262890683122, 1.000000000000000000, 0.9659258262890683122, 1.000000000000000000, 0.9659258262890683122, 1.000000000000000000, 0.9659258262890683122, 1.000000000000000000, 0.9659258262890683122, 1.000000000000000000, 0.9659258262890683122, 1.000000000000000000, 0.9659258262890683122, 1.000000000000000000, 0.9659258262890683122, 1.000000000000000000, 0.9659258262890683122, 1.000000000000000000, 0.9659258262890683122, 1.000000000000000000, 0.9659258262890683122, 1.000000000000000000, 0.9659258262890683122, 1.000000000000000000, 0.9659258262890683122, 1.000000000000000000, 0.9659258262890683122, 1.000000000000000000, 0.9659258262890683122, 1.000000000000000000, 0.9659258262890683122, 1.000000000000000000, 0.9659258262890683122, 1.000000000000000000, 0.9659258262890683122, 1.000000000000000000, 0.9659258262890683122, 1.000000000000000000, 0.9659258262890683122, 1.000000000000000000, 0.9659258262890683122, 1.000000000000000000, 0.9659258262890683122, 1.000000000000000000, 0.9659258262890683122, 1.000000000000000000, 0.9659258262890683122, 1.000000000000000000, 0.9659258262890683122, 1.000000000000000000, 0.9659258262890683122, 1.000000000000000000, 0.9659258262890683122, 1.000000000000000000, 0.9659258262890683122, 1.000000000000000000, 0.9659258262890683122, 1.000000000000000000, 0.9659258262890683122, 1.000000000000000000, 0.9659258262890683122, 1.000000000000000000, 0.9659258262890683122, 1.000000000000000000, 0.9659258262890683122, 1.000000000000000000, 0.9659258262890683122, 1.000000000000000000, 0.9659258262890683122, 1.000000000000000000, 0.9659258262890683122, 1.000000000000000000, 0.9659258262890683122, 1.000000000000000000, 0.9659258262890683122, 1.000000000000000000, 0.9659258262890683122, 1.000000000000000000, 0.9659258262890683122, 1.000000000000000000, 0.9659258262890683122, 1.000000000000000000, 0.9659258262890683122, 1.000000000000000000, 0.9659258262890683122, 1.000000000000000000, 0.9659258262890683122, 1.000000000000000000, 0.9659258262890683122, 1.000000000000000000, 0.9659258262890683122, 1.000000000000000000, 0.9659258262890683122, 1.000000000000000000, 0.9659258262890683122, 1.000000000000000000, 0.9659258262890683122, 1.000000000000000000, 0.9659258262890683122, 1.000000000000000000, 0.9659258262890683122, 1.000000000000000000, 0.9659258262890683122, 1.000000000000000000, 0.9659258262890683122, 1.000000000000000000, 0.9659258262890683122, 1.000000000000000000, 0.9659258262890683122, 1.000000000000000000, 0.9659258262890683122, 1.000000000000000000, 0.9659258262890683122, 1.000000000000000000, 0.9659258262890683122, 1.000000000000000000, 0.9659258262890683122, 1.000000000000000000, 0.9659258262890683122, 1.000000000000000000, 0.9659258262890683122, 1.000000000000000000, 0.9659258262890683122, 1.000000000000000000, 0.9659258262890683122, 1.000000000000000000, 0.9659258262890683122, 1.000000000000000000, 0.9659258262890683122, 1.000000000000000000, 0.9659258262890683122, 1.000000000000000000, 0.9659258262890683122, 1.000000000000000000) ) ) 
 REPRESENTATION_ITEM ( '' )  SURFACE ( )  );
#34798 = CARTESIAN_POINT ( 'NONE',  ( -0.4068241469816264999, -0.3690944881889763329, 0.3153832671262228327 ) ) ;
#34799 = CARTESIAN_POINT ( 'NONE',  ( -0.6955380577427815458, -0.3690944881889765550, -0.3153832671262227771 ) ) ;
#34800 = CARTESIAN_POINT ( 'NONE',  ( -1.003937007874014853, 0.1660481256975885056, 0.3530559997133364547 ) ) ;
#34801 = CARTESIAN_POINT ( 'NONE',  ( 1.089238845144357537, -0.4281496062992124485, 0.4176697321401328655 ) ) ;
#34802 = CARTESIAN_POINT ( 'NONE',  ( -0.9186351706036736120, -0.6046776061558809534, -0.2411417322834644161 ) ) ;
#34803 = CARTESIAN_POINT ( 'NONE',  ( -0.1958661417322834220, -0.3392501089628018884, -0.05774278215223092176 ) ) ;
#34804 = ORIENTED_EDGE ( 'NONE', *, *, #75114, .F. ) ;
#34805 = CARTESIAN_POINT ( 'NONE',  ( -1.397637795275589623, -0.5400638737290845981, -0.3530559997133363437 ) ) ;
#34806 = CARTESIAN_POINT ( 'NONE',  ( -1.606174037523448561, 0.2952824826768989941, 0.01137383275704648665 ) ) ;
#34807 = CARTESIAN_POINT ( 'NONE',  ( -1.712598425196849572, 0.1660481256975885056, 0.3530559997133364547 ) ) ;
#34808 = CARTESIAN_POINT ( 'NONE',  ( -0.4724409448818895907, -0.1265901696524993070, -1.463254593175853158 ) ) ;
#34809 = CARTESIAN_POINT ( 'NONE',  ( 1.894990545102974044, 1.111478976311914613, -0.2095522481616541033 ) ) ;
#34810 = CARTESIAN_POINT ( 'NONE',  ( -0.1049643490035302024, -0.3917322834645671215, -0.5367454068241469534 ) ) ;
#34811 = CARTESIAN_POINT ( 'NONE',  ( -0.1958661417322834220, -0.3392501089628018884, -2.354986876640420057 ) ) ;
#34812 = CARTESIAN_POINT ( 'NONE',  ( -0.5577427821522301654, -0.3162353388693405765, 0.4822834645669290543 ) ) ;
#34813 = CARTESIAN_POINT ( 'NONE',  ( 1.253280839895013710, -0.05778040916215560624, -0.4822834645669293319 ) ) ;
#34814 = CARTESIAN_POINT ( 'NONE',  ( 0.1070741851644053388, 0.3996062992125986035, -0.07020997375328086321 ) ) ;
#34816 = DIRECTION ( 'NONE',  ( 0.000000000000000000, 0.000000000000000000, -1.000000000000000000 ) ) ;
#34815 = CARTESIAN_POINT ( 'NONE',  ( -1.561679790026246017, 0.05413385826771666132, 0.4176697321401328100 ) ) ;
#34817 = EDGE_CURVE ( 'NONE', #24575, #52448, #17739, .T. ) ;
#34818 = CARTESIAN_POINT ( 'NONE',  ( -1.338582677165353729, -0.1870078740157480879, -0.4822834645669291653 ) ) ;
#34819 = CARTESIAN_POINT ( 'NONE',  ( -0.9776902887139098386, -0.6692913385826771977, 0.1292274648535927661 ) ) ;
#34820 = CARTESIAN_POINT ( 'NONE',  ( 0.3392501089628018329, -0.1958661417322834497, 0.1299405756243587895 ) ) ;
#34821 = CARTESIAN_POINT ( 'NONE',  ( 0.4724409448818904789, -0.1870078740157479769, 0.3641732283464567677 ) ) ;
#34822 = CARTESIAN_POINT ( 'NONE',  ( 0.1049643490035304799, -0.3917322834645669549, -0.3274278215223098143 ) ) ;
#34823 = EDGE_CURVE ( 'NONE', #58545, #46767, #64953, .T. ) ;
#34824 = CARTESIAN_POINT ( 'NONE',  ( 0.2296587926509192634, -0.2845877964562159024, 0.3641732283464567677 ) ) ;
#34825 = CARTESIAN_POINT ( 'NONE',  ( 1.049868766404200127, -0.5023911411419708095, -0.1820866141732282451 ) ) ;
#34826 = CARTESIAN_POINT ( 'NONE',  ( 1.108923884514436242, -0.05778040916215522460, 0.4822834645669289988 ) ) ;
#34827 = CARTESIAN_POINT ( 'NONE',  ( -0.4790026246719152336, -0.08942795157528024563, -0.3641732283464568787 ) ) ;
#34828 = CARTESIAN_POINT ( 'NONE',  ( 0.1049643490035303689, 0.3917322834645670104, -2.032808398950130879 ) ) ;
#34829 = CARTESIAN_POINT ( 'NONE',  ( -1.187664041994749731, -0.3162353388693405765, 0.4822834645669290543 ) ) ;
#34830 = CARTESIAN_POINT ( 'NONE',  ( -1.102362204724408601, -0.1870078740157480601, -0.3641732283464567677 ) ) ;
#34831 = CARTESIAN_POINT ( 'NONE',  ( 0.2362204724409449064, 0.4091458600556404646, -0.5360892388451443669 ) ) ;
#34832 = CARTESIAN_POINT ( 'NONE',  ( -0.9514435695538050464, -0.08942795157528024563, -0.3641732283464568787 ) ) ;
#34833 = CARTESIAN_POINT ( 'NONE',  ( -0.2690288713910754526, -0.6692913385826771977, 0.1292274648535927661 ) ) ;
#34834 = DIRECTION ( 'NONE',  ( -0.000000000000000000, -1.000000000000000000, -0.000000000000000000 ) ) ;
#34835 = CARTESIAN_POINT ( 'NONE',  ( 0.5839895013123367340, -0.5511811023622048555, -0.09757992244046775898 ) ) ;
#34836 = CARTESIAN_POINT ( 'NONE',  ( -0.1115485564304456306, 0.1771653543307087075, -0.09757992244046823083 ) ) ;
#34837 = CARTESIAN_POINT ( 'NONE',  ( -0.6496062992125976043, 0.1660481256975883668, -0.3530559997133364547 ) ) ;
#34838 = CARTESIAN_POINT ( 'NONE',  ( -1.653543307086613234, -0.1870078740157480879, -0.4822834645669291653 ) ) ;
#34839 = CARTESIAN_POINT ( 'NONE',  ( -1.646051170424378096, -0.1870078740157480046, 1.254653134982923898E-17 ) ) ;
#34840 = CARTESIAN_POINT ( 'NONE',  ( -0.01312335958005186876, 0.05413385826771626580, -0.4176697321401330321 ) ) ;
#34841 = CARTESIAN_POINT ( 'NONE',  ( -0.1070741851644051862, -0.3996062992125986590, -1.566272965879265344 ) ) ;
#34842 = CARTESIAN_POINT ( 'NONE',  ( 1.430446194225722500, 0.05413385826771666132, 0.4176697321401328100 ) ) ;
#34843 = CARTESIAN_POINT ( 'NONE',  ( -0.4265091863517051496, 0.1771653543307087075, -0.09757992244046823083 ) ) ;
#34844 = CARTESIAN_POINT ( 'NONE',  ( 0.006561679790026889343, -0.05778040916215522460, 0.4822834645669289988 ) ) ;
#34845 = CARTESIAN_POINT ( 'NONE',  ( -1.568241469816272105, -0.3162353388693409650, -0.4822834645669289433 ) ) ;
#34846 = CARTESIAN_POINT ( 'NONE',  ( -1.633858267716534529, 0.07958543189024085140, 0.2665933059059887866 ) ) ;
#34847 = CARTESIAN_POINT ( 'NONE',  ( 1.338582677165355062, -0.1870078740157479769, 0.4822834645669291653 ) ) ;
#34848 = CARTESIAN_POINT ( 'NONE',  ( -0.6627296587926503335, -0.5511811023622046335, 0.09757992244046803654 ) ) ;
#34849 = DIRECTION ( 'NONE',  ( -0.000000000000000000, -1.000000000000000000, -0.000000000000000000 ) ) ;
#34850 = CARTESIAN_POINT ( 'NONE',  ( 0.1998031496062994405, -0.3460692066303958092, -0.09186351706036746667 ) ) ;
#34851 = B_SPLINE_CURVE_WITH_KNOTS ( 'NONE', 3,
 ( #60377, #73853, #55291, #48983, #48568, #15784, #42252, #67119, #9450, #35121, #67947, #10289 ),
 .UNSPECIFIED., .F., .F.,
 ( 4, 2, 2, 2, 2, 4 ),
 ( 0.007992874908875390386, 0.009303755029337522353, 0.01061463514979965432, 0.01192551527026178629, 0.01258095533049285661, 0.01323639539072392866 ),
 .UNSPECIFIED. ) ;
#34852 = CARTESIAN_POINT ( 'NONE',  ( 0.2891555358219910499, 0.2891555358219910499, 0.01968503937007868437 ) ) ;
#34853 = CARTESIAN_POINT ( 'NONE',  ( -0.07128922432405460086, -0.3857547143408426860, -1.492482962822815952E-17 ) ) ;
#34854 = CARTESIAN_POINT ( 'NONE',  ( 1.325459317585302665, -0.004921259842519870586, -0.3153832671262229437 ) ) ;
#34855 = DIRECTION ( 'NONE',  ( -0.000000000000000000, 1.000000000000000000, -0.000000000000000000 ) ) ;
#34856 = CARTESIAN_POINT ( 'NONE',  ( 0.6824146981627303710, 0.2306618581243847221, -0.2411417322834647770 ) ) ;
#34857 = CARTESIAN_POINT ( 'NONE',  ( -0.2867679344610365999, 0.2867679344610364889, -2.309055118110235671 ) ) ;
#34858 = CARTESIAN_POINT ( 'NONE',  ( 1.318897637795276356, -0.4536011799217367080, 0.2665933059059888421 ) ) ;
#34859 = CARTESIAN_POINT ( 'NONE',  ( 0.3083989501312343062, -0.05778040916215560624, -0.4822834645669293319 ) ) ;
#34860 = CARTESIAN_POINT ( 'NONE',  ( -0.4330708661417315697, -0.6692913385826771977, 8.415575281601705876E-17 ) ) ;
#34861 = CARTESIAN_POINT ( 'NONE',  ( 1.496062992125985147, -0.1870078740157479769, 0.4822834645669291653 ) ) ;
#34862 = CARTESIAN_POINT ( 'NONE',  ( -0.1265901696524993347, 0.4724409448818895907, -0.7939632545931758489 ) ) ;
#34863 = CARTESIAN_POINT ( 'NONE',  ( 0.1938976377952755792, -0.1938976377952756069, 0.07874015748031495954 ) ) ;
#34864 = CARTESIAN_POINT ( 'NONE',  ( 0.2099737532808405305, 0.1283753931104746893, -0.1820866141732285504 ) ) ;
#34865 = AXIS2_PLACEMENT_3D ( 'NONE', #19876, #77115, #77541 ) ;
#34866 = ORIENTED_EDGE ( 'NONE', *, *, #79768, .F. ) ;
#34867 = CARTESIAN_POINT ( 'NONE',  ( -0.3917322834645670104, -0.1049643490035307020, -0.2001505493776396805 ) ) ;
#34868 = VERTEX_POINT ( 'NONE', #20527 ) ;
#34869 = CARTESIAN_POINT ( 'NONE',  ( -0.4790026246719154557, -0.3162353388693405765, 0.4822834645669290543 ) ) ;
#34870 = CARTESIAN_POINT ( 'NONE',  ( 1.154855643044620184, 0.2306618581243847221, -0.2411417322834647770 ) ) ;
#34871 = CARTESIAN_POINT ( 'NONE',  ( 0.2034120734908144990, -0.6692913385826771977, 0.1292274648535927661 ) ) ;
#34872 = CARTESIAN_POINT ( 'NONE',  ( -0.4593175853018364174, -0.3690944881889765550, -0.3153832671262227771 ) ) ;
#34873 = CARTESIAN_POINT ( 'NONE',  ( 0.6299212598425204535, -0.1870078740157480879, -0.4822834645669291653 ) ) ;
#34874 = CARTESIAN_POINT ( 'NONE',  ( -1.122047244094487306, 0.1660481256975883668, -0.3530559997133364547 ) ) ;
#34875 = CARTESIAN_POINT ( 'NONE',  ( -0.5052493438320203589, -0.6692913385826771977, 0.1292274648535927661 ) ) ;
#34876 = CARTESIAN_POINT ( 'NONE',  ( -0.9186351706036736120, 0.2306618581243848609, 0.2411417322834645549 ) ) ;
#34877 = CARTESIAN_POINT ( 'NONE',  ( 1.049868766404200127, -0.6046776061558809534, -0.2411417322834644161 ) ) ;
#34878 = CARTESIAN_POINT ( 'NONE',  ( 0.7349081364829402885, -0.6046776061558809534, -0.2411417322834644161 ) ) ;
#34879 = CARTESIAN_POINT ( 'NONE',  ( 0.7742782152230979209, 0.05413385826771626580, -0.4176697321401330321 ) ) ;
#34880 = CARTESIAN_POINT ( 'NONE',  ( -0.3917322834645669549, -0.1049643490035306603, -0.6679790026246719137 ) ) ;
#34881 = CARTESIAN_POINT ( 'NONE',  ( -0.01968503937007793844, 0.07958543189024071263, -0.2665933059059888421 ) ) ;
#34882 = ORIENTED_EDGE ( 'NONE', *, *, #21903, .F. ) ;
#34883 = CARTESIAN_POINT ( 'NONE',  ( 0.2891555358219910499, -0.2891555358219909944, -0.8858267716535433989 ) ) ;
#34884 = ORIENTED_EDGE ( 'NONE', *, *, #48192, .F. ) ;
#34885 = CARTESIAN_POINT ( 'NONE',  ( -0.8792650918635160906, -0.004921259842519870586, -0.3153832671262229437 ) ) ;
#34886 = CARTESIAN_POINT ( 'NONE',  ( -0.3215223097112853146, -0.05778040916215560624, -0.4822834645669293319 ) ) ;
#34887 = CARTESIAN_POINT ( 'NONE',  ( 2.593354744918233923, 1.408268389154266220, 0.4567427728026669520 ) ) ;
#34888 = CARTESIAN_POINT ( 'NONE',  ( -0.4527559055118102749, 0.1660481256975885056, 0.3530559997133364547 ) ) ;
#34889 = CARTESIAN_POINT ( 'NONE',  ( -0.2690288713910754526, 0.2952755905511810774, -0.1292274648535930714 ) ) ;
#34890 = CARTESIAN_POINT ( 'NONE',  ( -1.345144356955379816, -0.3162353388693405765, 0.4822834645669290543 ) ) ;
#34891 = CARTESIAN_POINT ( 'NONE',  ( -1.430446194225721390, -0.4281496062992124485, 0.4176697321401328655 ) ) ;
#34892 = CARTESIAN_POINT ( 'NONE',  ( 1.108923884514436686, -0.2845877964562161244, -0.3641732283464567121 ) ) ;
#34893 = CARTESIAN_POINT ( 'NONE',  ( -0.2362204724409451284, 0.4091458600556402425, -0.4048556430446194621 ) ) ;
#34894 = CARTESIAN_POINT ( 'NONE',  ( 0.2362186021731760011, 0.1771678480211529849, 5.713829339669467267 ) ) ;
#34895 = CARTESIAN_POINT ( 'NONE',  ( 0.6627296587926515548, 0.1771653543307087630, 0.09757992244046791164 ) ) ;
#34896 = CARTESIAN_POINT ( 'NONE',  ( 0.03937007874015833325, -0.6692913385826771977, 8.415575281601705876E-17 ) ) ;
#34897 = CARTESIAN_POINT ( 'NONE',  ( 0.1509186351706045259, -0.05778040916215560624, -0.4822834645669293319 ) ) ;
#34898 = ORIENTED_EDGE ( 'NONE', *, *, #13664, .T. ) ;
#34899 = CARTESIAN_POINT ( 'NONE',  ( -0.1070741851644056997, 0.3996062992125986035, -1.738845144356955696 ) ) ;
#34900 = CARTESIAN_POINT ( 'NONE',  ( 0.5314960629920996160, 2.742784459617114923, 2.516666435443592142 ) ) ;
#34901 = ORIENTED_EDGE ( 'NONE', *, *, #26367, .F. ) ;
#34902 = CARTESIAN_POINT ( 'NONE',  ( 4.893765752498283308E-17, -0.3996062992125985480, -1.100393700787401619 ) ) ;
#34903 = CARTESIAN_POINT ( 'NONE',  ( 0.1998031496062992463, 0.3460692066303959202, -0.3786089238845143923 ) ) ;
#34904 = CARTESIAN_POINT ( 'NONE',  ( -0.5052493438320203589, -0.6692913385826771977, 0.1292274648535927661 ) ) ;
#34905 = CARTESIAN_POINT ( 'NONE',  ( 0.3458507752293908943, 0.3458507752293908943, -0.1377952755905511861 ) ) ;
#34906 = CARTESIAN_POINT ( 'NONE',  ( 0.1958661417322836440, -0.3392501089628017219, -2.381233595800524849 ) ) ;
#34907 = CARTESIAN_POINT ( 'NONE',  ( 1.660104986876641320, -0.05778040916215522460, 0.4822834645669289988 ) ) ;
#34908 = CARTESIAN_POINT ( 'NONE',  ( 0.9448818897637802916, -0.1870078740157479769, 0.4822834645669291653 ) ) ;
#34909 = CARTESIAN_POINT ( 'NONE',  ( 1.095800524934383846, -0.05778040916215560624, -0.4822834645669293319 ) ) ;
#34910 = CARTESIAN_POINT ( 'NONE',  ( -0.7874015748031489847, -0.1870078740157480601, -0.3641732283464567677 ) ) ;
#34911 = CARTESIAN_POINT ( 'NONE',  ( 5.463695987328526437E-16, -0.1870078740157479769, 0.4822834645669291653 ) ) ;
#34912 = CARTESIAN_POINT ( 'NONE',  ( 0.2362204724409449064, 0.4091458600556404646, -1.795931758530183719 ) ) ;
#34913 = CARTESIAN_POINT ( 'NONE',  ( 8.195543980992789655E-16, -0.1870078740157480601, -0.3641732283464567677 ) ) ;
#34914 = CARTESIAN_POINT ( 'NONE',  ( -0.3477690288713905509, -0.6692913385826771977, 0.1292274648535927661 ) ) ;
#34915 = ADVANCED_FACE ( 'NONE', ( #78618 ), #14225, .F. ) ;
#34916 = CARTESIAN_POINT ( 'NONE',  ( -9.674558042662122972E-17, 0.3949938075777409963, -1.809055118110236560 ) ) ;
#34917 = CARTESIAN_POINT ( 'NONE',  ( 1.548556430446194954, -0.5023911411419708095, 0.1820866141732285504 ) ) ;
#34918 = CARTESIAN_POINT ( 'NONE',  ( 0.1968503937007881344, 0.1771653543307087630, 0.000000000000000000 ) ) ;
#34919 = DIRECTION ( 'NONE',  ( 0.000000000000000000, -1.000000000000000000, 1.408710688920637755E-15 ) ) ;
#34920 = CARTESIAN_POINT ( 'NONE',  ( -1.174540682414697335, -0.3162353388693409650, -0.4822834645669289433 ) ) ;
#34921 = CARTESIAN_POINT ( 'NONE',  ( -0.7020997375328074108, -0.08942795157527998196, 0.3641732283464567121 ) ) ;
#34922 = CARTESIAN_POINT ( 'NONE',  ( 2.362204724409448620, 1.724409448818898127, 0.5118110236220555498 ) ) ;
#34923 = CARTESIAN_POINT ( 'NONE',  ( -1.089238845144356427, 0.05413385826771666132, 0.4176697321401328100 ) ) ;
#34924 = CARTESIAN_POINT ( 'NONE',  ( -0.1640419947506553400, -0.05778040916215560624, -0.4822834645669293319 ) ) ;
#34925 = CARTESIAN_POINT ( 'NONE',  ( 0.1070741851644053388, 0.3996062992125986035, -2.589895013123359568 ) ) ;
#34926 =( BOUNDED_CURVE ( )  B_SPLINE_CURVE ( 1, ( #19976, #25856 ),
 .UNSPECIFIED., .F., .F. ) 
 B_SPLINE_CURVE_WITH_KNOTS ( ( 2, 2 ),
 ( 3.469446951953614189E-18, 0.002000000000000005246 ),
 .UNSPECIFIED. ) 
 CURVE ( )  GEOMETRIC_REPRESENTATION_ITEM ( )  RATIONAL_B_SPLINE_CURVE ( ( 0.9875488213027527884, 0.9875488213027527884 ) ) 
 REPRESENTATION_ITEM ( '' )  );
#34927 = CARTESIAN_POINT ( 'NONE',  ( 0.3392501089628018329, -0.1958661417322834497, -2.547224778706350445 ) ) ;
#34928 = CARTESIAN_POINT ( 'NONE',  ( -0.5314960629921126056, 2.753838553078472362, -3.842312626974350831 ) ) ;
#34929 = CARTESIAN_POINT ( 'NONE',  ( 0.2821522309711292364, 0.1771653543307087075, -0.09757992244046823083 ) ) ;
#34930 = CARTESIAN_POINT ( 'NONE',  ( 1.161417322834646271, 0.1660481256975883668, -0.3530559997133364547 ) ) ;
#34931 = CARTESIAN_POINT ( 'NONE',  ( -1.122047244094487306, -0.4536011799217367080, 0.2665933059059888421 ) ) ;
#34932 = CARTESIAN_POINT ( 'NONE',  ( 1.128608923884515169, -0.6046776061558809534, -0.2411417322834644161 ) ) ;
#34933 = CARTESIAN_POINT ( 'NONE',  ( -1.397637795275589623, 0.07958543189024085140, 0.2665933059059887866 ) ) ;
#34934 = CARTESIAN_POINT ( 'NONE',  ( -0.5446194225721777693, -0.3162353388693409650, -0.4822834645669289433 ) ) ;
#34935 = CARTESIAN_POINT ( 'NONE',  ( 0.3412073490813655186, -0.5023911411419708095, -0.1820866141732282451 ) ) ;
#34936 = DIRECTION ( 'NONE',  ( 0.000000000000000000, -0.7071067811865496822, -0.7071067811865454633 ) ) ;
#34937 = CARTESIAN_POINT ( 'NONE',  ( 0.8398950131233602345, 0.1283753931104746893, -0.1820866141732285504 ) ) ;
#34938 = CARTESIAN_POINT ( 'NONE',  ( -0.01312335958005186876, 0.05413385826771626580, -0.4176697321401330321 ) ) ;
#34939 = CARTESIAN_POINT ( 'NONE',  ( 0.3460692066303959202, -0.1998031496062991630, -0.4967191601049869010 ) ) ;
#34940 = CARTESIAN_POINT ( 'NONE',  ( -0.8727034120734901146, -0.05778040916215560624, -0.4822834645669293319 ) ) ;
#34941 = CARTESIAN_POINT ( 'NONE',  ( 0.1958661417322836440, -0.3392501089628017219, -1.751312335958005395 ) ) ;
#34942 = CARTESIAN_POINT ( 'NONE',  ( 0.9448818897637802916, -0.1870078740157479769, 0.3641732283464567677 ) ) ;
#34943 = CARTESIAN_POINT ( 'NONE',  ( 0.2493438320209980519, 0.05413385826771666132, 0.4176697321401328100 ) ) ;
#34944 = CARTESIAN_POINT ( 'NONE',  ( -0.1115485564304453947, -0.6692913385826771977, 0.1292274648535927661 ) ) ;
#34945 = CARTESIAN_POINT ( 'NONE',  ( -0.5446194225721777693, -0.08942795157527998196, 0.3641732283464567121 ) ) ;
#34946 = CARTESIAN_POINT ( 'NONE',  ( 1.010498687664042716, 0.009842519685039144428, -0.3409548833797004797 ) ) ;
#34947 = CARTESIAN_POINT ( 'NONE',  ( -0.2952755905511803003, -0.4536011799217368745, -0.2665933059059886201 ) ) ;
#34948 = CARTESIAN_POINT ( 'NONE',  ( 0.2887139107611556010, 0.2306618581243847221, -0.2411417322834647770 ) ) ;
#34949 = CARTESIAN_POINT ( 'NONE',  ( -0.7283464566929126471, 0.07958543189024071263, -0.2665933059059888421 ) ) ;
#34950 = CARTESIAN_POINT ( 'NONE',  ( -0.2925321140481930149, -0.2925321140481933480, -0.7657480314960628531 ) ) ;
#34951 = CARTESIAN_POINT ( 'NONE',  ( -1.056430446194224881, -0.6692913385826771977, 0.1292274648535927661 ) ) ;
#34952 = CARTESIAN_POINT ( 'NONE',  ( 0.1938976377952755792, -0.1938976377952756069, -0.3740157480314971750 ) ) ;
#34953 = VERTEX_POINT ( 'NONE', #754 ) ;
#34954 = CARTESIAN_POINT ( 'NONE',  ( -1.207349081364828880, 0.1283753931104746893, -0.1820866141732285504 ) ) ;
#34955 = CARTESIAN_POINT ( 'NONE',  ( -0.4330708661417315697, 0.2952755905511811885, 0.000000000000000000 ) ) ;
#34956 = CARTESIAN_POINT ( 'NONE',  ( 0.3917864676224471765, 0.04037479286078551194, -1.220472440943932702 ) ) ;
#34957 = CARTESIAN_POINT ( 'NONE',  ( -1.207349081364828436, -0.6046776061558807314, 0.2411417322834647770 ) ) ;
#34958 = DIRECTION ( 'NONE',  ( 0.000000000000000000, 1.000000000000000000, -0.000000000000000000 ) ) ;
#34959 = CARTESIAN_POINT ( 'NONE',  ( 1.167979002624672580, -0.4281496062992124485, 0.4176697321401328655 ) ) ;
#34960 = CARTESIAN_POINT ( 'NONE',  ( 0.8989501312335964611, 0.2952755905511811885, 0.1292274648535926551 ) ) ;
#34961 = CYLINDRICAL_SURFACE ( 'NONE', #61043, 0.3149606299212598381 ) ;
#34962 = DIRECTION ( 'NONE',  ( -1.000000000000000000, -3.083952846180990281E-16, 0.000000000000000000 ) ) ;
#34963 = CARTESIAN_POINT ( 'NONE',  ( 1.437007874015748810, 0.07958543189024085140, 0.2665933059059887866 ) ) ;
#34964 = CARTESIAN_POINT ( 'NONE',  ( -9.787531504996567848E-17, 0.3996062992125986035, -0.6299212598425196763 ) ) ;
#34965 = ORIENTED_EDGE ( 'NONE', *, *, #13087, .F. ) ;
#34966 = CARTESIAN_POINT ( 'NONE',  ( -0.6692913385826764205, 0.1771653543307087630, 0.000000000000000000 ) ) ;
#34967 = CARTESIAN_POINT ( 'NONE',  ( 0.1049643490035303689, 0.3917322834645670104, -2.032808398950130879 ) ) ;
#34968 = ORIENTED_EDGE ( 'NONE', *, *, #35375, .F. ) ;
#34969 = CARTESIAN_POINT ( 'NONE',  ( 0.8267716535433077274, 0.2952755905511811885, 0.000000000000000000 ) ) ;
#34970 = CARTESIAN_POINT ( 'NONE',  ( -0.01312335958005186876, -0.4281496062992124485, 0.4176697321401328655 ) ) ;
#34971 = CARTESIAN_POINT ( 'NONE',  ( -0.5183727034120726440, 0.2952755905511811885, 0.1292274648535926551 ) ) ;
#34972 = CARTESIAN_POINT ( 'NONE',  ( 1.587926509186352586, -0.4281496062992127816, -0.4176697321401328100 ) ) ;
#34973 = CARTESIAN_POINT ( 'NONE',  ( -1.299212598425196097, 0.1771653543307087630, 0.000000000000000000 ) ) ;
#34974 = CARTESIAN_POINT ( 'NONE',  ( 0.5027385518334777093, 1.496062992125983815, -0.5309055118110237448 ) ) ;
#34975 = CARTESIAN_POINT ( 'NONE',  ( 0.2952755905511819101, 0.1660481256975883668, -0.3530559997133364547 ) ) ;
#34976 = CARTESIAN_POINT ( 'NONE',  ( -0.7545931758530176614, -0.6692913385826773087, -0.1292274648535924053 ) ) ;
#34977 = CARTESIAN_POINT ( 'NONE',  ( -0.2867679344610366554, 0.2867679344610365444, -1.359560736711598938 ) ) ;
#34978 = CARTESIAN_POINT ( 'NONE',  ( -1.200787401574802349, -0.5400638737290844871, 0.3530559997133364547 ) ) ;
#34979 = CARTESIAN_POINT ( 'NONE',  ( 0.1654368116759125928, 1.092466590690394090, -2.846817106506551287 ) ) ;
#34980 = CARTESIAN_POINT ( 'NONE',  ( 1.108923884514436686, -0.3162353388693409650, -0.4822834645669289433 ) ) ;
#34981 = CARTESIAN_POINT ( 'NONE',  ( 1.122047244094488860, -0.4536011799217368745, -0.2665933059059886201 ) ) ;
#34982 = VERTEX_POINT ( 'NONE', #20941 ) ;
#34983 = CARTESIAN_POINT ( 'NONE',  ( 0.3949938075777409408, 0.1058382717557500574, 0.03280839895013118457 ) ) ;
#34984 = CARTESIAN_POINT ( 'NONE',  ( -0.6102362204724400829, -0.5400638737290845981, -0.3530559997133363437 ) ) ;
#34985 = ORIENTED_EDGE ( 'NONE', *, *, #5920, .T. ) ;
#34986 = CARTESIAN_POINT ( 'NONE',  ( 0.2624671916010504757, -0.5023911411419708095, -0.1820866141732282451 ) ) ;
#34987 = CARTESIAN_POINT ( 'NONE',  ( -1.082677165354329896, 0.1660481256975885056, 0.3530559997133364547 ) ) ;
#34988 = CARTESIAN_POINT ( 'NONE',  ( 1.167979002624672580, 0.05413385826771626580, -0.4176697321401330321 ) ) ;
#34989 = CARTESIAN_POINT ( 'NONE',  ( 0.6627296587926515548, 0.2952755905511811885, 0.1292274648535926551 ) ) ;
#34990 = CARTESIAN_POINT ( 'NONE',  ( -0.2099737532808391705, -0.6046776061558809534, -0.2411417322834644161 ) ) ;
#34991 = CARTESIAN_POINT ( 'NONE',  ( -0.9842519685039360366, 0.2952755905511811885, 0.000000000000000000 ) ) ;
#34992 = CARTESIAN_POINT ( 'NONE',  ( 0.3392501089628018329, 0.1958661417322835607, -2.105643044619422533 ) ) ;
#34993 = CARTESIAN_POINT ( 'NONE',  ( -1.522309711286088607, 0.2306618581243847221, -0.2411417322834647770 ) ) ;
#34994 = CARTESIAN_POINT ( 'NONE',  ( -0.4330708661417315697, -0.6692913385826771977, 8.415575281601705876E-17 ) ) ;
#34995 = CARTESIAN_POINT ( 'NONE',  ( -0.6692913385826764205, 0.1771653543307087630, 0.000000000000000000 ) ) ;
#34996 = CARTESIAN_POINT ( 'NONE',  ( 1.272965879265092637, -0.4281496062992127816, -0.4176697321401328100 ) ) ;
#34997 = CARTESIAN_POINT ( 'NONE',  ( 1.515748031496063408, 0.1660481256975885056, 0.3530559997133364547 ) ) ;
#34998 = CARTESIAN_POINT ( 'NONE',  ( -0.9055118110236215490, 0.2952755905511811885, 0.000000000000000000 ) ) ;
#34999 = CARTESIAN_POINT ( 'NONE',  ( 0.3996062992125986035, -0.1070741851644052972, -0.03083989501312336262 ) ) ;
#35000 = CARTESIAN_POINT ( 'NONE',  ( 0.5511811023622054106, -0.1870078740157480879, -0.4822834645669291653 ) ) ;
#35001 = CARTESIAN_POINT ( 'NONE',  ( 0.3460692066303959757, -0.1998031496062991907, -1.679790026246719137 ) ) ;
#35002 = LINE ( 'NONE', #53926, #10659 ) ;
#35003 = ADVANCED_FACE ( 'NONE', ( #33567 ), #7483, .T. ) ;
#35004 = CARTESIAN_POINT ( 'NONE',  ( -0.09842519685039295696, -0.5400638737290844871, 0.3530559997133364547 ) ) ;
#35005 = CARTESIAN_POINT ( 'NONE',  ( -1.200787401574802349, -0.4536011799217367080, 0.2665933059059888421 ) ) ;
#35006 = CARTESIAN_POINT ( 'NONE',  ( 0.9514435695538062676, -0.2845877964562161244, -0.3641732283464567121 ) ) ;
#35007 = CARTESIAN_POINT ( 'NONE',  ( -0.4091458600556402980, -0.2362204724409451284, -0.6017060367454067915 ) ) ;
#35008 = CARTESIAN_POINT ( 'NONE',  ( 1.318897637795276356, -0.4536011799217367080, 0.2665933059059888421 ) ) ;
#35009 = CARTESIAN_POINT ( 'NONE',  ( 0.9842519685039375910, 0.2952755905511811885, 0.000000000000000000 ) ) ;
#35010 = ADVANCED_FACE ( 'NONE', ( #40706 ), #54582, .F. ) ;
#35011 = CARTESIAN_POINT ( 'NONE',  ( 0.3949938075777409963, 2.418639510665530743E-17, -0.5098425196850394636 ) ) ;
#35012 = CARTESIAN_POINT ( 'NONE',  ( -0.4986876640419942164, -0.6046776061558807314, 0.2411417322834647770 ) ) ;
#35013 = CARTESIAN_POINT ( 'NONE',  ( 2.362204724409448620, 1.724409448818900570, 8.247593713802677664E-15 ) ) ;
#35014 = CARTESIAN_POINT ( 'NONE',  ( 1.430446194225722500, -0.004921259842519576551, 0.3153832671262227771 ) ) ;
#35015 = CARTESIAN_POINT ( 'NONE',  ( -0.4855643044619415427, -0.4281496062992124485, 0.4176697321401328655 ) ) ;
#35016 = CARTESIAN_POINT ( 'NONE',  ( -0.1058382717557503072, 0.3949938075777408852, -0.3982939632545932640 ) ) ;
#35017 = CARTESIAN_POINT ( 'NONE',  ( 1.397637795275591177, 0.1660481256975883668, -0.3530559997133364547 ) ) ;
#35018 = CARTESIAN_POINT ( 'NONE',  ( 0.01968503937007930540, 0.1660481256975885056, 0.3530559997133364547 ) ) ;
#35019 = CARTESIAN_POINT ( 'NONE',  ( 0.5643044619422579178, -0.004921259842519576551, 0.3153832671262227771 ) ) ;
#35020 = CARTESIAN_POINT ( 'NONE',  ( -0.4026890765610274814, 1.286118078602604520, -1.047337338654595662 ) ) ;
#35021 = CARTESIAN_POINT ( 'NONE',  ( 0.4396325459317593221, 0.1771653543307087075, -0.09757992244046823083 ) ) ;
#35022 = CARTESIAN_POINT ( 'NONE',  ( -1.515748031496062076, -0.5400638737290844871, 0.3530559997133364547 ) ) ;
#35023 = CARTESIAN_POINT ( 'NONE',  ( 0.2925321140481932369, -0.2925321140481931814, -1.277559055118110187 ) ) ;
#35024 = CARTESIAN_POINT ( 'NONE',  ( 0.8333333333333340365, -0.6692913385826771977, 0.1292274648535927661 ) ) ;
#35025 = CARTESIAN_POINT ( 'NONE',  ( -0.3917322834645671215, 0.1049643490035301469, -0.9698162729658791337 ) ) ;
#35026 = CARTESIAN_POINT ( 'NONE',  ( 1.627296587926509996, -0.5023911411419708095, 0.1820866141732285504 ) ) ;
#35027 = CARTESIAN_POINT ( 'NONE',  ( 0.09842519685039433086, 0.1660481256975885056, 0.3530559997133364547 ) ) ;
#35028 = CARTESIAN_POINT ( 'NONE',  ( 0.1968503937007881344, 0.1771653543307087630, 0.000000000000000000 ) ) ;
#35029 = CARTESIAN_POINT ( 'NONE',  ( -0.02624671916010428221, 0.2306618581243847221, -0.2411417322834647770 ) ) ;
#35030 = CARTESIAN_POINT ( 'NONE',  ( 1.358267716535433323, 0.07958543189024085140, 0.2665933059059887866 ) ) ;
#35031 = CARTESIAN_POINT ( 'NONE',  ( -1.410761154855642463, -0.08942795157527998196, 0.3641732283464567121 ) ) ;
#35032 = CARTESIAN_POINT ( 'NONE',  ( -1.489501312335957062, -0.3162353388693409650, -0.4822834645669289433 ) ) ;
#35033 = CARTESIAN_POINT ( 'NONE',  ( 0.4002624671916016896, -0.05778040916215522460, 0.4822834645669289988 ) ) ;
#35034 = CARTESIAN_POINT ( 'NONE',  ( 1.069553805774278832, 0.2952755905511810774, -0.1292274648535930714 ) ) ;
#35035 = DIRECTION ( 'NONE',  ( 0.000000000000000000, 0.000000000000000000, -1.000000000000000000 ) ) ;
#35036 = CARTESIAN_POINT ( 'NONE',  ( 0.5774278215223103139, -0.6046776061558809534, -0.2411417322834644161 ) ) ;
#35037 = CARTESIAN_POINT ( 'NONE',  ( 1.351706036745407680, 0.05413385826771666132, 0.4176697321401328100 ) ) ;
#35038 = CARTESIAN_POINT ( 'NONE',  ( 1.043307086614173818, 0.1660481256975885056, 0.3530559997133364547 ) ) ;
#35039 = CARTESIAN_POINT ( 'NONE',  ( -0.1265901696524986964, -0.4724409448818899238, -0.3064304461942256586 ) ) ;
#35040 = CARTESIAN_POINT ( 'NONE',  ( 0.6430446194225729606, -0.3690944881889765550, -0.3153832671262227771 ) ) ;
#35041 = CARTESIAN_POINT ( 'NONE',  ( 1.502624671916010790, -0.05778040916215522460, 0.4822834645669289988 ) ) ;
#35042 = CARTESIAN_POINT ( 'NONE',  ( -0.9711286089238838626, 0.1283753931104746893, -0.1820866141732285504 ) ) ;
#35043 = CARTESIAN_POINT ( 'NONE',  ( 0.7086614173228352742, -0.1870078740157480601, -0.3641732283464567677 ) ) ;
#35044 = CARTESIAN_POINT ( 'NONE',  ( 0.07874015748031558404, -0.1870078740157479769, 0.4822834645669291653 ) ) ;
#35045 = CARTESIAN_POINT ( 'NONE',  ( 0.6102362204724416372, -0.5400638737290844871, 0.3530559997133364547 ) ) ;
#35046 = CARTESIAN_POINT ( 'NONE',  ( -0.3937007874015740483, -0.1870078740157479769, 0.4822834645669291653 ) ) ;
#35047 = CARTESIAN_POINT ( 'NONE',  ( 0.2230971128608929543, -0.004921259842519870586, -0.3153832671262229437 ) ) ;
#35048 = CARTESIAN_POINT ( 'NONE',  ( 0.9842519685039375910, 0.2952755905511811885, 0.000000000000000000 ) ) ;
#35049 = DIRECTION ( 'NONE',  ( 0.000000000000000000, -0.5150380749100549327, -0.8571673007021117785 ) ) ;
#35050 = CARTESIAN_POINT ( 'NONE',  ( -1.102362204724408601, -0.1870078740157479769, 0.4822834645669291653 ) ) ;
#35052 = CARTESIAN_POINT ( 'NONE',  ( -0.1070741851644057135, 0.3996062992125985480, -0.7939632545931758489 ) ) ;
#35051 = CARTESIAN_POINT ( 'NONE',  ( -1.035207913594495599, 0.02791078216816347476, -0.4328096321851898631 ) ) ;
#35053 = FACE_BOUND ( 'NONE', #38185, .T. ) ;
#35054 = CARTESIAN_POINT ( 'NONE',  ( -0.8923884514435688198, -0.6046776061558807314, 0.2411417322834647770 ) ) ;
#35055 = CARTESIAN_POINT ( 'NONE',  ( -0.5183727034120726440, -0.6692913385826773087, -0.1292274648535924053 ) ) ;
#35056 = CARTESIAN_POINT ( 'NONE',  ( -9.787531504996567848E-17, 0.3996062992125986035, -2.834645669291338432 ) ) ;
#35057 = CARTESIAN_POINT ( 'NONE',  ( 0.3949938075777409408, 0.1058382717557500574, -2.486876640419947382 ) ) ;
#35058 = ORIENTED_EDGE ( 'NONE', *, *, #82449, .T. ) ;
#35059 = CARTESIAN_POINT ( 'NONE',  ( 0.5839895013123367340, 0.1771653543307087630, 0.09757992244046791164 ) ) ;
#35060 = CARTESIAN_POINT ( 'NONE',  ( -0.3917322834645669549, -0.1049643490035306603, -1.140419947506561282 ) ) ;
#35061 = CARTESIAN_POINT ( 'NONE',  ( 1.312335958005249825, 0.2306618581243847221, -0.2411417322834647770 ) ) ;
#35062 = EDGE_CURVE ( 'NONE', #3377, #44828, #70682, .T. ) ;
#35063 = CARTESIAN_POINT ( 'NONE',  ( 0.4128820156421557641, 1.303693191736402301, -1.389518450040436948 ) ) ;
#35064 = CARTESIAN_POINT ( 'NONE',  ( -1.364829396325458521, 0.1283753931104746893, -0.1820866141732285504 ) ) ;
#35065 = CARTESIAN_POINT ( 'NONE',  ( 1.607611548556431069, -0.6692913385826773087, -0.1292274648535924053 ) ) ;
#35066 = CARTESIAN_POINT ( 'NONE',  ( -1.666666666666665853, 0.05413385826771626580, -0.4176697321401330321 ) ) ;
#35067 = CARTESIAN_POINT ( 'NONE',  ( -0.3392501089628018329, -0.1958661417322836440, -0.4474872458979509138 ) ) ;
#35068 = CARTESIAN_POINT ( 'NONE',  ( -0.1640419947506553400, -0.05778040916215560624, -0.4822834645669293319 ) ) ;
#35069 = CARTESIAN_POINT ( 'NONE',  ( -0.7808398950131225646, -0.08942795157527998196, 0.3641732283464567121 ) ) ;
#35070 = CARTESIAN_POINT ( 'NONE',  ( 0.7349081364829402885, -0.6046776061558809534, -0.2411417322834644161 ) ) ;
#35071 = CARTESIAN_POINT ( 'NONE',  ( 0.07217847769028949700, -0.05778040916215560624, -0.4822834645669293319 ) ) ;
#35072 = CARTESIAN_POINT ( 'NONE',  ( -0.4724409448818898682, -8.678599364036362592E-17, -0.03937007874015747977 ) ) ;
#35073 = CARTESIAN_POINT ( 'NONE',  ( -0.3458507752293909498, 0.3458507752293908388, -1.122047244094488194 ) ) ;
#35074 = CARTESIAN_POINT ( 'NONE',  ( 0.3917322834645670659, -0.1049643490035303273, -1.525609866962941430 ) ) ;
#35075 = CARTESIAN_POINT ( 'NONE',  ( 0.8267716535433078384, -0.6692913385826771977, 8.415575281601705876E-17 ) ) ;
#35076 = CARTESIAN_POINT ( 'NONE',  ( 0.2493438320209980519, -0.4281496062992127816, -0.4176697321401328100 ) ) ;
#35077 = CARTESIAN_POINT ( 'NONE',  ( -0.8661417322834640276, -0.1870078740157479769, 0.4822834645669291653 ) ) ;
#35078 = CARTESIAN_POINT ( 'NONE',  ( 1.135170603674541256, 0.2952755905511811885, 0.1292274648535926551 ) ) ;
#35079 = CARTESIAN_POINT ( 'NONE',  ( 0.7939632545931766261, -0.3162353388693409650, -0.4822834645669289433 ) ) ;
#35080 = CARTESIAN_POINT ( 'NONE',  ( 0.1958661417322836440, -0.3392501089628017219, -1.121391076115485719 ) ) ;
#35081 = CARTESIAN_POINT ( 'NONE',  ( -0.4133858267716528645, 0.1660481256975883668, -0.3530559997133364547 ) ) ;
#35082 = CARTESIAN_POINT ( 'NONE',  ( 0.7414698162729663755, 0.2952755905511811885, 0.1292274648535926551 ) ) ;
#35083 = CARTESIAN_POINT ( 'NONE',  ( 0.006561679790026889343, -0.3162353388693409650, -0.4822834645669289433 ) ) ;
#35084 = CARTESIAN_POINT ( 'NONE',  ( 0.6692913385826778638, -0.5511811023622047445, 6.969142054262312111E-17 ) ) ;
#35085 = CARTESIAN_POINT ( 'NONE',  ( -1.410761154855642463, -0.05778040916215522460, 0.4822834645669289988 ) ) ;
#35086 = CARTESIAN_POINT ( 'NONE',  ( -0.1654213697349098400, 1.092461187568469994, -2.846822072454109787 ) ) ;
#35087 = CARTESIAN_POINT ( 'NONE',  ( 0.1246719160104994284, -0.6692913385826771977, 0.1292274648535927661 ) ) ;
#35088 = DIRECTION ( 'NONE',  ( 0.000000000000000000, 0.000000000000000000, -1.000000000000000000 ) ) ;
#35089 = CARTESIAN_POINT ( 'NONE',  ( 0.3392501089628018329, 0.1958661417322835607, -2.328083989501312345 ) ) ;
#35090 = ORIENTED_EDGE ( 'NONE', *, *, #82011, .T. ) ;
#35091 = ORIENTED_EDGE ( 'NONE', *, *, #51971, .T. ) ;
#35092 = CARTESIAN_POINT ( 'NONE',  ( 0.9908136482939640111, -0.6692913385826771977, 0.1292274648535927661 ) ) ;
#35093 = CARTESIAN_POINT ( 'NONE',  ( 0.6102362204724416372, -0.4536011799217367080, 0.2665933059059888421 ) ) ;
#35095 = DIRECTION ( 'NONE',  ( -3.491481338843132961E-15, -0.000000000000000000, 1.000000000000000000 ) ) ;
#35094 = FACE_OUTER_BOUND ( 'NONE', #82702, .T. ) ;
#35096 = CARTESIAN_POINT ( 'NONE',  ( -0.4744094488189107839, 1.569370081724417609, 3.908320185825790993 ) ) ;
#35097 = CARTESIAN_POINT ( 'NONE',  ( 0.1181102362204724254, 8.537024980200824098E-18, 0.000000000000000000 ) ) ;
#35098 = CARTESIAN_POINT ( 'NONE',  ( -0.3392501089628017219, -0.1958661417322836718, -1.396981627296587813 ) ) ;
#35099 = CARTESIAN_POINT ( 'NONE',  ( 0.1998031496062992463, 0.3460692066303959202, -2.425853018372703396 ) ) ;
#35100 = CARTESIAN_POINT ( 'NONE',  ( -0.9908136482939626788, 0.2952755905511811885, 0.1292274648535926551 ) ) ;
#35101 = CARTESIAN_POINT ( 'NONE',  ( -0.6758530183727028406, -0.6692913385826773087, -0.1292274648535924053 ) ) ;
#35102 = CARTESIAN_POINT ( 'NONE',  ( 0.6167979002624678353, -0.4281496062992124485, 0.4176697321401328655 ) ) ;
#35103 = ORIENTED_EDGE ( 'NONE', *, *, #50636, .T. ) ;
#35104 = VECTOR ( 'NONE', #65113, 39.37007874015748143 ) ;
#35105 = CARTESIAN_POINT ( 'NONE',  ( 1.384514435695538337, -0.6692913385826771977, 0.1292274648535927661 ) ) ;
#35106 = FACE_OUTER_BOUND ( 'NONE', #54822, .T. ) ;
#35107 = B_SPLINE_CURVE_WITH_KNOTS ( 'NONE', 3,
 ( #23405, #74357, #16701, #36042, #42755, #42341, #75182, #68039, #55382, #49072 ),
 .UNSPECIFIED., .F., .F.,
 ( 4, 2, 2, 2, 4 ),
 ( 1.301042606982605321E-18, 0.0007778963758021327198, 0.001555792751604264139, 0.002333689127406395666, 0.003111585503208526976 ),
 .UNSPECIFIED. ) ;
#35108 = CARTESIAN_POINT ( 'NONE',  ( 1.614173228346457378, -0.5511811023622047445, 6.969142054262312111E-17 ) ) ;
#35109 = CARTESIAN_POINT ( 'NONE',  ( -0.3996062992125986035, 0.1070741851644051584, -2.156824146981627166 ) ) ;
#35110 = CARTESIAN_POINT ( 'NONE',  ( -1.541994750656167090, -0.5511811023622048555, -0.09757992244046775898 ) ) ;
#35111 = CARTESIAN_POINT ( 'NONE',  ( 0.3307086614173228023, -0.3647102339900947787, 0.000000000000000000 ) ) ;
#35112 = CARTESIAN_POINT ( 'NONE',  ( 0.1443569553805781891, 0.05413385826771626580, -0.4176697321401330321 ) ) ;
#35114 = DIRECTION ( 'NONE',  ( -0.000000000000000000, 0.000000000000000000, -1.000000000000000000 ) ) ;
#35113 = CARTESIAN_POINT ( 'NONE',  ( 1.594488188976378673, -0.5400638737290845981, -0.3530559997133363437 ) ) ;
#35115 = CARTESIAN_POINT ( 'NONE',  ( -1.122047244094487306, -0.4536011799217367080, 0.2665933059059888421 ) ) ;
#35116 = CARTESIAN_POINT ( 'NONE',  ( 0.9055118110236227702, 0.2952755905511811885, 0.000000000000000000 ) ) ;
#35117 = CARTESIAN_POINT ( 'NONE',  ( 1.213910761154856299, -0.5511811023622048555, -0.09757992244046775898 ) ) ;
#35118 = CARTESIAN_POINT ( 'NONE',  ( -0.3917322834645668994, -0.1049643490035306742, -1.228327140911074089 ) ) ;
#35119 = CARTESIAN_POINT ( 'NONE',  ( -1.417322834645668772, -0.1870078740157479769, 0.3641732283464567677 ) ) ;
#35120 = CARTESIAN_POINT ( 'NONE',  ( 1.404199475065617708, 0.05413385826771626580, -0.4176697321401330321 ) ) ;
#35121 = CARTESIAN_POINT ( 'NONE',  ( 2.554860351194764956, 1.554815631980118074, -0.4741686481756392513 ) ) ;
#35122 = CARTESIAN_POINT ( 'NONE',  ( -0.1837270341207343505, -0.6046776061558807314, 0.2411417322834647770 ) ) ;
#35123 = CARTESIAN_POINT ( 'NONE',  ( -1.312335958005248715, 0.1283753931104748280, 0.1820866141732283561 ) ) ;
#35124 = CARTESIAN_POINT ( 'NONE',  ( -0.3149606299212590610, -0.1870078740157479769, 0.3641732283464567677 ) ) ;
#35125 = CIRCLE ( 'NONE', #68706, 0.2165354330708659791 ) ;
#35126 = EDGE_CURVE ( 'NONE', #54019, #66895, #1590, .T. ) ;
#35127 = CARTESIAN_POINT ( 'NONE',  ( -0.2755905511811018171, 0.2952755905511811885, 0.000000000000000000 ) ) ;
#35128 = CARTESIAN_POINT ( 'NONE',  ( -1.476377952755905110, 0.07958543189024085140, 0.2665933059059887866 ) ) ;
#35129 = CARTESIAN_POINT ( 'NONE',  ( -0.1049643490035307158, 0.3917322834645670104, -0.3182607855981121059 ) ) ;
#35130 = CARTESIAN_POINT ( 'NONE',  ( 0.2624671916010504757, -0.6046776061558809534, -0.2411417322834644161 ) ) ;
#35131 = EDGE_CURVE ( 'NONE', #24616, #66982, #78196, .T. ) ;
#35132 = CARTESIAN_POINT ( 'NONE',  ( -1.646051170424378096, 0.000000000000000000, -0.3464511005275205946 ) ) ;
#35133 = CARTESIAN_POINT ( 'NONE',  ( 0.4724409448818896462, 0.1265901696524990294, -1.776246719160104570 ) ) ;
#35134 = CARTESIAN_POINT ( 'NONE',  ( -1.279527559055116948, -0.5400638737290844871, 0.3530559997133364547 ) ) ;
#35135 = CARTESIAN_POINT ( 'NONE',  ( -0.5905511811023615998, 0.1771653543307087630, 0.000000000000000000 ) ) ;
#35136 = CARTESIAN_POINT ( 'NONE',  ( -1.555118110236219930, -0.5400638737290845981, -0.3530559997133363437 ) ) ;
#35137 = CARTESIAN_POINT ( 'NONE',  ( 0.1706036745406830368, -0.4281496062992127816, -0.4176697321401328100 ) ) ;
#35138 = CARTESIAN_POINT ( 'NONE',  ( 0.5577427821522316087, -0.08942795157527998196, 0.3641732283464567121 ) ) ;
#35139 = CARTESIAN_POINT ( 'NONE',  ( -0.8530183727034112984, -0.3690944881889765550, -0.3153832671262227771 ) ) ;
#35140 = CARTESIAN_POINT ( 'NONE',  ( -1.069553805774277722, 0.2952755905511811885, 0.1292274648535926551 ) ) ;
#35141 = CARTESIAN_POINT ( 'NONE',  ( -1.417322834645668772, -0.1870078740157479769, 0.4822834645669291653 ) ) ;
#35142 = CARTESIAN_POINT ( 'NONE',  ( 1.417322834645670104, -0.1870078740157480879, -0.4822834645669291653 ) ) ;
#35143 = CARTESIAN_POINT ( 'NONE',  ( 0.4177787735907000921, 0.000000000000000000, -1.244210979442979648 ) ) ;
#35144 = CARTESIAN_POINT ( 'NONE',  ( 0.8595800524934390507, -0.2845877964562159024, 0.3641732283464567677 ) ) ;
#35145 = CARTESIAN_POINT ( 'NONE',  ( 0.8989501312335964611, 0.2952755905511811885, 0.1292274648535926551 ) ) ;
#35146 = FACE_OUTER_BOUND ( 'NONE', #23960, .T. ) ;
#35147 = CARTESIAN_POINT ( 'NONE',  ( 1.312335958005249825, 0.1283753931104746893, -0.1820866141732285504 ) ) ;
#35148 = ORIENTED_EDGE ( 'NONE', *, *, #14394, .F. ) ;
#35149 = CARTESIAN_POINT ( 'NONE',  ( -0.7677165354330699465, -0.5400638737290845981, -0.3530559997133363437 ) ) ;
#35150 = B_SPLINE_CURVE_WITH_KNOTS ( 'NONE', 3,
 ( #68881, #48688, #43597, #10412 ),
 .UNSPECIFIED., .F., .F.,
 ( 4, 4 ),
 ( 3.593986969189856797E-07, 0.001287825409103300319 ),
 .UNSPECIFIED. ) ;
#35151 = CARTESIAN_POINT ( 'NONE',  ( -0.1070741851644051862, -0.3996062992125986590, -2.668635170603674833 ) ) ;
#35152 = EDGE_CURVE ( 'NONE', #49144, #79206, #76447, .T. ) ;
#35153 = CARTESIAN_POINT ( 'NONE',  ( -1.384514435695537005, -0.5511811023622048555, -0.09757992244046775898 ) ) ;
#35154 = CARTESIAN_POINT ( 'NONE',  ( -0.7742782152230962556, -0.4281496062992127816, -0.4176697321401328100 ) ) ;
#35155 = CARTESIAN_POINT ( 'NONE',  ( 0.5118110236220478892, 0.2952755905511811885, 0.000000000000000000 ) ) ;
#35156 = CARTESIAN_POINT ( 'NONE',  ( -1.541994750656167090, 0.1771653543307087630, 0.09757992244046791164 ) ) ;
#35157 = CARTESIAN_POINT ( 'NONE',  ( -0.2925321140481930149, -0.2925321140481933480, -2.340551181102362488 ) ) ;
#35158 = CARTESIAN_POINT ( 'NONE',  ( -1.535433070866141225, 0.2952755905511811885, 0.000000000000000000 ) ) ;
#35159 = CARTESIAN_POINT ( 'NONE',  ( 0.5446194225721792126, -0.3162353388693405765, 0.4822834645669290543 ) ) ;
#35160 = CARTESIAN_POINT ( 'NONE',  ( -0.03280839895013062252, 0.2952755905511810774, -0.1292274648535930714 ) ) ;
#35161 = CARTESIAN_POINT ( 'NONE',  ( 0.8595800524934390507, -0.05778040916215560624, -0.4822834645669293319 ) ) ;
#35162 = CARTESIAN_POINT ( 'NONE',  ( -0.2925321140481932924, 0.2925321140481931814, -1.909448818897637512 ) ) ;
#35163 = CARTESIAN_POINT ( 'NONE',  ( -0.1058382717557503211, 0.3949938075777409408, -0.9514435695538059345 ) ) ;
#35164 = CARTESIAN_POINT ( 'NONE',  ( 0.3460692066303959202, 0.1998031496062993295, -2.493438320209973469 ) ) ;
#35165 = CARTESIAN_POINT ( 'NONE',  ( -0.9548908091195642545, -2.567464376874931580E-15, -0.4445507791589072832 ) ) ;
#35166 = CARTESIAN_POINT ( 'NONE',  ( 0.1958661417322836440, -0.3392501089628017219, -0.08398950131233590133 ) ) ;
#35167 = CARTESIAN_POINT ( 'NONE',  ( -0.1443569553805768291, -0.004921259842519576551, 0.3153832671262227771 ) ) ;
#35168 = CARTESIAN_POINT ( 'NONE',  ( -0.4461942257217840213, 0.2306618581243848609, 0.2411417322834645549 ) ) ;
#35169 = CARTESIAN_POINT ( 'NONE',  ( 0.7020997375328090762, -0.05778040916215560624, -0.4822834645669293319 ) ) ;
#35170 = CARTESIAN_POINT ( 'NONE',  ( 0.1974969037888704704, 0.3420746716998660508, -1.953412073490814027 ) ) ;
#35171 = CARTESIAN_POINT ( 'NONE',  ( 0.05249343832021075018, -0.5023911411419708095, 0.1820866141732285504 ) ) ;
#35172 = CARTESIAN_POINT ( 'NONE',  ( -1.292650918635170010, 0.2952755905511810774, -0.1292274648535930714 ) ) ;
#35173 = CARTESIAN_POINT ( 'NONE',  ( 1.154855643044620184, 0.2306618581243847221, -0.2411417322834647770 ) ) ;
#35174 = CARTESIAN_POINT ( 'NONE',  ( 0.4724409448818897572, -0.1265901696524988906, -2.316272965879265122 ) ) ;
#35175 = CARTESIAN_POINT ( 'NONE',  ( -0.1070741851644051862, -0.3996062992125987146, -1.804461942257217677 ) ) ;
#35176 = CARTESIAN_POINT ( 'NONE',  ( -0.2017716535433071445, -0.2017716535433071445, 0.000000000000000000 ) ) ;
#35177 = ORIENTED_EDGE ( 'NONE', *, *, #24957, .F. ) ;
#35178 = ORIENTED_EDGE ( 'NONE', *, *, #67069, .F. ) ;
#35179 = CARTESIAN_POINT ( 'NONE',  ( 1.049868766404200127, -0.6046776061558809534, -0.2411417322834644161 ) ) ;
#35180 = CARTESIAN_POINT ( 'NONE',  ( -1.732283464566928277, -0.1870078740157479769, 0.4822834645669291653 ) ) ;
#35182 = CARTESIAN_POINT ( 'NONE',  ( -1.227034120734907141, -0.6692913385826773087, -0.1292274648535924053 ) ) ;
#35181 = CARTESIAN_POINT ( 'NONE',  ( -1.069553805774277722, -0.5511811023622048555, -0.09757992244046775898 ) ) ;
#35183 = CARTESIAN_POINT ( 'NONE',  ( 4.797336870675655290E-17, -0.3917322834645669549, -2.835938689467505380 ) ) ;
#35184 = CARTESIAN_POINT ( 'NONE',  ( -0.9842519685039360366, 0.2066929133858268208, 0.000000000000000000 ) ) ;
#35185 = CARTESIAN_POINT ( 'NONE',  ( 1.089238845144357759, 0.05413385826771626580, -0.4176697321401330321 ) ) ;
#35186 = DIRECTION ( 'NONE',  ( 0.000000000000000000, 1.000000000000000000, 0.000000000000000000 ) ) ;
#35187 = CARTESIAN_POINT ( 'NONE',  ( 0.05249343832021075018, 0.2306618581243847221, -0.2411417322834647770 ) ) ;
#35188 = CARTESIAN_POINT ( 'NONE',  ( -0.5708661417322828946, 0.1660481256975883668, -0.3530559997133364547 ) ) ;
#35189 = CARTESIAN_POINT ( 'NONE',  ( 1.581364829396326277, -0.05778040916215522460, 0.4822834645669289988 ) ) ;
#35190 = CARTESIAN_POINT ( 'NONE',  ( 0.3392501089628018884, -0.1958661417322834220, -0.1896325459317586282 ) ) ;
#35191 = CARTESIAN_POINT ( 'NONE',  ( 0.2427821522309716595, -0.3162353388693409650, -0.4822834645669289433 ) ) ;
#35192 = CARTESIAN_POINT ( 'NONE',  ( 0.3392501089628018884, -0.1958661417322834220, -2.144356955380577467 ) ) ;
#35193 = CARTESIAN_POINT ( 'NONE',  ( -1.430446194225720724, -0.004921259842519870586, -0.3153832671262229437 ) ) ;
#35194 = ORIENTED_EDGE ( 'NONE', *, *, #32413, .T. ) ;
#35195 = CARTESIAN_POINT ( 'NONE',  ( 0.2891555358219910499, -0.2891555358219909944, -2.303149606299212504 ) ) ;
#35196 = VERTEX_POINT ( 'NONE', #65876 ) ;
#35197 = CARTESIAN_POINT ( 'NONE',  ( -1.542758472124253988, 1.384765482578574902, 0.4491926697227655585 ) ) ;
#35198 = CARTESIAN_POINT ( 'NONE',  ( -1.581364829396324945, -0.3162353388693405765, 0.4822834645669290543 ) ) ;
#35199 = CARTESIAN_POINT ( 'NONE',  ( 0.1998031496062994405, -0.3460692066303958092, -1.036745406824147064 ) ) ;
#35200 = CARTESIAN_POINT ( 'NONE',  ( -1.699475065616797398, 0.2952755905511811885, 0.1292274648535926551 ) ) ;
#35201 = CARTESIAN_POINT ( 'NONE',  ( -1.587926509186350810, -0.4281496062992124485, 0.4176697321401328655 ) ) ;
#35202 = CARTESIAN_POINT ( 'NONE',  ( -0.9580052493438311334, 0.05413385826771626580, -0.4176697321401330321 ) ) ;
#35203 = LINE ( 'NONE', #48235, #32384 ) ;
#35204 = CARTESIAN_POINT ( 'NONE',  ( -0.1049643490035307020, 0.3917322834645669549, -0.09120734908136493568 ) ) ;
#35205 = CARTESIAN_POINT ( 'NONE',  ( -0.4724409448818890911, -0.1870078740157480601, -0.3641732283464567677 ) ) ;
#35206 = CARTESIAN_POINT ( 'NONE',  ( -0.7874015748031489847, -0.1870078740157479769, 0.3641732283464567677 ) ) ;
#35207 = CARTESIAN_POINT ( 'NONE',  ( -1.115485564304461219, 0.05413385826771626580, -0.4176697321401330321 ) ) ;
#35208 = CARTESIAN_POINT ( 'NONE',  ( 0.4986876640419954376, 0.2306618581243848609, 0.2411417322834645549 ) ) ;
#35209 = CARTESIAN_POINT ( 'NONE',  ( -1.003937007874014853, 0.1660481256975885056, 0.3530559997133364547 ) ) ;
#35210 = CARTESIAN_POINT ( 'NONE',  ( 0.5314960629921396951, 2.697992270790283698, -3.898836503597931991 ) ) ;
#35211 = VERTEX_POINT ( 'NONE', #70936 ) ;
#35212 = CARTESIAN_POINT ( 'NONE',  ( -1.423884514435694859, -0.05778040916215560624, -0.4822834645669293319 ) ) ;
#35213 = CARTESIAN_POINT ( 'NONE',  ( 0.000000000000000000, 2.677165354330708791, 0.000000000000000000 ) ) ;
#35214 = CARTESIAN_POINT ( 'NONE',  ( 0.4091458600556403535, 0.2362204724409449896, -1.863517060367454015 ) ) ;
#35215 = EDGE_CURVE ( 'NONE', #10037, #80676, #45236, .T. ) ;
#35216 = CARTESIAN_POINT ( 'NONE',  ( -1.614173228346457378, 1.055049524192299693, -0.1372047244094477536 ) ) ;
#35217 = CARTESIAN_POINT ( 'NONE',  ( -0.2867679344610365999, 0.2867679344610364889, -0.6417322834645668994 ) ) ;
#35218 = CARTESIAN_POINT ( 'NONE',  ( -9.594673741351313045E-17, 0.3917322834645670104, -2.604330708661416693 ) ) ;
#35219 = CARTESIAN_POINT ( 'NONE',  ( -0.8398950131233585692, 0.2306618581243848609, 0.2411417322834645549 ) ) ;
#35220 = CARTESIAN_POINT ( 'NONE',  ( 1.240157480314961314, 0.1660481256975883668, -0.3530559997133364547 ) ) ;
#35221 = CARTESIAN_POINT ( 'NONE',  ( -0.3996062992125985480, -7.340648628747423112E-17, -0.5885826771653542844 ) ) ;
#35223 = CARTESIAN_POINT ( 'NONE',  ( -0.6889763779527551257, 0.1012011053420777407, 0.2882089793578256898 ) ) ;
#35222 = CARTESIAN_POINT ( 'NONE',  ( 1.948818897637795367, 0.000000000000000000, 5.701968306260621233 ) ) ;
#35224 = CARTESIAN_POINT ( 'NONE',  ( -1.476377952755905110, -0.5400638737290845981, -0.3530559997133363437 ) ) ;
#35225 = CARTESIAN_POINT ( 'NONE',  ( -0.6496062992125976043, -0.5400638737290844871, 0.3530559997133364547 ) ) ;
#35226 = CARTESIAN_POINT ( 'NONE',  ( -0.2867679344610364334, -0.2867679344610368219, -0.1390882957667173292 ) ) ;
#35227 = CARTESIAN_POINT ( 'NONE',  ( 0.3018372703412079971, -0.3690944881889763329, 0.3153832671262228327 ) ) ;
#35228 = CARTESIAN_POINT ( 'NONE',  ( -0.1049643490035301885, -0.3917322834645671215, -0.3143044619422573072 ) ) ;
#35229 = CARTESIAN_POINT ( 'NONE',  ( 0.1312335958005257930, 0.1283753931104746893, -0.1820866141732285504 ) ) ;
#35230 = CARTESIAN_POINT ( 'NONE',  ( 1.036745406824147508, -0.3690944881889765550, -0.3153832671262227771 ) ) ;
#35231 = CARTESIAN_POINT ( 'NONE',  ( 1.102362204724410155, -0.1870078740157479769, 0.4822834645669291653 ) ) ;
#35232 = VECTOR ( 'NONE', #19404, 39.37007874015748854 ) ;
#35233 = CARTESIAN_POINT ( 'NONE',  ( -0.2755905511811015396, -0.5511811023622047445, 6.969142054262312111E-17 ) ) ;
#35234 = CARTESIAN_POINT ( 'NONE',  ( 0.2867679344610365999, 0.2867679344610365999, -2.177165354330708347 ) ) ;
#35235 = CARTESIAN_POINT ( 'NONE',  ( 1.509186351706037543, -0.4281496062992127816, -0.4176697321401328100 ) ) ;
#35236 = CARTESIAN_POINT ( 'NONE',  ( -1.391076115485563314, -0.5023911411419708095, -0.1820866141732282451 ) ) ;
#35237 = CARTESIAN_POINT ( 'NONE',  ( 0.1265901696524989462, 0.4724409448818897572, -0.2276902887139107545 ) ) ;
#35238 = B_SPLINE_CURVE_WITH_KNOTS ( 'NONE', 3,
 ( #69516, #11865, #18986, #37518 ),
 .UNSPECIFIED., .F., .F.,
 ( 4, 4 ),
 ( 2.857347768987377627E-07, 0.001436604392377181273 ),
 .UNSPECIFIED. ) ;
#35239 = CARTESIAN_POINT ( 'NONE',  ( 0.05905511811023709395, -0.5400638737290844871, 0.3530559997133364547 ) ) ;
#35240 = CARTESIAN_POINT ( 'NONE',  ( 1.541994750656168645, 0.1771653543307087075, -0.09757992244046823083 ) ) ;
#35241 = CARTESIAN_POINT ( 'NONE',  ( 0.3543307086614179147, 0.1771653543307087630, 0.000000000000000000 ) ) ;
#35242 = CARTESIAN_POINT ( 'NONE',  ( -0.3543307086614165824, -0.5511811023622047445, 6.969142054262312111E-17 ) ) ;
#35243 = CARTESIAN_POINT ( 'NONE',  ( -0.9317585301837263412, -0.4281496062992127816, -0.4176697321401328100 ) ) ;
#35244 = DIRECTION ( 'NONE',  ( -1.000000000000000000, -3.469446951953613696E-16, 0.000000000000000000 ) ) ;
#35245 = LINE ( 'NONE', #3261, #50197 ) ;
#35246 = CARTESIAN_POINT ( 'NONE',  ( 0.1246719160104994284, 0.2952755905511810774, -0.1292274648535930714 ) ) ;
#35247 = ORIENTED_EDGE ( 'NONE', *, *, #20205, .F. ) ;
#35248 = CARTESIAN_POINT ( 'NONE',  ( 0.2925321140481932369, -0.2925321140481931814, -1.750000000000000222 ) ) ;
#35249 = CARTESIAN_POINT ( 'NONE',  ( 0.3049517105654749871, 8.471767977567108961E-16, -0.4445507791589058955 ) ) ;
#35250 = CARTESIAN_POINT ( 'NONE',  ( -0.4133858267716528645, 0.07958543189024071263, -0.2665933059059888421 ) ) ;
#35251 = CARTESIAN_POINT ( 'NONE',  ( -0.2624671916010490880, 0.2306618581243847221, -0.2411417322834647770 ) ) ;
#35252 = CARTESIAN_POINT ( 'NONE',  ( -1.345144356955379816, -0.3162353388693405765, 0.4822834645669290543 ) ) ;
#35253 = CARTESIAN_POINT ( 'NONE',  ( -1.541994750656167090, -0.5511811023622048555, -0.09757992244046775898 ) ) ;
#35254 = CARTESIAN_POINT ( 'NONE',  ( 1.476377952755906442, -0.5400638737290844871, 0.3530559997133364547 ) ) ;
#35255 = CARTESIAN_POINT ( 'NONE',  ( -1.286089238845143479, 0.2306618581243847221, -0.2411417322834647770 ) ) ;
#35256 = CARTESIAN_POINT ( 'NONE',  ( -0.7283464566929126471, 0.07958543189024071263, -0.2665933059059888421 ) ) ;
#35257 = CARTESIAN_POINT ( 'NONE',  ( 0.3996062992125985480, 2.446882876249141654E-17, -0.1948818897637795700 ) ) ;
#35258 = CARTESIAN_POINT ( 'NONE',  ( 0.1998031496062992740, 0.3460692066303959757, -0.4593175853018372501 ) ) ;
#35259 = CARTESIAN_POINT ( 'NONE',  ( -9.594673741351313045E-17, 0.3917322834645670659, -2.831384145178164058 ) ) ;
#35260 = DIRECTION ( 'NONE',  ( -1.000000000000000000, -3.096699300667737957E-16, 1.692413147294446216E-16 ) ) ;
#35261 = CARTESIAN_POINT ( 'NONE',  ( 1.187664041994751285, -0.2845877964562161244, -0.3641732283464567121 ) ) ;
#35262 = CARTESIAN_POINT ( 'NONE',  ( -1.535433070866141225, 0.2952755905511811885, 0.000000000000000000 ) ) ;
#35263 = CARTESIAN_POINT ( 'NONE',  ( 0.7677165354330716118, -0.5400638737290844871, 0.3530559997133364547 ) ) ;
#35264 = CARTESIAN_POINT ( 'NONE',  ( -0.3420746716998660508, -0.1974969037888706924, -0.9166666666666668517 ) ) ;
#35265 = CARTESIAN_POINT ( 'NONE',  ( 1.292650918635171564, -0.5511811023622048555, -0.09757992244046775898 ) ) ;
#35266 = CARTESIAN_POINT ( 'NONE',  ( 0.2230971128608932319, -0.4281496062992124485, 0.4176697321401328655 ) ) ;
#35267 = CARTESIAN_POINT ( 'NONE',  ( -0.7020997375328074108, -0.05778040916215522460, 0.4822834645669289988 ) ) ;
#35268 = CARTESIAN_POINT ( 'NONE',  ( -3.908420089088291416, 1.569603073218160061, 0.4735885527812596085 ) ) ;
#35269 = CARTESIAN_POINT ( 'NONE',  ( 0.4724409448818896462, 0.1265901696524990294, -0.9120734908136483021 ) ) ;
#35270 = CARTESIAN_POINT ( 'NONE',  ( 0.3996062992125985480, 0.1070741851644054637, -2.329396325459317296 ) ) ;
#35271 = CARTESIAN_POINT ( 'NONE',  ( 0.3608923884514443348, 0.1771653543307087075, -0.09757992244046823083 ) ) ;
#35272 = EDGE_CURVE ( 'NONE', #21828, #42415, #13029, .T. ) ;
#35273 = ORIENTED_EDGE ( 'NONE', *, *, #76425, .T. ) ;
#35274 = CARTESIAN_POINT ( 'NONE',  ( 0.1958661417322836718, -0.3392501089628017219, -0.2460823079078234277 ) ) ;
#35275 = ORIENTED_EDGE ( 'NONE', *, *, #79779, .F. ) ;
#35276 = CARTESIAN_POINT ( 'NONE',  ( -0.5249343832020990641, -0.6046776061558809534, -0.2411417322834644161 ) ) ;
#35277 = PRODUCT_DEFINITION_SHAPE ( 'NONE', 'NONE',  #83318 ) ;
#35278 = CARTESIAN_POINT ( 'NONE',  ( -0.1837270341207340729, 0.2306618581243847221, -0.2411417322834647770 ) ) ;
#35279 = CARTESIAN_POINT ( 'NONE',  ( -0.4790026246719152336, -0.08942795157528024563, -0.3641732283464568787 ) ) ;
#35280 = CARTESIAN_POINT ( 'NONE',  ( 0.7086614173228353852, -0.1870078740157479769, 0.4822834645669291653 ) ) ;
#35281 = EDGE_CURVE ( 'NONE', #61268, #49328, #53216, .T. ) ;
#35282 = CARTESIAN_POINT ( 'NONE',  ( -0.7283464566929126471, -0.5400638737290844871, 0.3530559997133364547 ) ) ;
#35283 = CARTESIAN_POINT ( 'NONE',  ( -0.2296587926509179312, -0.3162353388693409650, -0.4822834645669289433 ) ) ;
#35284 = CARTESIAN_POINT ( 'NONE',  ( 1.207349081364829990, -0.6046776061558809534, -0.2411417322834644161 ) ) ;
#35285 = VECTOR ( 'NONE', #61126, 39.37007874015748143 ) ;
#35286 = CARTESIAN_POINT ( 'NONE',  ( 1.062992125984252745, -0.6692913385826771977, 8.415575281601705876E-17 ) ) ;
#35287 = CARTESIAN_POINT ( 'NONE',  ( 0.7086614173228353852, -0.1870078740157479769, 0.4822834645669291653 ) ) ;
#35288 = CARTESIAN_POINT ( 'NONE',  ( -0.3392501089628017219, -0.1958661417322836718, -0.5170603674540682482 ) ) ;
#35289 = CARTESIAN_POINT ( 'NONE',  ( -0.1509186351706028884, -0.2845877964562161244, -0.3641732283464567121 ) ) ;
#35290 = ORIENTED_EDGE ( 'NONE', *, *, #16168, .T. ) ;
#35291 = CARTESIAN_POINT ( 'NONE',  ( -0.1974969037888703871, -0.3420746716998661063, -0.8530183727034120755 ) ) ;
#35292 = ORIENTED_EDGE ( 'NONE', *, *, #79015, .T. ) ;
#35293 = CARTESIAN_POINT ( 'NONE',  ( -1.062992125984250968, 0.1771653543307087630, 0.000000000000000000 ) ) ;
#35294 = CARTESIAN_POINT ( 'NONE',  ( -0.5511811023622038563, -0.1870078740157479769, 0.4822834645669291653 ) ) ;
#35295 = CARTESIAN_POINT ( 'NONE',  ( 0.000000000000000000, 2.559055118110236560, 0.000000000000000000 ) ) ;
#35296 = CARTESIAN_POINT ( 'NONE',  ( -0.2230971128608915943, -0.4281496062992127816, -0.4176697321401328100 ) ) ;
#35297 = CARTESIAN_POINT ( 'NONE',  ( -0.6102362204724400829, 0.1660481256975885056, 0.3530559997133364547 ) ) ;
#35298 = CARTESIAN_POINT ( 'NONE',  ( -1.089238845144356427, -0.4281496062992127816, -0.4176697321401328100 ) ) ;
#35299 = CARTESIAN_POINT ( 'NONE',  ( -1.299212598425196097, -0.6692913385826771977, 8.415575281601705876E-17 ) ) ;
#35300 = CARTESIAN_POINT ( 'NONE',  ( 1.030183727034121421, -0.08942795157527998196, 0.3641732283464567121 ) ) ;
#35301 = DIRECTION ( 'NONE',  ( -0.000000000000000000, -1.000000000000000000, -0.000000000000000000 ) ) ;
#35302 = CARTESIAN_POINT ( 'NONE',  ( 0.2843957880255121862, 0.07959014333740671576, 5.860354325783368346 ) ) ;
#35303 = CARTESIAN_POINT ( 'NONE',  ( 0.3937007874015754361, -0.1870078740157480601, -0.3641732283464567677 ) ) ;
#35304 = CARTESIAN_POINT ( 'NONE',  ( -0.02624671916010428221, 0.2306618581243847221, -0.2411417322834647770 ) ) ;
#35305 = CARTESIAN_POINT ( 'NONE',  ( 0.4921259842519691285, -0.5400638737290845981, -0.3530559997133363437 ) ) ;
#35306 = VERTEX_POINT ( 'NONE', #58283 ) ;
#35307 = CARTESIAN_POINT ( 'NONE',  ( -9.787531504996567848E-17, 0.3996062992125986035, -1.889763779527559251 ) ) ;
#35308 = CARTESIAN_POINT ( 'NONE',  ( -0.6102362204724400829, 0.1660481256975885056, 0.3530559997133364547 ) ) ;
#35309 = ORIENTED_EDGE ( 'NONE', *, *, #15246, .T. ) ;
#35310 = CARTESIAN_POINT ( 'NONE',  ( 0.1998031496062992463, 0.3460692066303959202, -1.008530183727034180 ) ) ;
#35311 = CARTESIAN_POINT ( 'NONE',  ( -0.2925321140481932369, 0.2925321140481931259, -0.7263779527559056648 ) ) ;
#35312 = CARTESIAN_POINT ( 'NONE',  ( -0.7020997375328076329, -0.2845877964562161244, -0.3641732283464567121 ) ) ;
#35313 = CARTESIAN_POINT ( 'NONE',  ( -1.089238845144356427, 0.05413385826771666132, 0.4176697321401328100 ) ) ;
#35314 = CARTESIAN_POINT ( 'NONE',  ( 0.3996062992125986590, -0.1070741851644053111, -2.946194225721785465 ) ) ;
#35315 = CARTESIAN_POINT ( 'NONE',  ( -0.3917322834645669549, -0.1049643490035306603, -2.650262467191601079 ) ) ;
#35316 = CARTESIAN_POINT ( 'NONE',  ( 1.607611548556431069, -0.6692913385826773087, -0.1292274648535924053 ) ) ;
#35317 = CARTESIAN_POINT ( 'NONE',  ( 1.069553805774278610, -0.6692913385826771977, 0.1292274648535927661 ) ) ;
#35318 = CARTESIAN_POINT ( 'NONE',  ( 0.3083989501312343062, -0.05778040916215560624, -0.4822834645669293319 ) ) ;
#35319 = CARTESIAN_POINT ( 'NONE',  ( -0.6299212598425188991, -0.1870078740157480601, -0.3641732283464567677 ) ) ;
#35320 = CARTESIAN_POINT ( 'NONE',  ( 0.1246719160104994284, -0.6692913385826771977, 0.1292274648535927661 ) ) ;
#35321 = CARTESIAN_POINT ( 'NONE',  ( -0.1265901696524986964, -0.4724409448818899238, -1.881233595800524849 ) ) ;
#35322 = CARTESIAN_POINT ( 'NONE',  ( 0.03280839895013198948, -0.5511811023622048555, -0.09757992244046775898 ) ) ;
#35323 = CARTESIAN_POINT ( 'NONE',  ( -0.2559055118110230564, 0.1660481256975883668, -0.3530559997133364547 ) ) ;
#35324 = EDGE_CURVE ( 'NONE', #1754, #64485, #40193, .T. ) ;
#35325 = CARTESIAN_POINT ( 'NONE',  ( -0.2891555358219911054, 0.2891555358219909388, -1.828740157480315487 ) ) ;
#35326 = CARTESIAN_POINT ( 'NONE',  ( -1.614173228346456268, -0.6692913385826771977, 8.415575281601705876E-17 ) ) ;
#35327 = CARTESIAN_POINT ( 'NONE',  ( 0.006561679790026889343, -0.08942795157527998196, 0.3641732283464567121 ) ) ;
#35328 = CARTESIAN_POINT ( 'NONE',  ( 1.620734908136483465, -0.5511811023622046335, 0.09757992244046803654 ) ) ;
#35329 = CARTESIAN_POINT ( 'NONE',  ( -1.095800524934382292, -0.05778040916215522460, 0.4822834645669289988 ) ) ;
#35330 = CARTESIAN_POINT ( 'NONE',  ( -0.8398950131233585692, 0.1283753931104748280, 0.1820866141732283561 ) ) ;
#35331 = FACE_OUTER_BOUND ( 'NONE', #20445, .T. ) ;
#35332 = CARTESIAN_POINT ( 'NONE',  ( -0.9514435695538050464, -0.3162353388693405765, 0.4822834645669290543 ) ) ;
#35333 = CARTESIAN_POINT ( 'NONE',  ( -0.5511811023622038563, -0.1870078740157479769, 0.4822834645669291653 ) ) ;
#35334 = CARTESIAN_POINT ( 'NONE',  ( 0.2099737532808405305, -0.6046776061558807314, 0.2411417322834647770 ) ) ;
#35335 = CARTESIAN_POINT ( 'NONE',  ( -0.3392501089628019439, 0.1958661417322832554, -2.625964936186665266 ) ) ;
#35336 = CARTESIAN_POINT ( 'NONE',  ( 0.5314960629920852941, 2.729333734409945755, 3.881246834694722203 ) ) ;
#35337 = CARTESIAN_POINT ( 'NONE',  ( 0.3740157480314966754, -0.4536011799217367080, 0.2665933059059888421 ) ) ;
#35338 = CARTESIAN_POINT ( 'NONE',  ( 1.023622047244095112, -0.1870078740157480879, -0.4822834645669291653 ) ) ;
#35339 = B_SPLINE_CURVE_WITH_KNOTS ( 'NONE', 3,
 ( #6452, #63695, #44316, #44724, #77588, #38849, #39266 ),
 .UNSPECIFIED., .F., .F.,
 ( 4, 3, 4 ),
 ( 1.908195823574487804E-17, 0.001246232571205249445, 0.002492492258783241595 ),
 .UNSPECIFIED. ) ;
#35340 = CARTESIAN_POINT ( 'NONE',  ( -1.200787401574802349, 0.07958543189024071263, -0.2665933059059888421 ) ) ;
#35341 = CARTESIAN_POINT ( 'NONE',  ( 1.003937007874016407, -0.5400638737290844871, 0.3530559997133364547 ) ) ;
#35342 = CARTESIAN_POINT ( 'NONE',  ( -1.686351706036744558, 0.1771653543307087075, -0.09757992244046823083 ) ) ;
#35343 = AXIS2_PLACEMENT_3D ( 'NONE', #35213, #29309, #16285 ) ;
#35344 = CARTESIAN_POINT ( 'NONE',  ( -0.4921259842519677963, -0.5400638737290844871, 0.3530559997133364547 ) ) ;
#35345 = CARTESIAN_POINT ( 'NONE',  ( 0.2230971128608932319, -0.3690944881889763329, 0.3153832671262228327 ) ) ;
#35346 = PLANE ( 'NONE',  #27321 ) ;
#35347 = CARTESIAN_POINT ( 'NONE',  ( 0.7152230971128614723, -0.2845877964562161244, -0.3641732283464567121 ) ) ;
#35348 = CARTESIAN_POINT ( 'NONE',  ( -0.1443569553805765515, -0.4281496062992127816, -0.4176697321401328100 ) ) ;
#35349 = CARTESIAN_POINT ( 'NONE',  ( 0.3996062992125984925, 0.1070741851644054637, -0.3589238845144357426 ) ) ;
#35350 = CARTESIAN_POINT ( 'NONE',  ( -1.043307086614172707, 0.1660481256975883668, -0.3530559997133364547 ) ) ;
#35351 = CARTESIAN_POINT ( 'NONE',  ( 0.3917322834645670104, -0.1049643490035303411, -1.770997375328083656 ) ) ;
#35352 = CARTESIAN_POINT ( 'NONE',  ( 1.148293963254593653, 0.1771653543307087075, -0.09757992244046823083 ) ) ;
#35353 = CARTESIAN_POINT ( 'NONE',  ( 0.03280839895013198948, -0.6692913385826773087, -0.1292274648535924053 ) ) ;
#35354 = CARTESIAN_POINT ( 'NONE',  ( -0.2493438320209966919, -0.4281496062992124485, 0.4176697321401328655 ) ) ;
#35355 = CARTESIAN_POINT ( 'NONE',  ( -0.2887139107611542133, -0.5023911411419708095, -0.1820866141732282451 ) ) ;
#35356 = LINE ( 'NONE', #42477, #65598 ) ;
#35357 = CARTESIAN_POINT ( 'NONE',  ( -0.4330708661417315697, -0.5511811023622047445, 6.969142054262312111E-17 ) ) ;
#35358 = CARTESIAN_POINT ( 'NONE',  ( 0.3018372703412079971, 0.05413385826771626580, -0.4176697321401330321 ) ) ;
#35359 = CARTESIAN_POINT ( 'NONE',  ( -1.318897637795274802, -0.4536011799217368745, -0.2665933059059886201 ) ) ;
#35360 = CARTESIAN_POINT ( 'NONE',  ( 4.893765752498283308E-17, -0.3996062992125985480, -0.7854330708661416693 ) ) ;
#35361 = CARTESIAN_POINT ( 'NONE',  ( -1.181102362204723644, -0.1870078740157479769, 0.4822834645669291653 ) ) ;
#35362 = CYLINDRICAL_SURFACE ( 'NONE', #77028, 0.09842519685039351207 ) ;
#35363 = VERTEX_POINT ( 'NONE', #51964 ) ;
#35364 = CARTESIAN_POINT ( 'NONE',  ( -1.364829396325458521, 0.1283753931104746893, -0.1820866141732285504 ) ) ;
#35365 = CARTESIAN_POINT ( 'NONE',  ( -0.4527559055118102749, 0.1660481256975885056, 0.3530559997133364547 ) ) ;
#35366 = CARTESIAN_POINT ( 'NONE',  ( 0.2239781325220697450, 1.118900601684395202, 2.822659112694967831 ) ) ;
#35367 = CARTESIAN_POINT ( 'NONE',  ( -1.292650918635170010, 0.2952755905511810774, -0.1292274648535930714 ) ) ;
#35368 = CARTESIAN_POINT ( 'NONE',  ( 0.3917322834645670104, 2.398668435337828261E-17, -1.620078740157480324 ) ) ;
#35369 = DIRECTION ( 'NONE',  ( -0.000000000000000000, -1.000000000000000000, -0.000000000000000000 ) ) ;
#35370 = CARTESIAN_POINT ( 'NONE',  ( 1.397637795275591177, 0.1660481256975883668, -0.3530559997133364547 ) ) ;
#35371 = CARTESIAN_POINT ( 'NONE',  ( 1.003937007874016407, -0.5400638737290844871, 0.3530559997133364547 ) ) ;
#35372 = CARTESIAN_POINT ( 'NONE',  ( -0.1049643490035301885, -0.3917322834645671215, -2.741469816272965154 ) ) ;
#35373 = CARTESIAN_POINT ( 'NONE',  ( -0.7480314960629922405, 2.244094488188976388, 0.000000000000000000 ) ) ;
#35374 = CARTESIAN_POINT ( 'NONE',  ( -1.581364829396324945, -0.3162353388693405765, 0.4822834645669290543 ) ) ;
#35375 = EDGE_CURVE ( 'NONE', #17097, #3706, #33876, .T. ) ;
#35376 = CARTESIAN_POINT ( 'NONE',  ( -0.1070741851644051862, -0.3996062992125987146, -0.5446194225721783244 ) ) ;
#35377 = ORIENTED_EDGE ( 'NONE', *, *, #23429, .T. ) ;
#35378 = CARTESIAN_POINT ( 'NONE',  ( -0.5708661417322825615, -0.4536011799217367080, 0.2665933059059888421 ) ) ;
#35379 = CARTESIAN_POINT ( 'NONE',  ( 0.1049643490035303689, 0.3917322834645670104, -2.190288713910760521 ) ) ;
#35380 = VERTEX_POINT ( 'NONE', #59542 ) ;
#35381 = CARTESIAN_POINT ( 'NONE',  ( 0.8333333333333340365, 0.2952755905511810774, -0.1292274648535930714 ) ) ;
#35382 = CARTESIAN_POINT ( 'NONE',  ( -0.2952755905511804668, 0.1660481256975885056, 0.3530559997133364547 ) ) ;
#35383 = CARTESIAN_POINT ( 'NONE',  ( -1.154855643044618851, 0.2306618581243848609, 0.2411417322834645549 ) ) ;
#35384 = CARTESIAN_POINT ( 'NONE',  ( 1.502624671916010790, -0.05778040916215522460, 0.4822834645669289988 ) ) ;
#35385 = CARTESIAN_POINT ( 'NONE',  ( -1.371391076115484609, -0.5511811023622046335, 0.09757992244046803654 ) ) ;
#35386 = CARTESIAN_POINT ( 'NONE',  ( 0.008982673068357337198, 1.062992125984252523, -1.448165499020492186 ) ) ;
#35387 = CARTESIAN_POINT ( 'NONE',  ( 0.4396325459317593221, 0.2952755905511810774, -0.1292274648535930714 ) ) ;
#35388 = CARTESIAN_POINT ( 'NONE',  ( -0.9055118110236215490, -0.6692913385826771977, 8.415575281601705876E-17 ) ) ;
#35389 = CARTESIAN_POINT ( 'NONE',  ( -0.3917322834645670659, 0.1049643490035301607, -1.530164411252281420 ) ) ;
#35390 = CARTESIAN_POINT ( 'NONE',  ( -1.036745406824146176, -0.4281496062992124485, 0.4176697321401328655 ) ) ;
#35391 = CARTESIAN_POINT ( 'NONE',  ( 0.2248141966262373892, 1.118402650174323609, -2.823092204040328568 ) ) ;
#35392 = CARTESIAN_POINT ( 'NONE',  ( 1.115485564304462551, -0.4281496062992127816, -0.4176697321401328100 ) ) ;
#35393 = CARTESIAN_POINT ( 'NONE',  ( 1.437007874015748810, -0.4536011799217368745, -0.2665933059059886201 ) ) ;
#35394 = ORIENTED_EDGE ( 'NONE', *, *, #19351, .T. ) ;
#35395 = CARTESIAN_POINT ( 'NONE',  ( -0.2891555358219911054, 0.2891555358219909388, 0.1377952755905511306 ) ) ;
#35396 = CARTESIAN_POINT ( 'NONE',  ( -0.4527559055118102749, -0.5400638737290845981, -0.3530559997133363437 ) ) ;
#35397 = ORIENTED_EDGE ( 'NONE', *, *, #18824, .F. ) ;
#35398 = CARTESIAN_POINT ( 'NONE',  ( 0.4921259842519691285, 0.07958543189024085140, 0.2665933059059887866 ) ) ;
#35399 = CARTESIAN_POINT ( 'NONE',  ( -1.292650918635170010, -0.6692913385826771977, 0.1292274648535927661 ) ) ;
#35400 = CARTESIAN_POINT ( 'NONE',  ( 1.102362204724410155, -0.1870078740157479769, 0.4822834645669291653 ) ) ;
#35401 = CARTESIAN_POINT ( 'NONE',  ( 0.8858267716535438430, -0.5400638737290845981, -0.3530559997133363437 ) ) ;
#35402 = CARTESIAN_POINT ( 'NONE',  ( -0.3412073490813641308, -0.6046776061558807314, 0.2411417322834647770 ) ) ;
#35403 = CIRCLE ( 'NONE', #36700, 0.5118110236220471121 ) ;
#35404 = CARTESIAN_POINT ( 'NONE',  ( 0.1958661417322834775, 0.3392501089628018884, -1.400937950952442668 ) ) ;
#35405 = CARTESIAN_POINT ( 'NONE',  ( -0.8267716535433065062, 0.2952755905511811885, 0.000000000000000000 ) ) ;
#35406 = CARTESIAN_POINT ( 'NONE',  ( 0.1049643490035303689, 0.3917322834645670104, -2.282808398950130879 ) ) ;
#35407 = CARTESIAN_POINT ( 'NONE',  ( -1.666666666666665853, 0.05413385826771626580, -0.4176697321401330321 ) ) ;
#35408 = CARTESIAN_POINT ( 'NONE',  ( -0.8464566929133852113, 0.1660481256975885056, 0.3530559997133364547 ) ) ;
#35409 = CARTESIAN_POINT ( 'NONE',  ( 1.174540682414699111, -0.3162353388693405765, 0.4822834645669290543 ) ) ;
#35410 = CARTESIAN_POINT ( 'NONE',  ( 1.555118110236221041, 0.1660481256975883668, -0.3530559997133364547 ) ) ;
#35411 = CARTESIAN_POINT ( 'NONE',  ( -0.9842519685039365918, -0.6692913385826771977, 8.415575281601705876E-17 ) ) ;
#35412 = CARTESIAN_POINT ( 'NONE',  ( 0.3460692066303959202, -0.1998031496062991630, -0.02427821522309711946 ) ) ;
#35413 = CARTESIAN_POINT ( 'NONE',  ( 0.3805774278215230400, 0.05413385826771626580, -0.4176697321401330321 ) ) ;
#35414 = CARTESIAN_POINT ( 'NONE',  ( 0.3996062992125986035, 2.446882876249141962E-17, -1.850393700787401619 ) ) ;
#35415 = CARTESIAN_POINT ( 'NONE',  ( -0.5511811023622038563, -0.1870078740157479769, 0.4822834645669291653 ) ) ;
#35416 = CARTESIAN_POINT ( 'NONE',  ( -1.456692913385826182, 0.1771653543307087630, 0.000000000000000000 ) ) ;
#35417 = CARTESIAN_POINT ( 'NONE',  ( 0.7939632545931766261, -0.2845877964562161244, -0.3641732283464567121 ) ) ;
#35418 = CARTESIAN_POINT ( 'NONE',  ( 1.391076115485564868, -0.6046776061558807314, 0.2411417322834647770 ) ) ;
#35419 = CARTESIAN_POINT ( 'NONE',  ( -0.1265901696524993347, 0.4724409448818895907, -0.7132545931758530466 ) ) ;
#35420 = CARTESIAN_POINT ( 'NONE',  ( 1.030183727034121421, -0.08942795157527998196, 0.3641732283464567121 ) ) ;
#35421 = CARTESIAN_POINT ( 'NONE',  ( 0.8792650918635177559, -0.4281496062992127816, -0.4176697321401328100 ) ) ;
#35422 = CARTESIAN_POINT ( 'NONE',  ( -0.1974969037888706924, 0.3420746716998658843, -0.4048556430446195176 ) ) ;
#35423 = CARTESIAN_POINT ( 'NONE',  ( -0.3543307086614165824, -0.6692913385826771977, 8.415575281601705876E-17 ) ) ;
#35424 = LINE ( 'NONE', #35840, #78148 ) ;
#35425 = CARTESIAN_POINT ( 'NONE',  ( 1.371391076115485719, -0.5511811023622048555, -0.09757992244046775898 ) ) ;
#35426 = CARTESIAN_POINT ( 'NONE',  ( -0.6233595800524928121, -0.05778040916215522460, 0.4822834645669289988 ) ) ;
#35427 = CARTESIAN_POINT ( 'NONE',  ( -0.3420746716998660508, -0.1974969037888706924, -0.6017060367454067915 ) ) ;
#35428 = CARTESIAN_POINT ( 'NONE',  ( 1.338582677165355062, -0.1870078740157479769, 0.4822834645669291653 ) ) ;
#35429 = CARTESIAN_POINT ( 'NONE',  ( 0.2690288713910767848, -0.6692913385826773087, -0.1292274648535924053 ) ) ;
#35430 = CARTESIAN_POINT ( 'NONE',  ( 0.4593175853018380828, -0.004921259842519870586, -0.3153832671262229437 ) ) ;
#35431 = CARTESIAN_POINT ( 'NONE',  ( -1.646051170424378096, 0.8346805926620876059, -0.5309055118110233007 ) ) ;
#35432 = CARTESIAN_POINT ( 'NONE',  ( -0.03937007874015669567, 0.1771653543307087630, 0.000000000000000000 ) ) ;
#35433 = CARTESIAN_POINT ( 'NONE',  ( -1.568241469816272105, -0.3162353388693409650, -0.4822834645669289433 ) ) ;
#35434 = CARTESIAN_POINT ( 'NONE',  ( -0.3996062992125986590, 0.1070741851644051723, -1.369422572178477404 ) ) ;
#35435 = CARTESIAN_POINT ( 'NONE',  ( 0.8792650918635177559, 0.05413385826771666132, 0.4176697321401328100 ) ) ;
#35436 = CARTESIAN_POINT ( 'NONE',  ( -0.3917322834645671215, 0.1049643490035301469, -1.127296587926509108 ) ) ;
#35437 = CARTESIAN_POINT ( 'NONE',  ( 1.463254593175853824, -0.5511811023622046335, 0.09757992244046803654 ) ) ;
#35438 = FACE_OUTER_BOUND ( 'NONE', #25950, .T. ) ;
#35439 = CARTESIAN_POINT ( 'NONE',  ( 0.06561679790026316017, -0.004921259842519870586, -0.3153832671262229437 ) ) ;
#35440 = CARTESIAN_POINT ( 'NONE',  ( 0.1049868766404206816, 0.2306618581243848609, 0.2411417322834645549 ) ) ;
#35441 = CARTESIAN_POINT ( 'NONE',  ( 1.548556430446194954, 0.1283753931104746893, -0.1820866141732285504 ) ) ;
#35442 = CARTESIAN_POINT ( 'NONE',  ( -1.167979002624671470, -0.3690944881889765550, -0.3153832671262227771 ) ) ;
#35443 = CARTESIAN_POINT ( 'NONE',  ( -1.620734908136482577, -0.6692913385826773087, -0.1292274648535924053 ) ) ;
#35444 = CONICAL_SURFACE ( 'NONE', #28712, 1.181102362204724310, 0.7853981633974621568 ) ;
#35445 = CARTESIAN_POINT ( 'NONE',  ( 0.4265091863517067594, 0.2952755905511811885, 0.1292274648535926551 ) ) ;
#35446 = CARTESIAN_POINT ( 'NONE',  ( 1.266404199475066328, -0.3162353388693409650, -0.4822834645669289433 ) ) ;
#35447 = CARTESIAN_POINT ( 'NONE',  ( 1.080276388343102000E-18, 0.1968503937007874127, 0.000000000000000000 ) ) ;
#35448 = CARTESIAN_POINT ( 'NONE',  ( 0.1377952755905518800, -0.5400638737290844871, 0.3530559997133364547 ) ) ;
#35449 = CARTESIAN_POINT ( 'NONE',  ( 1.141732283464567788, -0.6692913385826771977, 8.415575281601705876E-17 ) ) ;
#35450 = CARTESIAN_POINT ( 'NONE',  ( 0.8727034120734913358, -0.05778040916215522460, 0.4822834645669289988 ) ) ;
#35451 = LINE ( 'NONE', #29134, #69601 ) ;
#35452 = CARTESIAN_POINT ( 'NONE',  ( 0.7939632545931766261, -0.2845877964562161244, -0.3641732283464567121 ) ) ;
#35453 = CARTESIAN_POINT ( 'NONE',  ( 1.417322834645670104, -0.1870078740157480879, -0.4822834645669291653 ) ) ;
#35454 = CARTESIAN_POINT ( 'NONE',  ( 0.4855643044619428750, -0.004921259842519576551, 0.3153832671262227771 ) ) ;
#35455 = CIRCLE ( 'NONE', #36765, 1.122047244094488194 ) ;
#35456 = CARTESIAN_POINT ( 'NONE',  ( -0.03937007874015669567, 0.2952755905511811885, 0.000000000000000000 ) ) ;
#35457 = CARTESIAN_POINT ( 'NONE',  ( 0.6627296587926515548, 0.2952755905511811885, 0.1292274648535926551 ) ) ;
#35458 = CARTESIAN_POINT ( 'NONE',  ( -0.2493438320209966919, -0.4281496062992124485, 0.4176697321401328655 ) ) ;
#35459 = CARTESIAN_POINT ( 'NONE',  ( -0.006561679790025524116, -0.2845877964562159024, 0.3641732283464567677 ) ) ;
#35460 = CARTESIAN_POINT ( 'NONE',  ( 0.8202099737532813073, 0.2952755905511811885, 0.1292274648535926551 ) ) ;
#35461 = ADVANCED_FACE ( 'NONE', ( #45652 ), #46904, .F. ) ;
#35462 = CARTESIAN_POINT ( 'NONE',  ( 2.543486866223389153, 2.716535433070866645, 0.5314960629921260393 ) ) ;
#35463 = CARTESIAN_POINT ( 'NONE',  ( -1.115485564304461219, -0.4281496062992124485, 0.4176697321401328655 ) ) ;
#35465 = CARTESIAN_POINT ( 'NONE',  ( -0.3996062992125985480, -0.1070741851644057135, -1.148293963254592986 ) ) ;
#35464 = CARTESIAN_POINT ( 'NONE',  ( -1.090776338374007226, 0.02791078216816064370, 0.4328096321851915285 ) ) ;
#35466 = CARTESIAN_POINT ( 'NONE',  ( 1.080276388343102000E-18, 0.000000000000000000, 0.000000000000000000 ) ) ;
#35467 = CARTESIAN_POINT ( 'NONE',  ( -1.377952755905511140, -0.6692913385826771977, 8.415575281601705876E-17 ) ) ;
#35468 = CARTESIAN_POINT ( 'NONE',  ( -0.4527559055118102749, 0.1660481256975885056, 0.3530559997133364547 ) ) ;
#35469 = CARTESIAN_POINT ( 'NONE',  ( -0.4091458600556402980, -0.2362204724409451284, 0.1049868766404199460 ) ) ;
#35470 = CARTESIAN_POINT ( 'NONE',  ( 0.1974969037888704704, 0.3420746716998660508, -2.191601049868766360 ) ) ;
#35471 = ORIENTED_EDGE ( 'NONE', *, *, #60504, .T. ) ;
#35472 = CARTESIAN_POINT ( 'NONE',  ( 0.6036745406824154392, 0.1283753931104746893, -0.1820866141732285504 ) ) ;
#35473 = CARTESIAN_POINT ( 'NONE',  ( -0.1049643490035307020, 0.3917322834645669549, -0.9435695538057740084 ) ) ;
#35474 = CARTESIAN_POINT ( 'NONE',  ( 0.9973753280839902091, 0.2306618581243847221, -0.2411417322834647770 ) ) ;
#35475 = CARTESIAN_POINT ( 'NONE',  ( 0.4724409448818898682, 2.892866454678787531E-17, -2.480314960629921295 ) ) ;
#35476 = DIRECTION ( 'NONE',  ( -1.000000000000000000, -3.553564358545519864E-16, 0.000000000000000000 ) ) ;
#35477 = CARTESIAN_POINT ( 'NONE',  ( -1.541994750656167090, 0.1771653543307087630, 0.09757992244046791164 ) ) ;
#35478 = CARTESIAN_POINT ( 'NONE',  ( 1.673228346456693494, 0.1660481256975885056, 0.3530559997133364547 ) ) ;
#35479 = CARTESIAN_POINT ( 'NONE',  ( -1.620734908136482577, -0.6692913385826773087, -0.1292274648535924053 ) ) ;
#35480 = CARTESIAN_POINT ( 'NONE',  ( 0.2559055118110243332, 0.1660481256975885056, 0.3530559997133364547 ) ) ;
#35481 = CARTESIAN_POINT ( 'NONE',  ( -0.1049643490035306742, 0.3917322834645668994, -0.4015554873677671943 ) ) ;
#35482 = CARTESIAN_POINT ( 'NONE',  ( 0.01968503937007957949, -0.5400638737290845981, -0.3530559997133363437 ) ) ;
#35483 = CARTESIAN_POINT ( 'NONE',  ( -0.7611548556430438595, 0.1283753931104748280, 0.1820866141732283561 ) ) ;
#35484 = CARTESIAN_POINT ( 'NONE',  ( 0.8792650918635177559, -0.4281496062992127816, -0.4176697321401328100 ) ) ;
#35485 = CARTESIAN_POINT ( 'NONE',  ( 0.08530183727034192087, -0.3162353388693409650, -0.4822834645669289433 ) ) ;
#35486 = DIRECTION ( 'NONE',  ( 0.000000000000000000, 0.000000000000000000, -1.000000000000000000 ) ) ;
#35487 = CARTESIAN_POINT ( 'NONE',  ( -0.2362204724409451284, 0.4091458600556402425, -1.115485564304461885 ) ) ;
#35488 = CARTESIAN_POINT ( 'NONE',  ( 0.3917322834645670659, 2.398668435337828261E-17, -1.689651861713597603 ) ) ;
#35489 = CARTESIAN_POINT ( 'NONE',  ( 0.9120734908136490793, 0.2952755905511810774, -0.1292274648535930714 ) ) ;
#35490 = CARTESIAN_POINT ( 'NONE',  ( 0.05249343832021075018, 0.2306618581243847221, -0.2411417322834647770 ) ) ;
#35491 = CARTESIAN_POINT ( 'NONE',  ( -0.8989501312335946848, -0.6692913385826771977, 0.1292274648535927661 ) ) ;
#35492 = CARTESIAN_POINT ( 'NONE',  ( 1.043307086614173818, -0.5400638737290845981, -0.3530559997133363437 ) ) ;
#35493 = CARTESIAN_POINT ( 'NONE',  ( 0.3543307086614181922, -0.6692913385826771977, 8.415575281601705876E-17 ) ) ;
#35494 = CARTESIAN_POINT ( 'NONE',  ( 0.3917322834645669549, 0.1049643490035304660, -0.9967191601049870675 ) ) ;
#35495 = CARTESIAN_POINT ( 'NONE',  ( -0.5052493438320203589, -0.6692913385826771977, 0.1292274648535927661 ) ) ;
#35496 = CARTESIAN_POINT ( 'NONE',  ( 0.7480314960629927956, 0.2952755905511811885, 0.000000000000000000 ) ) ;
#35497 = CARTESIAN_POINT ( 'NONE',  ( 0.1443569553805781891, 0.05413385826771626580, -0.4176697321401330321 ) ) ;
#35498 = VECTOR ( 'NONE', #4079, 39.37007874015748143 ) ;
#35499 = CARTESIAN_POINT ( 'NONE',  ( 0.6496062992125991586, -0.4536011799217368745, -0.2665933059059886201 ) ) ;
#35500 = FACE_OUTER_BOUND ( 'NONE', #52403, .T. ) ;
#35501 = CARTESIAN_POINT ( 'NONE',  ( -1.646981627296586703, -0.3162353388693409650, -0.4822834645669289433 ) ) ;
#35502 = CARTESIAN_POINT ( 'NONE',  ( 0.4199475065616803948, -0.6046776061558809534, -0.2411417322834644161 ) ) ;
#35503 = CARTESIAN_POINT ( 'NONE',  ( 0.000000000000000000, 2.755905511811024056, 0.000000000000000000 ) ) ;
#35504 = CARTESIAN_POINT ( 'NONE',  ( -0.3917322834645669549, -0.1049643490035306603, -2.400262467191600635 ) ) ;
#35505 = ORIENTED_EDGE ( 'NONE', *, *, #49907, .F. ) ;
#35506 = EDGE_LOOP ( 'NONE', ( #1159, #17208, #26998, #68946 ) ) ;
#35507 = CARTESIAN_POINT ( 'NONE',  ( 1.141732283464567788, -0.6692913385826771977, 8.415575281601705876E-17 ) ) ;
#35508 = CARTESIAN_POINT ( 'NONE',  ( 0.4396325459317590445, -0.5511811023622046335, 0.09757992244046803654 ) ) ;
#35510 = CARTESIAN_POINT ( 'NONE',  ( 1.348312163386739426, 0.2755905511811023723, 0.6402614161801758463 ) ) ;
#35509 = CARTESIAN_POINT ( 'NONE',  ( 0.1181102362204724254, 8.537024980200824098E-18, 0.000000000000000000 ) ) ;
#35511 = CARTESIAN_POINT ( 'NONE',  ( -9.594673741351313045E-17, 0.3917322834645670104, -0.8720472440944883052 ) ) ;
#35512 = DIRECTION ( 'NONE',  ( 0.000000000000000000, 0.000000000000000000, -1.000000000000000000 ) ) ;
#35513 = CARTESIAN_POINT ( 'NONE',  ( 0.3965571307776156740, 0.02707642104391132579, -1.929133858267719104 ) ) ;
#35514 = CARTESIAN_POINT ( 'NONE',  ( 0.3917322834645670104, 2.398668435337828261E-17, -1.462598425196850460 ) ) ;
#35515 = CIRCLE ( 'NONE', #73132, 0.3129921259842520787 ) ;
#35516 = CARTESIAN_POINT ( 'NONE',  ( 0.3996062992125986035, -0.1070741851644052972, -2.550524934383202158 ) ) ;
#35517 = CARTESIAN_POINT ( 'NONE',  ( 0.9448818897637802916, -0.1870078740157479769, 0.4822834645669291653 ) ) ;
#35518 = CARTESIAN_POINT ( 'NONE',  ( -0.9055118110236215490, -0.6692913385826771977, 8.415575281601705876E-17 ) ) ;
#35519 = CARTESIAN_POINT ( 'NONE',  ( -0.6364829396325453192, -0.3162353388693405765, 0.4822834645669290543 ) ) ;
#35520 = CARTESIAN_POINT ( 'NONE',  ( 0.5249343832021003964, 0.2306618581243847221, -0.2411417322834647770 ) ) ;
#35521 = ORIENTED_EDGE ( 'NONE', *, *, #21285, .F. ) ;
#35522 = CARTESIAN_POINT ( 'NONE',  ( 1.246719160104987623, -0.4281496062992124485, 0.4176697321401328655 ) ) ;
#35523 = CARTESIAN_POINT ( 'NONE',  ( -2.795275590551183686, 1.338582677165354395, -1.990688069879260956E-16 ) ) ;
#35524 = CARTESIAN_POINT ( 'NONE',  ( 1.102362204724410155, -0.1870078740157480601, -0.3641732283464567677 ) ) ;
#35525 = CARTESIAN_POINT ( 'NONE',  ( -0.3996062992125985480, -7.340648628747423112E-17, -2.163385826771653697 ) ) ;
#35526 = CARTESIAN_POINT ( 'NONE',  ( -1.286089238845143479, 0.1283753931104746893, -0.1820866141732285504 ) ) ;
#35527 = CARTESIAN_POINT ( 'NONE',  ( -9.594673741351313045E-17, 0.3917322834645670104, 0.007874015748031541057 ) ) ;
#35528 = CARTESIAN_POINT ( 'NONE',  ( 0.2755905511811031494, 0.2952755905511811885, 0.000000000000000000 ) ) ;
#35530 = CARTESIAN_POINT ( 'NONE',  ( -1.220472440944882386, -0.1870078740157480046, 1.254653134982923898E-17 ) ) ;
#35529 = CARTESIAN_POINT ( 'NONE',  ( 1.686351706036745890, 0.2952755905511811885, 0.1292274648535926551 ) ) ;
#35531 = CARTESIAN_POINT ( 'NONE',  ( -1.082677165354329896, 0.07958543189024085140, 0.2665933059059887866 ) ) ;
#35532 = CARTESIAN_POINT ( 'NONE',  ( 0.5708661417322842269, 0.1660481256975885056, 0.3530559997133364547 ) ) ;
#35533 = CARTESIAN_POINT ( 'NONE',  ( 1.299212598425197429, 0.1771653543307087630, 0.000000000000000000 ) ) ;
#35534 = CARTESIAN_POINT ( 'NONE',  ( -9.594673741351310580E-17, 0.3917322834645669549, -1.024915067420260728 ) ) ;
#35535 = CARTESIAN_POINT ( 'NONE',  ( -1.345144356955379816, -0.08942795157528024563, -0.3641732283464568787 ) ) ;
#35536 = CARTESIAN_POINT ( 'NONE',  ( 1.227034120734908917, 0.2952755905511810774, -0.1292274648535930714 ) ) ;
#35537 = CARTESIAN_POINT ( 'NONE',  ( 0.2868249070713367876, 1.825030329442032917, 0.1258042619966805165 ) ) ;
#35538 = CARTESIAN_POINT ( 'NONE',  ( 0.006561679790026889343, -0.05778040916215522460, 0.4822834645669289988 ) ) ;
#35539 = CARTESIAN_POINT ( 'NONE',  ( -1.332020997375327642, -0.08942795157527998196, 0.3641732283464567121 ) ) ;
#35540 = CARTESIAN_POINT ( 'NONE',  ( -0.5183727034120726440, -0.5511811023622048555, -0.09757992244046775898 ) ) ;
#35541 = CARTESIAN_POINT ( 'NONE',  ( -0.8989501312335946848, 0.2952755905511810774, -0.1292274648535930714 ) ) ;
#35542 = CARTESIAN_POINT ( 'NONE',  ( -1.601049868766403650, 0.1283753931104746893, -0.1820866141732285504 ) ) ;
#35543 = CARTESIAN_POINT ( 'NONE',  ( -0.3917322834645671770, 0.1049643490035302024, -0.6594681346794770693 ) ) ;
#35544 = CARTESIAN_POINT ( 'NONE',  ( 0.1443569553805781891, -0.4281496062992124485, 0.4176697321401328655 ) ) ;
#35545 = FACE_OUTER_BOUND ( 'NONE', #29700, .T. ) ;
#35546 = CARTESIAN_POINT ( 'NONE',  ( 0.4724409448818896462, 0.1265901696524990294, -1.933727034120735100 ) ) ;
#35547 = CARTESIAN_POINT ( 'NONE',  ( -1.220472440944881054, 0.2952755905511811885, 0.000000000000000000 ) ) ;
#35548 = CARTESIAN_POINT ( 'NONE',  ( -0.6430446194225716283, -0.3690944881889763329, 0.3153832671262228327 ) ) ;
#35549 = CARTESIAN_POINT ( 'NONE',  ( -1.646981627296586703, -0.05778040916215522460, 0.4822834645669289988 ) ) ;
#35550 = CARTESIAN_POINT ( 'NONE',  ( 0.1640419947506569498, -0.3162353388693409650, -0.4822834645669289433 ) ) ;
#35551 = CARTESIAN_POINT ( 'NONE',  ( 0.2362204724409456558, -0.1870078740157479769, 0.3641732283464567677 ) ) ;
#35552 = CARTESIAN_POINT ( 'NONE',  ( -1.141732283464566011, -0.5511811023622047445, 6.969142054262312111E-17 ) ) ;
#35553 = CARTESIAN_POINT ( 'NONE',  ( -1.489501312335957062, -0.3162353388693409650, -0.4822834645669289433 ) ) ;
#35554 = CARTESIAN_POINT ( 'NONE',  ( -1.423884514435694859, -0.3162353388693405765, 0.4822834645669290543 ) ) ;
#35555 = CARTESIAN_POINT ( 'NONE',  ( 1.555118110236221041, 0.1660481256975883668, -0.3530559997133364547 ) ) ;
#35556 = CARTESIAN_POINT ( 'NONE',  ( -0.03443470937339728616, 0.2755905511811023723, -1.537015892239756099 ) ) ;
#35557 = CARTESIAN_POINT ( 'NONE',  ( 0.4593175853018380828, -0.004921259842519870586, -0.3153832671262229437 ) ) ;
#35558 = CIRCLE ( 'NONE', #66444, 0.2952755905511810774 ) ;
#35559 = CARTESIAN_POINT ( 'NONE',  ( 1.036745406824147731, 0.05413385826771666132, 0.4176697321401328100 ) ) ;
#35560 = FACE_BOUND ( 'NONE', #37373, .T. ) ;
#35561 = CARTESIAN_POINT ( 'NONE',  ( 1.391076115485564868, -0.5023911411419708095, 0.1820866141732285504 ) ) ;
#35562 = VERTEX_POINT ( 'NONE', #13694 ) ;
#35563 = CARTESIAN_POINT ( 'NONE',  ( -1.141732283464566011, 0.2952755905511811885, 0.000000000000000000 ) ) ;
#35564 = EDGE_CURVE ( 'NONE', #58335, #14206, #68976, .T. ) ;
#35565 = CARTESIAN_POINT ( 'NONE',  ( -1.036745406824146176, -0.4281496062992124485, 0.4176697321401328655 ) ) ;
#35566 = CARTESIAN_POINT ( 'NONE',  ( 0.3608923884514443348, 0.2952755905511810774, -0.1292274648535930714 ) ) ;
#35567 = CARTESIAN_POINT ( 'NONE',  ( 0.1070741851644053666, 0.3996062992125986035, -0.1509186351706036655 ) ) ;
#35568 = CARTESIAN_POINT ( 'NONE',  ( 0.3996062992125986035, -0.1070741851644052972, -2.235564304461942431 ) ) ;
#35569 = CARTESIAN_POINT ( 'NONE',  ( 0.9055118110236227702, -0.6692913385826771977, 8.415575281601705876E-17 ) ) ;
#35570 = CARTESIAN_POINT ( 'NONE',  ( -1.679790026246718693, 0.2306618581243847221, -0.2411417322834647770 ) ) ;
#35571 = CARTESIAN_POINT ( 'NONE',  ( 0.2624671916010504757, 0.2306618581243848609, 0.2411417322834645549 ) ) ;
#35572 = CARTESIAN_POINT ( 'NONE',  ( 0.7611548556430451917, -0.6046776061558807314, 0.2411417322834647770 ) ) ;
#35573 = CARTESIAN_POINT ( 'NONE',  ( 0.1998031496062994405, -0.3460692066303958092, -1.666666666666666741 ) ) ;
#35574 = AXIS2_PLACEMENT_3D ( 'NONE', #3515, #48528, #11070 ) ;
#35575 = CARTESIAN_POINT ( 'NONE',  ( -0.3949938075777409963, -7.255918531996591613E-17, -0.9842519685039369248 ) ) ;
#35576 = CARTESIAN_POINT ( 'NONE',  ( -0.3996062992125986035, -7.340648628747425578E-17, -2.559055118110236560 ) ) ;
#35577 = CARTESIAN_POINT ( 'NONE',  ( -2.530077735013332330, 2.729661055914112566, 0.5314960629921260393 ) ) ;
#35578 = CARTESIAN_POINT ( 'NONE',  ( -9.594673741351313045E-17, 0.3917322834645670104, -0.3070866141732283006 ) ) ;
#35579 = CARTESIAN_POINT ( 'NONE',  ( -0.1312335958005241554, 0.1283753931104748280, 0.1820866141732283561 ) ) ;
#35580 = CARTESIAN_POINT ( 'NONE',  ( -0.4068241469816267775, 0.05413385826771626580, -0.4176697321401330321 ) ) ;
#35581 = CARTESIAN_POINT ( 'NONE',  ( 0.8136482939632553313, 0.2306618581243848609, 0.2411417322834645549 ) ) ;
#35582 = CARTESIAN_POINT ( 'NONE',  ( 0.3949938075777408852, 0.1058382717557500435, -2.091207349081364519 ) ) ;
#35583 = CARTESIAN_POINT ( 'NONE',  ( -0.1509186351706028884, -0.2845877964562161244, -0.3641732283464567121 ) ) ;
#35584 = CARTESIAN_POINT ( 'NONE',  ( -1.200787401574802349, -0.5400638737290844871, 0.3530559997133364547 ) ) ;
#35585 = CARTESIAN_POINT ( 'NONE',  ( 1.017060367454068581, -0.05778040916215560624, -0.4822834645669293319 ) ) ;
#35586 = CARTESIAN_POINT ( 'NONE',  ( 0.4091458600556403535, 0.2362204724409449896, -2.493438320209973469 ) ) ;
#35587 = CARTESIAN_POINT ( 'NONE',  ( -0.3996062992125987146, 0.1070741851644051862, -1.922572178477689908 ) ) ;
#35588 = FACE_OUTER_BOUND ( 'NONE', #70999, .T. ) ;
#35589 = VERTEX_POINT ( 'NONE', #73011 ) ;
#35590 = CARTESIAN_POINT ( 'NONE',  ( 0.8070866141732288002, 0.1660481256975885056, 0.3530559997133364547 ) ) ;
#35591 = CARTESIAN_POINT ( 'NONE',  ( 1.351706036745407458, -0.3690944881889765550, -0.3153832671262227771 ) ) ;
#35593 = CARTESIAN_POINT ( 'NONE',  ( 1.574803149606299746, -0.1870078740157479769, 0.4822834645669291653 ) ) ;
#35592 = CARTESIAN_POINT ( 'NONE',  ( 1.541994750656168645, 0.2952755905511810774, -0.1292274648535930714 ) ) ;
#35594 = CARTESIAN_POINT ( 'NONE',  ( -0.3917322834645669549, -7.196005306013483243E-17, -2.639088295766717884 ) ) ;
#35595 = CARTESIAN_POINT ( 'NONE',  ( -1.220472440944882386, -3.283890673957456492E-15, 0.4445507791589070057 ) ) ;
#35596 = CARTESIAN_POINT ( 'NONE',  ( 1.279527559055118724, -0.5400638737290845981, -0.3530559997133363437 ) ) ;
#35597 = LINE ( 'NONE', #9513, #63507 ) ;
#35598 = CARTESIAN_POINT ( 'NONE',  ( 0.07217847769028949700, -0.05778040916215560624, -0.4822834645669293319 ) ) ;
#35599 = CARTESIAN_POINT ( 'NONE',  ( -0.7677165354330699465, 0.1660481256975885056, 0.3530559997133364547 ) ) ;
#35600 = ADVANCED_FACE ( 'NONE', ( #29221, #41023 ), #36360, .T. ) ;
#35601 = CARTESIAN_POINT ( 'NONE',  ( 1.443569553805774897, 0.2306618581243848609, 0.2411417322834645549 ) ) ;
#35602 = CARTESIAN_POINT ( 'NONE',  ( -0.2867679344610365999, 0.2867679344610364889, -0.2618110236220473341 ) ) ;
#35603 = CARTESIAN_POINT ( 'NONE',  ( 0.02624671916010564918, 0.2306618581243848609, 0.2411417322834645549 ) ) ;
#35604 = CARTESIAN_POINT ( 'NONE',  ( -0.1958661417322836718, 0.3392501089628017219, -2.209973753280840114 ) ) ;
#35605 = CARTESIAN_POINT ( 'NONE',  ( -1.548556430446193399, -0.5023911411419708095, -0.1820866141732282451 ) ) ;
#35606 = ORIENTED_EDGE ( 'NONE', *, *, #77795, .T. ) ;
#35607 = CARTESIAN_POINT ( 'NONE',  ( -0.1058382717557497937, -0.3949938075777411628, -2.276902887139107712 ) ) ;
#35608 = EDGE_LOOP ( 'NONE', ( #64333, #70059, #77927, #44046 ) ) ;
#35609 = DIRECTION ( 'NONE',  ( 0.000000000000000000, -1.000000000000000000, 0.000000000000000000 ) ) ;
#35610 = CARTESIAN_POINT ( 'NONE',  ( -1.692913385826770645, 0.2952755905511811885, 0.000000000000000000 ) ) ;
#35611 = CARTESIAN_POINT ( 'NONE',  ( -0.3996062992125986035, -0.1070741851644056997, -0.8333333333333332593 ) ) ;
#35612 = DIRECTION ( 'NONE',  ( -3.491481338843132961E-15, -0.000000000000000000, 1.000000000000000000 ) ) ;
#35613 = CARTESIAN_POINT ( 'NONE',  ( -1.813482582612293559, 2.755905511811024056, -0.5314960629921260393 ) ) ;
#35614 = CARTESIAN_POINT ( 'NONE',  ( -0.9548908091195642545, -2.567464376874931580E-15, -0.4445507791589072832 ) ) ;
#35615 = CARTESIAN_POINT ( 'NONE',  ( 0.01218835185197312924, -0.3960428127060638404, -2.755905511811024056 ) ) ;
#35616 = CARTESIAN_POINT ( 'NONE',  ( 0.3917322834645669549, 0.1049643490035304660, -0.05183727034120744204 ) ) ;
#35617 = CARTESIAN_POINT ( 'NONE',  ( -0.1771653543307080136, 0.07958543189024071263, -0.2665933059059888421 ) ) ;
#35618 = CARTESIAN_POINT ( 'NONE',  ( -0.9383202099737524282, -0.08942795157527998196, 0.3641732283464567121 ) ) ;
#35619 = AXIS2_PLACEMENT_3D ( 'NONE', #21645, #32606, #34281 ) ;
#35620 = CARTESIAN_POINT ( 'NONE',  ( -1.292650918635170010, 0.2952755905511810774, -0.1292274648535930714 ) ) ;
#35621 = CARTESIAN_POINT ( 'NONE',  ( 0.6692913385826777528, 0.2952755905511811885, 0.000000000000000000 ) ) ;
#35622 = CARTESIAN_POINT ( 'NONE',  ( -1.207349081364828436, -0.6046776061558807314, 0.2411417322834647770 ) ) ;
#35623 = CARTESIAN_POINT ( 'NONE',  ( -0.3917322834645670104, -7.196005306013484475E-17, 0.1259842519685039908 ) ) ;
#35624 = VERTEX_POINT ( 'NONE', #22495 ) ;
#35625 = CARTESIAN_POINT ( 'NONE',  ( -1.292650918635170010, 0.2952755905511810774, -0.1292274648535930714 ) ) ;
#35626 = CARTESIAN_POINT ( 'NONE',  ( 1.220472440944881942, 2.401574803149606474, -0.5309055118110238558 ) ) ;
#35627 =( LENGTH_UNIT ( ) NAMED_UNIT ( * ) SI_UNIT ( $, .METRE. ) );
#35628 = CARTESIAN_POINT ( 'NONE',  ( 0.4724409448818898682, 2.892866454678787531E-17, -1.535433070866141669 ) ) ;
#35629 = CARTESIAN_POINT ( 'NONE',  ( 0.4177787735907000366, 1.299212598425196985, -1.559171609364239375 ) ) ;
#35630 = EDGE_CURVE ( 'NONE', #44018, #23879, #45126, .T. ) ;
#35631 = CARTESIAN_POINT ( 'NONE',  ( -0.3392501089628019995, 0.1958661417322832277, -0.8057742782152230721 ) ) ;
#35632 = CARTESIAN_POINT ( 'NONE',  ( 0.2867679344610366554, -0.2867679344610365444, -2.702755905511810663 ) ) ;
#35633 = CARTESIAN_POINT ( 'NONE',  ( -0.8727034120734901146, -0.3162353388693405765, 0.4822834645669290543 ) ) ;
#35634 = CARTESIAN_POINT ( 'NONE',  ( 1.574803149606299746, -0.1870078740157480879, -0.4822834645669291653 ) ) ;
#35636 = CARTESIAN_POINT ( 'NONE',  ( -1.614173228346457378, 1.606230626554505658, -0.1372047244094477536 ) ) ;
#35635 = CARTESIAN_POINT ( 'NONE',  ( -1.692913385826770645, 0.2952755905511811885, 0.000000000000000000 ) ) ;
#35637 = CARTESIAN_POINT ( 'NONE',  ( 1.528871391076116026, 0.2952755905511811885, 0.1292274648535926551 ) ) ;
#35638 = CARTESIAN_POINT ( 'NONE',  ( -0.6167979002624665030, 0.05413385826771666132, 0.4176697321401328100 ) ) ;
#35639 = TOROIDAL_SURFACE ( 'NONE', #80001, 3.858267716535433323, 0.07874015748031495954 ) ;
#35640 = CARTESIAN_POINT ( 'NONE',  ( -0.3917322834645668994, -0.1049643490035306742, 0.03151537877396508314 ) ) ;
#35641 = CARTESIAN_POINT ( 'NONE',  ( -0.05905511811023545637, -0.4536011799217368745, -0.2665933059059886201 ) ) ;
#35642 = CARTESIAN_POINT ( 'NONE',  ( -0.3917322834645670104, -7.196005306013484475E-17, -0.5964566929133858775 ) ) ;
#35643 = CARTESIAN_POINT ( 'NONE',  ( -0.1049868766404193215, -0.5023911411419708095, 0.1820866141732285504 ) ) ;
#35644 = CARTESIAN_POINT ( 'NONE',  ( 1.089238845144357537, -0.3690944881889763329, 0.3153832671262228327 ) ) ;
#35645 = CARTESIAN_POINT ( 'NONE',  ( 0.3937007874015754361, -0.1870078740157480879, -0.4822834645669291653 ) ) ;
#35646 = CARTESIAN_POINT ( 'NONE',  ( -0.1312335958005241554, -0.5023911411419708095, -0.1820866141732282451 ) ) ;
#35647 = CARTESIAN_POINT ( 'NONE',  ( -0.1958661417322836718, 0.3392501089628017219, -2.209973753280840114 ) ) ;
#35648 = CARTESIAN_POINT ( 'NONE',  ( -1.502624671916009680, -0.3162353388693405765, 0.4822834645669290543 ) ) ;
#35649 = CARTESIAN_POINT ( 'NONE',  ( -1.266404199475064773, -0.08942795157528024563, -0.3641732283464568787 ) ) ;
#35650 = CARTESIAN_POINT ( 'NONE',  ( 0.1265901696524989462, 0.4724409448818897572, -0.3851706036745406458 ) ) ;
#35651 = CARTESIAN_POINT ( 'NONE',  ( 0.06561679790026316017, 0.05413385826771626580, -0.4176697321401330321 ) ) ;
#35652 = CARTESIAN_POINT ( 'NONE',  ( -0.4068241469816264999, -0.4281496062992124485, 0.4176697321401328655 ) ) ;
#35653 = CARTESIAN_POINT ( 'NONE',  ( 0.01000891935578606708, -2.191421614605370878E-15, 0.4445507791589071167 ) ) ;
#35654 = CARTESIAN_POINT ( 'NONE',  ( 0.5183727034120741983, 0.1771653543307087075, -0.09757992244046823083 ) ) ;
#35655 = CARTESIAN_POINT ( 'NONE',  ( -0.2427821522309703550, -0.05778040916215560624, -0.4822834645669293319 ) ) ;
#35656 = CARTESIAN_POINT ( 'NONE',  ( -0.5839895013123351797, -0.6692913385826771977, 0.1292274648535927661 ) ) ;
#35657 = CARTESIAN_POINT ( 'NONE',  ( 0.000000000000000000, 2.755905511811024056, 0.000000000000000000 ) ) ;
#35658 = LINE ( 'NONE', #79058, #62284 ) ;
#35659 = CARTESIAN_POINT ( 'NONE',  ( -0.04593175853018302557, 0.2952755905511811885, 0.1292274648535926551 ) ) ;
#35660 = CARTESIAN_POINT ( 'NONE',  ( 0.1070741851644053388, 0.3996062992125986035, -1.487532808398950301 ) ) ;
#35661 = CARTESIAN_POINT ( 'NONE',  ( 1.581364829396326277, -0.05778040916215522460, 0.4822834645669289988 ) ) ;
#35662 = CARTESIAN_POINT ( 'NONE',  ( -0.1181102362204717315, 0.1771653543307087630, 0.000000000000000000 ) ) ;
#35663 = CARTESIAN_POINT ( 'NONE',  ( -0.3805774278215216522, -0.4281496062992127816, -0.4176697321401328100 ) ) ;
#35664 = CARTESIAN_POINT ( 'NONE',  ( -1.450131233595799651, 0.1771653543307087075, -0.09757992244046823083 ) ) ;
#35665 = CARTESIAN_POINT ( 'NONE',  ( 1.194225721784777594, 0.05413385826771666132, 0.4176697321401328100 ) ) ;
#35666 = CARTESIAN_POINT ( 'NONE',  ( -1.443569553805773564, 0.2306618581243847221, -0.2411417322834647770 ) ) ;
#35667 = CARTESIAN_POINT ( 'NONE',  ( -0.7349081364829390672, 0.1283753931104746893, -0.1820866141732285504 ) ) ;
#35668 = CARTESIAN_POINT ( 'NONE',  ( -0.3996062992125986035, 0.1070741851644051584, -0.2670603674540682482 ) ) ;
#35669 = CARTESIAN_POINT ( 'NONE',  ( 0.1070741851644054915, -0.3996062992125986035, -0.7152230971128609172 ) ) ;
#35670 = CARTESIAN_POINT ( 'NONE',  ( 0.1058382717557500713, -0.3949938075777409408, 0.07217847769028866434 ) ) ;
#35671 = CARTESIAN_POINT ( 'NONE',  ( 1.410761154855643795, -0.08942795157528024563, -0.3641732283464568787 ) ) ;
#35672 = CARTESIAN_POINT ( 'NONE',  ( 1.305774278215223960, 0.1771653543307087075, -0.09757992244046823083 ) ) ;
#35673 = CARTESIAN_POINT ( 'NONE',  ( 0.8989501312335963501, -0.6692913385826773087, -0.1292274648535924053 ) ) ;
#35674 = CARTESIAN_POINT ( 'NONE',  ( 0.4396325459317593221, 0.2066929133858267098, -0.1054918080437494132 ) ) ;
#35675 = CARTESIAN_POINT ( 'NONE',  ( 0.9514435695538062676, -0.05778040916215522460, 0.4822834645669289988 ) ) ;
#35676 = CARTESIAN_POINT ( 'NONE',  ( -0.1974969037888704149, -0.3420746716998661063, -0.9297900262467193588 ) ) ;
#35677 = CARTESIAN_POINT ( 'NONE',  ( 1.266404199475066328, -0.2845877964562161244, -0.3641732283464567121 ) ) ;
#35678 = CARTESIAN_POINT ( 'NONE',  ( 0.2493438320209980519, 0.05413385826771666132, 0.4176697321401328100 ) ) ;
#35679 = CARTESIAN_POINT ( 'NONE',  ( -0.6102362204724400829, -0.5400638737290845981, -0.3530559997133363437 ) ) ;
#35680 = CARTESIAN_POINT ( 'NONE',  ( 1.561679790026247350, 0.05413385826771626580, -0.4176697321401330321 ) ) ;
#35681 = CARTESIAN_POINT ( 'NONE',  ( -0.2362204724409451284, 0.4091458600556402425, -1.115485564304461885 ) ) ;
#35682 = CARTESIAN_POINT ( 'NONE',  ( -0.1070741851644057135, 0.3996062992125985480, -2.368766404199475151 ) ) ;
#35683 = AXIS2_PLACEMENT_3D ( 'NONE', #37088, #63587, #12253 ) ;
#35684 = CARTESIAN_POINT ( 'NONE',  ( 0.4790026246719167324, -0.08942795157527998196, 0.3641732283464567121 ) ) ;
#35685 = ORIENTED_EDGE ( 'NONE', *, *, #76828, .T. ) ;
#35686 = CARTESIAN_POINT ( 'NONE',  ( -0.2867679344610367109, 0.2867679344610365444, -0.6463447750994246732 ) ) ;
#35687 = ORIENTED_EDGE ( 'NONE', *, *, #672, .F. ) ;
#35688 = CARTESIAN_POINT ( 'NONE',  ( -0.4724409448818890911, -0.1870078740157479769, 0.4822834645669291653 ) ) ;
#35689 = CARTESIAN_POINT ( 'NONE',  ( -0.1115485564304453947, -0.6692913385826771977, 0.1292274648535927661 ) ) ;
#35690 = CARTESIAN_POINT ( 'NONE',  ( -0.4724409448818890911, -0.1870078740157480879, -0.4822834645669291653 ) ) ;
#35691 = CARTESIAN_POINT ( 'NONE',  ( 0.6233595800524942554, -0.05778040916215560624, -0.4822834645669293319 ) ) ;
#35692 = CARTESIAN_POINT ( 'NONE',  ( -0.8005249343832011588, 0.05413385826771626580, -0.4176697321401330321 ) ) ;
#35693 = CARTESIAN_POINT ( 'NONE',  ( -0.4199475065616791736, 0.2306618581243847221, -0.2411417322834647770 ) ) ;
#35694 = CARTESIAN_POINT ( 'NONE',  ( 1.043307086614173818, -0.5400638737290845981, -0.3530559997133363437 ) ) ;
#35695 = CARTESIAN_POINT ( 'NONE',  ( 0.4790026246719167324, -0.05778040916215522460, 0.4822834645669289988 ) ) ;
#35696 = CARTESIAN_POINT ( 'NONE',  ( 0.6824146981627303710, -0.6046776061558807314, 0.2411417322834647770 ) ) ;
#35697 = CARTESIAN_POINT ( 'NONE',  ( -0.3917322834645669549, -0.1049643490035306603, -0.8254593175853015552 ) ) ;
#35698 = CARTESIAN_POINT ( 'NONE',  ( -0.09842519685039295696, -0.4536011799217367080, 0.2665933059059888421 ) ) ;
#35699 = ORIENTED_EDGE ( 'NONE', *, *, #40855, .F. ) ;
#35700 = CARTESIAN_POINT ( 'NONE',  ( -0.1058382717557497937, -0.3949938075777411628, -1.174540682414698223 ) ) ;
#35701 = VERTEX_POINT ( 'NONE', #80593 ) ;
#35702 = CARTESIAN_POINT ( 'NONE',  ( -0.6561679790026240244, -0.5023911411419708095, 0.1820866141732285504 ) ) ;
#35703 = CARTESIAN_POINT ( 'NONE',  ( -0.5183727034120726440, 0.2952755905511811885, 0.1292274648535926551 ) ) ;
#35704 = DIRECTION ( 'NONE',  ( -0.7071067811865333619, 0.000000000000000000, -0.7071067811865615615 ) ) ;
#35705 = CARTESIAN_POINT ( 'NONE',  ( -0.8333333333333323711, -0.6692913385826773087, -0.1292274648535924053 ) ) ;
#35706 = CARTESIAN_POINT ( 'NONE',  ( -0.3412073490813641308, -0.6046776061558807314, 0.2411417322834647770 ) ) ;
#35707 = CARTESIAN_POINT ( 'NONE',  ( -1.115485564304461219, 0.05413385826771626580, -0.4176697321401330321 ) ) ;
#35708 = CARTESIAN_POINT ( 'NONE',  ( -1.476377952755905110, -0.5400638737290845981, -0.3530559997133363437 ) ) ;
#35709 = CARTESIAN_POINT ( 'NONE',  ( 0.8202099737532814183, -0.5511811023622048555, -0.09757992244046775898 ) ) ;
#35710 = CARTESIAN_POINT ( 'NONE',  ( 0.6299212598425338872, 2.165354330708662012, -3.886287458032460229 ) ) ;
#35711 = CARTESIAN_POINT ( 'NONE',  ( 0.2917302971764580977, 0.04706822171083047818, 5.873170128030150039 ) ) ;
#35712 = CARTESIAN_POINT ( 'NONE',  ( 0.4068241469816279987, -0.3690944881889765550, -0.3153832671262227771 ) ) ;
#35713 = CARTESIAN_POINT ( 'NONE',  ( -0.1574803149606292529, -0.1870078740157480879, -0.4822834645669291653 ) ) ;
#35714 = CARTESIAN_POINT ( 'NONE',  ( -0.1968503937007867743, 0.2952755905511811885, 0.000000000000000000 ) ) ;
#35715 = EDGE_LOOP ( 'NONE', ( #56190, #19841, #67288 ) ) ;
#35716 = CARTESIAN_POINT ( 'NONE',  ( 0.3460692066303959202, 0.1998031496062993295, -1.706036745406824151 ) ) ;
#35717 = CYLINDRICAL_SURFACE ( 'NONE', #66809, 0.3051181102362204856 ) ;
#35718 = ORIENTED_EDGE ( 'NONE', *, *, #36840, .T. ) ;
#35719 = CARTESIAN_POINT ( 'NONE',  ( -0.1998031496062991630, -0.3460692066303959202, -1.087270341207349000 ) ) ;
#35720 = DIRECTION ( 'NONE',  ( 0.000000000000000000, 0.000000000000000000, 1.000000000000000000 ) ) ;
#35721 = CARTESIAN_POINT ( 'NONE',  ( -0.8989501312335946848, 0.1771653543307087075, -0.09757992244046823083 ) ) ;
#35722 = CARTESIAN_POINT ( 'NONE',  ( -0.9251968503937002541, 0.1660481256975885056, 0.3530559997133364547 ) ) ;
#35723 = CARTESIAN_POINT ( 'NONE',  ( 0.4091458600556403535, 0.2362204724409449896, -0.2887139107611548794 ) ) ;
#35724 = CARTESIAN_POINT ( 'NONE',  ( 0.3917322834645670104, -0.1049643490035303411, -2.715879265091863726 ) ) ;
#35725 = CARTESIAN_POINT ( 'NONE',  ( 1.686351706036745890, 0.2952755905511811885, 0.1292274648535926551 ) ) ;
#35726 = CARTESIAN_POINT ( 'NONE',  ( 0.3608923884514443348, 0.2952755905511810774, -0.1292274648535930714 ) ) ;
#35727 = CARTESIAN_POINT ( 'NONE',  ( 0.5839895013123367340, 0.2952755905511811885, 0.1292274648535926551 ) ) ;
#35728 = CARTESIAN_POINT ( 'NONE',  ( -0.7283464566929126471, -0.4536011799217367080, 0.2665933059059888421 ) ) ;
#35729 = CARTESIAN_POINT ( 'NONE',  ( 0.08530183727034192087, -0.3162353388693409650, -0.4822834645669289433 ) ) ;
#35730 = CARTESIAN_POINT ( 'NONE',  ( 0.2362204724409449064, 0.4091458600556404646, -2.425853018372703396 ) ) ;
#35731 = CARTESIAN_POINT ( 'NONE',  ( -0.5577427821522301654, -0.2845877964562159024, 0.3641732283464567677 ) ) ;
#35732 = EDGE_CURVE ( 'NONE', #44828, #72873, #34851, .T. ) ;
#35733 = CARTESIAN_POINT ( 'NONE',  ( -0.5511811023622041894, -0.1870078740157480879, -0.4822834645669291653 ) ) ;
#35734 = CARTESIAN_POINT ( 'NONE',  ( -0.3420746716998662729, 0.1974969037888702206, -1.835301837270341130 ) ) ;
#35735 = CARTESIAN_POINT ( 'NONE',  ( 1.122047244094488860, 0.07958543189024085140, 0.2665933059059887866 ) ) ;
#35736 = CARTESIAN_POINT ( 'NONE',  ( 0.03937007874015806264, 0.1771653543307087630, 0.000000000000000000 ) ) ;
#35737 = CARTESIAN_POINT ( 'NONE',  ( 1.279527559055118724, -0.4536011799217368745, -0.2665933059059886201 ) ) ;
#35738 = CARTESIAN_POINT ( 'NONE',  ( -1.332020997375327642, -0.3162353388693409650, -0.4822834645669289433 ) ) ;
#35739 = CARTESIAN_POINT ( 'NONE',  ( -0.9317585301837263412, -0.3690944881889765550, -0.3153832671262227771 ) ) ;
#35740 = CARTESIAN_POINT ( 'NONE',  ( 1.586688153636164111, 1.522296263979924902, -0.1275903502784764554 ) ) ;
#35741 = CARTESIAN_POINT ( 'NONE',  ( -1.108923884514435132, -0.3162353388693405765, 0.4822834645669290543 ) ) ;
#35742 = CARTESIAN_POINT ( 'NONE',  ( -0.5905511811023613777, -0.6692913385826771977, 8.415575281601705876E-17 ) ) ;
#35743 = CARTESIAN_POINT ( 'NONE',  ( 0.5052493438320218022, -0.6692913385826773087, -0.1292274648535924053 ) ) ;
#35744 = CARTESIAN_POINT ( 'NONE',  ( -0.3392501089628019439, 0.1958661417322832554, -2.468484621226035181 ) ) ;
#35745 = VECTOR ( 'NONE', #40490, 39.37007874015748143 ) ;
#35746 = CARTESIAN_POINT ( 'NONE',  ( -1.857294464233399278, 1.070443199938749590, -0.08545185031209458215 ) ) ;
#35747 = CARTESIAN_POINT ( 'NONE',  ( 0.1640419947506569498, -0.2845877964562161244, -0.3641732283464567121 ) ) ;
#35748 = CARTESIAN_POINT ( 'NONE',  ( 0.8923884514435701520, -0.6046776061558809534, -0.2411417322834644161 ) ) ;
#35749 = CARTESIAN_POINT ( 'NONE',  ( -1.318897637795274802, -0.4536011799217368745, -0.2665933059059886201 ) ) ;
#35750 = EDGE_CURVE ( 'NONE', #57500, #67621, #74731, .T. ) ;
#35751 = CARTESIAN_POINT ( 'NONE',  ( 1.036745406824147731, 0.05413385826771666132, 0.4176697321401328100 ) ) ;
#35752 = CARTESIAN_POINT ( 'NONE',  ( -1.555118110236219930, 0.07958543189024085140, 0.2665933059059887866 ) ) ;
#35753 = CARTESIAN_POINT ( 'NONE',  ( -1.371391076115484831, 0.2952755905511810774, -0.1292274648535930714 ) ) ;
#35754 = CARTESIAN_POINT ( 'NONE',  ( -1.010498687664041384, -0.4281496062992127816, -0.4176697321401328100 ) ) ;
#35755 = CARTESIAN_POINT ( 'NONE',  ( 0.02624671916010564918, -0.5023911411419708095, -0.1820866141732282451 ) ) ;
#35756 = LINE ( 'NONE', #23120, #7132 ) ;
#35757 = CARTESIAN_POINT ( 'NONE',  ( 0.8464566929133865436, 0.07958543189024071263, -0.2665933059059888421 ) ) ;
#35758 = EDGE_CURVE ( 'NONE', #62196, #81967, #4372, .T. ) ;
#35759 = CARTESIAN_POINT ( 'NONE',  ( -0.2427821522309703550, -0.3162353388693405765, 0.4822834645669290543 ) ) ;
#35760 = CARTESIAN_POINT ( 'NONE',  ( 0.3996062992125985480, 2.446882876249141654E-17, -0.1948818897637795422 ) ) ;
#35761 = CARTESIAN_POINT ( 'NONE',  ( -1.108923884514435132, -0.3162353388693405765, 0.4822834645669290543 ) ) ;
#35762 = CARTESIAN_POINT ( 'NONE',  ( 0.3917322834645669549, 0.1049643490035304660, -1.784120734908136274 ) ) ;
#35763 = CARTESIAN_POINT ( 'NONE',  ( 0.9251968503937015864, -0.4536011799217367080, 0.2665933059059888421 ) ) ;
#35764 = CARTESIAN_POINT ( 'NONE',  ( -0.1377952755905504645, -0.5400638737290845981, -0.3530559997133363437 ) ) ;
#35765 = CARTESIAN_POINT ( 'NONE',  ( -0.1377952755905504645, -0.5400638737290845981, -0.3530559997133363437 ) ) ;
#35766 = CARTESIAN_POINT ( 'NONE',  ( -0.5314960629921250401, 0.07958543189024085140, 0.2665933059059887866 ) ) ;
#35767 = CARTESIAN_POINT ( 'NONE',  ( -1.313877454013331780, 0.2755905511811023723, 0.7983292792091805090 ) ) ;
#35768 = CARTESIAN_POINT ( 'NONE',  ( -0.4855643044619415427, -0.004921259842519870586, -0.3153832671262229437 ) ) ;
#35769 = CARTESIAN_POINT ( 'NONE',  ( 0.5052493438320218022, -0.6692913385826773087, -0.1292274648535924053 ) ) ;
#35770 = CARTESIAN_POINT ( 'NONE',  ( -1.253280839895012377, -0.08942795157527998196, 0.3641732283464567121 ) ) ;
#35771 = CARTESIAN_POINT ( 'NONE',  ( 0.3996062992125984925, 0.1070741851644054637, -0.9888451443569553634 ) ) ;
#35772 = CARTESIAN_POINT ( 'NONE',  ( 1.587926509186352142, 0.05413385826771666132, 0.4176697321401328100 ) ) ;
#35773 = CARTESIAN_POINT ( 'NONE',  ( -3.237502121466738103, 2.729657719074700672, 0.5314960629921260393 ) ) ;
#35774 = ORIENTED_EDGE ( 'NONE', *, *, #59249, .F. ) ;
#35775 = CARTESIAN_POINT ( 'NONE',  ( -1.410761154855642463, -0.08942795157527998196, 0.3641732283464567121 ) ) ;
#35776 = CARTESIAN_POINT ( 'NONE',  ( -0.5118110236220466680, -0.6692913385826771977, 8.415575281601705876E-17 ) ) ;
#35777 = EDGE_CURVE ( 'NONE', #60543, #82716, #76108, .T. ) ;
#35778 = CARTESIAN_POINT ( 'NONE',  ( -1.305774278215222184, 0.2952755905511811885, 0.1292274648535926551 ) ) ;
#35779 = CARTESIAN_POINT ( 'NONE',  ( -0.3917322834645671215, 0.1049643490035301469, -1.534776902887139194 ) ) ;
#35780 = CARTESIAN_POINT ( 'NONE',  ( 0.000000000000000000, 2.755905511811024056, 0.000000000000000000 ) ) ;
#35781 = CARTESIAN_POINT ( 'NONE',  ( 1.266404199475066328, -0.3162353388693409650, -0.4822834645669289433 ) ) ;
#35782 = CARTESIAN_POINT ( 'NONE',  ( 0.2887139107611556010, 0.2306618581243847221, -0.2411417322834647770 ) ) ;
#35783 = CARTESIAN_POINT ( 'NONE',  ( -0.1958661417322836718, 0.3392501089628017219, -2.682414698162729483 ) ) ;
#35784 = CIRCLE ( 'NONE', #16996, 0.5118110236220472231 ) ;
#35786 = AXIS2_PLACEMENT_3D ( 'NONE', #23207, #56009, #17336 ) ;
#35785 = CARTESIAN_POINT ( 'NONE',  ( -0.3996062992125986035, 0.1070741851644051584, -2.471784776902886893 ) ) ;
#35787 = CARTESIAN_POINT ( 'NONE',  ( 1.587926509186352142, -0.004921259842519576551, 0.3153832671262227771 ) ) ;
#35788 = CARTESIAN_POINT ( 'NONE',  ( 4.893765752498283924E-17, -0.3996062992125986035, -0.3937007874015748254 ) ) ;
#35790 = EDGE_CURVE ( 'NONE', #4444, #29055, #57201, .T. ) ;
#35789 = ORIENTED_EDGE ( 'NONE', *, *, #27285, .T. ) ;
#35791 = CARTESIAN_POINT ( 'NONE',  ( -0.8333333333333323711, 0.1771653543307087630, 0.09757992244046791164 ) ) ;
#35792 = CARTESIAN_POINT ( 'NONE',  ( 0.1958661417322834775, 0.3392501089628018884, -2.183727034120734878 ) ) ;
#35793 = ORIENTED_EDGE ( 'NONE', *, *, #67691, .T. ) ;
#35794 = CARTESIAN_POINT ( 'NONE',  ( 0.8989501312335963501, -0.6692913385826773087, -0.1292274648535924053 ) ) ;
#35795 = CARTESIAN_POINT ( 'NONE',  ( -0.5249343832020990641, -0.6046776061558809534, -0.2411417322834644161 ) ) ;
#35796 = CARTESIAN_POINT ( 'NONE',  ( -1.266404199475064773, -0.05778040916215560624, -0.4822834645669293319 ) ) ;
#35797 = CARTESIAN_POINT ( 'NONE',  ( 1.082677165354331228, 0.1660481256975883668, -0.3530559997133364547 ) ) ;
#35798 = CARTESIAN_POINT ( 'NONE',  ( -1.154855643044618851, 0.1283753931104748280, 0.1820866141732283561 ) ) ;
#35799 = DIRECTION ( 'NONE',  ( 0.000000000000000000, 0.000000000000000000, 1.000000000000000000 ) ) ;
#35800 = CARTESIAN_POINT ( 'NONE',  ( 0.2690288713910767848, 0.2952755905511811885, 0.1292274648535926551 ) ) ;
#35801 = CARTESIAN_POINT ( 'NONE',  ( -0.6758530183727028406, 0.2952755905511811885, 0.1292274648535926551 ) ) ;
#35802 = CARTESIAN_POINT ( 'NONE',  ( 0.3917322834645669549, 2.398668435337827645E-17, -1.615466248522622550 ) ) ;
#35803 = CARTESIAN_POINT ( 'NONE',  ( -1.049868766404198794, -0.6046776061558807314, 0.2411417322834647770 ) ) ;
#35804 = FACE_OUTER_BOUND ( 'NONE', #32896, .T. ) ;
#35805 = EDGE_CURVE ( 'NONE', #69360, #83014, #18657, .T. ) ;
#35806 = CARTESIAN_POINT ( 'NONE',  ( 1.102362204724410155, -0.1870078740157480879, -0.4822834645669291653 ) ) ;
#35807 = CARTESIAN_POINT ( 'NONE',  ( -0.2867679344610364334, -0.2867679344610367109, 0.1062992125984252439 ) ) ;
#35808 = CARTESIAN_POINT ( 'NONE',  ( 1.253280839895013710, -0.08942795157528024563, -0.3641732283464568787 ) ) ;
#35809 = ORIENTED_EDGE ( 'NONE', *, *, #42337, .F. ) ;
#35810 = CARTESIAN_POINT ( 'NONE',  ( -0.2891555358219908833, -0.2891555358219912164, 0.09842519685039366473 ) ) ;
#35811 = CARTESIAN_POINT ( 'NONE',  ( -0.3543307086614165824, 0.2952755905511811885, 0.000000000000000000 ) ) ;
#35812 = ORIENTED_EDGE ( 'NONE', *, *, #48506, .F. ) ;
#35814 = AXIS2_PLACEMENT_3D ( 'NONE', #83133, #57850, #38508 ) ;
#35813 = CARTESIAN_POINT ( 'NONE',  ( 0.3543307086614179147, 0.1771653543307087630, 0.000000000000000000 ) ) ;
#35815 = CARTESIAN_POINT ( 'NONE',  ( -1.614173228346456268, -0.6692913385826771977, 8.415575281601705876E-17 ) ) ;
#35816 = CARTESIAN_POINT ( 'NONE',  ( 0.6889763779527563470, 0.1660481256975883668, -0.3530559997133364547 ) ) ;
#35817 = CARTESIAN_POINT ( 'NONE',  ( 0.8923884514435701520, -0.6046776061558809534, -0.2411417322834644161 ) ) ;
#35818 = CARTESIAN_POINT ( 'NONE',  ( -0.08530183727034056085, -0.05778040916215560624, -0.4822834645669293319 ) ) ;
#35819 = CARTESIAN_POINT ( 'NONE',  ( -0.1958661417322836995, 0.3392501089628017219, -1.427184670112547682 ) ) ;
#35820 = CARTESIAN_POINT ( 'NONE',  ( -0.9120734908136475250, -0.6692913385826773087, -0.1292274648535924053 ) ) ;
#35821 = CARTESIAN_POINT ( 'NONE',  ( 0.1049643490035304938, -0.3917322834645669549, -2.217191601049868677 ) ) ;
#35822 = CARTESIAN_POINT ( 'NONE',  ( -1.712598425196849572, 0.1660481256975885056, 0.3530559997133364547 ) ) ;
#35823 = CARTESIAN_POINT ( 'NONE',  ( -1.095800524934382292, -0.3162353388693409650, -0.4822834645669289433 ) ) ;
#35824 = CARTESIAN_POINT ( 'NONE',  ( 1.233595800524935227, 0.2306618581243847221, -0.2411417322834647770 ) ) ;
#35825 = CARTESIAN_POINT ( 'NONE',  ( 1.601049868766404982, -0.6046776061558809534, -0.2411417322834644161 ) ) ;
#35826 = CARTESIAN_POINT ( 'NONE',  ( 0.3996062992125986035, 0.1070741851644054776, -0.4396325459317584339 ) ) ;
#35827 = CARTESIAN_POINT ( 'NONE',  ( -1.017060367454067249, -0.3162353388693409650, -0.4822834645669289433 ) ) ;
#35828 = CARTESIAN_POINT ( 'NONE',  ( 0.3996062992125986035, -0.1070741851644052972, 0.1266404199475065218 ) ) ;
#35829 = CARTESIAN_POINT ( 'NONE',  ( 0.1246719160104994284, -0.6692913385826771977, 0.1292274648535927661 ) ) ;
#35830 = CARTESIAN_POINT ( 'NONE',  ( -0.3996062992125987146, 0.1070741851644051862, -2.237532808398950301 ) ) ;
#35831 = CARTESIAN_POINT ( 'NONE',  ( -0.5643044619422565855, -0.4281496062992124485, 0.4176697321401328655 ) ) ;
#35832 = CARTESIAN_POINT ( 'NONE',  ( -1.594488188976377119, 0.07958543189024071263, -0.2665933059059888421 ) ) ;
#35833 = CARTESIAN_POINT ( 'NONE',  ( 0.7414698162729663755, 0.1771653543307087630, 0.09757992244046791164 ) ) ;
#35834 = CARTESIAN_POINT ( 'NONE',  ( 1.279527559055118724, 0.1660481256975885056, 0.3530559997133364547 ) ) ;
#35835 = CARTESIAN_POINT ( 'NONE',  ( -0.2362204724409451284, 0.4091458600556402425, -1.192257217847769057 ) ) ;
#35836 = CARTESIAN_POINT ( 'NONE',  ( 0.7939632545931766261, -0.2845877964562161244, -0.3641732283464567121 ) ) ;
#35837 = CARTESIAN_POINT ( 'NONE',  ( 0.6627296587926515548, 0.2952755905511811885, 0.1292274648535926551 ) ) ;
#35838 = CARTESIAN_POINT ( 'NONE',  ( -0.1974969037888704149, -0.3420746716998661063, -0.7723097112860893843 ) ) ;
#35839 = CARTESIAN_POINT ( 'NONE',  ( -0.4658792650918627265, -0.05778040916215522460, 0.4822834645669289988 ) ) ;
#35840 = CARTESIAN_POINT ( 'NONE',  ( 0.1938976377952755792, 0.1938976377952755792, 0.1574803149606299191 ) ) ;
#35841 = CARTESIAN_POINT ( 'NONE',  ( 1.325459317585302665, -0.004921259842519870586, -0.3153832671262229437 ) ) ;
#35842 = CARTESIAN_POINT ( 'NONE',  ( -0.5708661417322828946, 0.1660481256975883668, -0.3530559997133364547 ) ) ;
#35843 = CARTESIAN_POINT ( 'NONE',  ( 0.1574803149606306130, -0.1870078740157479769, 0.4822834645669291653 ) ) ;
#35844 = CARTESIAN_POINT ( 'NONE',  ( 0.09151288181857175630, 0.004960608223780119466, 0.3437734562760182411 ) ) ;
#35845 = CARTESIAN_POINT ( 'NONE',  ( -0.03280839895013062252, -0.6692913385826771977, 0.1292274648535927661 ) ) ;
#35846 = CARTESIAN_POINT ( 'NONE',  ( 0.6430446194225729606, -0.3690944881889765550, -0.3153832671262227771 ) ) ;
#35847 = CARTESIAN_POINT ( 'NONE',  ( -0.1539732359166575415, 1.088403462004246425, -1.111533894513872633 ) ) ;
#35848 = CARTESIAN_POINT ( 'NONE',  ( -0.09186351706036663400, -0.3690944881889763329, 0.3153832671262228327 ) ) ;
#35849 = CARTESIAN_POINT ( 'NONE',  ( 0.9317585301837276734, -0.3690944881889763329, 0.3153832671262228327 ) ) ;
#35850 = CARTESIAN_POINT ( 'NONE',  ( -1.082677165354329896, 0.1012011053420777407, 0.2882089793578257453 ) ) ;
#35851 = CARTESIAN_POINT ( 'NONE',  ( -0.3996062992125984925, -0.1070741851644056858, -1.225065616797899937 ) ) ;
#35852 = CARTESIAN_POINT ( 'NONE',  ( 0.7152230971128616943, -0.05778040916215522460, 0.4822834645669289988 ) ) ;
#35853 = AXIS2_PLACEMENT_3D ( 'NONE', #19050, #22996, #49073 ) ;
#35854 = CARTESIAN_POINT ( 'NONE',  ( -0.3917322834645669549, -0.1049643490035306603, -1.140419947506561282 ) ) ;
#35855 = CONICAL_SURFACE ( 'NONE', #884, 1.889763779527559251, 0.7853981633974500554 ) ;
#35856 = AXIS2_PLACEMENT_3D ( 'NONE', #66761, #65514, #8674 ) ;
#35857 = CARTESIAN_POINT ( 'NONE',  ( 0.2258813529811906362, 4.257495641787552160E-16, -0.4281993546915526805 ) ) ;
#35858 = CARTESIAN_POINT ( 'NONE',  ( -0.3902087894128231649, -0.03611438844012619664, 1.721458645558462781E-17 ) ) ;
#35859 = CARTESIAN_POINT ( 'NONE',  ( -0.09186351706036689768, -0.004921259842519870586, -0.3153832671262229437 ) ) ;
#35860 = EDGE_CURVE ( 'NONE', #7002, #39742, #55898, .T. ) ;
#35861 = CARTESIAN_POINT ( 'NONE',  ( 0.1443569553805781891, 0.05413385826771626580, -0.4176697321401330321 ) ) ;
#35862 = CARTESIAN_POINT ( 'NONE',  ( 1.397637795275591177, 0.07958543189024071263, -0.2665933059059888421 ) ) ;
#35863 = CARTESIAN_POINT ( 'NONE',  ( -1.174540682414697335, -0.2845877964562161244, -0.3641732283464567121 ) ) ;
#35864 = CARTESIAN_POINT ( 'NONE',  ( -1.318897637795274802, -0.5400638737290845981, -0.3530559997133363437 ) ) ;
#35865 = CARTESIAN_POINT ( 'NONE',  ( 0.2887139107611556010, 0.2306618581243847221, -0.2411417322834647770 ) ) ;
#35866 = CARTESIAN_POINT ( 'NONE',  ( 1.003937007874016407, -0.5400638737290844871, 0.3530559997133364547 ) ) ;
#35867 = CARTESIAN_POINT ( 'NONE',  ( 1.251578178566641997, 1.420967098491911607, -0.6060014054450971743 ) ) ;
#35868 = CARTESIAN_POINT ( 'NONE',  ( 0.1443569553805781891, -0.4281496062992124485, 0.4176697321401328655 ) ) ;
#35869 = CARTESIAN_POINT ( 'NONE',  ( 1.450131233595801428, -0.6692913385826773087, -0.1292274648535924053 ) ) ;
#35870 = CARTESIAN_POINT ( 'NONE',  ( 1.062992125984252745, 0.2952755905511811885, 0.000000000000000000 ) ) ;
#35871 = CARTESIAN_POINT ( 'NONE',  ( -1.604771003085129433, 2.146987379487327985, -0.1466069496707750608 ) ) ;
#35872 = CARTESIAN_POINT ( 'NONE',  ( 0.7283464566929143125, 0.07958543189024085140, 0.2665933059059887866 ) ) ;
#35873 = CARTESIAN_POINT ( 'NONE',  ( 1.614173228346457378, -0.6692913385826771977, 8.415575281601705876E-17 ) ) ;
#35874 = CARTESIAN_POINT ( 'NONE',  ( 0.06561679790026316017, -0.004921259842519870586, -0.3153832671262229437 ) ) ;
#35875 = CARTESIAN_POINT ( 'NONE',  ( 0.1246719160104994284, 0.2952755905511810774, -0.1292274648535930714 ) ) ;
#35876 = CARTESIAN_POINT ( 'NONE',  ( 0.8727034120734912248, -0.3162353388693409650, -0.4822834645669289433 ) ) ;
#35877 = CARTESIAN_POINT ( 'NONE',  ( -0.4396325459317577122, -0.6692913385826773087, -0.1292274648535924053 ) ) ;
#35878 = CARTESIAN_POINT ( 'NONE',  ( -0.4002624671916004129, -0.08942795157528024563, -0.3641732283464568787 ) ) ;
#35879 = CARTESIAN_POINT ( 'NONE',  ( 0.8398950131233602345, 0.2306618581243847221, -0.2411417322834647770 ) ) ;
#35880 = CARTESIAN_POINT ( 'NONE',  ( 1.036745406824147731, -0.004921259842519576551, 0.3153832671262227771 ) ) ;
#35881 = CYLINDRICAL_SURFACE ( 'NONE', #60811, 1.181102362204724310 ) ;
#35883 = CARTESIAN_POINT ( 'NONE',  ( 0.2925321140481932369, -0.2925321140481931814, -1.043307086614173151 ) ) ;
#35882 = DIRECTION ( 'NONE',  ( 0.000000000000000000, 0.000000000000000000, -1.000000000000000000 ) ) ;
#35884 = CARTESIAN_POINT ( 'NONE',  ( -0.1775461242611900137, 1.063099670987233569, 0.2580608039878784510 ) ) ;
#35885 = CARTESIAN_POINT ( 'NONE',  ( -1.154855643044618851, 0.2306618581243848609, 0.2411417322834645549 ) ) ;
#35886 = CARTESIAN_POINT ( 'NONE',  ( -0.4658792650918627265, -0.05778040916215522460, 0.4822834645669289988 ) ) ;
#35887 = CARTESIAN_POINT ( 'NONE',  ( 0.3458507752293908943, 0.3458507752293908943, 0.01968503937007874335 ) ) ;
#35888 = CARTESIAN_POINT ( 'NONE',  ( -0.1058382717557497937, -0.3949938075777411628, -2.276902887139107712 ) ) ;
#35889 = ORIENTED_EDGE ( 'NONE', *, *, #75955, .T. ) ;
#35890 = CARTESIAN_POINT ( 'NONE',  ( 0.1377952755905518800, 0.07958543189024071263, -0.2665933059059888421 ) ) ;
#35891 = CARTESIAN_POINT ( 'NONE',  ( 0.1049643490035303689, 0.3917322834645670104, -0.9304461942257216123 ) ) ;
#35892 = CARTESIAN_POINT ( 'NONE',  ( 0.9055118110236227702, -0.6692913385826771977, 8.415575281601705876E-17 ) ) ;
#35893 = CARTESIAN_POINT ( 'NONE',  ( -1.157146581871515012E-16, 0.4724409448818898682, -2.519685039370078705 ) ) ;
#35894 = CARTESIAN_POINT ( 'NONE',  ( -0.2362204724409451284, 0.4091458600556402425, -0.8772965879265091083 ) ) ;
#35895 = CARTESIAN_POINT ( 'NONE',  ( -0.5314960629921393620, 2.755905511811024056, 3.821484228344191880 ) ) ;
#35896 = CARTESIAN_POINT ( 'NONE',  ( 1.476377952755906442, -0.5400638737290844871, 0.3530559997133364547 ) ) ;
#35897 = CARTESIAN_POINT ( 'NONE',  ( 1.469816272965879911, 0.1283753931104746893, -0.1820866141732285504 ) ) ;
#35898 = CARTESIAN_POINT ( 'NONE',  ( 0.4002624671916016896, -0.05778040916215522460, 0.4822834645669289988 ) ) ;
#35899 = AXIS2_PLACEMENT_3D ( 'NONE', #18181, #9901, #56045 ) ;
#35900 = CARTESIAN_POINT ( 'NONE',  ( -0.3917322834645670659, 0.1049643490035301607, -0.4278022065278722641 ) ) ;
#35901 = CARTESIAN_POINT ( 'NONE',  ( 0.02624671916010564918, -0.6046776061558809534, -0.2411417322834644161 ) ) ;
#35902 = CARTESIAN_POINT ( 'NONE',  ( -1.069553805774277722, 0.1771653543307087630, 0.09757992244046791164 ) ) ;
#35903 = CARTESIAN_POINT ( 'NONE',  ( 0.2952755905511816326, -0.5400638737290844871, 0.3530559997133364547 ) ) ;
#35904 = CARTESIAN_POINT ( 'NONE',  ( 0.006561679790026889343, -0.05778040916215522460, 0.4822834645669289988 ) ) ;
#35905 =( BOUNDED_CURVE ( )  B_SPLINE_CURVE ( 2, ( #48598, #36390, #68796, #35985, #11558, #29660, #54914, #11141, #62476, #61655, #24167, #49836, #3996, #4811, #62064, #75535, #4403, #30487, #37215, #62894, #18283, #43926, #69622, #35567, #22932, #25812, #46000, #26660, #24980, #77601, #57792, #58213, #38861, #18688, #38033, #57381, #579, #63708, #64542, #45160, #51472, #51896, #32135, #77175, #6465, #37622, #7301, #50654, #63298, #19506, #51060, #32970, #5636, #19090, #38447, #58638, #31303, #44739, #26233, #64131, #78020, #12375, #44331, #70865, #6879, #76356, #1006, #13215, #19935, #70022, #6048, #159, #56967, #31720, #83075, #25396, #32549, #76760, #45584, #70434, #82665, #12791, #11967, #52313, #71277, #13626, #39278, #64965, #20348, #54395, #33809, #65396, #80106, #59887, #72941, #1827, #60718, #14471, #40125, #2241, #22425, #8558, #53979, #8144, #78442, #66634, #67049, #28318, #21590, #53566, #7732, #27906, #72532, #27487, #40540, #79691, #34226, #79275, #66220, #14050, #9382, #35052, #33399, #47252, #15711, #20768, #22008, #15293, #47668, #3067, #40954, #8971, #34645, #60310, #72113, #14880, #41368, #2659, #73362, #28734, #71696, #46421, #59474, #39704, #59061, #1416, #27072, #53145, #46838, #52731, #65811, #78858, #21183, #61552, #16538, #11451, #30791, #3480, #5126, #35883, #67459, #54815, #56457, #29147, #61960, #62792, #4704, #16120, #69103, #3896, #81752, #80517, #55628, #81337, #24063, #35465, #43403, #42183, #73784, #42999, #62366, #49732, #67878, #75431, #41766, #36691, #30377 ),
 .UNSPECIFIED., .F., .F. ) 
 B_SPLINE_CURVE_WITH_KNOTS ( ( 3, 2, 2, 2, 2, 2, 2, 2, 2, 2, 2, 2, 2, 2, 2, 2, 2, 2, 2, 2, 2, 2, 2, 2, 2, 2, 2, 2, 2, 2, 2, 2, 2, 2, 2, 2, 2, 2, 2, 2, 2, 2, 2, 2, 2, 2, 2, 2, 2, 2, 2, 2, 2, 2, 2, 2, 2, 2, 2, 2, 2, 2, 2, 2, 2, 2, 2, 2, 2, 2, 2, 2, 2, 2, 2, 2, 2, 2, 2, 2, 2, 2, 2, 2, 2, 2, 2, 2, 2, 2, 2, 2, 2, 3 ),
 ( 0.05000000000000000278, 0.05416666666666666852, 0.05833333333333333426, 0.06250000000000000000, 0.06666666666666666574, 0.07083333333333333148, 0.07499999999999999722, 0.07916666666666666297, 0.08333333333333332871, 0.08749999999999999445, 0.09166666666666664631, 0.09583333333333333981, 0.1000000000000000056, 0.1041666666666666574, 0.1083333333333333370, 0.1124999999999999889, 0.1166666666666666546, 0.1208333333333333204, 0.1249999999999999861, 0.1291666666666666519, 0.1333333333333333037, 0.1375000000000000111, 0.1416666666666666630, 0.1458333333333333148, 0.1499999999999999667, 0.1541666666666666741, 0.1583333333333333259, 0.1624999999999999778, 0.1666666666666666297, 0.1708333333333333093, 0.1749999999999999611, 0.1791666666666666408, 0.1833333333333332926, 0.1875000000000000000, 0.1916666666666666519, 0.1958333333333333037, 0.2000000000000000111, 0.2041666666666666630, 0.2083333333333333148, 0.2124999999999999667, 0.2166666666666666741, 0.2208333333333333259, 0.2249999999999999778, 0.2291666666666666297, 0.2333333333333333370, 0.2374999999999999889, 0.2416666666666666408, 0.2458333333333332926, 0.2500000000000000000, 0.2541666666666666519, 0.2583333333333333592, 0.2624999999999999556, 0.2666666666666666630, 0.2708333333333333148, 0.2750000000000000222, 0.2791666666666666741, 0.2833333333333333259, 0.2874999999999999223, 0.2916666666666666297, 0.2958333333333333370, 0.2999999999999999889, 0.3041666666666665853, 0.3083333333333332926, 0.3125000000000000000, 0.3166666666666665964, 0.3208333333333333037, 0.3249999999999999556, 0.3291666666666666075, 0.3333333333333332593, 0.3374999999999999667, 0.3416666666666666741, 0.3458333333333332704, 0.3499999999999999223, 0.3541666666666666297, 0.3583333333333332815, 0.3624999999999999334, 0.3666666666666665853, 0.3708333333333332926, 0.3749999999999999445, 0.3791666666666665964, 0.3833333333333333592, 0.3874999999999999556, 0.3916666666666666075, 0.3958333333333333148, 0.3999999999999999667, 0.4041666666666666186, 0.4083333333333332149, 0.4124999999999999223, 0.4166666666666666852, 0.4208333333333332815, 0.4249999999999999334, 0.4291666666666665853, 0.4333333333333332926, 0.4374999999999999445 ),
 .UNSPECIFIED. ) 
 CURVE ( )  GEOMETRIC_REPRESENTATION_ITEM ( )  RATIONAL_B_SPLINE_CURVE ( ( 1.000000000000000000, 0.9659258262890683122, 1.000000000000000000, 0.9659258262890683122, 1.000000000000000000, 0.9659258262890683122, 1.000000000000000000, 0.9659258262890683122, 1.000000000000000000, 0.9659258262890683122, 1.000000000000000000, 0.9659258262890683122, 1.000000000000000000, 0.9659258262890683122, 1.000000000000000000, 0.9659258262890683122, 1.000000000000000000, 0.9659258262890683122, 1.000000000000000000, 0.9659258262890683122, 1.000000000000000000, 0.9659258262890683122, 1.000000000000000000, 0.9659258262890683122, 1.000000000000000000, 0.9659258262890683122, 1.000000000000000000, 0.9659258262890683122, 1.000000000000000000, 0.9659258262890683122, 1.000000000000000000, 0.9659258262890683122, 1.000000000000000000, 0.9659258262890683122, 1.000000000000000000, 0.9659258262890683122, 1.000000000000000000, 0.9659258262890683122, 1.000000000000000000, 0.9659258262890683122, 1.000000000000000000, 0.9659258262890683122, 1.000000000000000000, 0.9659258262890683122, 1.000000000000000000, 0.9659258262890683122, 1.000000000000000000, 0.9659258262890683122, 1.000000000000000000, 0.9659258262890683122, 1.000000000000000000, 0.9659258262890683122, 1.000000000000000000, 0.9659258262890683122, 1.000000000000000000, 0.9659258262890683122, 1.000000000000000000, 0.9659258262890683122, 1.000000000000000000, 0.9659258262890683122, 1.000000000000000000, 0.9659258262890683122, 1.000000000000000000, 0.9659258262890683122, 1.000000000000000000, 0.9659258262890683122, 1.000000000000000000, 0.9659258262890683122, 1.000000000000000000, 0.9659258262890683122, 1.000000000000000000, 0.9659258262890683122, 1.000000000000000000, 0.9659258262890683122, 1.000000000000000000, 0.9659258262890683122, 1.000000000000000000, 0.9659258262890683122, 1.000000000000000000, 0.9659258262890683122, 1.000000000000000000, 0.9659258262890683122, 1.000000000000000000, 0.9659258262890683122, 1.000000000000000000, 0.9659258262890683122, 1.000000000000000000, 0.9659258262890683122, 1.000000000000000000, 0.9659258262890683122, 1.000000000000000000, 0.9659258262890683122, 1.000000000000000000, 0.9659258262890683122, 1.000000000000000000, 0.9659258262890683122, 1.000000000000000000, 0.9659258262890683122, 1.000000000000000000, 0.9659258262890683122, 1.000000000000000000, 0.9659258262890683122, 1.000000000000000000, 0.9659258262890683122, 1.000000000000000000, 0.9659258262890683122, 1.000000000000000000, 0.9659258262890683122, 1.000000000000000000, 0.9659258262890683122, 1.000000000000000000, 0.9659258262890683122, 1.000000000000000000, 0.9659258262890683122, 1.000000000000000000, 0.9659258262890683122, 1.000000000000000000, 0.9659258262890683122, 1.000000000000000000, 0.9659258262890683122, 1.000000000000000000, 0.9659258262890683122, 1.000000000000000000, 0.9659258262890683122, 1.000000000000000000, 0.9659258262890683122, 1.000000000000000000, 0.9659258262890683122, 1.000000000000000000, 0.9659258262890683122, 1.000000000000000000, 0.9659258262890683122, 1.000000000000000000, 0.9659258262890683122, 1.000000000000000000, 0.9659258262890683122, 1.000000000000000000, 0.9659258262890683122, 1.000000000000000000, 0.9659258262890683122, 1.000000000000000000, 0.9659258262890683122, 1.000000000000000000, 0.9659258262890683122, 1.000000000000000000, 0.9659258262890683122, 1.000000000000000000, 0.9659258262890683122, 1.000000000000000000, 0.9659258262890683122, 1.000000000000000000, 0.9659258262890683122, 1.000000000000000000, 0.9659258262890683122, 1.000000000000000000, 0.9659258262890683122, 1.000000000000000000, 0.9659258262890683122, 1.000000000000000000, 0.9659258262890683122, 1.000000000000000000, 0.9659258262890683122, 1.000000000000000000, 0.9659258262890683122, 1.000000000000000000, 0.9659258262890683122, 1.000000000000000000, 0.9659258262890683122, 1.000000000000000000, 0.9659258262890683122, 1.000000000000000000, 0.9659258262890683122, 1.000000000000000000, 0.9659258262890683122, 1.000000000000000000, 0.9659258262890683122, 1.000000000000000000, 0.9659258262890683122, 1.000000000000000000, 0.9659258262890683122, 1.000000000000000000, 0.9659258262890683122, 1.000000000000000000, 0.9659258262890683122, 1.000000000000000000, 0.9659258262890687563, 0.9999999999999995559 ) ) 
 REPRESENTATION_ITEM ( '' )  );
#35906 = CARTESIAN_POINT ( 'NONE',  ( 0.4855643044619428750, 0.05413385826771666132, 0.4176697321401328100 ) ) ;
#35907 = VECTOR ( 'NONE', #2101, 39.37007874015748854 ) ;
#35908 = CARTESIAN_POINT ( 'NONE',  ( 0.4102808022082901629, 1.299212598425196985, -1.736178228450289573 ) ) ;
#35909 = CARTESIAN_POINT ( 'NONE',  ( -0.1049643490035302301, -0.3917322834645671770, -1.486239788222784020 ) ) ;
#35910 = CARTESIAN_POINT ( 'NONE',  ( 0.7414698162729663755, 0.2952755905511811885, 0.1292274648535926551 ) ) ;
#35911 = CIRCLE ( 'NONE', #57385, 0.09842519685039372024 ) ;
#35912 = CARTESIAN_POINT ( 'NONE',  ( -0.2493438320209966919, 0.05413385826771626580, -0.4176697321401330321 ) ) ;
#35913 = CARTESIAN_POINT ( 'NONE',  ( -1.148293963254592542, 0.2952755905511811885, 0.1292274648535926551 ) ) ;
#35914 = CARTESIAN_POINT ( 'NONE',  ( 1.062992125984252745, -0.6692913385826771977, 8.415575281601705876E-17 ) ) ;
#35915 = CARTESIAN_POINT ( 'NONE',  ( 0.5905511811023629321, 0.2952755905511811885, 0.000000000000000000 ) ) ;
#35916 = CARTESIAN_POINT ( 'NONE',  ( -0.1958661417322834220, -0.3392501089628018884, -1.095144356955380704 ) ) ;
#35917 = CARTESIAN_POINT ( 'NONE',  ( -0.5511811023622041894, -0.1870078740157480879, -0.4822834645669291653 ) ) ;
#35918 = CARTESIAN_POINT ( 'NONE',  ( 0.3412073490813655186, -0.6046776061558809534, -0.2411417322834644161 ) ) ;
#35919 = CARTESIAN_POINT ( 'NONE',  ( -0.5446194225721777693, -0.05778040916215522460, 0.4822834645669289988 ) ) ;
#35920 = CARTESIAN_POINT ( 'NONE',  ( 0.3477690288713918276, -0.5511811023622048555, -0.09757992244046775898 ) ) ;
#35921 = CARTESIAN_POINT ( 'NONE',  ( -1.594488188976377563, -0.5400638737290844871, 0.3530559997133364547 ) ) ;
#35922 = CARTESIAN_POINT ( 'NONE',  ( -1.719160104986876103, 0.05413385826771666132, 0.4176697321401328100 ) ) ;
#35923 = CARTESIAN_POINT ( 'NONE',  ( 0.3149606299212603933, -0.1870078740157479769, 0.4822834645669291653 ) ) ;
#35924 = CARTESIAN_POINT ( 'NONE',  ( 1.384514435695538337, -0.6692913385826771977, 0.1292274648535927661 ) ) ;
#35925 = CARTESIAN_POINT ( 'NONE',  ( -0.3917322834645670104, -7.196005306013484475E-17, -2.551181102362204633 ) ) ;
#35926 = ORIENTED_EDGE ( 'NONE', *, *, #52272, .T. ) ;
#35927 = ORIENTED_EDGE ( 'NONE', *, *, #50646, .T. ) ;
#35928 = CARTESIAN_POINT ( 'NONE',  ( 0.7283464566929143125, 0.1660481256975885056, 0.3530559997133364547 ) ) ;
#35929 = CARTESIAN_POINT ( 'NONE',  ( 0.7480314960629927956, -0.5511811023622047445, 6.969142054262312111E-17 ) ) ;
#35931 = DIRECTION ( 'NONE',  ( 1.000000000000000000, 3.469446951953613203E-16, 0.000000000000000000 ) ) ;
#35930 = CARTESIAN_POINT ( 'NONE',  ( -1.019850064477911600, 1.617462848879257731, 0.4678763946775361671 ) ) ;
#35932 = CARTESIAN_POINT ( 'NONE',  ( -0.3392501089628019995, 0.1958661417322832277, -0.7408136482939633449 ) ) ;
#35933 = CARTESIAN_POINT ( 'NONE',  ( 0.4606732211678803424, 1.778019097314518016, -0.5309055118110237448 ) ) ;
#35934 = CARTESIAN_POINT ( 'NONE',  ( 0.3969271875946612238, 0.02899565511876848675, -1.929133858267718660 ) ) ;
#35935 = CARTESIAN_POINT ( 'NONE',  ( 0.1070741851644054776, -0.3996062992125984925, -2.524278215223096478 ) ) ;
#35936 = CARTESIAN_POINT ( 'NONE',  ( 0.8136482939632553313, 0.2306618581243848609, 0.2411417322834645549 ) ) ;
#35937 = CARTESIAN_POINT ( 'NONE',  ( -0.8595800524934373854, -0.05778040916215522460, 0.4822834645669289988 ) ) ;
#35938 = CARTESIAN_POINT ( 'NONE',  ( -0.5905511811023615998, 0.2952755905511811885, 0.000000000000000000 ) ) ;
#35939 = CARTESIAN_POINT ( 'NONE',  ( 0.7677165354330716118, -0.5400638737290844871, 0.3530559997133364547 ) ) ;
#35940 = CARTESIAN_POINT ( 'NONE',  ( 1.345144356955381593, -0.3162353388693409650, -0.4822834645669289433 ) ) ;
#35941 = CARTESIAN_POINT ( 'NONE',  ( -1.018296575816956206, 1.474731146291503148, 0.4712826680561278958 ) ) ;
#35942 = CARTESIAN_POINT ( 'NONE',  ( 1.443569553805774897, -0.5023911411419708095, -0.1820866141732282451 ) ) ;
#35943 = CARTESIAN_POINT ( 'NONE',  ( 1.614173228346456712, 2.401574803149606474, -0.1372047244094476703 ) ) ;
#35944 = CARTESIAN_POINT ( 'NONE',  ( -1.325459317585300889, -0.004921259842519576551, 0.3153832671262227771 ) ) ;
#35945 = CARTESIAN_POINT ( 'NONE',  ( -2.787279214012418738, 2.362204724409448620, 0.000000000000000000 ) ) ;
#35946 = CARTESIAN_POINT ( 'NONE',  ( 0.05905511811023709395, -0.5400638737290844871, 0.3530559997133364547 ) ) ;
#35948 = DIRECTION ( 'NONE',  ( -0.000000000000000000, 1.000000000000000000, -0.000000000000000000 ) ) ;
#35947 = CARTESIAN_POINT ( 'NONE',  ( 1.174540682414699111, -0.3162353388693405765, 0.4822834645669290543 ) ) ;
#35949 = CARTESIAN_POINT ( 'NONE',  ( -1.167979002624671470, -0.3690944881889765550, -0.3153832671262227771 ) ) ;
#35950 = CARTESIAN_POINT ( 'NONE',  ( 0.3805774278215230400, -0.4281496062992124485, 0.4176697321401328655 ) ) ;
#35951 = CARTESIAN_POINT ( 'NONE',  ( 1.174540682414699111, -0.08942795157528024563, -0.3641732283464568787 ) ) ;
#35952 = EDGE_CURVE ( 'NONE', #41264, #66355, #18911, .T. ) ;
#35953 = CARTESIAN_POINT ( 'NONE',  ( -0.1958661417322836440, 0.3392501089628016664, -1.667959686842832356 ) ) ;
#35954 = CARTESIAN_POINT ( 'NONE',  ( -1.043307086614172707, 0.07958543189024071263, -0.2665933059059888421 ) ) ;
#35955 = CARTESIAN_POINT ( 'NONE',  ( 1.450131233595801428, -0.6692913385826773087, -0.1292274648535924053 ) ) ;
#35956 = DIRECTION ( 'NONE',  ( 0.000000000000000000, -1.000000000000000000, -0.000000000000000000 ) ) ;
#35957 = CARTESIAN_POINT ( 'NONE',  ( 0.07217847769028949700, -0.08942795157528024563, -0.3641732283464568787 ) ) ;
#35958 = CARTESIAN_POINT ( 'NONE',  ( -0.1574803149606292529, -0.1870078740157479769, 0.4822834645669291653 ) ) ;
#35959 = CARTESIAN_POINT ( 'NONE',  ( -1.194225721784776262, -0.3690944881889763329, 0.3153832671262228327 ) ) ;
#35960 = CARTESIAN_POINT ( 'NONE',  ( -0.8923884514435688198, 0.2306618581243847221, -0.2411417322834647770 ) ) ;
#35961 = CARTESIAN_POINT ( 'NONE',  ( 1.646981627296588035, -0.3162353388693405765, 0.4822834645669290543 ) ) ;
#35962 = CARTESIAN_POINT ( 'NONE',  ( -0.1049643490035302301, -0.3917322834645671770, -0.3838775834983745860 ) ) ;
#35963 = CARTESIAN_POINT ( 'NONE',  ( 0.000000000000000000, 2.185078740157480937, 0.2362204724409449064 ) ) ;
#35964 = CARTESIAN_POINT ( 'NONE',  ( 1.614173228346457378, 0.2952755905511811885, 0.000000000000000000 ) ) ;
#35965 = CARTESIAN_POINT ( 'NONE',  ( -0.1265901696524993347, 0.4724409448818895907, -1.973097112860892510 ) ) ;
#35966 = CARTESIAN_POINT ( 'NONE',  ( -1.404199475065615932, 0.05413385826771666132, 0.4176697321401328100 ) ) ;
#35967 = CARTESIAN_POINT ( 'NONE',  ( -1.207349081364828436, -0.5023911411419708095, 0.1820866141732285504 ) ) ;
#35968 = CARTESIAN_POINT ( 'NONE',  ( -0.7545931758530177724, 0.1771653543307087630, 0.09757992244046791164 ) ) ;
#35969 = CARTESIAN_POINT ( 'NONE',  ( -1.653543307086613234, -0.1870078740157479769, 0.4822834645669291653 ) ) ;
#35970 = CARTESIAN_POINT ( 'NONE',  ( 0.2034120734908144990, -0.6692913385826771977, 0.1292274648535927661 ) ) ;
#35971 = CARTESIAN_POINT ( 'NONE',  ( 0.3871391076115493490, -0.2845877964562159024, 0.3641732283464567677 ) ) ;
#35972 = CARTESIAN_POINT ( 'NONE',  ( -1.213910761154854745, 0.1771653543307087075, -0.09757992244046823083 ) ) ;
#35973 = CARTESIAN_POINT ( 'NONE',  ( -1.299212598425196097, -0.6692913385826771977, 8.415575281601705876E-17 ) ) ;
#35974 = CARTESIAN_POINT ( 'NONE',  ( 1.227034120734908917, -0.5511811023622046335, 0.09757992244046803654 ) ) ;
#35975 = CARTESIAN_POINT ( 'NONE',  ( 1.404199475065617708, 0.05413385826771626580, -0.4176697321401330321 ) ) ;
#35976 = CARTESIAN_POINT ( 'NONE',  ( 0.4741693035498537601, 1.520070061304626075, 2.169550896612808977 ) ) ;
#35977 = CARTESIAN_POINT ( 'NONE',  ( 0.6364829396325465405, -0.2845877964562161244, -0.3641732283464567121 ) ) ;
#35978 = CARTESIAN_POINT ( 'NONE',  ( 0.9711286089238851948, -0.6046776061558809534, -0.2411417322834644161 ) ) ;
#35979 = LINE ( 'NONE', #50130, #39404 ) ;
#35980 = CARTESIAN_POINT ( 'NONE',  ( 0.9645669291338588858, 0.07958543189024085140, 0.2665933059059887866 ) ) ;
#35981 = EDGE_LOOP ( 'NONE', ( #69849, #66962, #24923 ) ) ;
#35982 = CARTESIAN_POINT ( 'NONE',  ( -1.318897637795274802, 0.1660481256975885056, 0.3530559997133364547 ) ) ;
#35983 = CARTESIAN_POINT ( 'NONE',  ( -0.7217847769028863381, -0.4281496062992124485, 0.4176697321401328655 ) ) ;
#35984 = CARTESIAN_POINT ( 'NONE',  ( -0.1509186351706028884, -0.05778040916215522460, 0.4822834645669289988 ) ) ;
#35985 = CARTESIAN_POINT ( 'NONE',  ( -0.2925321140481932369, 0.2925321140481931814, -0.01968503937007875723 ) ) ;
#35986 = CARTESIAN_POINT ( 'NONE',  ( -0.3460692066303957537, -0.1998031496062994405, -2.333989501312335957 ) ) ;
#35987 = CARTESIAN_POINT ( 'NONE',  ( 0.9120734908136489683, -0.6692913385826771977, 0.1292274648535927661 ) ) ;
#35988 = CARTESIAN_POINT ( 'NONE',  ( 1.417322834645670104, -0.1870078740157479769, 0.3641732283464567677 ) ) ;
#35989 = CARTESIAN_POINT ( 'NONE',  ( -0.07217847769028787330, -0.05778040916215522460, 0.4822834645669289988 ) ) ;
#35990 = CARTESIAN_POINT ( 'NONE',  ( 0.7414698162729663755, -0.6692913385826773087, -0.1292274648535924053 ) ) ;
#35991 = CARTESIAN_POINT ( 'NONE',  ( 0.1070741851644054915, -0.3996062992125986035, -1.660104986876640210 ) ) ;
#35992 = CARTESIAN_POINT ( 'NONE',  ( 0.1974969037888704704, 0.3420746716998660508, -0.9317585301837268963 ) ) ;
#35993 = CARTESIAN_POINT ( 'NONE',  ( 0.3996062992125986590, -0.1070741851644053111, -2.473753280839894764 ) ) ;
#35994 = CARTESIAN_POINT ( 'NONE',  ( -1.033630966599879297, -2.567464376874931580E-15, -0.4445507791589072832 ) ) ;
#35995 = CARTESIAN_POINT ( 'NONE',  ( -0.3392501089628017219, -0.1958661417322836718, -0.04461942257217842850 ) ) ;
#35996 = CARTESIAN_POINT ( 'NONE',  ( -0.2755905511811018171, 0.1771653543307087630, 0.000000000000000000 ) ) ;
#35997 = CARTESIAN_POINT ( 'NONE',  ( -0.8267716535433065062, -0.6692913385826771977, 8.415575281601705876E-17 ) ) ;
#35998 = CARTESIAN_POINT ( 'NONE',  ( 0.9383202099737536495, -0.3162353388693405765, 0.4822834645669290543 ) ) ;
#35999 = CARTESIAN_POINT ( 'NONE',  ( -0.1974969037888704149, -0.3420746716998661063, -2.032152230971128848 ) ) ;
#36000 = CARTESIAN_POINT ( 'NONE',  ( -0.5380577427821514602, -0.004921259842519576551, 0.3153832671262227771 ) ) ;
#36001 = CARTESIAN_POINT ( 'NONE',  ( 1.587926509186352142, 0.05413385826771666132, 0.4176697321401328100 ) ) ;
#36002 = CARTESIAN_POINT ( 'NONE',  ( 1.062992125984252745, -0.6692913385826771977, 8.415575281601705876E-17 ) ) ;
#36003 = CARTESIAN_POINT ( 'NONE',  ( -0.4724409448818895907, -0.1265901696524993070, -2.408136482939632561 ) ) ;
#36004 = CARTESIAN_POINT ( 'NONE',  ( -0.3460692066303960868, 0.1998031496062990242, -1.601049868766404094 ) ) ;
#36005 = CARTESIAN_POINT ( 'NONE',  ( 1.148293963254593653, 0.2952755905511810219, -0.1292274648535930437 ) ) ;
#36006 = ORIENTED_EDGE ( 'NONE', *, *, #49134, .T. ) ;
#36007 = CARTESIAN_POINT ( 'NONE',  ( 1.200787401574803681, -0.5400638737290845981, -0.3530559997133363437 ) ) ;
#36008 = CARTESIAN_POINT ( 'NONE',  ( 1.122047244094488860, 0.07958543189024085140, 0.2665933059059887866 ) ) ;
#36010 = CARTESIAN_POINT ( 'NONE',  ( -1.469816272965878357, 0.2306618581243848609, 0.2411417322834645549 ) ) ;
#36009 = CARTESIAN_POINT ( 'NONE',  ( -1.574803149606298192, -0.1870078740157480601, -0.3641732283464567677 ) ) ;
#36011 = CARTESIAN_POINT ( 'NONE',  ( 0.2867679344610365999, 0.2867679344610365999, 0.09251968503937001154 ) ) ;
#36012 = CARTESIAN_POINT ( 'NONE',  ( 0.9776902887139113929, -0.6692913385826773087, -0.1292274648535924053 ) ) ;
#36013 = CARTESIAN_POINT ( 'NONE',  ( -1.482939632545930975, -0.4281496062992127816, -0.4176697321401328100 ) ) ;
#36014 = CARTESIAN_POINT ( 'NONE',  ( -0.5380577427821514602, -0.4281496062992127816, -0.4176697321401328100 ) ) ;
#36015 = CARTESIAN_POINT ( 'NONE',  ( -0.3740157480314953431, -0.5400638737290845981, -0.3530559997133363437 ) ) ;
#36016 = CARTESIAN_POINT ( 'NONE',  ( 1.476377952755906220, 0.1660481256975883668, -0.3530559997133364547 ) ) ;
#36017 = CARTESIAN_POINT ( 'NONE',  ( -0.2867679344610365999, 0.2867679344610364889, 0.05314960629921249707 ) ) ;
#36018 = CARTESIAN_POINT ( 'NONE',  ( 0.2559055118110243332, -0.5400638737290845981, -0.3530559997133363437 ) ) ;
#36019 = CARTESIAN_POINT ( 'NONE',  ( -0.1958661417322834220, -0.3392501089628018884, -2.419947506561679784 ) ) ;
#36020 = CARTESIAN_POINT ( 'NONE',  ( -1.555118110236219930, -0.4536011799217368745, -0.2665933059059886201 ) ) ;
#36021 = VERTEX_POINT ( 'NONE', #19062 ) ;
#36022 = CARTESIAN_POINT ( 'NONE',  ( -0.2891555358219911054, 0.2891555358219909388, -2.854330708661418026 ) ) ;
#36023 = VERTEX_POINT ( 'NONE', #12763 ) ;
#36024 = CARTESIAN_POINT ( 'NONE',  ( -0.06632061457837669372, -2.294479370626195693E-15, 0.3464511005275217603 ) ) ;
#36025 = CARTESIAN_POINT ( 'NONE',  ( -1.358267716535432434, 0.1660481256975883668, -0.3530559997133364547 ) ) ;
#36026 = CARTESIAN_POINT ( 'NONE',  ( -0.1070741851644051862, -0.3996062992125987146, -0.8595800524934383846 ) ) ;
#36027 = DIRECTION ( 'NONE',  ( -0.8660254037844432595, 0.000000000000000000, 0.4999999999999918954 ) ) ;
#36028 = CARTESIAN_POINT ( 'NONE',  ( 0.002674255378541693599, -0.3979867861068596691, -2.755905511811025388 ) ) ;
#36029 = CARTESIAN_POINT ( 'NONE',  ( -9.594673741351313045E-17, 0.3917322834645670104, -0.5570866141732284671 ) ) ;
#36030 = CARTESIAN_POINT ( 'NONE',  ( -0.5249343832020990641, 0.1283753931104748280, 0.1820866141732283561 ) ) ;
#36031 = CARTESIAN_POINT ( 'NONE',  ( -1.174540682414697335, -0.2845877964562161244, -0.3641732283464567121 ) ) ;
#36032 = CARTESIAN_POINT ( 'NONE',  ( -1.561679790026246017, -0.4281496062992127816, -0.4176697321401328100 ) ) ;
#36033 = CARTESIAN_POINT ( 'NONE',  ( 0.7283464566929140904, -0.5400638737290845981, -0.3530559997133363437 ) ) ;
#36034 = CARTESIAN_POINT ( 'NONE',  ( -1.502624671916009680, -0.3162353388693405765, 0.4822834645669290543 ) ) ;
#36035 = CARTESIAN_POINT ( 'NONE',  ( 0.3392501089628018884, -0.1958661417322834220, -0.2545931758530183275 ) ) ;
#36036 = EDGE_LOOP ( 'NONE', ( #45509, #27624, #71790, #11909, #72441, #42429 ) ) ;
#36037 = B_SPLINE_CURVE_WITH_KNOTS ( 'NONE', 3,
 ( #67743, #59747, #35740, #14745 ),
 .UNSPECIFIED., .F., .F.,
 ( 4, 4 ),
 ( 0.000000000000000000, 0.001493228121701133202 ),
 .UNSPECIFIED. ) ;
#36038 = CARTESIAN_POINT ( 'NONE',  ( -1.463254593175852492, 0.2952755905511811885, 0.1292274648535926551 ) ) ;
#36039 = CYLINDRICAL_SURFACE ( 'NONE', #60866, 0.4724409448818898682 ) ;
#36040 = LENGTH_MEASURE_WITH_UNIT ( LENGTH_MEASURE( 0.02539999999999999897 ), #35627 );
#36041 = CARTESIAN_POINT ( 'NONE',  ( 0.4724409448818897572, -0.1265901696524988906, -1.686351706036745446 ) ) ;
#36042 = CARTESIAN_POINT ( 'NONE',  ( 0.1830245018656607436, 0.2318981092368783414, 0.1465342031617538343 ) ) ;
#36043 = EDGE_CURVE ( 'NONE', #37754, #60631, #17440, .T. ) ;
#36044 = CARTESIAN_POINT ( 'NONE',  ( 0.3149606299212736049, 2.755905511811024056, -3.924389226575467404 ) ) ;
#36045 = CARTESIAN_POINT ( 'NONE',  ( -0.8464566929133852113, 0.1660481256975885056, 0.3530559997133364547 ) ) ;
#36046 = CARTESIAN_POINT ( 'NONE',  ( 1.305774278215223960, -0.6692913385826771977, 0.1292274648535927661 ) ) ;
#36048 = CARTESIAN_POINT ( 'NONE',  ( -1.603475055217291612, 1.606158680897942670, -0.04573490813648262154 ) ) ;
#36047 = CARTESIAN_POINT ( 'NONE',  ( -1.607611548556429737, -0.6692913385826771977, 0.1292274648535927661 ) ) ;
#36049 = CARTESIAN_POINT ( 'NONE',  ( -1.719160104986876103, 0.05413385826771666132, 0.4176697321401328100 ) ) ;
#36050 = CARTESIAN_POINT ( 'NONE',  ( -0.6233595800524928121, -0.05778040916215522460, 0.4822834645669289988 ) ) ;
#36052 = B_SPLINE_CURVE_WITH_KNOTS ( 'NONE', 3,
 ( #52103, #51684, #31928, #25192, #83280, #45376, #57590 ),
 .UNSPECIFIED., .F., .F.,
 ( 4, 3, 4 ),
 ( 1.734723475976807094E-18, 0.001246232571205225159, 0.002492492258783242029 ),
 .UNSPECIFIED. ) ;
#36051 = CARTESIAN_POINT ( 'NONE',  ( -0.3917322834645670659, 0.1049643490035301607, 0.2021190533146474677 ) ) ;
#36053 = CARTESIAN_POINT ( 'NONE',  ( 0.1706036745406830368, -0.004921259842519576551, 0.3153832671262227771 ) ) ;
#36054 = CARTESIAN_POINT ( 'NONE',  ( -0.3392501089628019995, 0.1958661417322832277, -0.4258530183727035068 ) ) ;
#36055 = CARTESIAN_POINT ( 'NONE',  ( 0.09842519685039434474, 0.07958543189024085140, 0.2665933059059887866 ) ) ;
#36056 = CARTESIAN_POINT ( 'NONE',  ( 1.095800524934383846, -0.2845877964562159024, 0.3641732283464567677 ) ) ;
#36057 = CARTESIAN_POINT ( 'NONE',  ( 0.3608923884514443348, 0.2952755905511810774, -0.1292274648535930714 ) ) ;
#36058 = CARTESIAN_POINT ( 'NONE',  ( -0.3149606299212590610, -0.1870078740157480601, -0.3641732283464567677 ) ) ;
#36059 = CARTESIAN_POINT ( 'NONE',  ( -0.3917322834645669549, -0.1049643490035306603, -2.242782152230970993 ) ) ;
#36060 = CARTESIAN_POINT ( 'NONE',  ( 1.535433070866142335, -0.6692913385826771977, 8.415575281601705876E-17 ) ) ;
#36061 = CARTESIAN_POINT ( 'NONE',  ( -0.8792650918635160906, -0.4281496062992124485, 0.4176697321401328655 ) ) ;
#36062 = CARTESIAN_POINT ( 'NONE',  ( 0.4091458600556403535, 0.2362204724409449896, -0.6804461942257218343 ) ) ;
#36063 = CARTESIAN_POINT ( 'NONE',  ( 0.1443569553805781891, -0.4281496062992124485, 0.4176697321401328655 ) ) ;
#36064 = CARTESIAN_POINT ( 'NONE',  ( -0.5052493438320203589, 0.2952755905511810774, -0.1292274648535930714 ) ) ;
#36065 = CARTESIAN_POINT ( 'NONE',  ( 1.574803149606299746, -0.1870078740157480601, -0.3641732283464567677 ) ) ;
#36066 = CARTESIAN_POINT ( 'NONE',  ( 0.08530183727034192087, -0.2845877964562161244, -0.3641732283464567121 ) ) ;
#36067 = CARTESIAN_POINT ( 'NONE',  ( -0.2755905511811018171, 0.2952755905511811885, 0.000000000000000000 ) ) ;
#36068 = CARTESIAN_POINT ( 'NONE',  ( -0.8136482939632537770, 0.2306618581243847221, -0.2411417322834647770 ) ) ;
#36069 = CARTESIAN_POINT ( 'NONE',  ( 3.210901142567240907, 2.729659900128873495, -0.5314960629921260393 ) ) ;
#36070 = CARTESIAN_POINT ( 'NONE',  ( 0.4091458600556403535, 0.2362204724409449896, -0.2887139107611548794 ) ) ;
#36071 = CARTESIAN_POINT ( 'NONE',  ( 0.1771653543307093182, -0.5400638737290845981, -0.3530559997133363437 ) ) ;
#36072 = ORIENTED_EDGE ( 'NONE', *, *, #8432, .F. ) ;
#36073 = B_SPLINE_CURVE_WITH_KNOTS ( 'NONE', 3,
 ( #38574, #704, #33101, #77727, #57507, #25940, #64255, #19214, #8268, #51599 ),
 .UNSPECIFIED., .F., .F.,
 ( 4, 2, 2, 2, 4 ),
 ( 0.000000000000000000, 0.001551611299846697867, 0.002327416949770047885, 0.002715319774731723545, 0.003103222599693399204 ),
 .UNSPECIFIED. ) ;
#36074 = CARTESIAN_POINT ( 'NONE',  ( -0.3996062992125984925, -0.1070741851644056858, -2.169947506561679340 ) ) ;
#36075 = CARTESIAN_POINT ( 'NONE',  ( 1.417322834645670104, -0.1870078740157479769, 0.4822834645669291653 ) ) ;
#36076 = CARTESIAN_POINT ( 'NONE',  ( -0.5314960629921254842, -0.4536011799217368745, -0.2665933059059886201 ) ) ;
#36077 = CARTESIAN_POINT ( 'NONE',  ( -0.4855643044619415427, -0.4281496062992124485, 0.4176697321401328655 ) ) ;
#36078 = CARTESIAN_POINT ( 'NONE',  ( 1.384514435695538559, 0.2952755905511810774, -0.1292274648535930714 ) ) ;
#36079 = CARTESIAN_POINT ( 'NONE',  ( 1.174540682414699111, -0.3162353388693405765, 0.4822834645669290543 ) ) ;
#36080 = CARTESIAN_POINT ( 'NONE',  ( -1.601049868766403650, 0.2306618581243847221, -0.2411417322834647770 ) ) ;
#36081 = CARTESIAN_POINT ( 'NONE',  ( -0.9251968503937002541, 0.07958543189024085140, 0.2665933059059887866 ) ) ;
#36082 = CARTESIAN_POINT ( 'NONE',  ( -0.3460692066303960313, 0.1998031496062989965, -0.4179790026246719137 ) ) ;
#36083 = CARTESIAN_POINT ( 'NONE',  ( -0.3996062992125987146, 0.1070741851644051862, -0.5052493438320209140 ) ) ;
#36084 = CARTESIAN_POINT ( 'NONE',  ( 0.3917322834645670659, -0.1049643490035303273, -2.942932701608610646 ) ) ;
#36085 = CARTESIAN_POINT ( 'NONE',  ( 1.679790026246720025, 0.1283753931104748280, 0.1820866141732283561 ) ) ;
#36086 = CARTESIAN_POINT ( 'NONE',  ( 1.135170603674541256, 0.1771653543307087630, 0.09757992244046791164 ) ) ;
#36087 = CARTESIAN_POINT ( 'NONE',  ( 0.8333333333333340365, 0.2952755905511810774, -0.1292274648535930714 ) ) ;
#36088 = CARTESIAN_POINT ( 'NONE',  ( -1.646981627296586703, -0.3162353388693409650, -0.4822834645669289433 ) ) ;
#36089 = CARTESIAN_POINT ( 'NONE',  ( 0.9580052493438326877, 0.05413385826771666132, 0.4176697321401328100 ) ) ;
#36090 = CARTESIAN_POINT ( 'NONE',  ( -0.1058382717557503072, 0.3949938075777408852, -1.028215223097112885 ) ) ;
#36091 = CARTESIAN_POINT ( 'NONE',  ( 1.233595800524935227, 0.1283753931104746893, -0.1820866141732285504 ) ) ;
#36092 = CARTESIAN_POINT ( 'NONE',  ( 0.2887139107611556010, 0.2306618581243847221, -0.2411417322834647770 ) ) ;
#36093 = CARTESIAN_POINT ( 'NONE',  ( -0.9776902887139098386, 0.2952755905511810774, -0.1292274648535930714 ) ) ;
#36094 = CARTESIAN_POINT ( 'NONE',  ( 1.213910761154856299, 0.2952755905511811885, 0.1292274648535926551 ) ) ;
#36095 = CARTESIAN_POINT ( 'NONE',  ( -0.4091458600556402980, -0.2362204724409451284, -1.154855643044619518 ) ) ;
#36096 = CARTESIAN_POINT ( 'NONE',  ( 0.3996062992125986035, 2.446882876249141962E-17, -2.165354330708661568 ) ) ;
#36097 = CARTESIAN_POINT ( 'NONE',  ( 0.3871391076115492380, -0.08942795157528024563, -0.3641732283464568787 ) ) ;
#36098 = VERTEX_POINT ( 'NONE', #82232 ) ;
#36099 = CARTESIAN_POINT ( 'NONE',  ( -0.1958661417322836995, 0.3392501089628017219, -0.9547437252306580913 ) ) ;
#36100 = ORIENTED_EDGE ( 'NONE', *, *, #23015, .F. ) ;
#36101 = CARTESIAN_POINT ( 'NONE',  ( -0.9120734908136475250, 0.2952755905511811885, 0.1292274648535926551 ) ) ;
#36102 = CARTESIAN_POINT ( 'NONE',  ( -0.2099737532808391705, 0.2306618581243848609, 0.2411417322834645549 ) ) ;
#36103 = CARTESIAN_POINT ( 'NONE',  ( -0.5118110236220466680, 0.2952755905511811885, 0.000000000000000000 ) ) ;
#36104 = CARTESIAN_POINT ( 'NONE',  ( 0.8136482939632553313, -0.6046776061558809534, -0.2411417322834644161 ) ) ;
#36105 = CARTESIAN_POINT ( 'NONE',  ( -1.325459317585300889, 0.05413385826771666132, 0.4176697321401328100 ) ) ;
#36106 = CARTESIAN_POINT ( 'NONE',  ( -0.2427821522309703550, -0.05778040916215560624, -0.4822834645669293319 ) ) ;
#36107 = CARTESIAN_POINT ( 'NONE',  ( 0.5905511811023629321, -0.6692913385826771977, 8.415575281601705876E-17 ) ) ;
#36108 = CARTESIAN_POINT ( 'NONE',  ( 0.3805774278215230400, 0.05413385826771626580, -0.4176697321401330321 ) ) ;
#36109 = CARTESIAN_POINT ( 'NONE',  ( 0.8136482939632553313, -0.6046776061558809534, -0.2411417322834644161 ) ) ;
#36110 = CARTESIAN_POINT ( 'NONE',  ( 0.3917322834645670104, 2.398668435337828261E-17, -0.8976377952755905110 ) ) ;
#36111 = CARTESIAN_POINT ( 'NONE',  ( -0.3083989501312330295, -0.2845877964562161244, -0.3641732283464567121 ) ) ;
#36112 = ORIENTED_EDGE ( 'NONE', *, *, #1873, .T. ) ;
#36113 = CARTESIAN_POINT ( 'NONE',  ( 0.3420746716998660508, -0.1974969037888703871, -1.522309711286089273 ) ) ;
#36114 = ORIENTED_EDGE ( 'NONE', *, *, #45969, .T. ) ;
#36115 = CARTESIAN_POINT ( 'NONE',  ( -0.6824146981627291497, -0.5023911411419708095, -0.1820866141732282451 ) ) ;
#36116 = CARTESIAN_POINT ( 'NONE',  ( -0.3083989501312330295, -0.3162353388693409650, -0.4822834645669289433 ) ) ;
#36117 = CARTESIAN_POINT ( 'NONE',  ( -0.8661417322834640276, -0.1870078740157480879, -0.4822834645669291653 ) ) ;
#36118 = CARTESIAN_POINT ( 'NONE',  ( -0.9776902887139098386, -0.6692913385826771977, 0.1292274648535927661 ) ) ;
#36119 = CARTESIAN_POINT ( 'NONE',  ( -1.325459317585300889, 0.05413385826771666132, 0.4176697321401328100 ) ) ;
#36120 = CARTESIAN_POINT ( 'NONE',  ( -1.233595800524933894, 0.2306618581243848609, 0.2411417322834645549 ) ) ;
#36121 = CARTESIAN_POINT ( 'NONE',  ( 0.9186351706036752773, 0.1283753931104746893, -0.1820866141732285504 ) ) ;
#36122 = DIRECTION ( 'NONE',  ( -0.000000000000000000, -1.000000000000000000, -0.000000000000000000 ) ) ;
#36123 = CARTESIAN_POINT ( 'NONE',  ( 0.3458507752293908943, -0.3458507752293908943, -0.6476377952755905110 ) ) ;
#36124 = CARTESIAN_POINT ( 'NONE',  ( -0.06561679790026180015, -0.3690944881889765550, -0.3153832671262227771 ) ) ;
#36125 = CARTESIAN_POINT ( 'NONE',  ( 0.1574803149606306130, -0.1870078740157480879, -0.4822834645669291653 ) ) ;
#36126 = CARTESIAN_POINT ( 'NONE',  ( -0.2034120734908128059, 0.2952755905511811885, 0.1292274648535926551 ) ) ;
#36127 = ORIENTED_EDGE ( 'NONE', *, *, #65474, .T. ) ;
#36128 = CARTESIAN_POINT ( 'NONE',  ( 0.1998031496062994405, -0.3460692066303958092, -1.824146981627296604 ) ) ;
#36129 = CARTESIAN_POINT ( 'NONE',  ( -0.5971128608923876868, 0.2952755905511811885, 0.1292274648535926551 ) ) ;
#36130 = ORIENTED_EDGE ( 'NONE', *, *, #67725, .F. ) ;
#36131 = CARTESIAN_POINT ( 'NONE',  ( -0.3460692066303957537, -0.1998031496062994405, -1.704068241469816058 ) ) ;
#36132 = DIRECTION ( 'NONE',  ( 0.000000000000000000, 0.000000000000000000, 1.000000000000000000 ) ) ;
#36133 = CARTESIAN_POINT ( 'NONE',  ( -0.5511811023622041894, -0.1870078740157480601, -0.3641732283464567677 ) ) ;
#36134 = CARTESIAN_POINT ( 'NONE',  ( -0.8070866141732276899, -0.5400638737290844871, 0.3530559997133364547 ) ) ;
#36135 = CARTESIAN_POINT ( 'NONE',  ( -0.4091458600556402980, -0.2362204724409451284, -0.5249343832020997302 ) ) ;
#36136 = CARTESIAN_POINT ( 'NONE',  ( -0.03101036932649587838, 1.063748226153006682, 3.936916540055557245 ) ) ;
#36137 =( BOUNDED_CURVE ( )  B_SPLINE_CURVE ( 2, ( #44191, #37067, #5088, #56418, #69881, #61513, #3858, #80888, #31991, #18948, #7155, #7585, #52170 ),
 .UNSPECIFIED., .F., .F. ) 
 B_SPLINE_CURVE_WITH_KNOTS ( ( 3, 2, 2, 2, 2, 2, 3 ),
 ( 0.8096947309984371399, 0.8106060606060605522, 0.8143939393939394478, 0.8181818181818182323, 0.8219696969696970168, 0.8257575757575758013, 0.8266689053651993246 ),
 .UNSPECIFIED. ) 
 CURVE ( )  GEOMETRIC_REPRESENTATION_ITEM ( )  RATIONAL_B_SPLINE_CURVE ( ( 0.9875488213027523443, 0.9918020599134680371, 1.000000000000000000, 0.9659258262890683122, 1.000000000000000000, 0.9659258262890683122, 1.000000000000000000, 0.9659258262890683122, 1.000000000000000000, 0.9659258262890683122, 1.000000000000000000, 0.9918020599134671489, 0.9875488213027514561 ) ) 
 REPRESENTATION_ITEM ( '' )  );
#36138 = CARTESIAN_POINT ( 'NONE',  ( 0.1049643490035304938, -0.3917322834645669549, -2.374671916010498762 ) ) ;
#36139 = CARTESIAN_POINT ( 'NONE',  ( 1.102362204724410155, -0.1870078740157480879, -0.4822834645669291653 ) ) ;
#36140 = CARTESIAN_POINT ( 'NONE',  ( 0.5446194225721792126, -0.05778040916215560624, -0.4822834645669293319 ) ) ;
#36141 = CARTESIAN_POINT ( 'NONE',  ( 0.4527559055118117182, 0.1660481256975883668, -0.3530559997133364547 ) ) ;
#36142 = CARTESIAN_POINT ( 'NONE',  ( -0.8202099737532799750, 0.1771653543307087075, -0.09757992244046823083 ) ) ;
#36143 = CARTESIAN_POINT ( 'NONE',  ( 0.1640419947506569498, -0.05778040916215522460, 0.4822834645669289988 ) ) ;
#36144 = CARTESIAN_POINT ( 'NONE',  ( -0.1265901696524993347, 0.4724409448818895907, -2.445538057742782101 ) ) ;
#36145 = CARTESIAN_POINT ( 'NONE',  ( -0.2624671916010490880, 0.2306618581243847221, -0.2411417322834647770 ) ) ;
#36146 = CARTESIAN_POINT ( 'NONE',  ( -0.1974969037888706924, 0.3420746716998658843, -1.979658792650919041 ) ) ;
#36147 = CARTESIAN_POINT ( 'NONE',  ( 1.489501312335958172, -0.08942795157528024563, -0.3641732283464568787 ) ) ;
#36148 = CARTESIAN_POINT ( 'NONE',  ( -0.4461942257217840213, 0.1283753931104748280, 0.1820866141732283561 ) ) ;
#36149 = CARTESIAN_POINT ( 'NONE',  ( 1.135170603674541256, -0.5511811023622048555, -0.09757992244046775898 ) ) ;
#36150 = CARTESIAN_POINT ( 'NONE',  ( -1.345144356955379816, -0.05778040916215560624, -0.4822834645669293319 ) ) ;
#36151 = CARTESIAN_POINT ( 'NONE',  ( -0.9514435695538050464, -0.08942795157528024563, -0.3641732283464568787 ) ) ;
#36152 = CARTESIAN_POINT ( 'NONE',  ( 0.4606732211678789546, 1.763126522798926343, 0.5309055118110234117 ) ) ;
#36153 = CARTESIAN_POINT ( 'NONE',  ( -1.154855643044618851, -0.6046776061558809534, -0.2411417322834644161 ) ) ;
#36154 = CARTESIAN_POINT ( 'NONE',  ( -0.6430446194225712953, 0.05413385826771626580, -0.4176697321401330321 ) ) ;
#36155 = CARTESIAN_POINT ( 'NONE',  ( 0.3805774278215230400, -0.4281496062992124485, 0.4176697321401328655 ) ) ;
#36156 = CARTESIAN_POINT ( 'NONE',  ( -0.2867679344610366554, 0.2867679344610365444, -2.461922941436009094 ) ) ;
#36157 = CARTESIAN_POINT ( 'NONE',  ( 0.3805774278215230400, -0.3690944881889763329, 0.3153832671262228327 ) ) ;
#36158 = CARTESIAN_POINT ( 'NONE',  ( -1.535433070866141225, 0.1771653543307087630, 0.000000000000000000 ) ) ;
#36159 = CARTESIAN_POINT ( 'NONE',  ( 0.7480314960629927956, 0.2952755905511811885, 0.000000000000000000 ) ) ;
#36160 = CARTESIAN_POINT ( 'NONE',  ( -1.594488188976377563, -0.4536011799217367080, 0.2665933059059888421 ) ) ;
#36161 = CARTESIAN_POINT ( 'NONE',  ( 1.509186351706037543, -0.3690944881889765550, -0.3153832671262227771 ) ) ;
#36162 = CARTESIAN_POINT ( 'NONE',  ( -0.8333333333333323711, -0.6692913385826773087, -0.1292274648535924053 ) ) ;
#36163 = CARTESIAN_POINT ( 'NONE',  ( -0.1443569553805765515, -0.3690944881889765550, -0.3153832671262227771 ) ) ;
#36164 = CARTESIAN_POINT ( 'NONE',  ( -1.646051170424378096, 0.000000000000000000, 0.3464511005275205946 ) ) ;
#36165 = CARTESIAN_POINT ( 'NONE',  ( 0.4986876640419954376, 0.1283753931104748280, 0.1820866141732283561 ) ) ;
#36166 = ADVANCED_FACE ( 'NONE', ( #6019 ), #83045, .F. ) ;
#36167 = CARTESIAN_POINT ( 'NONE',  ( -0.1049868766404193215, -0.6046776061558807314, 0.2411417322834647770 ) ) ;
#36168 = CARTESIAN_POINT ( 'NONE',  ( 0.1070741851644054776, -0.3996062992125984925, -0.6345144356955381149 ) ) ;
#36169 = EDGE_CURVE ( 'NONE', #11296, #29058, #58606, .T. ) ;
#36170 = CARTESIAN_POINT ( 'NONE',  ( -9.594673741351313045E-17, 0.3917322834645670104, -1.816929133858267820 ) ) ;
#36171 = CARTESIAN_POINT ( 'NONE',  ( 0.6430446194225728496, -0.004921259842519576551, 0.3153832671262227771 ) ) ;
#36172 = CARTESIAN_POINT ( 'NONE',  ( 0.2034120734908144990, -0.6692913385826771977, 0.1292274648535927661 ) ) ;
#36173 = CARTESIAN_POINT ( 'NONE',  ( -0.7217847769028863381, -0.4281496062992124485, 0.4176697321401328655 ) ) ;
#36174 = CARTESIAN_POINT ( 'NONE',  ( -0.4461942257217840213, -0.5023911411419708095, -0.1820866141732282451 ) ) ;
#36175 = DIRECTION ( 'NONE',  ( 0.000000000000000000, -1.000000000000000000, 0.000000000000000000 ) ) ;
#36176 = CARTESIAN_POINT ( 'NONE',  ( -0.3149606299212590610, -0.1870078740157480601, -0.3641732283464567677 ) ) ;
#36177 = CARTESIAN_POINT ( 'NONE',  ( 0.2755905511811031494, 0.2952755905511811885, 0.000000000000000000 ) ) ;
#36178 = VECTOR ( 'NONE', #11706, 39.37007874015748143 ) ;
#36179 = CARTESIAN_POINT ( 'NONE',  ( -1.023622047244094002, -0.1870078740157480601, -0.3641732283464567677 ) ) ;
#36180 = CARTESIAN_POINT ( 'NONE',  ( 0.3996062992125984925, 0.1070741851644054637, -1.461286089238845065 ) ) ;
#36181 = CARTESIAN_POINT ( 'NONE',  ( 1.601049868766404982, 0.2306618581243848609, 0.2411417322834645549 ) ) ;
#36182 = CARTESIAN_POINT ( 'NONE',  ( -0.3458507752293909498, 0.3458507752293908388, -2.616141732283464361 ) ) ;
#36183 = ORIENTED_EDGE ( 'NONE', *, *, #39193, .F. ) ;
#36184 = CARTESIAN_POINT ( 'NONE',  ( -1.581364829396324945, -0.2845877964562159024, 0.3641732283464567677 ) ) ;
#36185 = CARTESIAN_POINT ( 'NONE',  ( -0.6364829396325453192, -0.3162353388693405765, 0.4822834645669290543 ) ) ;
#36186 = CARTESIAN_POINT ( 'NONE',  ( -1.312335958005248715, 0.2306618581243848609, 0.2411417322834645549 ) ) ;
#36187 = CARTESIAN_POINT ( 'NONE',  ( 0.1049643490035303689, 0.3917322834645670104, -1.652887139107611425 ) ) ;
#36188 = CARTESIAN_POINT ( 'NONE',  ( 1.141392835773559211, 0.000000000000000000, 1.141392835773562764 ) ) ;
#36189 = ADVANCED_FACE ( 'NONE', ( #44710 ), #81826, .T. ) ;
#36190 = CARTESIAN_POINT ( 'NONE',  ( 1.246719160104987623, 0.05413385826771626580, -0.4176697321401330321 ) ) ;
#36191 = CARTESIAN_POINT ( 'NONE',  ( 0.2362204724409456558, -0.1870078740157479769, 0.4822834645669291653 ) ) ;
#36192 = DIRECTION ( 'NONE',  ( 0.000000000000000000, 0.000000000000000000, -1.000000000000000000 ) ) ;
#36193 = CARTESIAN_POINT ( 'NONE',  ( 0.1998031496062994128, -0.3460692066303957537, -2.215879265091863726 ) ) ;
#36194 = ADVANCED_FACE ( 'NONE', ( #24949 ), #3526, .T. ) ;
#36195 = CARTESIAN_POINT ( 'NONE',  ( 1.482939632545932307, -0.004921259842519870586, -0.3153832671262229437 ) ) ;
#36196 = CARTESIAN_POINT ( 'NONE',  ( 0.2925321140481932369, 0.2925321140481932369, -0.9251968503937008093 ) ) ;
#36197 = ORIENTED_EDGE ( 'NONE', *, *, #53789, .F. ) ;
#36198 = CARTESIAN_POINT ( 'NONE',  ( -0.7283464566929126471, -0.4536011799217367080, 0.2665933059059888421 ) ) ;
#36199 = CARTESIAN_POINT ( 'NONE',  ( 0.3917322834645669549, 0.1049643490035304660, -2.479002624671915900 ) ) ;
#36200 = VERTEX_POINT ( 'NONE', #56529 ) ;
#36201 = B_SPLINE_CURVE_WITH_KNOTS ( 'NONE', 3,
 ( #1014, #54299, #73690, #32979, #60625, #8871, #26667, #26243, #38872, #28641, #45593, #40854, #13224, #58646, #51481, #20357, #71704, #15196, #66959, #34548, #9703, #77184, #19516, #60214, #64551, #21911, #6888, #2564, #77610, #41676, #15615, #28222, #2975, #53881, #79596, #587, #47573, #16030 ),
 .UNSPECIFIED., .F., .F.,
 ( 4, 2, 2, 2, 2, 2, 2, 2, 2, 2, 2, 2, 2, 2, 2, 2, 2, 2, 4 ),
 ( 7.825718265876660833E-19, 0.0009023223452592552115, 0.001804644690518509556, 0.002706967035777763358, 0.003609289381037017377, 0.004511611726296271829, 0.005413934071555525848, 0.006316256416814780734, 0.007218578762074035621, 0.008120901107333289640, 0.008572062279962875883, 0.009023223452592462127, 0.009925545797851638083, 0.01082786814311081057, 0.01173019048836998653, 0.01263251283362916075, 0.01353483517888833497, 0.01398599635151791427, 0.01443715752414749184 ),
 .UNSPECIFIED. ) ;
#36202 = CARTESIAN_POINT ( 'NONE',  ( 0.3805774278215230400, 0.05413385826771626580, -0.4176697321401330321 ) ) ;
#36203 = CARTESIAN_POINT ( 'NONE',  ( -0.5511811023622041894, -0.1870078740157480879, -0.4822834645669291653 ) ) ;
#36204 = CARTESIAN_POINT ( 'NONE',  ( -0.9055118110236215490, -0.6692913385826771977, 8.415575281601705876E-17 ) ) ;
#36205 = CARTESIAN_POINT ( 'NONE',  ( 0.9120734908136490793, 0.2952755905511810774, -0.1292274648535930714 ) ) ;
#36206 = CARTESIAN_POINT ( 'NONE',  ( -1.338582677165353729, -0.1870078740157479769, 0.3641732283464567677 ) ) ;
#36207 = CARTESIAN_POINT ( 'NONE',  ( 0.08983781461629372633, 7.699586553780600482E-16, 0.3954985857520059711 ) ) ;
#36208 = CARTESIAN_POINT ( 'NONE',  ( 0.2559055118110243332, 0.1660481256975885056, 0.3530559997133364547 ) ) ;
#36209 = CARTESIAN_POINT ( 'NONE',  ( -0.9645669291338575535, 0.1660481256975883668, -0.3530559997133364547 ) ) ;
#36210 = CARTESIAN_POINT ( 'NONE',  ( 0.3917322834645669549, 2.398668435337827645E-17, -2.087907193404512363 ) ) ;
#36211 = CARTESIAN_POINT ( 'NONE',  ( -1.515748031496062076, -0.5400638737290844871, 0.3530559997133364547 ) ) ;
#36212 = DIRECTION ( 'NONE',  ( 0.000000000000000000, 0.000000000000000000, -1.000000000000000000 ) ) ;
#36213 = CARTESIAN_POINT ( 'NONE',  ( -0.2867679344610365999, 0.2867679344610364889, -2.781496062992125040 ) ) ;
#36214 = CARTESIAN_POINT ( 'NONE',  ( 0.9448818897637802916, -0.1870078740157480601, -0.3641732283464567677 ) ) ;
#36215 = ORIENTED_EDGE ( 'NONE', *, *, #53092, .F. ) ;
#36216 = CARTESIAN_POINT ( 'NONE',  ( 0.1974969037888704704, 0.3420746716998660508, 0.01312335958005243601 ) ) ;
#36217 = CARTESIAN_POINT ( 'NONE',  ( -0.3215223097112853146, -0.05778040916215560624, -0.4822834645669293319 ) ) ;
#36218 = ORIENTED_EDGE ( 'NONE', *, *, #12655, .T. ) ;
#36219 = CARTESIAN_POINT ( 'NONE',  ( 0.5249343832021003964, 0.1283753931104746893, -0.1820866141732285504 ) ) ;
#36220 = CARTESIAN_POINT ( 'NONE',  ( -1.410761154855642463, -0.05778040916215522460, 0.4822834645669289988 ) ) ;
#36221 = CARTESIAN_POINT ( 'NONE',  ( 0.5380577427821529035, 0.05413385826771626580, -0.4176697321401330321 ) ) ;
#36222 = CARTESIAN_POINT ( 'NONE',  ( 0.4396325459317590445, -0.6692913385826771977, 0.1292274648535927661 ) ) ;
#36223 = CARTESIAN_POINT ( 'NONE',  ( -0.03280839895013062252, -0.6692913385826771977, 0.1292274648535927661 ) ) ;
#36224 = CARTESIAN_POINT ( 'NONE',  ( -0.3392501089628019995, 0.1958661417322831999, -1.125347399771340573 ) ) ;
#36225 = CARTESIAN_POINT ( 'NONE',  ( -0.6036745406824141069, -0.6046776061558809534, -0.2411417322834644161 ) ) ;
#36226 = CARTESIAN_POINT ( 'NONE',  ( 0.1958661417322834775, 0.3392501089628018884, -2.276246719160105236 ) ) ;
#36227 = CARTESIAN_POINT ( 'NONE',  ( 1.561679790026247350, -0.3690944881889763329, 0.3153832671262228327 ) ) ;
#36228 = CARTESIAN_POINT ( 'NONE',  ( -1.017060367454067249, -0.05778040916215522460, 0.4822834645669289988 ) ) ;
#36229 = CARTESIAN_POINT ( 'NONE',  ( 1.377952755905512472, 0.2952755905511811885, 0.000000000000000000 ) ) ;
#36230 = CARTESIAN_POINT ( 'NONE',  ( 1.036745406824147731, 0.05413385826771666132, 0.4176697321401328100 ) ) ;
#36231 = CARTESIAN_POINT ( 'NONE',  ( -0.2925321140481930704, -0.2925321140481933480, -0.3740157480314960092 ) ) ;
#36232 = CARTESIAN_POINT ( 'NONE',  ( -0.9514435695538050464, -0.3162353388693405765, 0.4822834645669290543 ) ) ;
#36233 = CARTESIAN_POINT ( 'NONE',  ( 0.3460692066303959202, -0.1998031496062991630, 0.1332020997375328031 ) ) ;
#36234 = CARTESIAN_POINT ( 'NONE',  ( 0.3149606299212603933, -0.1870078740157479769, 0.4822834645669291653 ) ) ;
#36235 = CARTESIAN_POINT ( 'NONE',  ( 0.3996062992125986035, 0.1070741851644054776, -2.171916010498687211 ) ) ;
#36236 = CARTESIAN_POINT ( 'NONE',  ( -0.5118110236220466680, 0.2952755905511811885, 0.000000000000000000 ) ) ;
#36237 = CARTESIAN_POINT ( 'NONE',  ( 1.640419947506562393, -0.4281496062992124485, 0.4176697321401328655 ) ) ;
#36238 = CARTESIAN_POINT ( 'NONE',  ( 0.5052493438320218022, -0.5511811023622048555, -0.09757992244046775898 ) ) ;
#36239 = CARTESIAN_POINT ( 'NONE',  ( 1.469816272965879911, 0.2306618581243847221, -0.2411417322834647770 ) ) ;
#36240 = CARTESIAN_POINT ( 'NONE',  ( 0.2362204724409451007, -0.4091458600556402980, -0.9560367454068241511 ) ) ;
#36242 = EDGE_CURVE ( 'NONE', #40260, #2780, #63265, .T. ) ;
#36241 = CARTESIAN_POINT ( 'NONE',  ( 0.9580052493438327987, -0.3690944881889765550, -0.3153832671262227771 ) ) ;
#36243 = CARTESIAN_POINT ( 'NONE',  ( 0.8202099737532813073, 0.2952755905511811885, 0.1292274648535926551 ) ) ;
#36244 = CARTESIAN_POINT ( 'NONE',  ( -0.3949938075777409963, -7.255918531996591613E-17, -0.4311023622047245318 ) ) ;
#36245 = CARTESIAN_POINT ( 'NONE',  ( -0.6233595800524928121, -0.05778040916215522460, 0.4822834645669289988 ) ) ;
#36246 = DIRECTION ( 'NONE',  ( 0.000000000000000000, -1.000000000000000000, 0.000000000000000000 ) ) ;
#36247 = CARTESIAN_POINT ( 'NONE',  ( 1.476377952755906220, 0.07958543189024071263, -0.2665933059059888421 ) ) ;
#36248 = CARTESIAN_POINT ( 'NONE',  ( -0.7808398950131225646, -0.05778040916215522460, 0.4822834645669289988 ) ) ;
#36249 = CARTESIAN_POINT ( 'NONE',  ( 0.03280839895013198948, 0.2952755905511811885, 0.1292274648535926551 ) ) ;
#36250 = CARTESIAN_POINT ( 'NONE',  ( 0.4624320255261049062, 8.471767977567108961E-16, -0.4445507791589058955 ) ) ;
#36251 = CARTESIAN_POINT ( 'NONE',  ( 0.08530183727034192087, -0.3162353388693409650, -0.4822834645669289433 ) ) ;
#36252 = CARTESIAN_POINT ( 'NONE',  ( 0.03280839895013198948, -0.5511811023622048555, -0.09757992244046775898 ) ) ;
#36253 = CARTESIAN_POINT ( 'NONE',  ( -2.874027875014218747, 1.062979042929934392, -0.007789085821668992674 ) ) ;
#36254 = CARTESIAN_POINT ( 'NONE',  ( 8.195543980992789655E-16, -0.1870078740157480601, -0.3641732283464567677 ) ) ;
#36255 = CARTESIAN_POINT ( 'NONE',  ( 0.5511811023622054106, -0.1870078740157480601, -0.3641732283464567677 ) ) ;
#36256 = CARTESIAN_POINT ( 'NONE',  ( -0.06095229741894689357, 1.066899628778971376, -1.625198944407316270 ) ) ;
#36257 = ADVANCED_FACE ( 'NONE', ( #64102 ), #38413, .F. ) ;
#36258 = CARTESIAN_POINT ( 'NONE',  ( 0.3996062992125984925, 0.1070741851644054637, -1.618766404199474929 ) ) ;
#36259 = CARTESIAN_POINT ( 'NONE',  ( 0.5314960629921267055, -0.5400638737290844871, 0.3530559997133364547 ) ) ;
#36260 = CARTESIAN_POINT ( 'NONE',  ( -0.1049643490035302024, -0.3917322834645671215, -1.639107611548556109 ) ) ;
#36261 = CARTESIAN_POINT ( 'NONE',  ( 1.561679790026247350, -0.004921259842519870586, -0.3153832671262229437 ) ) ;
#36262 = CARTESIAN_POINT ( 'NONE',  ( -0.3857315817373087041, 0.06912221444360990008, -1.138966262901371687E-17 ) ) ;
#36263 = CARTESIAN_POINT ( 'NONE',  ( -0.5774278215223089816, 0.1283753931104746893, -0.1820866141732285504 ) ) ;
#36264 = CARTESIAN_POINT ( 'NONE',  ( -0.03937007874015669567, 0.2952755905511811885, 0.000000000000000000 ) ) ;
#36265 = CARTESIAN_POINT ( 'NONE',  ( 1.161417322834646493, -0.4536011799217367080, 0.2665933059059888421 ) ) ;
#36266 = CARTESIAN_POINT ( 'NONE',  ( -1.161417322834644716, -0.4536011799217368745, -0.2665933059059886201 ) ) ;
#36267 = CARTESIAN_POINT ( 'NONE',  ( -1.450131233595799651, -0.6692913385826771977, 0.1292274648535927661 ) ) ;
#36268 = CARTESIAN_POINT ( 'NONE',  ( 0.1115485564304470323, 0.2952755905511811885, 0.1292274648535926551 ) ) ;
#36269 = CARTESIAN_POINT ( 'NONE',  ( 1.272965879265092637, -0.4281496062992127816, -0.4176697321401328100 ) ) ;
#36270 = LINE ( 'NONE', #79256, #32974 ) ;
#36271 = CARTESIAN_POINT ( 'NONE',  ( 0.08530183727034192087, -0.3162353388693409650, -0.4822834645669289433 ) ) ;
#36272 = CARTESIAN_POINT ( 'NONE',  ( 1.305774278215223960, -0.6692913385826771977, 0.1292274648535927661 ) ) ;
#36273 = CARTESIAN_POINT ( 'NONE',  ( 1.108923884514436686, -0.3162353388693409650, -0.4822834645669289433 ) ) ;
#36274 = CARTESIAN_POINT ( 'NONE',  ( -0.5314960629921171575, 2.716535433070866645, -2.543486866223390930 ) ) ;
#36275 = CARTESIAN_POINT ( 'NONE',  ( 0.8989501312335964611, 0.1771653543307087630, 0.09757992244046791164 ) ) ;
#36276 = CARTESIAN_POINT ( 'NONE',  ( -1.548556430446193399, -0.5023911411419708095, -0.1820866141732282451 ) ) ;
#36277 = CARTESIAN_POINT ( 'NONE',  ( 0.2624671916010504757, -0.5023911411419708095, -0.1820866141732282451 ) ) ;
#36278 = CARTESIAN_POINT ( 'NONE',  ( -0.1902887139107604098, 0.2952755905511810774, -0.1292274648535930714 ) ) ;
#36279 = CARTESIAN_POINT ( 'NONE',  ( 0.7283464566929140904, -0.5400638737290845981, -0.3530559997133363437 ) ) ;
#36280 = CARTESIAN_POINT ( 'NONE',  ( -0.5643044619422565855, -0.4281496062992124485, 0.4176697321401328655 ) ) ;
#36281 = CARTESIAN_POINT ( 'NONE',  ( -0.1049643490035302301, -0.3917322834645671770, -1.958680733104674276 ) ) ;
#36282 = CARTESIAN_POINT ( 'NONE',  ( -0.3608923884514428360, -0.5511811023622048555, -0.09757992244046775898 ) ) ;
#36283 = CARTESIAN_POINT ( 'NONE',  ( 0.8727034120734912248, -0.3162353388693409650, -0.4822834645669289433 ) ) ;
#36284 = CARTESIAN_POINT ( 'NONE',  ( 0.8792650918635177559, -0.004921259842519576551, 0.3153832671262227771 ) ) ;
#36285 = CARTESIAN_POINT ( 'NONE',  ( -0.6299212598425062426, 2.165354330708661568, -3.886287458032464226 ) ) ;
#36287 = CARTESIAN_POINT ( 'NONE',  ( 1.601049868766404982, 0.2306618581243848609, 0.2411417322834645549 ) ) ;
#36286 = CARTESIAN_POINT ( 'NONE',  ( -1.049868766404198794, 0.2306618581243847221, -0.2411417322834647770 ) ) ;
#36288 = CARTESIAN_POINT ( 'NONE',  ( -0.2526890999533557003, 1.111360978596734883, 0.1850246388144368703 ) ) ;
#36289 = CARTESIAN_POINT ( 'NONE',  ( -1.279527559055116948, 0.1660481256975883668, -0.3530559997133364547 ) ) ;
#36290 = CARTESIAN_POINT ( 'NONE',  ( -0.3018372703412066094, 0.05413385826771666132, 0.4176697321401328100 ) ) ;
#36291 = CARTESIAN_POINT ( 'NONE',  ( 4.893765752498283924E-17, -0.3996062992125986035, -2.913385826771653697 ) ) ;
#36292 = CARTESIAN_POINT ( 'NONE',  ( 0.1974969037888704704, 0.3420746716998660508, -2.821522309711286258 ) ) ;
#36293 = EDGE_LOOP ( 'NONE', ( #76981, #73591, #8039, #7442, #42811, #75353, #63929 ) ) ;
#36294 = CARTESIAN_POINT ( 'NONE',  ( 0.3018372703412079971, -0.004921259842519870586, -0.3153832671262229437 ) ) ;
#36295 = CARTESIAN_POINT ( 'NONE',  ( -0.1958661417322836718, 0.3392501089628017219, -1.422572178477690574 ) ) ;
#36296 = CARTESIAN_POINT ( 'NONE',  ( 1.043307086614173818, -0.5400638737290845981, -0.3530559997133363437 ) ) ;
#36297 = CARTESIAN_POINT ( 'NONE',  ( -0.2362204724409447953, -0.4091458600556404646, -2.585301837270341352 ) ) ;
#36298 = CARTESIAN_POINT ( 'NONE',  ( 0.4724409448818897017, 0.1265901696524990294, -0.8313648293963252778 ) ) ;
#36299 = PRESENTATION_STYLE_ASSIGNMENT (( #68307 ) ) ;
#36300 = CARTESIAN_POINT ( 'NONE',  ( 1.646981627296588035, -0.3162353388693405765, 0.4822834645669290543 ) ) ;
#36301 = CARTESIAN_POINT ( 'NONE',  ( 1.541994750656168645, -0.5511811023622046335, 0.09757992244046803654 ) ) ;
#36302 = CARTESIAN_POINT ( 'NONE',  ( 0.6102362204724416372, 0.1660481256975883668, -0.3530559997133364547 ) ) ;
#36303 = CARTESIAN_POINT ( 'NONE',  ( 0.1049643490035304522, -0.3917322834645668994, -0.4802956448480821261 ) ) ;
#36304 = CARTESIAN_POINT ( 'NONE',  ( -0.3805774278215216522, 0.05413385826771666132, 0.4176697321401328100 ) ) ;
#36305 = CARTESIAN_POINT ( 'NONE',  ( -1.056430446194224881, 0.1771653543307087075, -0.09757992244046823083 ) ) ;
#36306 = CARTESIAN_POINT ( 'NONE',  ( 0.6496062992125991586, 0.1660481256975885056, 0.3530559997133364547 ) ) ;
#36307 = CARTESIAN_POINT ( 'NONE',  ( 0.03937007874015806264, 0.2952755905511811885, 0.000000000000000000 ) ) ;
#36308 = CARTESIAN_POINT ( 'NONE',  ( 0.4573592755602257087, 1.664450716761304516, 3.910355061080106331 ) ) ;
#36309 = FACE_OUTER_BOUND ( 'NONE', #45821, .T. ) ;
#36310 = CARTESIAN_POINT ( 'NONE',  ( -0.1958661417322833942, -0.3392501089628018884, -1.637158423393387796 ) ) ;
#36311 = CARTESIAN_POINT ( 'NONE',  ( 0.9251968503937015864, 0.1660481256975883668, -0.3530559997133364547 ) ) ;
#36312 = CARTESIAN_POINT ( 'NONE',  ( -0.1771653543307080136, -0.5400638737290844871, 0.3530559997133364547 ) ) ;
#36313 = CARTESIAN_POINT ( 'NONE',  ( -1.279527559055116948, 0.1660481256975883668, -0.3530559997133364547 ) ) ;
#36314 = EDGE_CURVE ( 'NONE', #27310, #6933, #24551, .T. ) ;
#36315 = CARTESIAN_POINT ( 'NONE',  ( 1.049868766404200127, -0.6046776061558809534, -0.2411417322834644161 ) ) ;
#36316 = CARTESIAN_POINT ( 'NONE',  ( 0.4396325459317593221, 0.2952755905511810774, -0.1292274648535930714 ) ) ;
#36317 = CARTESIAN_POINT ( 'NONE',  ( 0.2867679344610365999, 0.2867679344610365999, -0.8523622047244096001 ) ) ;
#36318 = CARTESIAN_POINT ( 'NONE',  ( -0.3608923884514428360, -0.6692913385826773087, -0.1292274648535924053 ) ) ;
#36319 = CARTESIAN_POINT ( 'NONE',  ( 0.1049868766404206816, 0.2306618581243848609, 0.2411417322834645549 ) ) ;
#36320 = CARTESIAN_POINT ( 'NONE',  ( -0.6299212598425188991, -0.1870078740157480879, -0.4822834645669291653 ) ) ;
#36321 = ADVANCED_FACE ( 'NONE', ( #49806 ), #49398, .T. ) ;
#36322 = CARTESIAN_POINT ( 'NONE',  ( 0.3608923884514443348, -0.5511811023622046335, 0.09757992244046803654 ) ) ;
#36323 = CARTESIAN_POINT ( 'NONE',  ( 1.640419947506562393, -0.3690944881889763329, 0.3153832671262228327 ) ) ;
#36324 = CARTESIAN_POINT ( 'NONE',  ( -1.673228346456691717, 0.1660481256975883668, -0.3530559997133364547 ) ) ;
#36325 = CARTESIAN_POINT ( 'NONE',  ( 0.5052493438320215802, 0.2952755905511811885, 0.1292274648535926551 ) ) ;
#36326 = FILL_AREA_STYLE ('',( #3936 ) ) ;
#36327 = CARTESIAN_POINT ( 'NONE',  ( 1.561679790026247350, -0.4281496062992124485, 0.4176697321401328655 ) ) ;
#36328 = CARTESIAN_POINT ( 'NONE',  ( 0.3917322834645670104, 2.398668435337828261E-17, -2.157480314960630086 ) ) ;
#36329 = EDGE_LOOP ( 'NONE', ( #5988, #15622, #38917 ) ) ;
#36330 = ORIENTED_EDGE ( 'NONE', *, *, #50107, .T. ) ;
#36331 = CARTESIAN_POINT ( 'NONE',  ( 0.6430446194225729606, -0.4281496062992127816, -0.4176697321401328100 ) ) ;
#36332 = CARTESIAN_POINT ( 'NONE',  ( 0.1706036745406830368, -0.004921259842519576551, 0.3153832671262227771 ) ) ;
#36334 = CARTESIAN_POINT ( 'NONE',  ( -3.937007874015748143, 1.724409448818897905, 0.6299212598425196763 ) ) ;
#36333 = FACE_OUTER_BOUND ( 'NONE', #14776, .T. ) ;
#36335 = CARTESIAN_POINT ( 'NONE',  ( 0.3917322834645670104, -0.1049643490035303411, -0.6686351706036747222 ) ) ;
#36336 = DIRECTION ( 'NONE',  ( 3.096699300667737957E-16, -1.000000000000000000, 0.000000000000000000 ) ) ;
#36337 =( CONVERSION_BASED_UNIT ( 'INCH', #75070 ) LENGTH_UNIT ( ) NAMED_UNIT ( #69059 ) );
#36338 = CARTESIAN_POINT ( 'NONE',  ( -0.3996062992125985480, -7.340648628747423112E-17, -2.478346456692913868 ) ) ;
#36339 = CARTESIAN_POINT ( 'NONE',  ( 0.5839895013123367340, -0.6692913385826773087, -0.1292274648535924053 ) ) ;
#36340 = CARTESIAN_POINT ( 'NONE',  ( -0.9317585301837263412, -0.4281496062992127816, -0.4176697321401328100 ) ) ;
#36341 = CARTESIAN_POINT ( 'NONE',  ( -0.5511811023622041894, -0.1870078740157480879, -0.4822834645669291653 ) ) ;
#36342 = CARTESIAN_POINT ( 'NONE',  ( 0.7349081364829402885, -0.6046776061558809534, -0.2411417322834644161 ) ) ;
#36343 = CARTESIAN_POINT ( 'NONE',  ( 1.187664041994751285, -0.3162353388693409650, -0.4822834645669289433 ) ) ;
#36344 = CARTESIAN_POINT ( 'NONE',  ( 1.627296587926509996, -0.5023911411419708095, 0.1820866141732285504 ) ) ;
#36345 = ITEM_DEFINED_TRANSFORMATION ( 'NONE', 'NONE', #30192,  #22098 ) ;
#36346 = CARTESIAN_POINT ( 'NONE',  ( 1.161417322834646493, -0.4536011799217367080, 0.2665933059059888421 ) ) ;
#36347 = CARTESIAN_POINT ( 'NONE',  ( -0.8398950131233585692, 0.2306618581243848609, 0.2411417322834645549 ) ) ;
#36348 = CARTESIAN_POINT ( 'NONE',  ( -1.653543307086613234, -0.1870078740157479769, 0.3641732283464567677 ) ) ;
#36349 = CARTESIAN_POINT ( 'NONE',  ( -2.362204724409448620, 0.03937007874015751446, -2.474278114140802984E-14 ) ) ;
#36350 = CARTESIAN_POINT ( 'NONE',  ( -0.2887139107611542133, -0.6046776061558809534, -0.2411417322834644161 ) ) ;
#36352 = CARTESIAN_POINT ( 'NONE',  ( 0.000000000000000000, 0.000000000000000000, 0.000000000000000000 ) ) ;
#36351 = CARTESIAN_POINT ( 'NONE',  ( 1.233595800524935227, 0.2306618581243847221, -0.2411417322834647770 ) ) ;
#36353 = CARTESIAN_POINT ( 'NONE',  ( -0.9580052493438311334, -0.3690944881889763329, 0.3153832671262228327 ) ) ;
#36354 = CARTESIAN_POINT ( 'NONE',  ( 0.3412073490813655186, -0.6046776061558809534, -0.2411417322834644161 ) ) ;
#36355 = CARTESIAN_POINT ( 'NONE',  ( 1.181102362204724976, -0.1870078740157480601, -0.3641732283464567677 ) ) ;
#36356 = CARTESIAN_POINT ( 'NONE',  ( 0.1049643490035303689, 0.3917322834645668994, -1.648274647472754095 ) ) ;
#36357 = B_SPLINE_CURVE_WITH_KNOTS ( 'NONE', 3,
 ( #33863, #45640, #1884, #58271 ),
 .UNSPECIFIED., .F., .F.,
 ( 4, 4 ),
 ( 1.999999999927407068E-07, 0.006970199999999936863 ),
 .UNSPECIFIED. ) ;
#36358 = CARTESIAN_POINT ( 'NONE',  ( -1.246719160104986512, -0.004921259842519576551, 0.3153832671262227771 ) ) ;
#36359 = CARTESIAN_POINT ( 'NONE',  ( 1.318897637795276356, -0.5400638737290844871, 0.3530559997133364547 ) ) ;
#36360 = PLANE ( 'NONE',  #59931 ) ;
#36361 = CARTESIAN_POINT ( 'NONE',  ( -0.01312335958005186876, -0.3690944881889763329, 0.3153832671262228327 ) ) ;
#36362 = CARTESIAN_POINT ( 'NONE',  ( -0.2165354330708654795, -0.5400638737290845981, -0.3530559997133363437 ) ) ;
#36363 = CARTESIAN_POINT ( 'NONE',  ( -1.404199475065615932, -0.3690944881889765550, -0.3153832671262227771 ) ) ;
#36364 = CARTESIAN_POINT ( 'NONE',  ( -0.8858267716535425107, 0.1660481256975883668, -0.3530559997133364547 ) ) ;
#36365 = VECTOR ( 'NONE', #11286, 39.37007874015748143 ) ;
#36366 = CARTESIAN_POINT ( 'NONE',  ( 1.463254593175853824, -0.6692913385826771977, 0.1292274648535927661 ) ) ;
#36367 = CARTESIAN_POINT ( 'NONE',  ( 0.3392501089628018329, 0.1958661417322835607, -0.4429327016086107571 ) ) ;
#36368 = CARTESIAN_POINT ( 'NONE',  ( -0.8727034120734901146, -0.2845877964562159024, 0.3641732283464567677 ) ) ;
#36369 = DIRECTION ( 'NONE',  ( 1.692413147294446216E-16, -0.000000000000000000, 1.000000000000000000 ) ) ;
#36370 = CARTESIAN_POINT ( 'NONE',  ( 1.456692913385827515, 0.2952755905511811885, 0.000000000000000000 ) ) ;
#36371 = CARTESIAN_POINT ( 'NONE',  ( -0.2362204724409447953, -0.4091458600556404646, -2.189632545931758489 ) ) ;
#36372 = CARTESIAN_POINT ( 'NONE',  ( -1.174540682414697335, -0.3162353388693409650, -0.4822834645669289433 ) ) ;
#36373 = CARTESIAN_POINT ( 'NONE',  ( -1.194225721784776262, -0.3690944881889763329, 0.3153832671262228327 ) ) ;
#36374 = CARTESIAN_POINT ( 'NONE',  ( -0.6889763779527552368, -0.4536011799217368745, -0.2665933059059886201 ) ) ;
#36375 = CARTESIAN_POINT ( 'NONE',  ( -1.614173228346455824, 0.2952755905511811885, 0.000000000000000000 ) ) ;
#36376 = CARTESIAN_POINT ( 'NONE',  ( 0.07217847769028949700, -0.3162353388693405765, 0.4822834645669290543 ) ) ;
#36377 = CARTESIAN_POINT ( 'NONE',  ( -0.1574803149606292529, -0.1870078740157480601, -0.3641732283464567677 ) ) ;
#36378 = CARTESIAN_POINT ( 'NONE',  ( -1.286089238845143479, -0.5023911411419708095, 0.1820866141732285504 ) ) ;
#36379 = CARTESIAN_POINT ( 'NONE',  ( -1.272965879265091305, -0.4281496062992124485, 0.4176697321401328655 ) ) ;
#36380 = CARTESIAN_POINT ( 'NONE',  ( 1.443569553805774897, 0.1283753931104748280, 0.1820866141732283561 ) ) ;
#36381 = CARTESIAN_POINT ( 'NONE',  ( 0.8661417322834653598, -0.1870078740157479769, 0.4822834645669291653 ) ) ;
#36382 = FACE_OUTER_BOUND ( 'NONE', #76505, .T. ) ;
#36383 = CARTESIAN_POINT ( 'NONE',  ( 0.5380577427821529035, -0.3690944881889763329, 0.3153832671262228327 ) ) ;
#36384 = CARTESIAN_POINT ( 'NONE',  ( 0.8333333333333340365, -0.6692913385826771977, 0.1292274648535927661 ) ) ;
#36385 = CARTESIAN_POINT ( 'NONE',  ( 1.161417322834646271, 0.07958543189024071263, -0.2665933059059888421 ) ) ;
#36386 = VERTEX_POINT ( 'NONE', #50622 ) ;
#36387 = CARTESIAN_POINT ( 'NONE',  ( -1.404199475065615932, -0.4281496062992127816, -0.4176697321401328100 ) ) ;
#36388 = CARTESIAN_POINT ( 'NONE',  ( -1.076115485564303809, -0.6046776061558809534, -0.2411417322834644161 ) ) ;
#36389 = CARTESIAN_POINT ( 'NONE',  ( -0.02624671916010428221, -0.6046776061558807314, 0.2411417322834647770 ) ) ;
#36390 = CARTESIAN_POINT ( 'NONE',  ( -0.1070741851644057135, 0.3996062992125985480, -0.006561679790026264843 ) ) ;
#36391 = CARTESIAN_POINT ( 'NONE',  ( -0.2925321140481932369, 0.2925321140481931259, -2.143700787401574548 ) ) ;
#36392 = CARTESIAN_POINT ( 'NONE',  ( 0.9776902887139113929, 0.2952755905511811885, 0.1292274648535926551 ) ) ;
#36393 = CARTESIAN_POINT ( 'NONE',  ( 1.391076115485564868, -0.5023911411419708095, 0.1820866141732285504 ) ) ;
#36394 = CARTESIAN_POINT ( 'NONE',  ( 0.1968503937007881344, -0.6692913385826771977, 8.415575281601705876E-17 ) ) ;
#36395 = CARTESIAN_POINT ( 'NONE',  ( 0.7349081364829402885, -0.6046776061558809534, -0.2411417322834644161 ) ) ;
#36396 = CARTESIAN_POINT ( 'NONE',  ( -0.3996062992125986035, -0.1070741851644056997, -1.620734908136482799 ) ) ;
#36397 = CARTESIAN_POINT ( 'NONE',  ( -0.1974969037888706647, 0.3420746716998658843, -0.9580052493438320216 ) ) ;
#36398 = CARTESIAN_POINT ( 'NONE',  ( 0.3996062992125986035, 2.446882876249141962E-17, -2.637795275590551380 ) ) ;
#36399 = CARTESIAN_POINT ( 'NONE',  ( 0.4724409448818898682, 2.892866454678787531E-17, -0.5905511811023621549 ) ) ;
#36400 = CARTESIAN_POINT ( 'NONE',  ( -0.3917322834645669549, -0.1049643490035306603, -0.5104986876640419391 ) ) ;
#36401 = CARTESIAN_POINT ( 'NONE',  ( -0.4921259842519677963, -0.4536011799217367080, 0.2665933059059888421 ) ) ;
#36402 = CARTESIAN_POINT ( 'NONE',  ( -0.6955380577427815458, -0.4281496062992127816, -0.4176697321401328100 ) ) ;
#36403 = CARTESIAN_POINT ( 'NONE',  ( 0.2493438320209980519, -0.4281496062992127816, -0.4176697321401328100 ) ) ;
#36404 = CARTESIAN_POINT ( 'NONE',  ( -0.2891555358219911054, 0.2891555358219909388, -2.301181102362205078 ) ) ;
#36405 = CARTESIAN_POINT ( 'NONE',  ( 1.535433070866142335, -0.6692913385826771977, 8.415575281601705876E-17 ) ) ;
#36406 = CARTESIAN_POINT ( 'NONE',  ( 1.200787401574803681, -0.5400638737290845981, -0.3530559997133363437 ) ) ;
#36407 = CARTESIAN_POINT ( 'NONE',  ( 0.1265901696524989462, 0.4724409448818897572, -2.355643044619422533 ) ) ;
#36408 = CARTESIAN_POINT ( 'NONE',  ( 0.3460692066303959202, 0.1998031496062993295, -1.706036745406824151 ) ) ;
#36409 = LINE ( 'NONE', #48208, #70741 ) ;
#36410 = B_SPLINE_CURVE_WITH_KNOTS ( 'NONE', 3,
 ( #41509, #40261, #21321, #53702, #2800, #67194, #60448, #35197, #79001, #60858, #79411, #3212, #15017, #47393, #9117, #34789, #28874, #54536, #80252, #48229 ),
 .UNSPECIFIED., .F., .F.,
 ( 4, 2, 2, 2, 2, 2, 2, 2, 2, 4 ),
 ( 0.0005422360305776513902, 0.003127735116393569673, 0.004420484659301528868, 0.005066859430755498925, 0.005713234202209468982, 0.006036421587936466153, 0.006359608973663460722, 0.007005983745117451596, 0.008298733288025460231, 0.01088423237384148617 ),
 .UNSPECIFIED. ) ;
#36411 = CARTESIAN_POINT ( 'NONE',  ( 0.9317585301837276734, -0.4281496062992124485, 0.4176697321401328655 ) ) ;
#36412 = EDGE_CURVE ( 'NONE', #32791, #81796, #48417, .T. ) ;
#36413 = CARTESIAN_POINT ( 'NONE',  ( 0.8267716535433077274, 0.2952755905511811885, 0.000000000000000000 ) ) ;
#36414 = CARTESIAN_POINT ( 'NONE',  ( 1.135170603674541256, 0.1771653543307087630, 0.09757992244046791164 ) ) ;
#36416 = CARTESIAN_POINT ( 'NONE',  ( -1.620734908136482577, 0.2952755905511811885, 0.1292274648535926551 ) ) ;
#36415 = CARTESIAN_POINT ( 'NONE',  ( -1.587926509186350810, -0.004921259842519870586, -0.3153832671262229437 ) ) ;
#36417 = CARTESIAN_POINT ( 'NONE',  ( -9.594673741351313045E-17, 0.3917322834645670104, 0.2303149606299211838 ) ) ;
#36418 = DIRECTION ( 'NONE',  ( -0.000000000000000000, -0.000000000000000000, 1.000000000000000000 ) ) ;
#36419 = CARTESIAN_POINT ( 'NONE',  ( 1.010498687664042716, -0.4281496062992124485, 0.4176697321401328655 ) ) ;
#36420 = CARTESIAN_POINT ( 'NONE',  ( 1.476377952755906442, -0.4536011799217367080, 0.2665933059059888421 ) ) ;
#36421 = CARTESIAN_POINT ( 'NONE',  ( -0.6299212598425188991, -0.1870078740157479769, 0.4822834645669291653 ) ) ;
#36422 = CARTESIAN_POINT ( 'NONE',  ( -0.6167979002624665030, 0.05413385826771666132, 0.4176697321401328100 ) ) ;
#36423 = CARTESIAN_POINT ( 'NONE',  ( -1.528871391076114250, -0.6692913385826771977, 0.1292274648535927661 ) ) ;
#36424 = CARTESIAN_POINT ( 'NONE',  ( -0.3917322834645671215, 0.1049643490035301469, 0.04002624671916000382 ) ) ;
#36425 = CARTESIAN_POINT ( 'NONE',  ( 0.3608923884514443348, 0.2952755905511810774, -0.1292274648535930714 ) ) ;
#36426 = CARTESIAN_POINT ( 'NONE',  ( -9.594673741351313045E-17, 0.3917322834645670104, -2.354330708661417138 ) ) ;
#36427 = CARTESIAN_POINT ( 'NONE',  ( 1.587926509186352586, -0.4281496062992127816, -0.4176697321401328100 ) ) ;
#36428 = ORIENTED_EDGE ( 'NONE', *, *, #23876, .T. ) ;
#36429 = CARTESIAN_POINT ( 'NONE',  ( -0.3420746716998659953, -0.1974969037888706647, -2.572178477690288734 ) ) ;
#36430 = ORIENTED_EDGE ( 'NONE', *, *, #36782, .F. ) ;
#36431 = CARTESIAN_POINT ( 'NONE',  ( -1.586052503253849499, 0.4724409448818907564, 0.1653254495020552439 ) ) ;
#36432 = CARTESIAN_POINT ( 'NONE',  ( 1.200787401574803681, -0.4536011799217368745, -0.2665933059059886201 ) ) ;
#36433 = CARTESIAN_POINT ( 'NONE',  ( 0.1070741851644054915, -0.3996062992125986035, -1.187664041994750619 ) ) ;
#36434 = CYLINDRICAL_SURFACE ( 'NONE', #59930, 0.4724409448818898682 ) ;
#36435 = CARTESIAN_POINT ( 'NONE',  ( 0.3307086614173228023, 0.000000000000000000, 0.000000000000000000 ) ) ;
#36436 = DIRECTION ( 'NONE',  ( 0.000000000000000000, 0.000000000000000000, -1.000000000000000000 ) ) ;
#36437 = CARTESIAN_POINT ( 'NONE',  ( 0.4531182788721078158, 1.771653543307086354, 0.5309055118110234117 ) ) ;
#36438 = CARTESIAN_POINT ( 'NONE',  ( -0.3917322834645670104, -7.196005306013484475E-17, -0.2814960629921260393 ) ) ;
#36439 = CARTESIAN_POINT ( 'NONE',  ( -0.1968503937007867743, 0.1771653543307087630, 0.000000000000000000 ) ) ;
#36440 = CARTESIAN_POINT ( 'NONE',  ( -1.371391076115484831, 0.1771653543307087075, -0.09757992244046823083 ) ) ;
#36441 = CARTESIAN_POINT ( 'NONE',  ( 1.469816272965879911, 0.2306618581243847221, -0.2411417322834647770 ) ) ;
#36442 = CARTESIAN_POINT ( 'NONE',  ( 0.6233595800524939223, -0.3162353388693405765, 0.4822834645669290543 ) ) ;
#36443 = CARTESIAN_POINT ( 'NONE',  ( -1.443569553805773564, 0.2306618581243847221, -0.2411417322834647770 ) ) ;
#36444 = CARTESIAN_POINT ( 'NONE',  ( -0.2867679344610365999, 0.2867679344610364889, -0.1692913385826771144 ) ) ;
#36445 = ORIENTED_EDGE ( 'NONE', *, *, #67062, .T. ) ;
#36446 = CARTESIAN_POINT ( 'NONE',  ( -1.646981627296586703, -0.05778040916215522460, 0.4822834645669289988 ) ) ;
#36447 = CARTESIAN_POINT ( 'NONE',  ( -0.1990279662527743021, -0.1990279662527743021, 0.1112963449492364171 ) ) ;
#36448 = CARTESIAN_POINT ( 'NONE',  ( 0.4724409448818896462, 0.1265901696524990294, -1.699475065616798064 ) ) ;
#36449 = CARTESIAN_POINT ( 'NONE',  ( 2.138259192565330924, 1.653403552777526153, 0.4602852883866581646 ) ) ;
#36450 = CARTESIAN_POINT ( 'NONE',  ( 0.3392501089628018329, 0.1958661417322835607, -2.735564304461941987 ) ) ;
#36451 = CARTESIAN_POINT ( 'NONE',  ( -0.8267716535433065062, 0.2952755905511811885, 0.000000000000000000 ) ) ;
#36452 = CARTESIAN_POINT ( 'NONE',  ( 1.364829396325460076, 0.2306618581243848609, 0.2411417322834645549 ) ) ;
#36454 = CARTESIAN_POINT ( 'NONE',  ( 1.603475055217291612, 0.9922665159524515222, 0.04573490813648272563 ) ) ;
#36453 = FACE_OUTER_BOUND ( 'NONE', #49159, .T. ) ;
#36455 = CARTESIAN_POINT ( 'NONE',  ( 1.463254593175853824, -0.6692913385826771977, 0.1292274648535927661 ) ) ;
#36456 = CARTESIAN_POINT ( 'NONE',  ( -0.8333333333333323711, -0.6692913385826773087, -0.1292274648535924053 ) ) ;
#36457 = CARTESIAN_POINT ( 'NONE',  ( 0.3917322834645668994, -0.1049643490035303134, -0.1915817340869272467 ) ) ;
#36458 = CARTESIAN_POINT ( 'NONE',  ( -0.1115485564304456306, 0.1771653543307087075, -0.09757992244046823083 ) ) ;
#36459 = CARTESIAN_POINT ( 'NONE',  ( -0.3917322834645670104, -7.196005306013484475E-17, -0.2814960629921260393 ) ) ;
#36460 = CARTESIAN_POINT ( 'NONE',  ( -0.07874015748031421014, -0.1870078740157479769, 0.3641732283464567677 ) ) ;
#36461 = CARTESIAN_POINT ( 'NONE',  ( 0.5446194225721792126, -0.08942795157528024563, -0.3641732283464568787 ) ) ;
#36462 = CARTESIAN_POINT ( 'NONE',  ( 0.3740157480314966754, 0.1660481256975883668, -0.3530559997133364547 ) ) ;
#36463 = CARTESIAN_POINT ( 'NONE',  ( -0.8727034120734901146, -0.2845877964562159024, 0.3641732283464567677 ) ) ;
#36464 = CARTESIAN_POINT ( 'NONE',  ( -0.3392501089628019995, 0.1958661417322832277, -2.538057742782152015 ) ) ;
#36465 = CARTESIAN_POINT ( 'NONE',  ( 1.443569553805774897, 0.2306618581243848609, 0.2411417322834645549 ) ) ;
#36466 = CARTESIAN_POINT ( 'NONE',  ( -0.8070866141732276899, 0.1660481256975883668, -0.3530559997133364547 ) ) ;
#36467 = CARTESIAN_POINT ( 'NONE',  ( -0.4091458600556402980, -0.2362204724409451284, -0.6017060367454067915 ) ) ;
#36468 = CARTESIAN_POINT ( 'NONE',  ( -0.1115485564304456306, 0.2952755905511810774, -0.1292274648535930714 ) ) ;
#36469 = CARTESIAN_POINT ( 'NONE',  ( -0.6430446194225712953, 0.05413385826771626580, -0.4176697321401330321 ) ) ;
#36470 = CARTESIAN_POINT ( 'NONE',  ( 1.299212598425197429, -0.5511811023622047445, 6.969142054262312111E-17 ) ) ;
#36471 = CARTESIAN_POINT ( 'NONE',  ( 0.2296587926509192634, -0.08942795157528024563, -0.3641732283464568787 ) ) ;
#36472 = CARTESIAN_POINT ( 'NONE',  ( -0.1640419947506555343, -0.3162353388693405765, 0.4822834645669290543 ) ) ;
#36473 = CARTESIAN_POINT ( 'NONE',  ( -0.8464566929133852113, 0.1660481256975885056, 0.3530559997133364547 ) ) ;
#36474 = CARTESIAN_POINT ( 'NONE',  ( -0.6155095129758836325, 1.955395699586894409, -0.5046436704918447758 ) ) ;
#36475 = CARTESIAN_POINT ( 'NONE',  ( 1.555118110236221041, 0.07958543189024071263, -0.2665933059059888421 ) ) ;
#36476 = CARTESIAN_POINT ( 'NONE',  ( 0.1377952755905518800, 0.1660481256975883668, -0.3530559997133364547 ) ) ;
#36477 = CIRCLE ( 'NONE', #62017, 0.2736220472440938911 ) ;
#36478 = VERTEX_POINT ( 'NONE', #13599 ) ;
#36479 = CARTESIAN_POINT ( 'NONE',  ( -0.3996062992125985480, -7.340648628747423112E-17, -1.848425196850393526 ) ) ;
#36480 = CARTESIAN_POINT ( 'NONE',  ( 1.233595800524935227, -0.6046776061558807314, 0.2411417322834647770 ) ) ;
#36481 = CARTESIAN_POINT ( 'NONE',  ( -0.4658792650918627265, -0.08942795157527998196, 0.3641732283464567121 ) ) ;
#36482 = CARTESIAN_POINT ( 'NONE',  ( -0.4330708661417315697, 0.2952755905511811885, 0.000000000000000000 ) ) ;
#36483 = CARTESIAN_POINT ( 'NONE',  ( 1.404199475065617708, 0.05413385826771626580, -0.4176697321401330321 ) ) ;
#36484 = CARTESIAN_POINT ( 'NONE',  ( 0.8202099737532814183, -0.6692913385826773087, -0.1292274648535924053 ) ) ;
#36485 = CARTESIAN_POINT ( 'NONE',  ( -1.496062992125983815, -0.1870078740157479769, 0.4822834645669291653 ) ) ;
#36486 = CARTESIAN_POINT ( 'NONE',  ( -1.030183727034119867, -0.08942795157528024563, -0.3641732283464568787 ) ) ;
#36487 = CARTESIAN_POINT ( 'NONE',  ( -0.3460692066303957537, -0.1998031496062994405, -0.4442257217847768724 ) ) ;
#36488 = CARTESIAN_POINT ( 'NONE',  ( -0.1070741851644051862, -0.3996062992125987146, -0.3871391076115485719 ) ) ;
#36489 = CARTESIAN_POINT ( 'NONE',  ( 0.3420746716998660508, -0.1974969037888703871, 0.05249343832020991057 ) ) ;
#36490 = CARTESIAN_POINT ( 'NONE',  ( 1.522309711286089939, 0.1283753931104748280, 0.1820866141732283561 ) ) ;
#36491 = CARTESIAN_POINT ( 'NONE',  ( 0.6233595800524939223, -0.2845877964562159024, 0.3641732283464567677 ) ) ;
#36492 = CARTESIAN_POINT ( 'NONE',  ( 0.4855643044619428750, 0.05413385826771666132, 0.4176697321401328100 ) ) ;
#36493 = CARTESIAN_POINT ( 'NONE',  ( 2.795275590551181466, 0.5118110236220471121, -3.234977217930338483E-16 ) ) ;
#36494 = CARTESIAN_POINT ( 'NONE',  ( -0.3949938075777409963, -7.255918531996591613E-17, -1.061023622047243986 ) ) ;
#36495 = CARTESIAN_POINT ( 'NONE',  ( 0.6824146981627303710, -0.5023911411419708095, 0.1820866141732285504 ) ) ;
#36496 = EDGE_CURVE ( 'NONE', #1243, #14206, #64935, .T. ) ;
#36497 = CARTESIAN_POINT ( 'NONE',  ( -0.3805774278215216522, 0.05413385826771666132, 0.4176697321401328100 ) ) ;
#36498 = CARTESIAN_POINT ( 'NONE',  ( -0.8661417322834640276, -0.1870078740157479769, 0.4822834645669291653 ) ) ;
#36499 = CARTESIAN_POINT ( 'NONE',  ( 1.154855643044620184, -0.6046776061558807314, 0.2411417322834647770 ) ) ;
#36500 = CARTESIAN_POINT ( 'NONE',  ( -0.4724409448818895907, -0.1265901696524993070, -1.148293963254592986 ) ) ;
#36501 = CARTESIAN_POINT ( 'NONE',  ( 0.3996062992125986035, 2.446882876249141962E-17, -2.480314960629921295 ) ) ;
#36502 = CARTESIAN_POINT ( 'NONE',  ( -0.006561679790025524116, -0.2845877964562159024, 0.3641732283464567677 ) ) ;
#36503 = VERTEX_POINT ( 'NONE', #21158 ) ;
#36504 = CARTESIAN_POINT ( 'NONE',  ( -0.3392501089628019995, 0.1958661417322831999, -0.9678670848107107094 ) ) ;
#36505 = VERTEX_POINT ( 'NONE', #77149 ) ;
#36506 = ADVANCED_FACE ( 'NONE', ( #77575 ), #78832, .F. ) ;
#36507 = CARTESIAN_POINT ( 'NONE',  ( -1.036745406824146176, 0.05413385826771626580, -0.4176697321401330321 ) ) ;
#36508 = CARTESIAN_POINT ( 'NONE',  ( -0.06561679790026180015, 0.05413385826771666132, 0.4176697321401328100 ) ) ;
#36509 = CARTESIAN_POINT ( 'NONE',  ( -0.4658792650918627265, -0.3162353388693409650, -0.4822834645669289433 ) ) ;
#36510 = CARTESIAN_POINT ( 'NONE',  ( 0.4133858267716541968, 0.1660481256975885056, 0.3530559997133364547 ) ) ;
#36511 = CARTESIAN_POINT ( 'NONE',  ( -0.6167979002624665030, -0.4281496062992127816, -0.4176697321401328100 ) ) ;
#36512 = CARTESIAN_POINT ( 'NONE',  ( -1.213910761154854745, -0.6692913385826771977, 0.1292274648535927661 ) ) ;
#36513 = CARTESIAN_POINT ( 'NONE',  ( -0.9383202099737524282, -0.05778040916215522460, 0.4822834645669289988 ) ) ;
#36514 = CARTESIAN_POINT ( 'NONE',  ( 0.9186351706036751663, -0.6046776061558807314, 0.2411417322834647770 ) ) ;
#36515 = CARTESIAN_POINT ( 'NONE',  ( 0.4593175853018379162, -0.4281496062992124485, 0.4176697321401328655 ) ) ;
#36516 = CARTESIAN_POINT ( 'NONE',  ( 0.2867679344610365999, -0.2867679344610365444, -1.035433070866141447 ) ) ;
#36517 = CARTESIAN_POINT ( 'NONE',  ( -0.5314960629921250401, 0.07958543189024085140, 0.2665933059059887866 ) ) ;
#36518 = EDGE_LOOP ( 'NONE', ( #57058, #57199, #60031, #52553 ) ) ;
#36519 = CARTESIAN_POINT ( 'NONE',  ( 0.1058382717557500713, -0.3949938075777409408, -1.502624671916010790 ) ) ;
#36520 = ORIENTED_EDGE ( 'NONE', *, *, #4112, .F. ) ;
#36521 = CARTESIAN_POINT ( 'NONE',  ( -1.272965879265091305, -0.3690944881889763329, 0.3153832671262228327 ) ) ;
#36522 = CARTESIAN_POINT ( 'NONE',  ( -0.3018372703412066094, -0.4281496062992127816, -0.4176697321401328100 ) ) ;
#36523 = DIRECTION ( 'NONE',  ( -1.000000000000000000, -0.000000000000000000, -0.000000000000000000 ) ) ;
#36524 = CARTESIAN_POINT ( 'NONE',  ( -0.7349081364829390672, 0.2306618581243847221, -0.2411417322834647770 ) ) ;
#36525 = CARTESIAN_POINT ( 'NONE',  ( -0.6561679790026240244, -0.6046776061558807314, 0.2411417322834647770 ) ) ;
#36527 = CARTESIAN_POINT ( 'NONE',  ( -1.640419947506561060, 0.05413385826771666132, 0.4176697321401328100 ) ) ;
#36526 = B_SPLINE_CURVE_WITH_KNOTS ( 'NONE', 3,
 ( #34511, #60176, #15996, #73227, #15578, #67748, #40405, #41643, #2529, #59753, #28187, #67334, #2940, #41236, #27773, #42052, #28604, #54261, #79977, #61000, #3348, #72402, #29014, #80391, #22703, #35746, #3763, #80794, #8422, #34090, #23111, #29427, #79145, #36979, #24344, #31483, #42460, #61830, #69389, #31068, #62660, #69797, #23521, #23936, #37801, #29834, #49191, #74892, #17240, #81206, #11321, #42868, #74476, #57144, #50013, #37398, #55497, #68562, #56737, #5000 ),
 .UNSPECIFIED., .F., .F.,
 ( 4, 2, 2, 2, 2, 2, 2, 2, 2, 2, 2, 2, 2, 2, 2, 2, 2, 2, 2, 2, 2, 2, 2, 2, 2, 2, 2, 2, 2, 4 ),
 ( 0.01323639539072319141, 0.01388181161316683759, 0.01452722783561048205, 0.01581806028049779350, 0.01710889272538510322, 0.01839972517027241294, 0.02098139006004704626, 0.02356305494982167958, 0.02485388739470899278, 0.02614471983959630944, 0.02743555228448362263, 0.02872638472937093929, 0.03130804961914556567, 0.03259888206403287886, 0.03388971450892019205, 0.03453513073136384171, 0.03518054695380749830, 0.03647137939869481843, 0.03776221184358213162, 0.03905304428846944481, 0.04034387673335675800, 0.04163470917824407813, 0.04421637406801870451, 0.04679803895779334477, 0.04937970384756797115, 0.05067053629245528434, 0.05196136873734259753, 0.05325220118222991073, 0.05389761740467358120, 0.05454303362711723779 ),
 .UNSPECIFIED. ) ;
#36528 = LINE ( 'NONE', #31444, #24092 ) ;
#36529 = CARTESIAN_POINT ( 'NONE',  ( 1.062992125984252745, 0.1771653543307087630, 0.000000000000000000 ) ) ;
#36530 = CARTESIAN_POINT ( 'NONE',  ( -0.3392501089628019995, 0.1958661417322832277, -0.1108923884514436548 ) ) ;
#36531 = CARTESIAN_POINT ( 'NONE',  ( -0.006561679790025524116, -0.2845877964562159024, 0.3641732283464567677 ) ) ;
#36532 = CARTESIAN_POINT ( 'NONE',  ( -0.3477690288713902178, 0.2952755905511810774, -0.1292274648535930714 ) ) ;
#36533 = CARTESIAN_POINT ( 'NONE',  ( 1.614173228346457378, 0.2952755905511811885, 0.000000000000000000 ) ) ;
#36534 = CARTESIAN_POINT ( 'NONE',  ( 0.06561679790026316017, -0.4281496062992124485, 0.4176697321401328655 ) ) ;
#36535 = VERTEX_POINT ( 'NONE', #46395 ) ;
#36536 = CARTESIAN_POINT ( 'NONE',  ( -0.3460692066303960868, 0.1998031496062990242, -1.916010498687664043 ) ) ;
#36537 = FACE_OUTER_BOUND ( 'NONE', #81560, .T. ) ;
#36538 = ORIENTED_EDGE ( 'NONE', *, *, #59829, .F. ) ;
#36539 = CARTESIAN_POINT ( 'NONE',  ( 0.3460692066303958092, 0.1998031496062993018, -1.625328083989501460 ) ) ;
#36540 = CARTESIAN_POINT ( 'NONE',  ( 1.013613127888309595, -4.408777212815537393E-16, -0.4445507791589063395 ) ) ;
#36541 = CARTESIAN_POINT ( 'NONE',  ( -0.8005249343832013809, -0.3690944881889763329, 0.3153832671262228327 ) ) ;
#36542 = CARTESIAN_POINT ( 'NONE',  ( -1.167979002624671470, -0.4281496062992127816, -0.4176697321401328100 ) ) ;
#36543 = CARTESIAN_POINT ( 'NONE',  ( 0.3458507752293908943, 0.3458507752293908943, -0.2952755905511811330 ) ) ;
#36544 = CARTESIAN_POINT ( 'NONE',  ( 1.220472440944879722, 0.000000000000000000, 0.5309055118110233007 ) ) ;
#36545 = CARTESIAN_POINT ( 'NONE',  ( -0.2867679344610364334, -0.2867679344610367109, -2.820866141732283339 ) ) ;
#36546 = CARTESIAN_POINT ( 'NONE',  ( 1.174540682414699111, -0.3162353388693405765, 0.4822834645669290543 ) ) ;
#36547 = CARTESIAN_POINT ( 'NONE',  ( 0.2887139107611556010, -0.6046776061558807314, 0.2411417322834647770 ) ) ;
#36548 = CARTESIAN_POINT ( 'NONE',  ( 0.6561679790026253567, -0.6046776061558809534, -0.2411417322834644161 ) ) ;
#36549 = CARTESIAN_POINT ( 'NONE',  ( -0.6889763779527552368, 0.07958543189024085140, 0.2665933059059887866 ) ) ;
#36550 = CARTESIAN_POINT ( 'NONE',  ( -0.3018372703412066094, 0.05413385826771666132, 0.4176697321401328100 ) ) ;
#36551 = CARTESIAN_POINT ( 'NONE',  ( -0.4091458600556405756, 0.2362204724409446288, -2.465223097112860806 ) ) ;
#36552 = CARTESIAN_POINT ( 'NONE',  ( -0.9645669291338575535, -0.5400638737290844871, 0.3530559997133364547 ) ) ;
#36553 = CARTESIAN_POINT ( 'NONE',  ( -0.3949938075777411073, 0.1058382717557497660, -2.156824146981627610 ) ) ;
#36554 = CARTESIAN_POINT ( 'NONE',  ( 1.299212598425197429, 0.1771653543307087630, 0.000000000000000000 ) ) ;
#36555 = CARTESIAN_POINT ( 'NONE',  ( -0.3543307086614165824, -0.5511811023622047445, 6.969142054262312111E-17 ) ) ;
#36556 = CARTESIAN_POINT ( 'NONE',  ( 1.122047244094488860, -0.4536011799217368745, -0.2665933059059886201 ) ) ;
#36557 = CARTESIAN_POINT ( 'NONE',  ( -1.725721784776902190, -0.05778040916215522460, 0.4822834645669289988 ) ) ;
#36558 = CARTESIAN_POINT ( 'NONE',  ( -1.069553805774277722, -0.5511811023622048555, -0.09757992244046775898 ) ) ;
#36559 = CARTESIAN_POINT ( 'NONE',  ( 1.607611548556431069, 0.2952755905511811885, 0.1292274648535926551 ) ) ;
#36560 = CARTESIAN_POINT ( 'NONE',  ( -0.9842519685039365918, -0.6692913385826771977, 8.415575281601705876E-17 ) ) ;
#36561 = CARTESIAN_POINT ( 'NONE',  ( -0.4593175853018364174, -0.4281496062992127816, -0.4176697321401328100 ) ) ;
#36562 = CARTESIAN_POINT ( 'NONE',  ( 0.2690288713910768403, 0.2952755905511811885, 0.1292274648535926551 ) ) ;
#36563 = CARTESIAN_POINT ( 'NONE',  ( -0.2099737532808391705, 0.1283753931104748280, 0.1820866141732283561 ) ) ;
#36564 = CARTESIAN_POINT ( 'NONE',  ( -1.561679790026246017, -0.004921259842519576551, 0.3153832671262227771 ) ) ;
#36565 = CARTESIAN_POINT ( 'NONE',  ( 0.9514435695538062676, -0.3162353388693409650, -0.4822834645669289433 ) ) ;
#36566 = DIRECTION ( 'NONE',  ( -1.000000000000000000, -0.000000000000000000, -0.000000000000000000 ) ) ;
#36567 = CARTESIAN_POINT ( 'NONE',  ( 1.292650918635171564, 0.1771653543307087630, 0.09757992244046791164 ) ) ;
#36568 = CARTESIAN_POINT ( 'NONE',  ( -0.9055118110236215490, 0.2952755905511811885, 0.000000000000000000 ) ) ;
#36569 = CARTESIAN_POINT ( 'NONE',  ( -0.1640419947506553400, -0.08942795157528024563, -0.3641732283464568787 ) ) ;
#36570 = DIRECTION ( 'NONE',  ( 3.096699300667737957E-16, -1.000000000000000000, 0.000000000000000000 ) ) ;
#36571 = CARTESIAN_POINT ( 'NONE',  ( 0.3871391076115492380, -0.08942795157528024563, -0.3641732283464568787 ) ) ;
#36572 = CARTESIAN_POINT ( 'NONE',  ( -0.1902887139107604098, 0.2952755905511810774, -0.1292274648535930714 ) ) ;
#36573 = CARTESIAN_POINT ( 'NONE',  ( -9.787531504996566615E-17, 0.3996062992125985480, -0.7066929133858268486 ) ) ;
#36574 = CARTESIAN_POINT ( 'NONE',  ( -0.1958661417322834220, -0.3392501089628018884, -2.197506561679789971 ) ) ;
#36575 = CARTESIAN_POINT ( 'NONE',  ( 0.7874015748031503170, -0.1870078740157479769, 0.3641732283464567677 ) ) ;
#36576 = CARTESIAN_POINT ( 'NONE',  ( -0.1706036745406816491, 0.05413385826771626580, -0.4176697321401330321 ) ) ;
#36577 = CARTESIAN_POINT ( 'NONE',  ( -0.8202099737532799750, 0.2952755905511810774, -0.1292274648535930714 ) ) ;
#36578 = CARTESIAN_POINT ( 'NONE',  ( -0.8464566929133852113, 0.07958543189024085140, 0.2665933059059887866 ) ) ;
#36579 = CARTESIAN_POINT ( 'NONE',  ( -3.933480768563217378, 1.093172257416577864, -0.1672395799304293440 ) ) ;
#36580 = CARTESIAN_POINT ( 'NONE',  ( -0.5839895013123351797, -0.5511811023622046335, 0.09757992244046803654 ) ) ;
#36581 = CARTESIAN_POINT ( 'NONE',  ( -0.1049868766404193215, -0.6046776061558807314, 0.2411417322834647770 ) ) ;
#36582 = CARTESIAN_POINT ( 'NONE',  ( -0.9842519685039365918, -0.5511811023622047445, 6.969142054262312111E-17 ) ) ;
#36583 = CARTESIAN_POINT ( 'NONE',  ( -1.404199475065615932, -0.4281496062992127816, -0.4176697321401328100 ) ) ;
#36584 = CARTESIAN_POINT ( 'NONE',  ( 0.2234477481026895529, 0.004960608223778500969, -0.3437734562760191848 ) ) ;
#36585 = ORIENTED_EDGE ( 'NONE', *, *, #38333, .F. ) ;
#36586 = CARTESIAN_POINT ( 'NONE',  ( -1.371391076115484831, 0.1771653543307087075, -0.09757992244046823083 ) ) ;
#36587 = AXIS2_PLACEMENT_3D ( 'NONE', #9381, #47667, #35882 ) ;
#36588 = CARTESIAN_POINT ( 'NONE',  ( -0.3083989501312330295, -0.05778040916215522460, 0.4822834645669289988 ) ) ;
#36589 = CARTESIAN_POINT ( 'NONE',  ( -1.017060367454067249, -0.05778040916215522460, 0.4822834645669289988 ) ) ;
#36590 = CARTESIAN_POINT ( 'NONE',  ( 0.2867679344610365999, -0.2867679344610365444, -1.442913385826771755 ) ) ;
#36591 = DIRECTION ( 'NONE',  ( -0.000000000000000000, -1.000000000000000000, -0.000000000000000000 ) ) ;
#36592 = CARTESIAN_POINT ( 'NONE',  ( 0.8858267716535438430, 0.1660481256975885056, 0.3530559997133364547 ) ) ;
#36593 = CARTESIAN_POINT ( 'NONE',  ( 0.5249343832021005074, -0.6046776061558807314, 0.2411417322834647770 ) ) ;
#36594 = LINE ( 'NONE', #43307, #74518 ) ;
#36595 = CARTESIAN_POINT ( 'NONE',  ( -0.1070741851644057135, 0.3996062992125984925, -2.445538057742782101 ) ) ;
#36596 = CARTESIAN_POINT ( 'NONE',  ( 0.9908136482939640111, 0.1771653543307087075, -0.09757992244046823083 ) ) ;
#36597 = CARTESIAN_POINT ( 'NONE',  ( -0.2925321140481930704, -0.2925321140481933480, -1.003937007874015741 ) ) ;
#36598 = ORIENTED_EDGE ( 'NONE', *, *, #57736, .F. ) ;
#36599 = CARTESIAN_POINT ( 'NONE',  ( -0.9120734908136475250, -0.5511811023622048555, -0.09757992244046775898 ) ) ;
#36600 = CARTESIAN_POINT ( 'NONE',  ( 4.797336870675656522E-17, -0.3917322834645670104, -2.590551181102362044 ) ) ;
#36601 = ORIENTED_EDGE ( 'NONE', *, *, #17740, .T. ) ;
#36602 = CARTESIAN_POINT ( 'NONE',  ( 0.2362204724409456558, -0.1870078740157480879, -0.4822834645669291653 ) ) ;
#36603 = CARTESIAN_POINT ( 'NONE',  ( -0.3215223097112853146, -0.3162353388693405765, 0.4822834645669290543 ) ) ;
#36604 = CARTESIAN_POINT ( 'NONE',  ( -1.095800524934382292, -0.3162353388693409650, -0.4822834645669289433 ) ) ;
#36605 = CARTESIAN_POINT ( 'NONE',  ( 1.227034120734908917, 0.2952755905511810774, -0.1292274648535930714 ) ) ;
#36606 = CARTESIAN_POINT ( 'NONE',  ( -1.272965879265091305, -0.004921259842519870586, -0.3153832671262229437 ) ) ;
#36607 = LINE ( 'NONE', #16456, #21185 ) ;
#36608 = CARTESIAN_POINT ( 'NONE',  ( -0.07874015748031421014, -0.1870078740157479769, 0.4822834645669291653 ) ) ;
#36609 = CARTESIAN_POINT ( 'NONE',  ( -1.181102362204723644, -0.1870078740157479769, 0.4822834645669291653 ) ) ;
#36610 = CARTESIAN_POINT ( 'NONE',  ( 0.1958661417322836162, -0.3392501089628018329, -1.904180159283777485 ) ) ;
#36611 = DIRECTION ( 'NONE',  ( 0.000000000000000000, -1.000000000000000000, -0.000000000000000000 ) ) ;
#36612 = CARTESIAN_POINT ( 'NONE',  ( -1.559171609364246924, 0.3937007874015748254, 0.7327394035119333404 ) ) ;
#36613 =( BOUNDED_CURVE ( )  B_SPLINE_CURVE ( 2, ( #55112, #61443, #17264, #29454, #80416, #22728, #24367, #49626, #81649, #36182, #16432, #5024, #61025 ),
 .UNSPECIFIED., .F., .F. ) 
 B_SPLINE_CURVE_WITH_KNOTS ( ( 3, 2, 2, 2, 2, 2, 3 ),
 ( 0.8875000000000000666, 0.8916666666666668295, 0.8958333333333334814, 0.9000000000000001332, 0.9041666666666667851, 0.9083333333333334370, 0.9125000000000000888 ),
 .UNSPECIFIED. ) 
 CURVE ( )  GEOMETRIC_REPRESENTATION_ITEM ( )  RATIONAL_B_SPLINE_CURVE ( ( 0.9999999999999991118, 0.9659258262890692004, 1.000000000000000000, 0.9659258262890683122, 1.000000000000000000, 0.9659258262890683122, 1.000000000000000000, 0.9659258262890683122, 1.000000000000000000, 0.9659258262890683122, 1.000000000000000000, 0.9659258262890674240, 1.000000000000000888 ) ) 
 REPRESENTATION_ITEM ( '' )  );
#36614 = CARTESIAN_POINT ( 'NONE',  ( 0.1958661417322834775, 0.3392501089628018884, -2.748687664041994605 ) ) ;
#36615 = CARTESIAN_POINT ( 'NONE',  ( 0.7939632545931766261, -0.2845877964562161244, -0.3641732283464567121 ) ) ;
#36616 = VERTEX_POINT ( 'NONE', #45557 ) ;
#36617 = CARTESIAN_POINT ( 'NONE',  ( -0.3949938075777409408, -0.1058382717557502933, -0.04593175853018378885 ) ) ;
#36618 = CARTESIAN_POINT ( 'NONE',  ( -0.7414698162729651543, -0.6692913385826771977, 0.1292274648535927661 ) ) ;
#36619 = ORIENTED_EDGE ( 'NONE', *, *, #81291, .T. ) ;
#36620 = CARTESIAN_POINT ( 'NONE',  ( -0.1902887139107604098, -0.5511811023622046335, 0.09757992244046803654 ) ) ;
#36621 = CARTESIAN_POINT ( 'NONE',  ( -1.404199475065615932, 0.05413385826771666132, 0.4176697321401328100 ) ) ;
#36623 = CLOSED_SHELL ( 'NONE', ( #64958, #7374, #25752, #54935, #70733, #51735, #1821, #47944, #25333, #76522, #26848, #19885, #69142, #11075, #28052, #16220, #70674, #39242, #832, #75662, #68040, #5147, #77950, #43611, #77659, #82379, #81980, #40748, #50614, #78792, #15751, #14196, #60182, #14522, #48146, #11046, #59035, #54292, #51886, #39068, #59857, #6339, #74921, #72851, #49593, #18277, #12501, #14127, #73582, #71804, #64091, #77573, #3078, #47044, #66647, #66049, #61028, #5709, #58286, #24472, #7053, #23813, #2977, #45457, #58343, #39934, #309, #28884, #32150, #73262, #35010, #24462, #57649, #44305, #76875, #11664, #76847, #5941, #34915, #41318, #31832, #7728, #23210, #5737, #25393, #67534, #57858, #55403, #57842, #76353, #25465, #11498, #55879, #38874, #2362, #74437, #72839, #31144, #17528, #13143, #79426, #34691, #77306, #66262, #2188, #67096, #66697, #36794, #62011, #30890, #77379, #12279, #10915, #25890, #52736, #14702, #58774, #42821, #82319, #43048, #55731, #17187, #65609, #42977, #61218, #5469, #71477, #75798, #54272, #29285, #72193, #21036, #26888, #66171, #67147, #31018, #62738, #498, #43515, #3646, #80808, #34219, #29759, #65220, #13620, #43768, #69699, #8530, #16801, #49553, #36730, #43829, #70097, #70096, #4241, #73139, #5762, #51057, #20883, #54303, #79323, #81613, #78731, #2287, #39454, #83155, #45513, #70149 ) ) ;
#36622 = CARTESIAN_POINT ( 'NONE',  ( 0.7217847769028878924, -0.4281496062992127816, -0.4176697321401328100 ) ) ;
#36624 = CARTESIAN_POINT ( 'NONE',  ( 0.5118110236220478892, 0.2952755905511811885, 0.000000000000000000 ) ) ;
#36625 = CARTESIAN_POINT ( 'NONE',  ( -0.3740157480314953431, -0.5400638737290845981, -0.3530559997133363437 ) ) ;
#36626 = CARTESIAN_POINT ( 'NONE',  ( 0.2867679344610366554, 0.2867679344610366554, -1.079415641241156854 ) ) ;
#36627 = CARTESIAN_POINT ( 'NONE',  ( -0.6102362204724400829, -0.5400638737290845981, -0.3530559997133363437 ) ) ;
#36628 = CARTESIAN_POINT ( 'NONE',  ( 0.1958661417322834775, 0.3392501089628018884, -2.748687664041994605 ) ) ;
#36629 = CARTESIAN_POINT ( 'NONE',  ( 1.259842519685040019, -0.1870078740157479769, 0.3641732283464567677 ) ) ;
#36630 = CARTESIAN_POINT ( 'NONE',  ( -1.174540682414697335, -0.05778040916215522460, 0.4822834645669289988 ) ) ;
#36631 = CARTESIAN_POINT ( 'NONE',  ( 0.7677165354330716118, 0.1660481256975883668, -0.3530559997133364547 ) ) ;
#36632 = CARTESIAN_POINT ( 'NONE',  ( 1.069553805774278832, 0.2952755905511810774, -0.1292274648535930714 ) ) ;
#36633 = EDGE_CURVE ( 'NONE', #43843, #22229, #12208, .T. ) ;
#36634 = CARTESIAN_POINT ( 'NONE',  ( -0.1998031496062991907, -0.3460692066303959757, -0.8530183727034120755 ) ) ;
#36635 = CARTESIAN_POINT ( 'NONE',  ( -1.482939632545930975, -0.4281496062992127816, -0.4176697321401328100 ) ) ;
#36636 = CARTESIAN_POINT ( 'NONE',  ( 0.2925321140481932369, -0.2925321140481931814, -0.3326771653543306728 ) ) ;
#36637 = CARTESIAN_POINT ( 'NONE',  ( 0.3477690288713918276, 0.2952755905511811885, 0.1292274648535926551 ) ) ;
#36638 = CARTESIAN_POINT ( 'NONE',  ( -0.3460692066303958092, -0.1998031496062994683, -2.414698162729658648 ) ) ;
#36639 = CARTESIAN_POINT ( 'NONE',  ( -1.528871391076114250, -0.5511811023622046335, 0.09757992244046803654 ) ) ;
#36640 = CARTESIAN_POINT ( 'NONE',  ( 0.6889763779527566800, -0.4536011799217367080, 0.2665933059059888421 ) ) ;
#36641 = CARTESIAN_POINT ( 'NONE',  ( 1.030183727034121421, -0.3162353388693409650, -0.4822834645669289433 ) ) ;
#36642 = CARTESIAN_POINT ( 'NONE',  ( -0.1265901696524993347, 0.4724409448818895907, -1.028215223097112663 ) ) ;
#36643 = CARTESIAN_POINT ( 'NONE',  ( 0.8530183727034128527, -0.3690944881889763329, 0.3153832671262228327 ) ) ;
#36644 = CARTESIAN_POINT ( 'NONE',  ( 0.6561679790026253567, 0.2306618581243848609, 0.2411417322834645549 ) ) ;
#36645 = CIRCLE ( 'NONE', #51402, 0.4724409448818898682 ) ;
#36646 = CARTESIAN_POINT ( 'NONE',  ( -0.3949938075777408852, -0.1058382717557502933, -0.9101049868766403206 ) ) ;
#36647 = CARTESIAN_POINT ( 'NONE',  ( -0.8530183727034112984, -0.4281496062992127816, -0.4176697321401328100 ) ) ;
#36648 = CARTESIAN_POINT ( 'NONE',  ( 0.3458507752293908943, -0.3458507752293908943, -1.120078740157480324 ) ) ;
#36649 = CARTESIAN_POINT ( 'NONE',  ( 0.9908136482939640111, 0.1771653543307087075, -0.09757992244046823083 ) ) ;
#36650 = CARTESIAN_POINT ( 'NONE',  ( -0.6299212598425188991, -0.1870078740157479769, 0.4822834645669291653 ) ) ;
#36651 = CARTESIAN_POINT ( 'NONE',  ( -0.03280839895013062252, -0.6692913385826771977, 0.1292274648535927661 ) ) ;
#36652 = CYLINDRICAL_SURFACE ( 'NONE', #2327, 0.4724409448818898682 ) ;
#36653 = CARTESIAN_POINT ( 'NONE',  ( -0.2493438320209966919, 0.05413385826771626580, -0.4176697321401330321 ) ) ;
#36654 = CARTESIAN_POINT ( 'NONE',  ( 0.2624671916010504757, 0.1283753931104748280, 0.1820866141732283561 ) ) ;
#36655 = CARTESIAN_POINT ( 'NONE',  ( -2.808244076867886019, 1.134815007188475722, 0.2514610820057449070 ) ) ;
#36656 = CARTESIAN_POINT ( 'NONE',  ( 0.07217847769028949700, -0.2845877964562159024, 0.3641732283464567677 ) ) ;
#36657 = CARTESIAN_POINT ( 'NONE',  ( 0.7939632545931766261, -0.08942795157527998196, 0.3641732283464567121 ) ) ;
#36658 = CARTESIAN_POINT ( 'NONE',  ( 0.4724409448818898682, 0.000000000000000000, -2.755905511811024056 ) ) ;
#36659 = CARTESIAN_POINT ( 'NONE',  ( 0.1070741851644054776, -0.3996062992125984925, -1.736876640419947826 ) ) ;
#36660 = CARTESIAN_POINT ( 'NONE',  ( 0.4527559055118117182, 0.1660481256975883668, -0.3530559997133364547 ) ) ;
#36661 = EDGE_CURVE ( 'NONE', #19658, #23658, #62441, .T. ) ;
#36662 = CARTESIAN_POINT ( 'NONE',  ( 4.797336870675656522E-17, -0.3917322834645670104, -1.330708661417322691 ) ) ;
#36663 = CARTESIAN_POINT ( 'NONE',  ( 1.443569553805774897, -0.5023911411419708095, -0.1820866141732282451 ) ) ;
#36664 = CARTESIAN_POINT ( 'NONE',  ( 0.4824498642376759960, 1.223219560026271499E-15, 0.4445507791589056734 ) ) ;
#36665 = CARTESIAN_POINT ( 'NONE',  ( -0.2427821522309703550, -0.08942795157528024563, -0.3641732283464568787 ) ) ;
#36666 = CARTESIAN_POINT ( 'NONE',  ( -0.1706036745406816491, 0.05413385826771626580, -0.4176697321401330321 ) ) ;
#36667 = CARTESIAN_POINT ( 'NONE',  ( 1.174540682414699111, -0.2845877964562159024, 0.3641732283464567677 ) ) ;
#36668 = CARTESIAN_POINT ( 'NONE',  ( -0.2952755905511810774, -3.179810529374183920E-17, 5.879133660591329580 ) ) ;
#36669 = CARTESIAN_POINT ( 'NONE',  ( 1.384514435695538337, -0.5511811023622046335, 0.09757992244046803654 ) ) ;
#36670 = CARTESIAN_POINT ( 'NONE',  ( -0.06561679790026180015, 0.05413385826771666132, 0.4176697321401328100 ) ) ;
#36671 = CARTESIAN_POINT ( 'NONE',  ( 1.312335958005250269, -0.6046776061558807314, 0.2411417322834647770 ) ) ;
#36672 = CARTESIAN_POINT ( 'NONE',  ( 0.1938976377952755792, -0.1938976377952756069, 0.09542247959850379269 ) ) ;
#36673 = CARTESIAN_POINT ( 'NONE',  ( 0.03937007874015806264, 0.2952755905511811885, 0.000000000000000000 ) ) ;
#36674 = CARTESIAN_POINT ( 'NONE',  ( 1.489501312335958172, -0.3162353388693405765, 0.4822834645669290543 ) ) ;
#36675 = CARTESIAN_POINT ( 'NONE',  ( 0.4330708661417329575, 0.2952755905511811885, 0.000000000000000000 ) ) ;
#36676 = CARTESIAN_POINT ( 'NONE',  ( 0.2362204724409451007, -0.4091458600556402980, -0.3261154855643044748 ) ) ;
#36677 = CARTESIAN_POINT ( 'NONE',  ( 0.8923884514435703741, 0.1283753931104748280, 0.1820866141732283561 ) ) ;
#36678 = CARTESIAN_POINT ( 'NONE',  ( 1.364829396325460076, 0.2306618581243848609, 0.2411417322834645549 ) ) ;
#36679 = B_SPLINE_CURVE_WITH_KNOTS ( 'NONE', 3,
 ( #47145, #72835, #15185, #15603, #40842, #67358, #78329 ),
 .UNSPECIFIED., .F., .F.,
 ( 4, 3, 4 ),
 ( 3.642919299551294898E-17, 0.001246232571205267226, 0.002492492258783278024 ),
 .UNSPECIFIED. ) ;
#36680 = CARTESIAN_POINT ( 'NONE',  ( 0.02624671916010564918, 0.1283753931104748280, 0.1820866141732283561 ) ) ;
#36681 = CARTESIAN_POINT ( 'NONE',  ( -0.2755905511811015396, -0.6692913385826771977, 8.415575281601705876E-17 ) ) ;
#36682 = CARTESIAN_POINT ( 'NONE',  ( 0.6955380577427828781, 0.05413385826771626580, -0.4176697321401330321 ) ) ;
#36683 = CARTESIAN_POINT ( 'NONE',  ( -0.6824146981627288167, 0.2306618581243848609, 0.2411417322834645549 ) ) ;
#36684 = VECTOR ( 'NONE', #70106, 39.37007874015748143 ) ;
#36685 = CARTESIAN_POINT ( 'NONE',  ( -0.3346456692913377662, -0.4536011799217367080, 0.2665933059059888421 ) ) ;
#36686 = CARTESIAN_POINT ( 'NONE',  ( 0.5971128608923890191, -0.6692913385826771977, 0.1292274648535927661 ) ) ;
#36687 = CARTESIAN_POINT ( 'NONE',  ( 1.017060367454068803, -0.2845877964562159024, 0.3641732283464567677 ) ) ;
#36688 = CARTESIAN_POINT ( 'NONE',  ( 0.09186351706036827158, 0.05413385826771666132, 0.4176697321401328100 ) ) ;
#36689 = FACE_OUTER_BOUND ( 'NONE', #65322, .T. ) ;
#36691 = CARTESIAN_POINT ( 'NONE',  ( 0.3996062992125979929, -0.1070741851644065740, -1.213910761154855411 ) ) ;
#36690 = CARTESIAN_POINT ( 'NONE',  ( 0.9881811337016640495, 0.000000000000000000, 0.5314960629921260393 ) ) ;
#36692 = CARTESIAN_POINT ( 'NONE',  ( -0.4624320255261038515, -2.191421614605370878E-15, 0.4445507791589071167 ) ) ;
#36693 = CARTESIAN_POINT ( 'NONE',  ( -0.1958661417322834220, -0.3392501089628018884, -2.104986876640420057 ) ) ;
#36694 = CARTESIAN_POINT ( 'NONE',  ( -1.141732283464566011, 0.2952755905511811885, 0.000000000000000000 ) ) ;
#36695 = CARTESIAN_POINT ( 'NONE',  ( -0.4921259842519677963, -0.5400638737290844871, 0.3530559997133364547 ) ) ;
#36696 = CARTESIAN_POINT ( 'NONE',  ( -0.4091458600556402980, -0.2362204724409451284, -0.5249343832020997302 ) ) ;
#36697 = CARTESIAN_POINT ( 'NONE',  ( 0.1058382717557500713, -0.3949938075777409408, -2.604986876640420501 ) ) ;
#36698 = ORIENTED_EDGE ( 'NONE', *, *, #815, .T. ) ;
#36699 = CARTESIAN_POINT ( 'NONE',  ( 0.1968503937007881344, -0.5511811023622047445, 6.969142054262312111E-17 ) ) ;
#36701 = CARTESIAN_POINT ( 'NONE',  ( -9.594673741351313045E-17, 0.3917322834645670104, -1.251968503937008093 ) ) ;
#36700 = AXIS2_PLACEMENT_3D ( 'NONE', #18576, #45886, #39593 ) ;
#36702 = CARTESIAN_POINT ( 'NONE',  ( 0.5249343832021003964, 0.2306618581243847221, -0.2411417322834647770 ) ) ;
#36703 = CARTESIAN_POINT ( 'NONE',  ( 0.4724409448818898682, 2.892866454678787531E-17, -2.637795275590551380 ) ) ;
#36704 = LINE ( 'NONE', #62378, #34588 ) ;
#36705 = CARTESIAN_POINT ( 'NONE',  ( -1.666666666666665853, -0.004921259842519870586, -0.3153832671262229437 ) ) ;
#36706 = CARTESIAN_POINT ( 'NONE',  ( 1.076115485564305141, 0.2306618581243847221, -0.2411417322834647770 ) ) ;
#36707 = CARTESIAN_POINT ( 'NONE',  ( 1.456692913385827515, 0.1771653543307087630, 0.000000000000000000 ) ) ;
#36708 = CARTESIAN_POINT ( 'NONE',  ( 0.06561679790026316017, -0.4281496062992124485, 0.4176697321401328655 ) ) ;
#36709 = CARTESIAN_POINT ( 'NONE',  ( 0.3917322834645668994, 0.1049643490035304522, -0.8346263535094994301 ) ) ;
#36710 = CARTESIAN_POINT ( 'NONE',  ( -0.3412073490813641308, 0.2306618581243847221, -0.2411417322834647770 ) ) ;
#36711 = CARTESIAN_POINT ( 'NONE',  ( -1.102362204724408601, -0.1870078740157479769, 0.3641732283464567677 ) ) ;
#36712 = CARTESIAN_POINT ( 'NONE',  ( 0.5643044619422579178, -0.4281496062992127816, -0.4176697321401328100 ) ) ;
#36713 = CARTESIAN_POINT ( 'NONE',  ( -0.6561679790026240244, -0.6046776061558807314, 0.2411417322834647770 ) ) ;
#36714 = CARTESIAN_POINT ( 'NONE',  ( -1.191801538614237099, -5.582469467804009507E-15, -0.4118484887281986251 ) ) ;
#36715 = DIRECTION ( 'NONE',  ( 1.000000000000000000, -0.000000000000000000, 1.224646799147353207E-16 ) ) ;
#36716 = ORIENTED_EDGE ( 'NONE', *, *, #47083, .F. ) ;
#36717 = CARTESIAN_POINT ( 'NONE',  ( 0.1049643490035304799, -0.3917322834645670104, -1.971804092684726228 ) ) ;
#36718 = CARTESIAN_POINT ( 'NONE',  ( 0.3805774278215230400, -0.4281496062992124485, 0.4176697321401328655 ) ) ;
#36719 = CARTESIAN_POINT ( 'NONE',  ( -0.1902887139107604098, -0.6692913385826771977, 0.1292274648535927661 ) ) ;
#36720 = CARTESIAN_POINT ( 'NONE',  ( -1.443569553805773564, 0.2306618581243847221, -0.2411417322834647770 ) ) ;
#36721 = CARTESIAN_POINT ( 'NONE',  ( 1.259842519685040019, -0.1870078740157479769, 0.4822834645669291653 ) ) ;
#36722 = CARTESIAN_POINT ( 'NONE',  ( 0.3083989501312343062, -0.05778040916215560624, -0.4822834645669293319 ) ) ;
#36723 = CARTESIAN_POINT ( 'NONE',  ( -0.1049643490035302024, -0.3917322834645671215, -0.7867454068241470644 ) ) ;
#36724 = CARTESIAN_POINT ( 'NONE',  ( -0.8595800524934373854, -0.3162353388693409650, -0.4822834645669289433 ) ) ;
#36725 = CARTESIAN_POINT ( 'NONE',  ( 0.3477690288713918276, -0.6692913385826773087, -0.1292274648535924053 ) ) ;
#36726 = CARTESIAN_POINT ( 'NONE',  ( -0.4790026246719152336, -0.05778040916215560624, -0.4822834645669293319 ) ) ;
#36727 = CARTESIAN_POINT ( 'NONE',  ( 0.4068241469816281097, -0.004921259842519576551, 0.3153832671262227771 ) ) ;
#36728 = CARTESIAN_POINT ( 'NONE',  ( 1.574803149606299746, -0.1870078740157480601, -0.3641732283464567677 ) ) ;
#36729 = CARTESIAN_POINT ( 'NONE',  ( -0.2373513483963055337, -0.1756490242921440736, 5.678081160219037749 ) ) ;
#36730 = ADVANCED_FACE ( 'NONE', ( #14854 ), #39821, .F. ) ;
#36731 = CARTESIAN_POINT ( 'NONE',  ( 0.1509186351706042484, -0.3162353388693405765, 0.4822834645669290543 ) ) ;
#36732 = DIRECTION ( 'NONE',  ( 8.881784197001252323E-16, 1.460819769243627131E-15, -1.000000000000000000 ) ) ;
#36733 = CARTESIAN_POINT ( 'NONE',  ( 1.555118110236221041, -0.5400638737290844871, 0.3530559997133364547 ) ) ;
#36734 = CARTESIAN_POINT ( 'NONE',  ( -0.3392501089628017219, -0.1958661417322836718, -2.721784776902886893 ) ) ;
#36735 = ORIENTED_EDGE ( 'NONE', *, *, #59271, .T. ) ;
#36736 = ORIENTED_EDGE ( 'NONE', *, *, #10612, .T. ) ;
#36737 = CARTESIAN_POINT ( 'NONE',  ( 0.8595800524934390507, -0.3162353388693405765, 0.4822834645669290543 ) ) ;
#36738 = CARTESIAN_POINT ( 'NONE',  ( 0.1771653543307093182, 0.07958543189024085140, 0.2665933059059887866 ) ) ;
#36740 = LINE ( 'NONE', #37979, #59948 ) ;
#36739 = CARTESIAN_POINT ( 'NONE',  ( -1.022773273020813667, 1.648670715164695544, 0.4614513048051138155 ) ) ;
#36741 = CARTESIAN_POINT ( 'NONE',  ( -0.2867679344610365999, 0.2867679344610364889, -0.7342519685039372579 ) ) ;
#36742 = CARTESIAN_POINT ( 'NONE',  ( -0.3458507752293909498, 0.3458507752293907833, 0.2185039370078740162 ) ) ;
#36743 = CARTESIAN_POINT ( 'NONE',  ( 0.7201575634750010391, 1.521610601467410833E-15, 0.3791483426435167670 ) ) ;
#36744 = CARTESIAN_POINT ( 'NONE',  ( -0.1070741851644051862, -0.3996062992125986590, -2.511154855643044748 ) ) ;
#36745 = CARTESIAN_POINT ( 'NONE',  ( 0.6036745406824153282, -0.6046776061558807314, 0.2411417322834647770 ) ) ;
#36746 = CARTESIAN_POINT ( 'NONE',  ( -1.246719160104985846, -0.4281496062992127816, -0.4176697321401328100 ) ) ;
#36747 = AXIS2_PLACEMENT_3D ( 'NONE', #71056, #39053, #77370 ) ;
#36748 = CARTESIAN_POINT ( 'NONE',  ( -1.227034120734907585, 0.2952755905511811885, 0.1292274648535926551 ) ) ;
#36749 = CARTESIAN_POINT ( 'NONE',  ( 0.8661417322834652488, -0.1870078740157480879, -0.4822834645669291653 ) ) ;
#36750 = CARTESIAN_POINT ( 'NONE',  ( 1.423884514435696191, -0.05778040916215522460, 0.4822834645669289988 ) ) ;
#36751 = CARTESIAN_POINT ( 'NONE',  ( 1.450131233595801428, -0.5511811023622048555, -0.09757992244046775898 ) ) ;
#36752 = CONTEXT_DEPENDENT_SHAPE_REPRESENTATION ( #62705, #15807 ) ;
#36753 = CARTESIAN_POINT ( 'NONE',  ( 1.135170603674541256, -0.5511811023622048555, -0.09757992244046775898 ) ) ;
#36754 = CARTESIAN_POINT ( 'NONE',  ( -0.7874015748031489847, -0.1870078740157480879, -0.4822834645669291653 ) ) ;
#36755 = CARTESIAN_POINT ( 'NONE',  ( 0.1998031496062994128, -0.3460692066303957537, -0.3261154855643044748 ) ) ;
#36756 = CARTESIAN_POINT ( 'NONE',  ( 1.417322834645670104, -0.1870078740157480879, -0.4822834645669291653 ) ) ;
#36757 = CARTESIAN_POINT ( 'NONE',  ( 0.3917322834645669549, 0.1049643490035304660, -0.2742782152230970327 ) ) ;
#36758 = CARTESIAN_POINT ( 'NONE',  ( -0.3740157480314953431, 0.1660481256975885056, 0.3530559997133364547 ) ) ;
#36760 = CARTESIAN_POINT ( 'NONE',  ( 0.4768132735438215253, 1.796500554427757690, -0.5050878842330656093 ) ) ;
#36759 = CARTESIAN_POINT ( 'NONE',  ( 1.325459317585302665, -0.4281496062992124485, 0.4176697321401328655 ) ) ;
#36761 = CARTESIAN_POINT ( 'NONE',  ( -1.069553805774277722, 0.1771653543307087630, 0.09757992244046791164 ) ) ;
#36762 = CARTESIAN_POINT ( 'NONE',  ( 0.2887139107611556010, 0.2306618581243847221, -0.2411417322834647770 ) ) ;
#36763 = CARTESIAN_POINT ( 'NONE',  ( 0.9120734908136489683, -0.5511811023622046335, 0.09757992244046803654 ) ) ;
#36764 = CARTESIAN_POINT ( 'NONE',  ( -0.3392501089628019439, 0.1958661417322832554, -1.838563361383515504 ) ) ;
#36765 = AXIS2_PLACEMENT_3D ( 'NONE', #19428, #81775, #76275 ) ;
#36766 = CARTESIAN_POINT ( 'NONE',  ( -1.115485564304461219, -0.3690944881889763329, 0.3153832671262228327 ) ) ;
#36767 = CARTESIAN_POINT ( 'NONE',  ( 0.7545931758530189937, 0.2952755905511810774, -0.1292274648535930714 ) ) ;
#36768 = DIRECTION ( 'NONE',  ( -3.491481338843132961E-15, -0.000000000000000000, 1.000000000000000000 ) ) ;
#36769 = CARTESIAN_POINT ( 'NONE',  ( -0.4724409448818890911, -0.1870078740157479769, 0.3641732283464567677 ) ) ;
#36770 = CARTESIAN_POINT ( 'NONE',  ( -0.2230971128608915943, -0.4281496062992127816, -0.4176697321401328100 ) ) ;
#36771 = CARTESIAN_POINT ( 'NONE',  ( -1.482939632545930975, -0.004921259842519576551, 0.3153832671262227771 ) ) ;
#36772 = CARTESIAN_POINT ( 'NONE',  ( -0.8333333333333323711, -0.6692913385826773087, -0.1292274648535924053 ) ) ;
#36773 = CARTESIAN_POINT ( 'NONE',  ( 1.292650918635171564, -0.6692913385826773087, -0.1292274648535924053 ) ) ;
#36774 = CARTESIAN_POINT ( 'NONE',  ( -9.594673741351313045E-17, 0.3917322834645670659, -0.3116991058080859078 ) ) ;
#36775 = CARTESIAN_POINT ( 'NONE',  ( -0.7939632545931750718, -0.08942795157528024563, -0.3641732283464568787 ) ) ;
#36776 = CARTESIAN_POINT ( 'NONE',  ( 1.122040030454554138, 1.063009187292368596, 0.03164884633124447760 ) ) ;
#36777 = CARTESIAN_POINT ( 'NONE',  ( 1.430446194225722500, 0.05413385826771666132, 0.4176697321401328100 ) ) ;
#36778 = CARTESIAN_POINT ( 'NONE',  ( 0.4724409448818897572, -0.1265901696524988906, -2.235564304461942431 ) ) ;
#36779 = CARTESIAN_POINT ( 'NONE',  ( -1.358267716535432434, 0.1660481256975883668, -0.3530559997133364547 ) ) ;
#36780 = CARTESIAN_POINT ( 'NONE',  ( 1.686351706036745890, 0.2952755905511811885, 0.1292274648535926551 ) ) ;
#36781 = CARTESIAN_POINT ( 'NONE',  ( -0.7874015748031489847, -0.1870078740157479769, 0.3641732283464567677 ) ) ;
#36782 = EDGE_CURVE ( 'NONE', #6582, #17097, #73978, .T. ) ;
#36783 = CARTESIAN_POINT ( 'NONE',  ( 0.4935044252197980930, 1.488513638086841118, 0.5309055118110234117 ) ) ;
#36784 = CARTESIAN_POINT ( 'NONE',  ( -0.006561679790025524116, -0.05778040916215560624, -0.4822834645669293319 ) ) ;
#36785 = CARTESIAN_POINT ( 'NONE',  ( 0.05905511811023709395, -0.4536011799217367080, 0.2665933059059888421 ) ) ;
#36786 = CARTESIAN_POINT ( 'NONE',  ( -1.279527559055116948, -0.4536011799217367080, 0.2665933059059888421 ) ) ;
#36787 = CARTESIAN_POINT ( 'NONE',  ( -1.358267716535432434, 0.1660481256975883668, -0.3530559997133364547 ) ) ;
#36788 = CARTESIAN_POINT ( 'NONE',  ( 1.174540682414699111, -0.08942795157528024563, -0.3641732283464568787 ) ) ;
#36789 = CARTESIAN_POINT ( 'NONE',  ( 1.036745406824147731, 0.05413385826771666132, 0.4176697321401328100 ) ) ;
#36790 = CARTESIAN_POINT ( 'NONE',  ( 0.4426149705447037230, 1.366040861858875077, 2.104991000353118480 ) ) ;
#36791 = CARTESIAN_POINT ( 'NONE',  ( 0.4199475065616805614, 0.1283753931104748280, 0.1820866141732283561 ) ) ;
#36792 = DIMENSIONAL_EXPONENTS ( 1.000000000000000000, 0.000000000000000000, 0.000000000000000000, 0.000000000000000000, 0.000000000000000000, 0.000000000000000000, 0.000000000000000000 ) ;
#36793 = CARTESIAN_POINT ( 'NONE',  ( 1.043307086614173818, 0.1660481256975885056, 0.3530559997133364547 ) ) ;
#36794 = ADVANCED_FACE ( 'NONE', ( #40325 ), #80211, .F. ) ;
#36795 = CARTESIAN_POINT ( 'NONE',  ( 0.8923884514435701520, -0.5023911411419708095, -0.1820866141732282451 ) ) ;
#36796 = VERTEX_POINT ( 'NONE', #32609 ) ;
#36797 = CARTESIAN_POINT ( 'NONE',  ( -1.410761154855641575, -0.3162353388693409650, -0.4822834645669289433 ) ) ;
#36798 = CARTESIAN_POINT ( 'NONE',  ( -0.7349081364829387342, -0.6046776061558807314, 0.2411417322834647770 ) ) ;
#36799 = CARTESIAN_POINT ( 'NONE',  ( -0.1706036745406816491, -0.4281496062992124485, 0.4176697321401328655 ) ) ;
#36800 = DIRECTION ( 'NONE',  ( -0.000000000000000000, -1.000000000000000000, -0.000000000000000000 ) ) ;
#36801 = CARTESIAN_POINT ( 'NONE',  ( -0.3996062992125985480, -7.340648628747423112E-17, -2.635826771653543066 ) ) ;
#36802 = CARTESIAN_POINT ( 'NONE',  ( 0.6561679790026253567, 0.2306618581243848609, 0.2411417322834645549 ) ) ;
#36803 = CARTESIAN_POINT ( 'NONE',  ( 1.601049868766404982, 0.1283753931104748280, 0.1820866141732283561 ) ) ;
#36804 = CARTESIAN_POINT ( 'NONE',  ( 0.05905511811023709395, -0.5400638737290844871, 0.3530559997133364547 ) ) ;
#36805 = CARTESIAN_POINT ( 'NONE',  ( 0.9251968503937015864, -0.5400638737290844871, 0.3530559997133364547 ) ) ;
#36806 = CARTESIAN_POINT ( 'NONE',  ( 0.3460692066303959757, -0.1998031496062991907, -1.994750656167979086 ) ) ;
#36807 = CARTESIAN_POINT ( 'NONE',  ( -0.1058382717557497937, -0.3949938075777411628, -1.332020997375328086 ) ) ;
#36808 = CARTESIAN_POINT ( 'NONE',  ( -0.4497483405553294178, 1.383294989906824313, 1.028048643305481846 ) ) ;
#36809 = FACE_OUTER_BOUND ( 'NONE', #55318, .T. ) ;
#36810 = AXIS2_PLACEMENT_3D ( 'NONE', #26972, #34129, #71597 ) ;
#36811 = CARTESIAN_POINT ( 'NONE',  ( -0.1049643490035307020, 0.3917322834645669549, -0.7860892388451442558 ) ) ;
#36812 = CARTESIAN_POINT ( 'NONE',  ( -0.5118110236220466680, -0.5511811023622047445, 6.969142054262312111E-17 ) ) ;
#36813 = CARTESIAN_POINT ( 'NONE',  ( -0.8792650918635160906, 0.05413385826771626580, -0.4176697321401330321 ) ) ;
#36814 = CARTESIAN_POINT ( 'NONE',  ( 0.3740157480314966754, 0.1660481256975883668, -0.3530559997133364547 ) ) ;
#36815 = CARTESIAN_POINT ( 'NONE',  ( -0.3949938075777408852, -0.1058382717557502933, -2.484908136482939955 ) ) ;
#36816 = EDGE_CURVE ( 'NONE', #57928, #3606, #28310, .T. ) ;
#36817 = CARTESIAN_POINT ( 'NONE',  ( 0.7742782152230979209, 0.05413385826771626580, -0.4176697321401330321 ) ) ;
#36818 = CARTESIAN_POINT ( 'NONE',  ( 1.502624671916010790, -0.3162353388693409650, -0.4822834645669289433 ) ) ;
#36819 = CARTESIAN_POINT ( 'NONE',  ( 1.299212598425197429, 0.2952755905511811885, 0.000000000000000000 ) ) ;
#36820 = CARTESIAN_POINT ( 'NONE',  ( 0.1265901696524989462, 0.4724409448818897572, -2.513123359580052174 ) ) ;
#36821 = CARTESIAN_POINT ( 'NONE',  ( -0.2925321140481930704, -0.2925321140481933480, -2.263779527559055094 ) ) ;
#36822 = FACE_OUTER_BOUND ( 'NONE', #78598, .T. ) ;
#36823 = CARTESIAN_POINT ( 'NONE',  ( 1.010498687664042716, 0.05413385826771626580, -0.4176697321401330321 ) ) ;
#36824 = CARTESIAN_POINT ( 'NONE',  ( 0.5118110236220478892, 0.2952755905511811885, 0.000000000000000000 ) ) ;
#36825 = EDGE_CURVE ( 'NONE', #20402, #1757, #49313, .T. ) ;
#36826 = CIRCLE ( 'NONE', #82550, 0.5118110236220471121 ) ;
#36827 = CARTESIAN_POINT ( 'NONE',  ( 1.253280839895013710, -0.2845877964562159024, 0.3641732283464567677 ) ) ;
#36829 = CARTESIAN_POINT ( 'NONE',  ( 1.515748031496063186, -0.5400638737290845981, -0.3530559997133363437 ) ) ;
#36828 = CARTESIAN_POINT ( 'NONE',  ( -1.509186351706035767, -0.3690944881889763329, 0.3153832671262228327 ) ) ;
#36830 = CARTESIAN_POINT ( 'NONE',  ( -0.3392501089628018329, -0.1958661417322836440, -2.652211655346770502 ) ) ;
#36831 = LENGTH_MEASURE_WITH_UNIT ( LENGTH_MEASURE( 0.02539999999999999897 ), #30099 );
#36832 = CARTESIAN_POINT ( 'NONE',  ( 0.7086614173228353852, -0.1870078740157479769, 0.4822834645669291653 ) ) ;
#36833 = CARTESIAN_POINT ( 'NONE',  ( 1.522309711286089939, 0.1283753931104748280, 0.1820866141732283561 ) ) ;
#36834 = CARTESIAN_POINT ( 'NONE',  ( -0.4461942257217840213, 0.2306618581243848609, 0.2411417322834645549 ) ) ;
#36835 = CARTESIAN_POINT ( 'NONE',  ( -0.7152230971128602510, -0.05778040916215560624, -0.4822834645669293319 ) ) ;
#36836 = CARTESIAN_POINT ( 'NONE',  ( 1.384514435695538337, -0.6692913385826771977, 0.1292274648535927661 ) ) ;
#36837 = CARTESIAN_POINT ( 'NONE',  ( -0.3392501089628017219, -0.1958661417322836718, 0.02034120734908127781 ) ) ;
#36838 = CARTESIAN_POINT ( 'NONE',  ( 0.1049643490035303689, 0.3917322834645670104, -1.717847769028871596 ) ) ;
#36839 = CARTESIAN_POINT ( 'NONE',  ( -0.3917322834645671215, 0.1049643490035301469, -2.387139107611548905 ) ) ;
#36840 = EDGE_CURVE ( 'NONE', #42095, #50308, #67999, .T. ) ;
#36841 = CARTESIAN_POINT ( 'NONE',  ( 1.653543307086614789, -0.1870078740157479769, 0.4822834645669291653 ) ) ;
#36842 = VERTEX_POINT ( 'NONE', #78076 ) ;
#36843 = CARTESIAN_POINT ( 'NONE',  ( -0.1058382717557503211, 0.3949938075777409408, -2.841207349081365408 ) ) ;
#36844 = VERTEX_POINT ( 'NONE', #65454 ) ;
#36845 = DIRECTION ( 'NONE',  ( -0.6427876096865343669, 0.7660444431189822323, 0.000000000000000000 ) ) ;
#36846 = CARTESIAN_POINT ( 'NONE',  ( 1.423884514435696191, -0.08942795157527998196, 0.3641732283464567121 ) ) ;
#36847 = CARTESIAN_POINT ( 'NONE',  ( -0.3996062992125986035, -0.1070741851644056997, -1.148293963254592986 ) ) ;
#36848 = CARTESIAN_POINT ( 'NONE',  ( 0.4177787735907000366, 1.299212598425196985, -1.559171609364239375 ) ) ;
#36849 = CARTESIAN_POINT ( 'NONE',  ( -0.4724409448818898682, -8.678599364036362592E-17, -0.7460629921259841479 ) ) ;
#36850 = CARTESIAN_POINT ( 'NONE',  ( -0.5314960629921146040, 2.742781086379890265, -3.250800424960315294 ) ) ;
#36851 = CARTESIAN_POINT ( 'NONE',  ( 0.2362204724409449064, 1.566969329617675860E-17, -0.1279527559055117503 ) ) ;
#36852 = CARTESIAN_POINT ( 'NONE',  ( -0.3917322834645671215, 0.1049643490035301469, -0.5898950131233595684 ) ) ;
#36853 = CARTESIAN_POINT ( 'NONE',  ( -0.8398950131233585692, 0.1283753931104748280, 0.1820866141732283561 ) ) ;
#36854 = CARTESIAN_POINT ( 'NONE',  ( -1.023622047244094002, -0.1870078740157480601, -0.3641732283464567677 ) ) ;
#36855 = CARTESIAN_POINT ( 'NONE',  ( 0.7086614173228352742, -0.1870078740157480879, -0.4822834645669291653 ) ) ;
#36856 = CARTESIAN_POINT ( 'NONE',  ( -1.148293963254592542, 0.2952755905511811885, 0.1292274648535926551 ) ) ;
#36857 = CARTESIAN_POINT ( 'NONE',  ( 0.3917322834645669549, 0.1049643490035304660, -0.2742782152230970327 ) ) ;
#36858 = ORIENTED_EDGE ( 'NONE', *, *, #20829, .F. ) ;
#36859 = CARTESIAN_POINT ( 'NONE',  ( 1.528871391076116026, -0.6692913385826773087, -0.1292274648535924053 ) ) ;
#36860 = FACE_OUTER_BOUND ( 'NONE', #26449, .T. ) ;
#36861 = DIRECTION ( 'NONE',  ( 0.000000000000000000, 1.000000000000000000, 0.000000000000000000 ) ) ;
#36862 = CARTESIAN_POINT ( 'NONE',  ( 0.1265901696524990294, -0.4724409448818896462, -1.817585301837270517 ) ) ;
#36863 = CARTESIAN_POINT ( 'NONE',  ( 2.170146923806595129, 1.537401574803149984, 0.4744094488188975722 ) ) ;
#36864 = CARTESIAN_POINT ( 'NONE',  ( 0.1958661417322834775, 0.3392501089628018884, -2.748687664041994605 ) ) ;
#36865 = CARTESIAN_POINT ( 'NONE',  ( -1.076115485564303809, -0.6046776061558809534, -0.2411417322834644161 ) ) ;
#36866 = CARTESIAN_POINT ( 'NONE',  ( 0.8136482939632553313, -0.6046776061558809534, -0.2411417322834644161 ) ) ;
#36868 = CARTESIAN_POINT ( 'NONE',  ( 0.6627296587926515548, 0.2066929133858267931, 0.1054918080437490802 ) ) ;
#36867 = CARTESIAN_POINT ( 'NONE',  ( 0.5314960629921062774, 2.742776604255995565, 1.881759016064410428 ) ) ;
#36869 = DIRECTION ( 'NONE',  ( 1.000000000000000000, -0.000000000000000000, -0.000000000000000000 ) ) ;
#36870 = CARTESIAN_POINT ( 'NONE',  ( -1.207349081364828880, 0.2306618581243847221, -0.2411417322834647770 ) ) ;
#36871 = CARTESIAN_POINT ( 'NONE',  ( 0.3392501089628018329, 0.1958661417322835052, -0.5262274033782657900 ) ) ;
#36872 = CARTESIAN_POINT ( 'NONE',  ( -0.04593175853018302557, -0.5511811023622048555, -0.09757992244046775898 ) ) ;
#36873 = CARTESIAN_POINT ( 'NONE',  ( 0.1049643490035303689, 0.3917322834645670104, -1.022965879265091749 ) ) ;
#36874 = AXIS2_PLACEMENT_3D ( 'NONE', #17939, #75186, #17532 ) ;
#36875 = CARTESIAN_POINT ( 'NONE',  ( -0.03280839895013062252, 0.1771653543307087075, -0.09757992244046823083 ) ) ;
#36876 = CARTESIAN_POINT ( 'NONE',  ( 0.4396325459317590445, -0.5511811023622046335, 0.09757992244046803654 ) ) ;
#36877 = CARTESIAN_POINT ( 'NONE',  ( 0.3805774278215230400, 0.05413385826771626580, -0.4176697321401330321 ) ) ;
#36878 = CARTESIAN_POINT ( 'NONE',  ( -0.8989501312335946848, -0.5511811023622046335, 0.09757992244046803654 ) ) ;
#36879 = CARTESIAN_POINT ( 'NONE',  ( 0.1958661417322834775, 0.3392501089628018884, -2.183727034120734878 ) ) ;
#36880 = CARTESIAN_POINT ( 'NONE',  ( 1.463254593175853824, 0.2952755905511810774, -0.1292274648535930714 ) ) ;
#36881 = CARTESIAN_POINT ( 'NONE',  ( -1.056430446194224881, -0.6692913385826771977, 0.1292274648535927661 ) ) ;
#36882 = CARTESIAN_POINT ( 'NONE',  ( -0.4091458600556402980, -0.2362204724409451284, -0.7591863517060367661 ) ) ;
#36883 = CARTESIAN_POINT ( 'NONE',  ( -0.1574803149606292529, -0.1870078740157479769, 0.4822834645669291653 ) ) ;
#36884 = EDGE_CURVE ( 'NONE', #2979, #28061, #72137, .T. ) ;
#36885 = CARTESIAN_POINT ( 'NONE',  ( -0.3674540682414689785, 0.2306618581243848609, 0.2411417322834645549 ) ) ;
#36886 = CARTESIAN_POINT ( 'NONE',  ( 1.430446194225722500, -0.3690944881889765550, -0.3153832671262227771 ) ) ;
#36887 = AXIS2_PLACEMENT_3D ( 'NONE', #31937, #57598, #7949 ) ;
#36888 = CARTESIAN_POINT ( 'NONE',  ( 0.1574803149606306130, -0.1870078740157479769, 0.3641732283464567677 ) ) ;
#36889 = CARTESIAN_POINT ( 'NONE',  ( -0.1246719160104980823, 0.2952755905511811885, 0.1292274648535926551 ) ) ;
#36890 = CARTESIAN_POINT ( 'NONE',  ( -1.351706036745406347, -0.4281496062992124485, 0.4176697321401328655 ) ) ;
#36891 = CARTESIAN_POINT ( 'NONE',  ( -0.6575345472709128725, 1.929133858267715773, -0.5309055118110235227 ) ) ;
#36892 = CARTESIAN_POINT ( 'NONE',  ( 1.633858267716535639, -0.4536011799217367080, 0.2665933059059888421 ) ) ;
#36893 = CARTESIAN_POINT ( 'NONE',  ( -0.09186351706036663400, -0.4281496062992124485, 0.4176697321401328655 ) ) ;
#36894 = VERTEX_POINT ( 'NONE', #26291 ) ;
#36895 = CARTESIAN_POINT ( 'NONE',  ( 0.1998031496062994128, -0.3460692066303957537, -1.900918635170603554 ) ) ;
#36896 = CARTESIAN_POINT ( 'NONE',  ( 1.364829396325459854, -0.6046776061558809534, -0.2411417322834644161 ) ) ;
#36897 = CARTESIAN_POINT ( 'NONE',  ( -0.7545931758530177724, 0.1771653543307087630, 0.09757992244046791164 ) ) ;
#36898 = CARTESIAN_POINT ( 'NONE',  ( -0.4199475065616791736, 0.2306618581243847221, -0.2411417322834647770 ) ) ;
#36899 = CARTESIAN_POINT ( 'NONE',  ( 1.318897637795276356, -0.5400638737290844871, 0.3530559997133364547 ) ) ;
#36900 = CARTESIAN_POINT ( 'NONE',  ( 0.8464566929133866546, -0.5400638737290844871, 0.3530559997133364547 ) ) ;
#36901 = CARTESIAN_POINT ( 'NONE',  ( -1.528871391076114250, -0.6692913385826771977, 0.1292274648535927661 ) ) ;
#36902 = CARTESIAN_POINT ( 'NONE',  ( -1.167979002624671470, -0.3690944881889765550, -0.3153832671262227771 ) ) ;
#36903 = CARTESIAN_POINT ( 'NONE',  ( -0.1998031496062991630, -0.3460692066303959202, -0.2998687664041995160 ) ) ;
#36904 = CARTESIAN_POINT ( 'NONE',  ( -0.3460692066303958092, -0.1998031496062994683, -0.3674540682414698112 ) ) ;
#36905 = CARTESIAN_POINT ( 'NONE',  ( 0.2891555358219910499, -0.2891555358219909944, -0.2559055118110237226 ) ) ;
#36906 = CARTESIAN_POINT ( 'NONE',  ( 0.4725409811166971785, 1.494519345219279094, 2.558828502325778853 ) ) ;
#36907 = CARTESIAN_POINT ( 'NONE',  ( 1.581364829396326277, -0.2845877964562161244, -0.3641732283464567121 ) ) ;
#36908 = CARTESIAN_POINT ( 'NONE',  ( 0.9317585301837276734, -0.3690944881889763329, 0.3153832671262228327 ) ) ;
#36909 = CARTESIAN_POINT ( 'NONE',  ( 0.3412073490813655186, 0.2306618581243848609, 0.2411417322834645549 ) ) ;
#36910 = CARTESIAN_POINT ( 'NONE',  ( 0.2491186766705762723, -0.1588297147722000924, 0.1541304905092664712 ) ) ;
#36911 = CARTESIAN_POINT ( 'NONE',  ( 0.3949938075777409963, 2.418639510665530743E-17, -0.9822834645669292764 ) ) ;
#36912 = CARTESIAN_POINT ( 'NONE',  ( 0.6102362204724416372, 0.07958543189024071263, -0.2665933059059888421 ) ) ;
#36913 = CARTESIAN_POINT ( 'NONE',  ( -0.3280839895013117347, 0.05413385826771626580, -0.4176697321401330321 ) ) ;
#36914 = CARTESIAN_POINT ( 'NONE',  ( -0.7480314960629914633, -0.6692913385826771977, 8.415575281601705876E-17 ) ) ;
#36915 = CARTESIAN_POINT ( 'NONE',  ( 1.227034120734908917, 0.2952755905511810774, -0.1292274648535930714 ) ) ;
#36916 = CARTESIAN_POINT ( 'NONE',  ( -0.4091458600556402980, -0.2362204724409451284, -0.9973753280839895430 ) ) ;
#36917 = CARTESIAN_POINT ( 'NONE',  ( -0.1070741851644057135, 0.3996062992125985480, -2.526246719160104792 ) ) ;
#36918 = CARTESIAN_POINT ( 'NONE',  ( 0.1377952755905518800, -0.4536011799217367080, 0.2665933059059888421 ) ) ;
#36919 = ORIENTED_EDGE ( 'NONE', *, *, #60874, .F. ) ;
#36920 = CARTESIAN_POINT ( 'NONE',  ( 0.2867679344610366554, -0.2867679344610365999, -0.8825652475403695796 ) ) ;
#36921 = EDGE_LOOP ( 'NONE', ( #62118, #44856, #54729, #12730 ) ) ;
#36922 = CARTESIAN_POINT ( 'NONE',  ( -1.062992125984250968, 0.2952755905511811885, 0.000000000000000000 ) ) ;
#36923 = CARTESIAN_POINT ( 'NONE',  ( -0.2427821522309703550, -0.3162353388693405765, 0.4822834645669290543 ) ) ;
#36924 = CARTESIAN_POINT ( 'NONE',  ( -0.4921259842519677963, 0.1660481256975883668, -0.3530559997133364547 ) ) ;
#36925 = CARTESIAN_POINT ( 'NONE',  ( 0.6955380577427828781, -0.004921259842519870586, -0.3153832671262229437 ) ) ;
#36926 = CARTESIAN_POINT ( 'NONE',  ( 0.2755905511811031494, 0.2952755905511811885, 0.000000000000000000 ) ) ;
#36927 = CARTESIAN_POINT ( 'NONE',  ( -0.3543307086614165824, 0.2952755905511811885, 0.000000000000000000 ) ) ;
#36928 = CARTESIAN_POINT ( 'NONE',  ( -1.266404199475064773, -0.05778040916215560624, -0.4822834645669293319 ) ) ;
#36929 = CARTESIAN_POINT ( 'NONE',  ( -0.7677165354330699465, 0.1660481256975885056, 0.3530559997133364547 ) ) ;
#36930 = CARTESIAN_POINT ( 'NONE',  ( 0.8398950131233602345, 0.2306618581243847221, -0.2411417322834647770 ) ) ;
#36931 = CARTESIAN_POINT ( 'NONE',  ( 0.3917322834645670104, -0.1049643490035303411, -1.048556430446194287 ) ) ;
#36932 = CARTESIAN_POINT ( 'NONE',  ( -0.2427821522309703550, -0.2845877964562159024, 0.3641732283464567677 ) ) ;
#36933 = ORIENTED_EDGE ( 'NONE', *, *, #49705, .F. ) ;
#36934 = CARTESIAN_POINT ( 'NONE',  ( 0.3949938075777409963, 2.418639510665530435E-17, -1.377952755905511584 ) ) ;
#36935 = ORIENTED_EDGE ( 'NONE', *, *, #31097, .F. ) ;
#36936 = CARTESIAN_POINT ( 'NONE',  ( -1.397637795275589623, 0.07958543189024085140, 0.2665933059059887866 ) ) ;
#36937 = CARTESIAN_POINT ( 'NONE',  ( -1.017060367454067249, -0.05778040916215522460, 0.4822834645669289988 ) ) ;
#36938 = CARTESIAN_POINT ( 'NONE',  ( -0.9120734908136475250, -0.6692913385826773087, -0.1292274648535924053 ) ) ;
#36939 = CARTESIAN_POINT ( 'NONE',  ( 0.3460692066303959757, -0.1998031496062991907, 0.05249343832020996609 ) ) ;
#36940 = CARTESIAN_POINT ( 'NONE',  ( -0.6561679790026240244, -0.6046776061558807314, 0.2411417322834647770 ) ) ;
#36941 = CARTESIAN_POINT ( 'NONE',  ( -0.7086614173228339419, -0.1870078740157480879, -0.4822834645669291653 ) ) ;
#36942 = DIRECTION ( 'NONE',  ( -0.8479387356305996271, -2.625811289636364142E-16, -0.5300942374872417151 ) ) ;
#36943 = CARTESIAN_POINT ( 'NONE',  ( 0.5411721830064198935, 8.471767977567108961E-16, -0.4445507791589058955 ) ) ;
#36944 = AXIS2_PLACEMENT_3D ( 'NONE', #57012, #43146, #31346 ) ;
#36945 = CARTESIAN_POINT ( 'NONE',  ( 0.4790026246719168435, -0.2845877964562161244, -0.3641732283464567121 ) ) ;
#36946 = CARTESIAN_POINT ( 'NONE',  ( 1.595398199321655275, 1.013096522517429987, -0.1559797534342494130 ) ) ;
#36947 = CARTESIAN_POINT ( 'NONE',  ( -0.3917322834645671215, 0.1049643490035301469, 0.04002624671916000382 ) ) ;
#36948 = CARTESIAN_POINT ( 'NONE',  ( 0.2362204724409456558, -0.1870078740157480601, -0.3641732283464567677 ) ) ;
#36949 = CARTESIAN_POINT ( 'NONE',  ( -0.3543307086614165824, 0.2952755905511811885, 0.000000000000000000 ) ) ;
#36950 = CARTESIAN_POINT ( 'NONE',  ( 1.581364829396326277, -0.05778040916215522460, 0.4822834645669289988 ) ) ;
#36951 = CARTESIAN_POINT ( 'NONE',  ( 0.1115485564304470323, 0.2952755905511811885, 0.1292274648535926551 ) ) ;
#36952 = ORIENTED_EDGE ( 'NONE', *, *, #23423, .F. ) ;
#36953 = CARTESIAN_POINT ( 'NONE',  ( 0.3460692066303959202, 0.1998031496062993295, -2.178477690288713742 ) ) ;
#36954 = DIRECTION ( 'NONE',  ( -0.000000000000000000, -1.000000000000000000, -0.000000000000000000 ) ) ;
#36955 = ORIENTED_EDGE ( 'NONE', *, *, #67735, .F. ) ;
#36956 = CARTESIAN_POINT ( 'NONE',  ( 4.893765752498283308E-17, -0.3996062992125985480, -1.730314960629921517 ) ) ;
#36957 = CARTESIAN_POINT ( 'NONE',  ( 1.561679790026247350, -0.4281496062992124485, 0.4176697321401328655 ) ) ;
#36958 = CARTESIAN_POINT ( 'NONE',  ( -0.9186351706036736120, 0.1283753931104748280, 0.1820866141732283561 ) ) ;
#36959 = CARTESIAN_POINT ( 'NONE',  ( -0.9776902887139098386, -0.6692913385826771977, 0.1292274648535927661 ) ) ;
#36960 = CARTESIAN_POINT ( 'NONE',  ( -0.4724409448818898682, -8.678599364036362592E-17, -0.3543307086614173040 ) ) ;
#36961 = CARTESIAN_POINT ( 'NONE',  ( -0.5120078740157480990, 0.3045572308828553565, -0.01849200668098333403 ) ) ;
#36962 = CARTESIAN_POINT ( 'NONE',  ( -0.1958661417322834220, -0.3392501089628018884, -0.05774278215223092176 ) ) ;
#36963 = CARTESIAN_POINT ( 'NONE',  ( 1.377952755905512472, 0.2952755905511811885, 0.000000000000000000 ) ) ;
#36964 = CARTESIAN_POINT ( 'NONE',  ( 0.2559055118110243332, -0.5400638737290845981, -0.3530559997133363437 ) ) ;
#36965 = CARTESIAN_POINT ( 'NONE',  ( 0.3871391076115493490, -0.3162353388693405765, 0.4822834645669290543 ) ) ;
#36966 = CARTESIAN_POINT ( 'NONE',  ( -1.227034120734907141, -0.5511811023622048555, -0.09757992244046775898 ) ) ;
#36967 = CARTESIAN_POINT ( 'NONE',  ( -0.2165354330708654795, -0.5400638737290845981, -0.3530559997133363437 ) ) ;
#36968 = CARTESIAN_POINT ( 'NONE',  ( 0.1265901696524990294, -0.4724409448818896462, -2.209317585301837195 ) ) ;
#36969 = CARTESIAN_POINT ( 'NONE',  ( -0.9383202099737524282, -0.05778040916215522460, 0.4822834645669289988 ) ) ;
#36970 = CARTESIAN_POINT ( 'NONE',  ( -0.3949938075777409963, -7.255918531996591613E-17, -2.320866141732283339 ) ) ;
#36971 = CARTESIAN_POINT ( 'NONE',  ( 1.502624671916010790, -0.2845877964562161244, -0.3641732283464567121 ) ) ;
#36972 = CARTESIAN_POINT ( 'NONE',  ( -0.4330708661417315697, 0.1771653543307087630, 0.000000000000000000 ) ) ;
#36973 = CARTESIAN_POINT ( 'NONE',  ( 1.351706036745407680, -0.004921259842519576551, 0.3153832671262227771 ) ) ;
#36974 = CARTESIAN_POINT ( 'NONE',  ( 1.581364829396326277, -0.08942795157527998196, 0.3641732283464567121 ) ) ;
#36975 = CARTESIAN_POINT ( 'NONE',  ( -1.115485564304461219, -0.004921259842519870586, -0.3153832671262229437 ) ) ;
#36976 = CARTESIAN_POINT ( 'NONE',  ( 0.2726377952755905665, 0.1133856558944469489, 0.1574803149606299191 ) ) ;
#36977 = CARTESIAN_POINT ( 'NONE',  ( 0.7152230971128616943, -0.08942795157527998196, 0.3641732283464567121 ) ) ;
#36978 = CARTESIAN_POINT ( 'NONE',  ( -0.5446194225721777693, -0.05778040916215522460, 0.4822834645669289988 ) ) ;
#36979 = CARTESIAN_POINT ( 'NONE',  ( -1.854617417371079657, 1.067551433859871723, 0.06782095098400266198 ) ) ;
#36980 = CARTESIAN_POINT ( 'NONE',  ( -0.2887139107611542133, -0.5023911411419708095, -0.1820866141732282451 ) ) ;
#36981 = CARTESIAN_POINT ( 'NONE',  ( -1.614173228346456268, -0.5511811023622047445, 6.969142054262312111E-17 ) ) ;
#36982 =( BOUNDED_CURVE ( )  B_SPLINE_CURVE ( 2, ( #65442, #25440, #58682, #51106, #6512, #38495, #76803, #13260, #39746, #32182, #71322, #39323, #7344 ),
 .UNSPECIFIED., .F., .F. ) 
 B_SPLINE_CURVE_WITH_KNOTS ( ( 3, 2, 2, 2, 2, 2, 3 ),
 ( 0.4915129128166190742, 0.4924242424242424310, 0.4962121212121212155, 0.5000000000000000000, 0.5037878787878787845, 0.5075757575757575690, 0.5084870871833810924 ),
 .UNSPECIFIED. ) 
 CURVE ( )  GEOMETRIC_REPRESENTATION_ITEM ( )  RATIONAL_B_SPLINE_CURVE ( ( 0.9875488213027530104, 0.9918020599134685922, 1.000000000000000000, 0.9659258262890683122, 1.000000000000000000, 0.9659258262890683122, 1.000000000000000000, 0.9659258262890683122, 1.000000000000000000, 0.9659258262890683122, 1.000000000000000000, 0.9918020599134671489, 0.9875488213027514561 ) ) 
 REPRESENTATION_ITEM ( '' )  );
#36983 = EDGE_CURVE ( 'NONE', #80344, #24500, #64004, .T. ) ;
#36984 = CARTESIAN_POINT ( 'NONE',  ( 0.8989501312335964611, 0.2952755905511811885, 0.1292274648535926551 ) ) ;
#36985 = CARTESIAN_POINT ( 'NONE',  ( 0.6955380577427828781, 0.05413385826771626580, -0.4176697321401330321 ) ) ;
#36986 = CARTESIAN_POINT ( 'NONE',  ( 1.167979002624672580, -0.004921259842519870586, -0.3153832671262229437 ) ) ;
#36987 = CARTESIAN_POINT ( 'NONE',  ( -1.102362204724408601, -0.1870078740157479769, 0.4822834645669291653 ) ) ;
#36988 = CARTESIAN_POINT ( 'NONE',  ( -0.1706036745406816491, -0.004921259842519870586, -0.3153832671262229437 ) ) ;
#36989 = CARTESIAN_POINT ( 'NONE',  ( -1.614173228346457378, 0.9921945702958913094, 0.1372047244094476981 ) ) ;
#36990 = CARTESIAN_POINT ( 'NONE',  ( 0.3937007874015754361, -0.1870078740157480601, -0.3641732283464567677 ) ) ;
#36991 = CARTESIAN_POINT ( 'NONE',  ( -0.3871391076115476282, -0.05778040916215522460, 0.4822834645669289988 ) ) ;
#36992 = CARTESIAN_POINT ( 'NONE',  ( -0.2925321140481932369, 0.2925321140481931259, -0.5688976377952755792 ) ) ;
#36993 = CARTESIAN_POINT ( 'NONE',  ( -0.1049643490035302024, -0.3917322834645671215, -2.204068241469816503 ) ) ;
#36994 = CARTESIAN_POINT ( 'NONE',  ( 0.5511811023622054106, -0.1870078740157480601, -0.3641732283464567677 ) ) ;
#36995 = CARTESIAN_POINT ( 'NONE',  ( -0.2821522309711278487, -0.6692913385826773087, -0.1292274648535924053 ) ) ;
#36996 = AXIS2_PLACEMENT_3D ( 'NONE', #81899, #74339, #75581 ) ;
#36997 = CARTESIAN_POINT ( 'NONE',  ( -0.6692913385826764205, 0.2952755905511811885, 0.000000000000000000 ) ) ;
#36998 = CARTESIAN_POINT ( 'NONE',  ( -0.6430446194225712953, -0.004921259842519870586, -0.3153832671262229437 ) ) ;
#36999 = CARTESIAN_POINT ( 'NONE',  ( -3.935204781620320169, 1.078156475484197685, 0.1229597680020024647 ) ) ;
#37000 = CARTESIAN_POINT ( 'NONE',  ( 0.03937007874015833325, -0.6692913385826771977, 8.415575281601705876E-17 ) ) ;
#37001 = CARTESIAN_POINT ( 'NONE',  ( -1.122047244094487306, -0.4536011799217367080, 0.2665933059059888421 ) ) ;
#37002 = CONICAL_SURFACE ( 'NONE', #73318, 1.220472440944881942, 0.7853981633974621568 ) ;
#37003 = CARTESIAN_POINT ( 'NONE',  ( -1.528871391076114250, -0.6692913385826771977, 0.1292274648535927661 ) ) ;
#37004 = FACE_OUTER_BOUND ( 'NONE', #60560, .T. ) ;
#37005 = ORIENTED_EDGE ( 'NONE', *, *, #44178, .T. ) ;
#37006 = CARTESIAN_POINT ( 'NONE',  ( -1.692913385826770645, 0.1771653543307087630, 0.000000000000000000 ) ) ;
#37007 = CARTESIAN_POINT ( 'NONE',  ( -1.568241469816272105, -0.05778040916215522460, 0.4822834645669289988 ) ) ;
#37008 = CARTESIAN_POINT ( 'NONE',  ( -0.9514435695538050464, -0.3162353388693405765, 0.4822834645669290543 ) ) ;
#37009 = CARTESIAN_POINT ( 'NONE',  ( -1.633858267716534529, 0.1660481256975885056, 0.3530559997133364547 ) ) ;
#37010 = CARTESIAN_POINT ( 'NONE',  ( -0.1958661417322834220, -0.3392501089628018884, -1.567585301837270295 ) ) ;
#37011 = CARTESIAN_POINT ( 'NONE',  ( 0.1504864506494466569, 0.3622863298689281142, -1.220472440944881054 ) ) ;
#37012 = CARTESIAN_POINT ( 'NONE',  ( 0.8595800524934390507, -0.3162353388693405765, 0.4822834645669290543 ) ) ;
#37013 = CARTESIAN_POINT ( 'NONE',  ( 0.3018372703412079971, 0.05413385826771626580, -0.4176697321401330321 ) ) ;
#37014 = PLANE ( 'NONE',  #63790 ) ;
#37015 = CARTESIAN_POINT ( 'NONE',  ( -0.2925321140481932369, 0.2925321140481930704, -2.458661417322834719 ) ) ;
#37016 = CARTESIAN_POINT ( 'NONE',  ( 1.299212598425197429, 0.1771653543307087630, 0.000000000000000000 ) ) ;
#37017 = CARTESIAN_POINT ( 'NONE',  ( 0.2925321140481932369, -0.2925321140481932369, -1.043307086614173151 ) ) ;
#37018 = ORIENTED_EDGE ( 'NONE', *, *, #37700, .F. ) ;
#37019 = CARTESIAN_POINT ( 'NONE',  ( -0.9055118110236215490, -0.5511811023622047445, 6.969142054262312111E-17 ) ) ;
#37020 = CARTESIAN_POINT ( 'NONE',  ( -0.3917322834645669549, -0.1049643490035306603, -2.715223097112861250 ) ) ;
#37021 = ORIENTED_EDGE ( 'NONE', *, *, #42894, .F. ) ;
#37022 = CARTESIAN_POINT ( 'NONE',  ( 0.2427821522309716595, -0.3162353388693409650, -0.4822834645669289433 ) ) ;
#37023 = CARTESIAN_POINT ( 'NONE',  ( -0.4265091863517051496, 0.2952755905511810774, -0.1292274648535930714 ) ) ;
#37024 = CARTESIAN_POINT ( 'NONE',  ( -1.076115485564303809, -0.6046776061558809534, -0.2411417322834644161 ) ) ;
#37025 = CARTESIAN_POINT ( 'NONE',  ( 0.8661417322834653598, -0.1870078740157479769, 0.4822834645669291653 ) ) ;
#37026 = CARTESIAN_POINT ( 'NONE',  ( 1.594488188976378673, -0.5400638737290845981, -0.3530559997133363437 ) ) ;
#37027 = DIRECTION ( 'NONE',  ( -0.000000000000000000, -1.000000000000000000, -0.000000000000000000 ) ) ;
#37028 = CARTESIAN_POINT ( 'NONE',  ( -0.2034120734908128059, 0.2952755905511811885, 0.1292274648535926551 ) ) ;
#37029 = CARTESIAN_POINT ( 'NONE',  ( -1.089238845144356427, -0.4281496062992127816, -0.4176697321401328100 ) ) ;
#37030 = LINE ( 'NONE', #50469, #43355 ) ;
#37031 = CARTESIAN_POINT ( 'NONE',  ( 0.4744094488189065095, 1.520194873416442549, -2.554262525012259477 ) ) ;
#37032 = CARTESIAN_POINT ( 'NONE',  ( 0.1049643490035303689, 0.3917322834645670104, -2.755249343832020248 ) ) ;
#37033 = CARTESIAN_POINT ( 'NONE',  ( 0.6692913385826778638, -0.5511811023622047445, 6.969142054262312111E-17 ) ) ;
#37034 = ORIENTED_EDGE ( 'NONE', *, *, #82019, .T. ) ;
#37035 = CARTESIAN_POINT ( 'NONE',  ( -0.2891555358219911054, 0.2891555358219909388, -0.3346456692913387099 ) ) ;
#37036 = CARTESIAN_POINT ( 'NONE',  ( -0.6364829396325453192, -0.05778040916215560624, -0.4822834645669293319 ) ) ;
#37037 = VERTEX_POINT ( 'NONE', #64602 ) ;
#37038 = CARTESIAN_POINT ( 'NONE',  ( 0.1246719160104994284, -0.5511811023622046335, 0.09757992244046803654 ) ) ;
#37039 = CARTESIAN_POINT ( 'NONE',  ( 0.3458507752293908943, 0.3458507752293908943, -0.1377952755905511861 ) ) ;
#37040 = CARTESIAN_POINT ( 'NONE',  ( 0.7020997375328090762, -0.05778040916215560624, -0.4822834645669293319 ) ) ;
#37041 = CARTESIAN_POINT ( 'NONE',  ( 0.4527559055118117182, -0.5400638737290844871, 0.3530559997133364547 ) ) ;
#37042 = CARTESIAN_POINT ( 'NONE',  ( -0.4527559055118102749, 0.1660481256975885056, 0.3530559997133364547 ) ) ;
#37043 = CARTESIAN_POINT ( 'NONE',  ( -0.1958661417322833942, -0.3392501089628018884, -1.322197793472127625 ) ) ;
#37044 = CARTESIAN_POINT ( 'NONE',  ( -1.384514435695537005, -0.6692913385826773087, -0.1292274648535924053 ) ) ;
#37045 = CARTESIAN_POINT ( 'NONE',  ( 0.3392501089628018884, -0.1958661417322834220, -2.551837270341207109 ) ) ;
#37046 = CARTESIAN_POINT ( 'NONE',  ( 1.463254593175853824, 0.1771653543307087075, -0.09757992244046823083 ) ) ;
#37047 = CARTESIAN_POINT ( 'NONE',  ( -1.220472440944881054, -0.6692913385826771977, 8.415575281601705876E-17 ) ) ;
#37048 = CARTESIAN_POINT ( 'NONE',  ( 0.6889763779527566800, -0.5400638737290844871, 0.3530559997133364547 ) ) ;
#37049 = CARTESIAN_POINT ( 'NONE',  ( 1.030183727034121421, -0.05778040916215522460, 0.4822834645669289988 ) ) ;
#37050 = CARTESIAN_POINT ( 'NONE',  ( 0.1998031496062992740, 0.3460692066303959757, -0.9317585301837270073 ) ) ;
#37051 = CARTESIAN_POINT ( 'NONE',  ( -1.154855643044618851, -0.6046776061558809534, -0.2411417322834644161 ) ) ;
#37052 = CARTESIAN_POINT ( 'NONE',  ( -0.3460692066303957537, -0.1998031496062994405, -0.4442257217847768724 ) ) ;
#37053 = CARTESIAN_POINT ( 'NONE',  ( 0.3674540682414705883, 0.2306618581243847221, -0.2411417322834647770 ) ) ;
#37054 = CARTESIAN_POINT ( 'NONE',  ( -0.3460692066303958092, -0.1998031496062994683, -2.257217847769029007 ) ) ;
#37055 = CARTESIAN_POINT ( 'NONE',  ( -0.2867679344610364334, -0.2867679344610367109, -1.718503937007874072 ) ) ;
#37056 = CARTESIAN_POINT ( 'NONE',  ( -1.646981627296586703, -0.08942795157527998196, 0.3641732283464567121 ) ) ;
#37057 = CARTESIAN_POINT ( 'NONE',  ( 0.7611548556430454138, 0.1283753931104746893, -0.1820866141732285504 ) ) ;
#37058 = CARTESIAN_POINT ( 'NONE',  ( 1.089238845144357537, -0.4281496062992124485, 0.4176697321401328655 ) ) ;
#37059 = CARTESIAN_POINT ( 'NONE',  ( -0.4091458600556402980, -0.2362204724409451284, -1.231627296587926468 ) ) ;
#37060 = CARTESIAN_POINT ( 'NONE',  ( 0.9514435695538062676, -0.2845877964562161244, -0.3641732283464567121 ) ) ;
#37061 = CARTESIAN_POINT ( 'NONE',  ( 0.2493438320209980519, -0.4281496062992127816, -0.4176697321401328100 ) ) ;
#37062 = CARTESIAN_POINT ( 'NONE',  ( 0.1974969037888706092, -0.3420746716998660508, -0.9560367454068241511 ) ) ;
#37063 = CARTESIAN_POINT ( 'NONE',  ( -0.8661417322834640276, -0.1870078740157480879, -0.4822834645669291653 ) ) ;
#37064 = CARTESIAN_POINT ( 'NONE',  ( -1.614173228346457378, 2.157411728916712068, -0.1372047244094477536 ) ) ;
#37065 = CARTESIAN_POINT ( 'NONE',  ( 1.030183727034121421, -0.2845877964562161244, -0.3641732283464567121 ) ) ;
#37066 = CARTESIAN_POINT ( 'NONE',  ( 0.2230971128608929543, 0.05413385826771626580, -0.4176697321401330321 ) ) ;
#37067 = CARTESIAN_POINT ( 'NONE',  ( -1.113948071074810420, 0.02791078216816347476, -0.4328096321851898631 ) ) ;
#37068 = CARTESIAN_POINT ( 'NONE',  ( -0.1049868766404193215, 0.2306618581243847221, -0.2411417322834647770 ) ) ;
#37069 = CARTESIAN_POINT ( 'NONE',  ( -0.07874015748031421014, -0.1870078740157479769, 0.3641732283464567677 ) ) ;
#37070 = CARTESIAN_POINT ( 'NONE',  ( -2.585342365690450617, 1.422987107291903364, -0.4606739315415587233 ) ) ;
#37071 = CARTESIAN_POINT ( 'NONE',  ( -0.3805774278215216522, -0.4281496062992127816, -0.4176697321401328100 ) ) ;
#37072 = CARTESIAN_POINT ( 'NONE',  ( 0.6299212598425204535, -0.1870078740157479769, 0.3641732283464567677 ) ) ;
#37073 = CARTESIAN_POINT ( 'NONE',  ( 1.220472440944881942, 0.4405861044731111953, -0.5309055118110238558 ) ) ;
#37074 = CARTESIAN_POINT ( 'NONE',  ( -0.2925321140481932369, 0.2925321140481931259, -1.828740157480315265 ) ) ;
#37075 = CARTESIAN_POINT ( 'NONE',  ( 0.4461942257217856311, 0.2306618581243847221, -0.2411417322834647770 ) ) ;
#37076 = ADVANCED_FACE ( 'NONE', ( #6525 ), #1060, .T. ) ;
#37077 = CARTESIAN_POINT ( 'NONE',  ( 1.227034120734908917, 0.1771653543307087075, -0.09757992244046823083 ) ) ;
#37078 = FACE_OUTER_BOUND ( 'NONE', #70170, .T. ) ;
#37079 = CARTESIAN_POINT ( 'NONE',  ( -0.4527559055118102749, 0.07958543189024085140, 0.2665933059059887866 ) ) ;
#37080 = CARTESIAN_POINT ( 'NONE',  ( -0.9251968503937002541, 0.07958543189024085140, 0.2665933059059887866 ) ) ;
#37081 = B_SPLINE_CURVE_WITH_KNOTS ( 'NONE', 3,
 ( #1149, #64687, #20914, #77745, #71006, #51615, #26800 ),
 .UNSPECIFIED., .F., .F.,
 ( 4, 3, 4 ),
 ( 1.734723475976807094E-18, 0.001246232571205225159, 0.002492492258783241162 ),
 .UNSPECIFIED. ) ;
#37082 = CARTESIAN_POINT ( 'NONE',  ( -0.2690288713910754526, -0.6692913385826771977, 0.1292274648535927661 ) ) ;
#37083 = CARTESIAN_POINT ( 'NONE',  ( 0.4265091863517067039, -0.6692913385826773087, -0.1292274648535924053 ) ) ;
#37084 = CARTESIAN_POINT ( 'NONE',  ( 0.9908136482939640111, -0.5511811023622046335, 0.09757992244046803654 ) ) ;
#37085 = CARTESIAN_POINT ( 'NONE',  ( -1.673228346456691717, 0.07958543189024071263, -0.2665933059059888421 ) ) ;
#37086 = CARTESIAN_POINT ( 'NONE',  ( 1.607611548556431069, 0.1771653543307087630, 0.09757992244046791164 ) ) ;
#37087 = CARTESIAN_POINT ( 'NONE',  ( 0.7217847769028878924, 0.05413385826771666132, 0.4176697321401328100 ) ) ;
#37088 = CARTESIAN_POINT ( 'NONE',  ( 1.403614904275686858E-14, 1.537401574803149984, -3.937007874015761910 ) ) ;
#37089 = CARTESIAN_POINT ( 'NONE',  ( 0.1968503937007881344, 0.2952755905511811885, 0.000000000000000000 ) ) ;
#37090 = CARTESIAN_POINT ( 'NONE',  ( -0.3917322834645671215, 0.1049643490035301469, -0.9048556430446195176 ) ) ;
#37091 = CARTESIAN_POINT ( 'NONE',  ( 1.010498687664042716, -0.4281496062992124485, 0.4176697321401328655 ) ) ;
#37092 = AXIS2_PLACEMENT_3D ( 'NONE', #43894, #75092, #69591 ) ;
#37093 = CARTESIAN_POINT ( 'NONE',  ( 0.6167979002624679463, 0.05413385826771626580, -0.4176697321401330321 ) ) ;
#37094 = CARTESIAN_POINT ( 'NONE',  ( -0.01548461523783284562, 1.062992125984253411, -3.937007874015749476 ) ) ;
#37095 = CARTESIAN_POINT ( 'NONE',  ( 0.5249343832021005074, -0.5023911411419708095, 0.1820866141732285504 ) ) ;
#37096 = CARTESIAN_POINT ( 'NONE',  ( 1.082677165354331228, 0.1660481256975883668, -0.3530559997133364547 ) ) ;
#37097 = CARTESIAN_POINT ( 'NONE',  ( 0.1706036745406830368, -0.004921259842519576551, 0.3153832671262227771 ) ) ;
#37098 = CARTESIAN_POINT ( 'NONE',  ( -0.2493438320209966919, -0.4281496062992124485, 0.4176697321401328655 ) ) ;
#37099 = CARTESIAN_POINT ( 'NONE',  ( 0.2690288713910767848, -0.6692913385826773087, -0.1292274648535924053 ) ) ;
#37100 = CARTESIAN_POINT ( 'NONE',  ( -0.8070866141732276899, 0.1660481256975883668, -0.3530559997133364547 ) ) ;
#37101 = CARTESIAN_POINT ( 'NONE',  ( -0.4790026246719154557, -0.2845877964562159024, 0.3641732283464567677 ) ) ;
#37102 = CARTESIAN_POINT ( 'NONE',  ( 0.2230971128608929543, 0.05413385826771626580, -0.4176697321401330321 ) ) ;
#37103 = CARTESIAN_POINT ( 'NONE',  ( 0.9711286089238851948, -0.5023911411419708095, -0.1820866141732282451 ) ) ;
#37104 = CARTESIAN_POINT ( 'NONE',  ( -0.2362204724409440182, -0.1870078740157479769, 0.4822834645669291653 ) ) ;
#37105 =( BOUNDED_CURVE ( )  B_SPLINE_CURVE ( 2, ( #80188, #27146, #27982, #79769, #53642, #79350, #52810, #21669, #3148, #15370, #8220, #15793, #67541 ),
 .UNSPECIFIED., .F., .F. ) 
 B_SPLINE_CURVE_WITH_KNOTS ( ( 3, 2, 2, 2, 2, 2, 3 ),
 ( 0.1125000000000000028, 0.1166666666666666685, 0.1208333333333333343, 0.1250000000000000000, 0.1291666666666666796, 0.1333333333333333315, 0.1375000000000000111 ),
 .UNSPECIFIED. ) 
 CURVE ( )  GEOMETRIC_REPRESENTATION_ITEM ( )  RATIONAL_B_SPLINE_CURVE ( ( 1.000000000000000000, 0.9659258262890683122, 1.000000000000000000, 0.9659258262890683122, 1.000000000000000000, 0.9659258262890683122, 1.000000000000000000, 0.9659258262890683122, 1.000000000000000000, 0.9659258262890683122, 1.000000000000000000, 0.9659258262890683122, 1.000000000000000000 ) ) 
 REPRESENTATION_ITEM ( '' )  );
#37106 = CARTESIAN_POINT ( 'NONE',  ( 1.115134929062665980, 0.004960608223778823628, 0.3437734562760190182 ) ) ;
#37108 = CARTESIAN_POINT ( 'NONE',  ( -0.03443470937339728616, 1.062992125984252079, -1.537015892239756099 ) ) ;
#37107 = CARTESIAN_POINT ( 'NONE',  ( 0.000000000000000000, 0.000000000000000000, 0.000000000000000000 ) ) ;
#37109 = CARTESIAN_POINT ( 'NONE',  ( 1.548556430446194954, 0.2306618581243847221, -0.2411417322834647770 ) ) ;
#37110 = CARTESIAN_POINT ( 'NONE',  ( -0.3598931997249494308, -0.1601112597069882237, -1.931802261947322519 ) ) ;
#37112 = VECTOR ( 'NONE', #20406, 39.37007874015748143 ) ;
#37111 = CARTESIAN_POINT ( 'NONE',  ( -1.108923884514435132, -0.05778040916215560624, -0.4822834645669293319 ) ) ;
#37113 = CARTESIAN_POINT ( 'NONE',  ( -0.8333333333333323711, -0.6692913385826773087, -0.1292274648535924053 ) ) ;
#37114 = CARTESIAN_POINT ( 'NONE',  ( 0.4091458600556404646, -0.2362204724409448231, -0.4199475065616797842 ) ) ;
#37115 = CARTESIAN_POINT ( 'NONE',  ( 0.3949938075777411073, -0.1058382717557499464, -2.631233595800525293 ) ) ;
#37116 = ORIENTED_EDGE ( 'NONE', *, *, #25485, .F. ) ;
#37117 = CARTESIAN_POINT ( 'NONE',  ( 0.2559055118110243332, 0.07958543189024085140, 0.2665933059059887866 ) ) ;
#37118 = CARTESIAN_POINT ( 'NONE',  ( 0.1049643490035304938, -0.3917322834645669549, -1.179790026246718915 ) ) ;
#37119 = CARTESIAN_POINT ( 'NONE',  ( 0.7086614173228352742, -0.1870078740157480879, -0.4822834645669291653 ) ) ;
#37120 = CARTESIAN_POINT ( 'NONE',  ( -0.1265901696524993347, 0.4724409448818895907, -2.526246719160104792 ) ) ;
#37121 = DIRECTION ( 'NONE',  ( 1.000000000000000000, -0.000000000000000000, -0.000000000000000000 ) ) ;
#37122 = CARTESIAN_POINT ( 'NONE',  ( -1.712598425196849572, 0.07958543189024085140, 0.2665933059059887866 ) ) ;
#37123 = CARTESIAN_POINT ( 'NONE',  ( 1.148293963254593875, -0.6692913385826771977, 0.1292274648535927661 ) ) ;
#37124 = CARTESIAN_POINT ( 'NONE',  ( 1.476377952755906220, 0.07958543189024071263, -0.2665933059059888421 ) ) ;
#37125 = CARTESIAN_POINT ( 'NONE',  ( 0.006561679790026889343, -0.3162353388693409650, -0.4822834645669289433 ) ) ;
#37126 = CARTESIAN_POINT ( 'NONE',  ( 0.2867679344610365999, -0.2867679344610365999, -0.8083796343493945269 ) ) ;
#37127 = CARTESIAN_POINT ( 'NONE',  ( -0.4790026246719152336, -0.05778040916215560624, -0.4822834645669293319 ) ) ;
#37128 = CARTESIAN_POINT ( 'NONE',  ( -1.528871391076114250, 0.1771653543307087075, -0.09757992244046823083 ) ) ;
#37129 = CARTESIAN_POINT ( 'NONE',  ( 0.5905511811023629321, -0.6692913385826771977, 8.415575281601705876E-17 ) ) ;
#37130 = CARTESIAN_POINT ( 'NONE',  ( -0.3674540682414692561, -0.6046776061558809534, -0.2411417322834644161 ) ) ;
#37131 = CARTESIAN_POINT ( 'NONE',  ( 1.607611548556431069, -0.6692913385826773087, -0.1292274648535924053 ) ) ;
#37132 = CARTESIAN_POINT ( 'NONE',  ( -0.1341302950245069070, 1.082049466318360631, -1.868010872266428590 ) ) ;
#37133 = VERTEX_POINT ( 'NONE', #71752 ) ;
#37134 = CARTESIAN_POINT ( 'NONE',  ( -0.1049643490035302301, -0.3917322834645671770, -1.958680733104674276 ) ) ;
#37135 = CARTESIAN_POINT ( 'NONE',  ( 0.5708661417322842269, 0.1660481256975885056, 0.3530559997133364547 ) ) ;
#37136 = CARTESIAN_POINT ( 'NONE',  ( -0.2755905511811018171, 0.2952755905511811885, 0.000000000000000000 ) ) ;
#37137 = CARTESIAN_POINT ( 'NONE',  ( -1.528871391076114250, -0.6692913385826771977, 0.1292274648535927661 ) ) ;
#37138 = CARTESIAN_POINT ( 'NONE',  ( 0.8727034120734912248, -0.3162353388693409650, -0.4822834645669289433 ) ) ;
#37139 = CARTESIAN_POINT ( 'NONE',  ( 0.6627296587926517768, -0.6692913385826773087, -0.1292274648535924053 ) ) ;
#37140 = CARTESIAN_POINT ( 'NONE',  ( -0.1049643490035307020, 0.3917322834645669549, -1.193569553805774452 ) ) ;
#37141 = CARTESIAN_POINT ( 'NONE',  ( -0.6496062992125976043, -0.5400638737290844871, 0.3530559997133364547 ) ) ;
#37142 = CARTESIAN_POINT ( 'NONE',  ( 0.04593175853018440641, -0.6692913385826771977, 0.1292274648535927661 ) ) ;
#37143 = CARTESIAN_POINT ( 'NONE',  ( -0.5708661417322825615, -0.5400638737290844871, 0.3530559997133364547 ) ) ;
#37144 = CARTESIAN_POINT ( 'NONE',  ( 0.2755905511811031494, 0.1771653543307087630, 0.000000000000000000 ) ) ;
#37145 = CARTESIAN_POINT ( 'NONE',  ( -1.627296587926508442, -0.6046776061558809534, -0.2411417322834644161 ) ) ;
#37146 = CARTESIAN_POINT ( 'NONE',  ( -0.2445717520902165876, -0.1654678116698105328, 5.638396876410332048 ) ) ;
#37147 = CARTESIAN_POINT ( 'NONE',  ( -0.2821522309711278487, 0.2952755905511811885, 0.1292274648535926551 ) ) ;
#37148 = CARTESIAN_POINT ( 'NONE',  ( 0.3438254193631122280, -0.3704879858182168473, -0.01311675794578956791 ) ) ;
#37149 = CARTESIAN_POINT ( 'NONE',  ( 1.358267716535433323, -0.5400638737290845981, -0.3530559997133363437 ) ) ;
#37150 = CARTESIAN_POINT ( 'NONE',  ( 0.1958661417322836440, -0.3392501089628017219, -2.918635170603674389 ) ) ;
#37151 = ORIENTED_EDGE ( 'NONE', *, *, #45942, .F. ) ;
#37152 = ORIENTED_EDGE ( 'NONE', *, *, #31362, .T. ) ;
#37153 = AXIS2_PLACEMENT_3D ( 'NONE', #81920, #10794, #68045 ) ;
#37154 = CARTESIAN_POINT ( 'NONE',  ( 0.8464566929133866546, -0.5400638737290844871, 0.3530559997133364547 ) ) ;
#37155 = CARTESIAN_POINT ( 'NONE',  ( 0.2624671916010504757, -0.5023911411419708095, -0.1820866141732282451 ) ) ;
#37156 = AXIS2_PLACEMENT_3D ( 'NONE', #25081, #18385, #13729 ) ;
#37157 = VECTOR ( 'NONE', #55278, 39.37007874015748143 ) ;
#37159 = DIRECTION ( 'NONE',  ( -0.000000000000000000, 0.000000000000000000, -1.000000000000000000 ) ) ;
#37158 = CARTESIAN_POINT ( 'NONE',  ( 0.5314960629921068325, 2.742788234388598756, 1.827151616986595339 ) ) ;
#37160 = CARTESIAN_POINT ( 'NONE',  ( -0.3917322834645670104, -7.196005306013484475E-17, -1.068897637795275690 ) ) ;
#37161 = CARTESIAN_POINT ( 'NONE',  ( -1.157146581871515012E-16, 0.4724409448818898682, 0.08070866141732283006 ) ) ;
#37162 = SURFACE_STYLE_FILL_AREA ( #23703 ) ;
#37163 = CARTESIAN_POINT ( 'NONE',  ( 0.1998031496062994128, -0.3460692066303957537, -2.845800524934383624 ) ) ;
#37164 = CARTESIAN_POINT ( 'NONE',  ( 0.2952755905511816326, -0.5400638737290844871, 0.3530559997133364547 ) ) ;
#37165 = CARTESIAN_POINT ( 'NONE',  ( -1.345144356955379816, -0.3162353388693405765, 0.4822834645669290543 ) ) ;
#37166 = CARTESIAN_POINT ( 'NONE',  ( -0.9514435695538050464, -0.3162353388693405765, 0.4822834645669290543 ) ) ;
#37167 = CARTESIAN_POINT ( 'NONE',  ( 0.2821522309711292364, -0.6692913385826771977, 0.1292274648535927661 ) ) ;
#37168 = CARTESIAN_POINT ( 'NONE',  ( 1.049868766404200127, -0.6046776061558809534, -0.2411417322834644161 ) ) ;
#37169 = CARTESIAN_POINT ( 'NONE',  ( 1.482939632545932307, -0.3690944881889763329, 0.3153832671262228327 ) ) ;
#37170 = CARTESIAN_POINT ( 'NONE',  ( 1.318897637795276356, -0.4536011799217367080, 0.2665933059059888421 ) ) ;
#37171 = CARTESIAN_POINT ( 'NONE',  ( -1.030183727034119867, -0.3162353388693405765, 0.4822834645669290543 ) ) ;
#37172 = CARTESIAN_POINT ( 'NONE',  ( -0.1070741851644051862, -0.3996062992125986590, -0.4639107611548556331 ) ) ;
#37173 = CARTESIAN_POINT ( 'NONE',  ( 1.594488188976378673, -0.5400638737290845981, -0.3530559997133363437 ) ) ;
#37174 = CARTESIAN_POINT ( 'NONE',  ( -0.1958661417322834220, -0.3392501089628018884, -0.3727034120734908362 ) ) ;
#37175 = CARTESIAN_POINT ( 'NONE',  ( -0.4133858267716528645, -0.5400638737290844871, 0.3530559997133364547 ) ) ;
#37176 = AXIS2_PLACEMENT_3D ( 'NONE', #71528, #52979, #13875 ) ;
#37178 = PLANE ( 'NONE',  #43861 ) ;
#37177 = CARTESIAN_POINT ( 'NONE',  ( 1.069553805774278832, 0.2952755905511810774, -0.1292274648535930714 ) ) ;
#37179 = CARTESIAN_POINT ( 'NONE',  ( -1.430446194225721390, -0.3690944881889763329, 0.3153832671262228327 ) ) ;
#37180 = CARTESIAN_POINT ( 'NONE',  ( 0.3149606299212606708, -0.1870078740157480879, -0.4822834645669291653 ) ) ;
#37181 = CARTESIAN_POINT ( 'NONE',  ( 1.030183727034121421, -0.2845877964562161244, -0.3641732283464567121 ) ) ;
#37182 = CARTESIAN_POINT ( 'NONE',  ( -0.5314960629921124946, 2.712196231959916215, -3.892860353355075631 ) ) ;
#37183 = CARTESIAN_POINT ( 'NONE',  ( 0.7414698162729663755, 0.2952755905511811885, 0.1292274648535926551 ) ) ;
#37184 = DIRECTION ( 'NONE',  ( 0.000000000000000000, 0.000000000000000000, 1.000000000000000000 ) ) ;
#37185 = CARTESIAN_POINT ( 'NONE',  ( -0.6299212598425188991, -0.1870078740157479769, 0.3641732283464567677 ) ) ;
#37186 = CARTESIAN_POINT ( 'NONE',  ( -0.5249343832020990641, -0.6046776061558809534, -0.2411417322834644161 ) ) ;
#37187 = CARTESIAN_POINT ( 'NONE',  ( -1.568241469816272105, -0.2845877964562161244, -0.3641732283464567121 ) ) ;
#37188 = CARTESIAN_POINT ( 'NONE',  ( -0.8530183727034112984, -0.4281496062992127816, -0.4176697321401328100 ) ) ;
#37189 = CARTESIAN_POINT ( 'NONE',  ( 1.456692913385827515, -0.6692913385826771977, 8.415575281601705876E-17 ) ) ;
#37190 = CARTESIAN_POINT ( 'NONE',  ( -0.2867679344610367109, 0.2867679344610365444, -0.9613054050206844003 ) ) ;
#37191 = CARTESIAN_POINT ( 'NONE',  ( -1.036745406824146176, -0.3690944881889763329, 0.3153832671262228327 ) ) ;
#37192 = CARTESIAN_POINT ( 'NONE',  ( 1.119419862066250548, 1.069231759244661628, -0.07826300840915889623 ) ) ;
#37193 = CARTESIAN_POINT ( 'NONE',  ( 1.489501312335958172, -0.05778040916215560624, -0.4822834645669293319 ) ) ;
#37194 = CARTESIAN_POINT ( 'NONE',  ( 0.3458507752293908943, 0.3458507752293908943, -1.946850393700787274 ) ) ;
#37195 = CARTESIAN_POINT ( 'NONE',  ( -1.673228346456691717, 0.1660481256975883668, -0.3530559997133364547 ) ) ;
#37196 = CARTESIAN_POINT ( 'NONE',  ( -1.528871391076114250, -0.5511811023622046335, 0.09757992244046803654 ) ) ;
#37197 = CARTESIAN_POINT ( 'NONE',  ( -0.8661417322834640276, -0.1870078740157480601, -0.3641732283464567677 ) ) ;
#37198 = CARTESIAN_POINT ( 'NONE',  ( 0.9285414500055709786, 2.165354330708661568, -0.6299212598425196763 ) ) ;
#37199 = CARTESIAN_POINT ( 'NONE',  ( -0.2362204724409440182, -0.1870078740157479769, 0.4822834645669291653 ) ) ;
#37200 = CARTESIAN_POINT ( 'NONE',  ( 0.1902887139107617975, -0.5511811023622048555, -0.09757992244046775898 ) ) ;
#37201 = CARTESIAN_POINT ( 'NONE',  ( -1.154855643044618851, -0.5023911411419708095, -0.1820866141732282451 ) ) ;
#37202 = CARTESIAN_POINT ( 'NONE',  ( 1.332020997375328974, -0.08942795157528024563, -0.3641732283464568787 ) ) ;
#37203 = CARTESIAN_POINT ( 'NONE',  ( 0.8333333333333340365, -0.6692913385826771977, 0.1292274648535927661 ) ) ;
#37204 = CARTESIAN_POINT ( 'NONE',  ( 1.561679790026247350, -0.4281496062992124485, 0.4176697321401328655 ) ) ;
#37205 = CARTESIAN_POINT ( 'NONE',  ( 0.6496062992125991586, -0.4536011799217368745, -0.2665933059059886201 ) ) ;
#37206 = CARTESIAN_POINT ( 'NONE',  ( 0.6627296587926517768, -0.6692913385826773087, -0.1292274648535924053 ) ) ;
#37207 = EDGE_CURVE ( 'NONE', #23894, #42095, #46891, .T. ) ;
#37208 = CARTESIAN_POINT ( 'NONE',  ( 0.9711286089238851948, 0.1283753931104748280, 0.1820866141732283561 ) ) ;
#37209 = ORIENTED_EDGE ( 'NONE', *, *, #18554, .F. ) ;
#37211 = CARTESIAN_POINT ( 'NONE',  ( -1.358267716535432434, -0.5400638737290844871, 0.3530559997133364547 ) ) ;
#37210 = CIRCLE ( 'NONE', #47961, 0.5118110236220471121 ) ;
#37212 = EDGE_CURVE ( 'NONE', #39102, #68390, #2211, .T. ) ;
#37213 = CARTESIAN_POINT ( 'NONE',  ( -1.312335958005248715, 0.2306618581243848609, 0.2411417322834645549 ) ) ;
#37214 = CARTESIAN_POINT ( 'NONE',  ( 0.09842519685039434474, -0.5400638737290845981, -0.3530559997133363437 ) ) ;
#37215 = CARTESIAN_POINT ( 'NONE',  ( 0.3996062992125986035, 2.446882876249141962E-17, -0.1181102362204724671 ) ) ;
#37216 = CARTESIAN_POINT ( 'NONE',  ( 0.3460692066303958092, 0.1998031496062993018, -2.727690288713910949 ) ) ;
#37217 = CARTESIAN_POINT ( 'NONE',  ( 0.4986876640419954376, 0.2306618581243848609, 0.2411417322834645549 ) ) ;
#37218 = CARTESIAN_POINT ( 'NONE',  ( 1.345144356955381593, -0.2845877964562161244, -0.3641732283464567121 ) ) ;
#37219 = CIRCLE ( 'NONE', #81578, 3.937007874015748143 ) ;
#37220 = CONICAL_SURFACE ( 'NONE', #50659, 1.181102362204724310, 0.7853981633974621568 ) ;
#37221 = CARTESIAN_POINT ( 'NONE',  ( 0.2296587926509192634, -0.3162353388693405765, 0.4822834645669290543 ) ) ;
#37222 = CARTESIAN_POINT ( 'NONE',  ( 0.3346456692913390985, 0.1660481256975885056, 0.3530559997133364547 ) ) ;
#37223 = CARTESIAN_POINT ( 'NONE',  ( 0.2925321140481932369, 0.2925321140481932369, -2.185039370078739829 ) ) ;
#37224 = CARTESIAN_POINT ( 'NONE',  ( 4.837279021331060870E-17, -0.3949938075777409963, -1.496062992125984037 ) ) ;
#37225 = CARTESIAN_POINT ( 'NONE',  ( -0.1998031496062994683, 0.3460692066303958092, -2.847769028871391050 ) ) ;
#37226 = CARTESIAN_POINT ( 'NONE',  ( -0.4091458600556405756, 0.2362204724409446288, -2.545931758530183497 ) ) ;
#37227 = CARTESIAN_POINT ( 'NONE',  ( 0.3917322834645670104, -0.1049643490035303273, -0.5761154855643044748 ) ) ;
#37228 = CARTESIAN_POINT ( 'NONE',  ( -0.5839895013123351797, 0.1771653543307087075, -0.09757992244046823083 ) ) ;
#37229 = CARTESIAN_POINT ( 'NONE',  ( -0.6102362204724400829, 0.1660481256975885056, 0.3530559997133364547 ) ) ;
#37230 = CARTESIAN_POINT ( 'NONE',  ( 0.5446194225721792126, -0.05778040916215560624, -0.4822834645669293319 ) ) ;
#37231 = CARTESIAN_POINT ( 'NONE',  ( 0.1058382717557499880, 0.3949938075777409408, -2.589895013123359124 ) ) ;
#37232 = CARTESIAN_POINT ( 'NONE',  ( 0.7152230971128616943, -0.05778040916215522460, 0.4822834645669289988 ) ) ;
#37233 = EDGE_CURVE ( 'NONE', #79833, #32475, #49226, .T. ) ;
#37234 = CARTESIAN_POINT ( 'NONE',  ( -1.502624671916009680, -0.3162353388693405765, 0.4822834645669290543 ) ) ;
#37235 = CARTESIAN_POINT ( 'NONE',  ( 0.9448818897637802916, -0.1870078740157479769, 0.4822834645669291653 ) ) ;
#37236 = CARTESIAN_POINT ( 'NONE',  ( -0.6192220670824142292, -3.724876541855331158E-15, 0.4118477457932994135 ) ) ;
#37237 = CARTESIAN_POINT ( 'NONE',  ( 0.3460692066303959757, -0.1998031496062991907, -2.309711286089239035 ) ) ;
#37238 = CARTESIAN_POINT ( 'NONE',  ( 1.469816272965879911, -0.6046776061558807314, 0.2411417322834647770 ) ) ;
#37239 = EDGE_CURVE ( 'NONE', #48621, #19643, #36357, .T. ) ;
#37240 = CARTESIAN_POINT ( 'NONE',  ( 1.069553805774278610, -0.6692913385826771977, 0.1292274648535927661 ) ) ;
#37241 = CARTESIAN_POINT ( 'NONE',  ( 0.4265091863517067039, -0.6692913385826773087, -0.1292274648535924053 ) ) ;
#37242 = CARTESIAN_POINT ( 'NONE',  ( 1.082677165354331228, -0.4536011799217367080, 0.2665933059059888421 ) ) ;
#37243 = PRODUCT_DEFINITION ( 'UNKNOWN', '', #40964, #41947 ) ;
#37245 = CARTESIAN_POINT ( 'NONE',  ( -1.397637795275589623, -0.5400638737290845981, -0.3530559997133363437 ) ) ;
#37244 = CARTESIAN_POINT ( 'NONE',  ( -1.496062992125983815, -0.1870078740157479769, 0.3641732283464567677 ) ) ;
#37246 = CARTESIAN_POINT ( 'NONE',  ( 0.3917322834645670104, -0.1049643490035303411, -0.03871391076115493490 ) ) ;
#37247 = DIRECTION ( 'NONE',  ( 0.000000000000000000, 0.000000000000000000, 1.000000000000000000 ) ) ;
#37248 = CARTESIAN_POINT ( 'NONE',  ( 0.7874015748031503170, -0.1870078740157480879, -0.4822834645669291653 ) ) ;
#37249 = DIRECTION ( 'NONE',  ( -3.096699300667737957E-16, 1.000000000000000000, -0.000000000000000000 ) ) ;
#37250 = CARTESIAN_POINT ( 'NONE',  ( -0.6364829396325453192, -0.3162353388693405765, 0.4822834645669290543 ) ) ;
#37251 = CARTESIAN_POINT ( 'NONE',  ( -0.9842519685039365918, -0.6692913385826771977, 8.415575281601705876E-17 ) ) ;
#37252 = CARTESIAN_POINT ( 'NONE',  ( 1.128608923884514947, 0.2306618581243848609, 0.2411417322834645549 ) ) ;
#37253 = CARTESIAN_POINT ( 'NONE',  ( -0.3392501089628017219, -0.1958661417322836718, -0.4520997375328084655 ) ) ;
#37254 = CARTESIAN_POINT ( 'NONE',  ( 0.1049643490035304938, -0.3917322834645669549, -1.494750656167978642 ) ) ;
#37255 = CARTESIAN_POINT ( 'NONE',  ( 0.3392501089628018884, -0.1958661417322834220, -2.774278215223096922 ) ) ;
#37256 = CARTESIAN_POINT ( 'NONE',  ( 1.692913385826772421, 0.2952755905511811885, 0.000000000000000000 ) ) ;
#37257 = ORIENTED_EDGE ( 'NONE', *, *, #14549, .T. ) ;
#37258 = CARTESIAN_POINT ( 'NONE',  ( 4.837279021331060870E-17, -0.3949938075777409963, -2.913385826771653253 ) ) ;
#37259 = ORIENTED_EDGE ( 'NONE', *, *, #54140, .F. ) ;
#37260 = CYLINDRICAL_SURFACE ( 'NONE', #69081, 0.1937007874015747588 ) ;
#37261 = CARTESIAN_POINT ( 'NONE',  ( 1.522309711286089939, -0.5023911411419708095, -0.1820866141732282451 ) ) ;
#37262 = CARTESIAN_POINT ( 'NONE',  ( -0.3996062992125986035, -0.1070741851644056997, -1.463254593175853158 ) ) ;
#37263 = CARTESIAN_POINT ( 'NONE',  ( 1.397637795275591177, 0.07958543189024071263, -0.2665933059059888421 ) ) ;
#37264 = CYLINDRICAL_SURFACE ( 'NONE', #2107, 0.1181102362204724116 ) ;
#37265 = DIRECTION ( 'NONE',  ( -0.000000000000000000, -1.000000000000000000, -0.000000000000000000 ) ) ;
#37266 = CARTESIAN_POINT ( 'NONE',  ( -0.6299212598425059095, 2.165354330708661568, -3.937007874015764131 ) ) ;
#37267 = CARTESIAN_POINT ( 'NONE',  ( -0.3917322834645669549, -0.1049643490035306603, -0.4455380577427821565 ) ) ;
#37268 = CARTESIAN_POINT ( 'NONE',  ( -0.9186351706036736120, -0.5023911411419708095, -0.1820866141732282451 ) ) ;
#37269 = CARTESIAN_POINT ( 'NONE',  ( -1.272965879265091305, -0.3690944881889763329, 0.3153832671262228327 ) ) ;
#37270 = CARTESIAN_POINT ( 'NONE',  ( -1.305774278215222184, 0.2952755905511811885, 0.1292274648535926551 ) ) ;
#37271 = ADVANCED_FACE ( 'NONE', ( #8197 ), #27544, .F. ) ;
#37272 = CARTESIAN_POINT ( 'NONE',  ( 0.1509186351706042484, -0.3162353388693405765, 0.4822834645669290543 ) ) ;
#37273 = CARTESIAN_POINT ( 'NONE',  ( -1.410761154855641575, -0.3162353388693409650, -0.4822834645669289433 ) ) ;
#37274 = EDGE_LOOP ( 'NONE', ( #16283, #50648, #73593, #53350 ) ) ;
#37275 = CARTESIAN_POINT ( 'NONE',  ( 1.515748031496063186, -0.5400638737290845981, -0.3530559997133363437 ) ) ;
#37276 = CARTESIAN_POINT ( 'NONE',  ( 0.3492006680983059663, -0.3045572308828553565, -0.01849200668098333403 ) ) ;
#37277 = CARTESIAN_POINT ( 'NONE',  ( 0.4724409448818896462, 0.1265901696524990294, -2.014435695538057569 ) ) ;
#37278 = CARTESIAN_POINT ( 'NONE',  ( -0.7426113562972000981, 2.362204724409448620, -0.5309055118110235227 ) ) ;
#37279 = CARTESIAN_POINT ( 'NONE',  ( -0.6561679790026240244, 0.1283753931104746893, -0.1820866141732285504 ) ) ;
#37280 = AXIS2_PLACEMENT_3D ( 'NONE', #26518, #70717, #38723 ) ;
#37281 = CARTESIAN_POINT ( 'NONE',  ( -0.9776902887139098386, 0.2952755905511810774, -0.1292274648535930714 ) ) ;
#37282 = CARTESIAN_POINT ( 'NONE',  ( 0.9317585301837276734, 0.05413385826771626580, -0.4176697321401330321 ) ) ;
#37283 = ORIENTED_EDGE ( 'NONE', *, *, #19019, .T. ) ;
#37285 = CARTESIAN_POINT ( 'NONE',  ( 1.603475055217291612, 0.9922665159524516332, -0.04573490813648244807 ) ) ;
#37284 = CARTESIAN_POINT ( 'NONE',  ( 0.7349081364829403995, 0.2306618581243848609, 0.2411417322834645549 ) ) ;
#37286 = CARTESIAN_POINT ( 'NONE',  ( -1.706036745406823485, 0.2306618581243848609, 0.2411417322834645549 ) ) ;
#37287 = CARTESIAN_POINT ( 'NONE',  ( -1.410761154855642463, -0.05778040916215522460, 0.4822834645669289988 ) ) ;
#37288 = CARTESIAN_POINT ( 'NONE',  ( 0.3917322834645668994, -0.1049643490035303134, -0.3490620490475572768 ) ) ;
#37289 = CARTESIAN_POINT ( 'NONE',  ( 0.06561679790026316017, -0.004921259842519870586, -0.3153832671262229437 ) ) ;
#37290 = CARTESIAN_POINT ( 'NONE',  ( 0.3917322834645669549, 0.1049643490035304660, -0.8392388451443569819 ) ) ;
#37291 = CARTESIAN_POINT ( 'NONE',  ( -0.5380577427821514602, -0.004921259842519576551, 0.3153832671262227771 ) ) ;
#37292 = CARTESIAN_POINT ( 'NONE',  ( 0.5708661417322841158, -0.4536011799217368745, -0.2665933059059886201 ) ) ;
#37293 = CARTESIAN_POINT ( 'NONE',  ( 0.6692913385826777528, 0.2952755905511811885, 0.000000000000000000 ) ) ;
#37294 = CARTESIAN_POINT ( 'NONE',  ( -0.7152230971128602510, -0.2845877964562159024, 0.3641732283464567677 ) ) ;
#37295 = CARTESIAN_POINT ( 'NONE',  ( -0.1049643490035302024, -0.3917322834645671215, -2.741469816272964710 ) ) ;
#37296 = CARTESIAN_POINT ( 'NONE',  ( 1.122047244094488860, 0.1660481256975885056, 0.3530559997133364547 ) ) ;
#37297 = ADVANCED_FACE ( 'NONE', ( #33026 ), #32194, .F. ) ;
#37298 = CARTESIAN_POINT ( 'NONE',  ( -0.8136482939632537770, 0.2306618581243847221, -0.2411417322834647770 ) ) ;
#37299 = CARTESIAN_POINT ( 'NONE',  ( 5.785732909357575061E-17, -0.4724409448818898682, -0.6279527559055118058 ) ) ;
#37300 = CARTESIAN_POINT ( 'NONE',  ( 0.1574803149606306130, -0.1870078740157479769, 0.4822834645669291653 ) ) ;
#37301 = CARTESIAN_POINT ( 'NONE',  ( -0.4855643044619415427, 0.05413385826771626580, -0.4176697321401330321 ) ) ;
#37302 = CARTESIAN_POINT ( 'NONE',  ( 1.371391076115485941, 0.1771653543307087630, 0.09757992244046791164 ) ) ;
#37303 = CARTESIAN_POINT ( 'NONE',  ( 0.2165354330708668673, 0.07958543189024071263, -0.2665933059059888421 ) ) ;
#37304 = CARTESIAN_POINT ( 'NONE',  ( -0.3543307086614165824, -0.6692913385826771977, 8.415575281601705876E-17 ) ) ;
#37305 = CARTESIAN_POINT ( 'NONE',  ( -1.253280839895012377, -0.3162353388693409650, -0.4822834645669289433 ) ) ;
#37306 = DIRECTION ( 'NONE',  ( 0.000000000000000000, 0.000000000000000000, -1.000000000000000000 ) ) ;
#37307 = CARTESIAN_POINT ( 'NONE',  ( 1.607611548556431069, -0.5511811023622048555, -0.09757992244046775898 ) ) ;
#37308 = CARTESIAN_POINT ( 'NONE',  ( -0.07217847769028787330, -0.05778040916215522460, 0.4822834645669289988 ) ) ;
#37309 = CARTESIAN_POINT ( 'NONE',  ( -0.9317585301837263412, 0.05413385826771666132, 0.4176697321401328100 ) ) ;
#37310 = ORIENTED_EDGE ( 'NONE', *, *, #18464, .F. ) ;
#37311 = CARTESIAN_POINT ( 'NONE',  ( -0.3996062992125984925, -0.1070741851644056858, -1.854986876640420057 ) ) ;
#37312 = EDGE_CURVE ( 'NONE', #54857, #34118, #218, .T. ) ;
#37313 = CARTESIAN_POINT ( 'NONE',  ( 1.259842519685040019, -0.1870078740157479769, 0.4822834645669291653 ) ) ;
#37314 = CARTESIAN_POINT ( 'NONE',  ( -0.4593175853018366950, -0.004921259842519576551, 0.3153832671262227771 ) ) ;
#37315 = CARTESIAN_POINT ( 'NONE',  ( -0.5183727034120726440, -0.6692913385826773087, -0.1292274648535924053 ) ) ;
#37316 = CARTESIAN_POINT ( 'NONE',  ( 1.279527559055118724, -0.5400638737290845981, -0.3530559997133363437 ) ) ;
#37317 = CARTESIAN_POINT ( 'NONE',  ( 1.043307086614173818, 0.1660481256975885056, 0.3530559997133364547 ) ) ;
#37318 = B_SPLINE_CURVE_WITH_KNOTS ( 'NONE', 3,
 ( #63193, #5533, #82559, #25707, #24878, #50546, #76250 ),
 .UNSPECIFIED., .F., .F.,
 ( 4, 3, 4 ),
 ( 1.561251128379126385E-17, 0.001246230184515585400, 0.002492489877932649398 ),
 .UNSPECIFIED. ) ;
#37319 = CARTESIAN_POINT ( 'NONE',  ( 2.795275590551181466, 1.338582677165354395, -1.617488608965169241E-16 ) ) ;
#37320 = CARTESIAN_POINT ( 'NONE',  ( -1.095800524934382292, -0.08942795157527998196, 0.3641732283464567121 ) ) ;
#37321 = CARTESIAN_POINT ( 'NONE',  ( 0.3460692066303959202, -0.1998031496062991630, -0.6541994750656167090 ) ) ;
#37322 = CARTESIAN_POINT ( 'NONE',  ( -9.787531504996567848E-17, 0.3996062992125986035, -1.102362204724409489 ) ) ;
#37323 = CARTESIAN_POINT ( 'NONE',  ( -0.1058382717557497937, -0.3949938075777411628, -0.07217847769028878924 ) ) ;
#37324 = CARTESIAN_POINT ( 'NONE',  ( 0.3003296953575904649, 1.169860122871911434, 2.776875277198005421 ) ) ;
#37325 = CARTESIAN_POINT ( 'NONE',  ( 1.154855643044620184, -0.5023911411419708095, 0.1820866141732285504 ) ) ;
#37326 = CARTESIAN_POINT ( 'NONE',  ( 0.5774278215223103139, -0.5023911411419708095, -0.1820866141732282451 ) ) ;
#37327 = CARTESIAN_POINT ( 'NONE',  ( 0.5708661417322841158, -0.5400638737290845981, -0.3530559997133363437 ) ) ;
#37328 = CARTESIAN_POINT ( 'NONE',  ( 0.2891555358219910499, 0.2891555358219910499, -1.474409448818897683 ) ) ;
#37329 = CARTESIAN_POINT ( 'NONE',  ( 0.7283464566929143125, 0.07958543189024085140, 0.2665933059059887866 ) ) ;
#37330 = CARTESIAN_POINT ( 'NONE',  ( -0.3018372703412066094, -0.4281496062992127816, -0.4176697321401328100 ) ) ;
#37331 = CARTESIAN_POINT ( 'NONE',  ( -1.056430446194224881, -0.6692913385826771977, 0.1292274648535927661 ) ) ;
#37332 = CARTESIAN_POINT ( 'NONE',  ( 1.062992125984252745, 0.2952755905511811885, 0.000000000000000000 ) ) ;
#37333 = CARTESIAN_POINT ( 'NONE',  ( 0.4724409448818896462, 0.1265901696524990294, -1.384514435695537671 ) ) ;
#37334 = AXIS2_PLACEMENT_3D ( 'NONE', #30364, #21993, #47654 ) ;
#37335 = DIRECTION ( 'NONE',  ( -1.776356839400250465E-15, 0.000000000000000000, -1.000000000000000000 ) ) ;
#37336 = CARTESIAN_POINT ( 'NONE',  ( 0.1246719160104994284, -0.5511811023622046335, 0.09757992244046803654 ) ) ;
#37337 = VERTEX_POINT ( 'NONE', #51952 ) ;
#37338 = ORIENTED_EDGE ( 'NONE', *, *, #61119, .F. ) ;
#37339 = CARTESIAN_POINT ( 'NONE',  ( -0.9908136482939626788, -0.6692913385826773087, -0.1292274648535924053 ) ) ;
#37340 = CARTESIAN_POINT ( 'NONE',  ( -0.6889763779527552368, 0.1660481256975885056, 0.3530559997133364547 ) ) ;
#37341 = CARTESIAN_POINT ( 'NONE',  ( -0.2821522309711278487, -0.6692913385826773087, -0.1292274648535924053 ) ) ;
#37342 = DIMENSIONAL_EXPONENTS ( 1.000000000000000000, 0.000000000000000000, 0.000000000000000000, 0.000000000000000000, 0.000000000000000000, 0.000000000000000000, 0.000000000000000000 ) ;
#37343 = CARTESIAN_POINT ( 'NONE',  ( 0.3608923884514443348, -0.6692913385826771977, 0.1292274648535927661 ) ) ;
#37344 = CARTESIAN_POINT ( 'NONE',  ( -0.3608923884514428360, 0.2952755905511811885, 0.1292274648535926551 ) ) ;
#37345 = CARTESIAN_POINT ( 'NONE',  ( -1.522309711286088607, -0.6046776061558807314, 0.2411417322834647770 ) ) ;
#37346 = CARTESIAN_POINT ( 'NONE',  ( -0.9776902887139098386, -0.6692913385826771977, 0.1292274648535927661 ) ) ;
#37347 = CARTESIAN_POINT ( 'NONE',  ( 0.9448818897637802916, -0.1870078740157479769, 0.4822834645669291653 ) ) ;
#37348 = CARTESIAN_POINT ( 'NONE',  ( 0.3392501089628018329, 0.1958661417322835607, -1.068241469816272771 ) ) ;
#37349 = CARTESIAN_POINT ( 'NONE',  ( -0.4330708661417315697, -0.5511811023622047445, 6.969142054262312111E-17 ) ) ;
#37350 = ORIENTED_EDGE ( 'NONE', *, *, #3392, .F. ) ;
#37351 = CARTESIAN_POINT ( 'NONE',  ( -0.1974969037888703871, -0.3420746716998661063, -1.640419947506561948 ) ) ;
#37352 = VERTEX_POINT ( 'NONE', #19989 ) ;
#37353 = CARTESIAN_POINT ( 'NONE',  ( -1.082677165354329896, 0.07958543189024085140, 0.2665933059059887866 ) ) ;
#37354 = CARTESIAN_POINT ( 'NONE',  ( -0.9842519685039360366, 0.2952755905511811885, 0.000000000000000000 ) ) ;
#37355 = CARTESIAN_POINT ( 'NONE',  ( -0.7283464566929126471, -0.5400638737290844871, 0.3530559997133364547 ) ) ;
#37356 = CARTESIAN_POINT ( 'NONE',  ( -0.1070741851644051862, -0.3996062992125987146, -0.3871391076115485719 ) ) ;
#37357 = CARTESIAN_POINT ( 'NONE',  ( -0.6496062992125976043, -0.5400638737290844871, 0.3530559997133364547 ) ) ;
#37358 = CARTESIAN_POINT ( 'NONE',  ( -0.6627296587926503335, -0.6692913385826771977, 0.1292274648535927661 ) ) ;
#37359 = LINE ( 'NONE', #31031, #14927 ) ;
#37360 = EDGE_CURVE ( 'NONE', #51592, #82476, #71335, .T. ) ;
#37361 = LINE ( 'NONE', #44068, #36178 ) ;
#37362 = CARTESIAN_POINT ( 'NONE',  ( 0.4658792650918641698, -0.08942795157528024563, -0.3641732283464568787 ) ) ;
#37363 = CARTESIAN_POINT ( 'NONE',  ( 1.586052503253845281, 1.023622047244095556, -0.1653254495020587966 ) ) ;
#37364 = CARTESIAN_POINT ( 'NONE',  ( -0.1958661417322834220, -0.3392501089628018884, 0.1646981627296586759 ) ) ;
#37365 = CARTESIAN_POINT ( 'NONE',  ( -0.1312335958005241554, 0.1283753931104748280, 0.1820866141732283561 ) ) ;
#37366 = CARTESIAN_POINT ( 'NONE',  ( -0.3740157480314953431, 0.1660481256975885056, 0.3530559997133364547 ) ) ;
#37367 = ADVANCED_FACE ( 'NONE', ( #15349 ), #67935, .F. ) ;
#37368 = CARTESIAN_POINT ( 'NONE',  ( 1.496062992125984703, -0.1870078740157480879, -0.4822834645669291653 ) ) ;
#37369 = CARTESIAN_POINT ( 'NONE',  ( 0.1049868766404206816, 0.2306618581243848609, 0.2411417322834645549 ) ) ;
#37370 = VERTEX_POINT ( 'NONE', #29209 ) ;
#37371 = CARTESIAN_POINT ( 'NONE',  ( -0.3996062992125986035, -0.1070741851644056997, -2.250656167979002920 ) ) ;
#37372 = CARTESIAN_POINT ( 'NONE',  ( -0.8530183727034112984, 0.009842519685039467087, 0.3409548833797002021 ) ) ;
#37373 = EDGE_LOOP ( 'NONE', ( #42923, #64248 ) ) ;
#37374 = CARTESIAN_POINT ( 'NONE',  ( 0.1070741851644053388, 0.3996062992125986035, -1.487532808398950301 ) ) ;
#37375 = FACE_OUTER_BOUND ( 'NONE', #9706, .T. ) ;
#37376 = CARTESIAN_POINT ( 'NONE',  ( -1.003937007874015297, -0.4536011799217368745, -0.2665933059059886201 ) ) ;
#37377 = CARTESIAN_POINT ( 'NONE',  ( -1.561679790026246017, 0.05413385826771666132, 0.4176697321401328100 ) ) ;
#37378 = CARTESIAN_POINT ( 'NONE',  ( 0.2362204724409449064, 0.4091458600556404646, -0.4593175853018372501 ) ) ;
#37379 = CARTESIAN_POINT ( 'NONE',  ( 1.586052503253845503, 0.7480314960629931287, 0.1653254495020587966 ) ) ;
#37380 = CARTESIAN_POINT ( 'NONE',  ( -0.1049643490035302024, -0.3917322834645671215, -0.06430446194225715451 ) ) ;
#37381 = CARTESIAN_POINT ( 'NONE',  ( 1.259842519685040019, -0.1870078740157480879, -0.4822834645669291653 ) ) ;
#37382 = CARTESIAN_POINT ( 'NONE',  ( 0.4396325459317590445, -0.6692913385826771977, 0.1292274648535927661 ) ) ;
#37383 = CARTESIAN_POINT ( 'NONE',  ( 0.1968503937007881344, -0.6692913385826771977, 8.415575281601705876E-17 ) ) ;
#37384 = CARTESIAN_POINT ( 'NONE',  ( -0.8923884514435688198, -0.5023911411419708095, 0.1820866141732285504 ) ) ;
#37385 = CARTESIAN_POINT ( 'NONE',  ( -0.2296587926509179312, -0.3162353388693409650, -0.4822834645669289433 ) ) ;
#37386 = CARTESIAN_POINT ( 'NONE',  ( 0.2362204724409449064, 0.4091458600556404646, -2.268372703412073310 ) ) ;
#37387 = CARTESIAN_POINT ( 'NONE',  ( -1.030183727034119867, -0.05778040916215560624, -0.4822834645669293319 ) ) ;
#37388 = CARTESIAN_POINT ( 'NONE',  ( 0.3420746716998660508, 0.1974969037888705814, -2.255249343832021136 ) ) ;
#37389 = CARTESIAN_POINT ( 'NONE',  ( 1.213910761154856299, -0.5511811023622048555, -0.09757992244046775898 ) ) ;
#37390 = CARTESIAN_POINT ( 'NONE',  ( -0.3083989501312330295, -0.08942795157527998196, 0.3641732283464567121 ) ) ;
#37391 = CARTESIAN_POINT ( 'NONE',  ( 1.371391076115485941, 0.1771653543307087630, 0.09757992244046791164 ) ) ;
#37392 = CARTESIAN_POINT ( 'NONE',  ( -1.371391076115484831, 0.2952755905511810774, -0.1292274648535930714 ) ) ;
#37393 = CARTESIAN_POINT ( 'NONE',  ( -1.220472440944881054, -0.5511811023622047445, 6.969142054262312111E-17 ) ) ;
#37394 = CARTESIAN_POINT ( 'NONE',  ( 0.3307086614173228023, -0.3051181102362204856, 0.000000000000000000 ) ) ;
#37395 = CARTESIAN_POINT ( 'NONE',  ( 0.3477690288713918276, -0.5511811023622048555, -0.09757992244046775898 ) ) ;
#37396 = CARTESIAN_POINT ( 'NONE',  ( -0.9776902887139098386, 0.2952755905511810774, -0.1292274648535930714 ) ) ;
#37397 = VECTOR ( 'NONE', #33915, 39.37007874015748143 ) ;
#37398 = CARTESIAN_POINT ( 'NONE',  ( -2.165607527688992562, 1.494646310179102544, 0.4725519687354810539 ) ) ;
#37399 = CARTESIAN_POINT ( 'NONE',  ( -0.01968503937007793844, 0.07958543189024071263, -0.2665933059059888421 ) ) ;
#37400 = CARTESIAN_POINT ( 'NONE',  ( -1.522309711286088607, 0.1283753931104746893, -0.1820866141732285504 ) ) ;
#37401 = CARTESIAN_POINT ( 'NONE',  ( 0.6496062992125991586, -0.5400638737290845981, -0.3530559997133363437 ) ) ;
#37402 = LINE ( 'NONE', #44925, #47849 ) ;
#37403 = CARTESIAN_POINT ( 'NONE',  ( 1.332020997375328974, -0.08942795157528024563, -0.3641732283464568787 ) ) ;
#37404 = CARTESIAN_POINT ( 'NONE',  ( -1.095800524934382292, -0.05778040916215522460, 0.4822834645669289988 ) ) ;
#37405 = CARTESIAN_POINT ( 'NONE',  ( -0.3477690288713902178, 0.1771653543307087075, -0.09757992244046823083 ) ) ;
#37406 = CARTESIAN_POINT ( 'NONE',  ( -1.603475055217291612, 0.9922665159524542977, -0.04573490813648263542 ) ) ;
#37407 = CARTESIAN_POINT ( 'NONE',  ( 0.4068241469816279987, -0.3690944881889765550, -0.3153832671262227771 ) ) ;
#37408 = CARTESIAN_POINT ( 'NONE',  ( -1.181102362204723644, -0.1870078740157480879, -0.4822834645669291653 ) ) ;
#37409 = CARTESIAN_POINT ( 'NONE',  ( -0.5971128608923877978, -0.6692913385826773087, -0.1292274648535924053 ) ) ;
#37410 = CARTESIAN_POINT ( 'NONE',  ( 0.1998031496062992463, 0.3460692066303959202, -0.6935695538057742304 ) ) ;
#37411 = CARTESIAN_POINT ( 'NONE',  ( -0.1958661417322836718, 0.3392501089628017219, -2.459973753280839670 ) ) ;
#37412 = CARTESIAN_POINT ( 'NONE',  ( 0.5446194225721792126, -0.08942795157528024563, -0.3641732283464568787 ) ) ;
#37413 = CARTESIAN_POINT ( 'NONE',  ( -0.1968503937007867743, 0.2952755905511811885, 0.000000000000000000 ) ) ;
#37414 = CARTESIAN_POINT ( 'NONE',  ( -0.7874015748031489847, -0.1870078740157480879, -0.4822834645669291653 ) ) ;
#37415 = CARTESIAN_POINT ( 'NONE',  ( -0.9973753280839886548, 0.1283753931104748280, 0.1820866141732283561 ) ) ;
#37416 = CARTESIAN_POINT ( 'NONE',  ( -3.908691076466078496, 1.475530872617185185, 0.4713832733224261329 ) ) ;
#37417 = CARTESIAN_POINT ( 'NONE',  ( -0.1837270341207340729, 0.2306618581243847221, -0.2411417322834647770 ) ) ;
#37418 = CARTESIAN_POINT ( 'NONE',  ( -1.515748031496062076, 0.07958543189024071263, -0.2665933059059888421 ) ) ;
#37419 = CARTESIAN_POINT ( 'NONE',  ( -1.351706036745406347, -0.4281496062992124485, 0.4176697321401328655 ) ) ;
#37420 = CARTESIAN_POINT ( 'NONE',  ( -0.4724409448818904789, -0.1265901696524977804, -0.6758530183727032847 ) ) ;
#37421 = ORIENTED_EDGE ( 'NONE', *, *, #36825, .F. ) ;
#37422 = FACE_BOUND ( 'NONE', #57420, .T. ) ;
#37423 = CARTESIAN_POINT ( 'NONE',  ( -1.443569553805773564, -0.6046776061558807314, 0.2411417322834647770 ) ) ;
#37424 = CARTESIAN_POINT ( 'NONE',  ( -1.036745406824146176, 0.05413385826771626580, -0.4176697321401330321 ) ) ;
#37425 = CARTESIAN_POINT ( 'NONE',  ( 1.515748031496063186, -0.5400638737290845981, -0.3530559997133363437 ) ) ;
#37426 = CARTESIAN_POINT ( 'NONE',  ( -9.594673741351313045E-17, 0.3917322834645670104, -2.131889763779527769 ) ) ;
#37427 = DIRECTION ( 'NONE',  ( -1.000000000000000000, -0.000000000000000000, -0.000000000000000000 ) ) ;
#37428 = CARTESIAN_POINT ( 'NONE',  ( 0.8530183727034128527, -0.4281496062992124485, 0.4176697321401328655 ) ) ;
#37429 = CARTESIAN_POINT ( 'NONE',  ( 0.6102362204724416372, 0.1660481256975883668, -0.3530559997133364547 ) ) ;
#37430 = LINE ( 'NONE', #55944, #27512 ) ;
#37431 = CARTESIAN_POINT ( 'NONE',  ( -9.787531504996566615E-17, 0.3996062992125985480, -2.281496062992125928 ) ) ;
#37432 = CARTESIAN_POINT ( 'NONE',  ( 1.089238845144357537, -0.3690944881889763329, 0.3153832671262228327 ) ) ;
#37433 = CARTESIAN_POINT ( 'NONE',  ( -9.787531504996567848E-17, 0.3996062992125986035, -1.102362204724409489 ) ) ;
#37434 = ORIENTED_EDGE ( 'NONE', *, *, #65412, .F. ) ;
#37435 = CARTESIAN_POINT ( 'NONE',  ( -0.2867679344610365999, 0.2867679344610364889, -2.688976377952755570 ) ) ;
#37436 = ORIENTED_EDGE ( 'NONE', *, *, #55337, .F. ) ;
#37437 = CARTESIAN_POINT ( 'NONE',  ( 0.3937007874015754361, -0.1870078740157480879, -0.4822834645669291653 ) ) ;
#37438 = CARTESIAN_POINT ( 'NONE',  ( -0.7480314960629914633, 0.2952755905511811885, 0.000000000000000000 ) ) ;
#37439 = CARTESIAN_POINT ( 'NONE',  ( -1.410761154855641575, -0.3162353388693409650, -0.4822834645669289433 ) ) ;
#37440 = CARTESIAN_POINT ( 'NONE',  ( 1.010498687664042716, -0.4281496062992124485, 0.4176697321401328655 ) ) ;
#37441 = CARTESIAN_POINT ( 'NONE',  ( 1.601049868766404982, -0.6046776061558809534, -0.2411417322834644161 ) ) ;
#37442 = CARTESIAN_POINT ( 'NONE',  ( 0.4177787735907000366, 0.3937007874015748254, -1.559171609364239375 ) ) ;
#37443 = CARTESIAN_POINT ( 'NONE',  ( -0.2362204724409440182, -0.1870078740157479769, 0.4822834645669291653 ) ) ;
#37444 = CARTESIAN_POINT ( 'NONE',  ( -1.095800524934382292, -0.3162353388693409650, -0.4822834645669289433 ) ) ;
#37445 = CARTESIAN_POINT ( 'NONE',  ( -1.541994750656167090, -0.6692913385826773087, -0.1292274648535924053 ) ) ;
#37446 = CARTESIAN_POINT ( 'NONE',  ( 0.4672625608940805253, 1.453874696264120026, -2.571193713084665600 ) ) ;
#37447 = CARTESIAN_POINT ( 'NONE',  ( 0.1958661417322836440, -0.3392501089628017219, -2.853674540682414662 ) ) ;
#37448 = CARTESIAN_POINT ( 'NONE',  ( 1.049868766404200349, 0.1283753931104748280, 0.1820866141732283561 ) ) ;
#37449 = ORIENTED_EDGE ( 'NONE', *, *, #36169, .F. ) ;
#37450 = CARTESIAN_POINT ( 'NONE',  ( 0.1058382717557499880, 0.3949938075777411073, -0.3083989501312336956 ) ) ;
#37451 = ORIENTED_EDGE ( 'NONE', *, *, #60460, .T. ) ;
#37452 = CARTESIAN_POINT ( 'NONE',  ( -0.1312335958005241554, 0.1283753931104748280, 0.1820866141732283561 ) ) ;
#37453 = CARTESIAN_POINT ( 'NONE',  ( 0.1265901696524989184, 0.4724409448818898127, -0.1509186351706036655 ) ) ;
#37454 = CARTESIAN_POINT ( 'NONE',  ( 0.5774278215223103139, -0.6046776061558809534, -0.2411417322834644161 ) ) ;
#37455 = CARTESIAN_POINT ( 'NONE',  ( 0.2755905511811031494, -0.6692913385826771977, 8.415575281601705876E-17 ) ) ;
#37456 = EDGE_CURVE ( 'NONE', #65086, #19973, #67518, .T. ) ;
#37457 = CARTESIAN_POINT ( 'NONE',  ( -0.7086614173228339419, -0.1870078740157480879, -0.4822834645669291653 ) ) ;
#37458 = CARTESIAN_POINT ( 'NONE',  ( 0.2867679344610366554, 0.2867679344610366554, -1.709336901083676086 ) ) ;
#37459 = CARTESIAN_POINT ( 'NONE',  ( -1.135170603674539924, 0.2952755905511810774, -0.1292274648535930714 ) ) ;
#37460 = CARTESIAN_POINT ( 'NONE',  ( -9.594673741351313045E-17, 0.3917322834645670104, -2.761811023622046779 ) ) ;
#37461 = CARTESIAN_POINT ( 'NONE',  ( 1.286089238845145033, 0.1283753931104748280, 0.1820866141732283561 ) ) ;
#37462 = CARTESIAN_POINT ( 'NONE',  ( -1.430446194225720724, 0.05413385826771626580, -0.4176697321401330321 ) ) ;
#37463 = CARTESIAN_POINT ( 'NONE',  ( 0.9055118110236227702, 0.2952755905511811885, 0.000000000000000000 ) ) ;
#37464 = CARTESIAN_POINT ( 'NONE',  ( 0.9842519685039378130, -0.6692913385826771977, 8.415575281601705876E-17 ) ) ;
#37465 = CARTESIAN_POINT ( 'NONE',  ( 0.1998031496062994405, -0.3460692066303958092, -1.036745406824147064 ) ) ;
#37466 = CARTESIAN_POINT ( 'NONE',  ( -1.299212598425196097, -0.6692913385826771977, 8.415575281601705876E-17 ) ) ;
#37467 = CARTESIAN_POINT ( 'NONE',  ( 0.3996062992125984925, 0.1070741851644054637, -0.2014435695538057958 ) ) ;
#37468 = CARTESIAN_POINT ( 'NONE',  ( 0.006561679790026889343, -0.05778040916215522460, 0.4822834645669289988 ) ) ;
#37469 = CARTESIAN_POINT ( 'NONE',  ( 0.3460692066303959757, -0.1998031496062991907, -2.467191601049868677 ) ) ;
#37470 = CARTESIAN_POINT ( 'NONE',  ( -0.3917322834645671215, 0.1049643490035301469, -1.692257217847769057 ) ) ;
#37471 = CARTESIAN_POINT ( 'NONE',  ( 1.541994750656168645, 0.2952755905511810774, -0.1292274648535930714 ) ) ;
#37472 = CARTESIAN_POINT ( 'NONE',  ( 0.1968503937007881344, -0.5511811023622047445, 6.969142054262312111E-17 ) ) ;
#37473 = CARTESIAN_POINT ( 'NONE',  ( 0.9514435695538062676, -0.05778040916215522460, 0.4822834645669289988 ) ) ;
#37474 = CARTESIAN_POINT ( 'NONE',  ( -1.157146581871515012E-16, 0.4724409448818898682, -1.179133858267716661 ) ) ;
#37475 = CARTESIAN_POINT ( 'NONE',  ( 0.7349081364829403995, 0.1283753931104748280, 0.1820866141732283561 ) ) ;
#37476 =( BOUNDED_CURVE ( )  B_SPLINE_CURVE ( 1, ( #29881, #81253 ),
 .UNSPECIFIED., .F., .F. ) 
 B_SPLINE_CURVE_WITH_KNOTS ( ( 2, 2 ),
 ( 6.938893903907228378E-18, 0.001999999999999994837 ),
 .UNSPECIFIED. ) 
 CURVE ( )  GEOMETRIC_REPRESENTATION_ITEM ( )  RATIONAL_B_SPLINE_CURVE ( ( 0.9875488213027535656, 0.9875488213027535656 ) ) 
 REPRESENTATION_ITEM ( '' )  );
#37477 = CARTESIAN_POINT ( 'NONE',  ( 0.3280839895013130669, 0.05413385826771666132, 0.4176697321401328100 ) ) ;
#37478 = CARTESIAN_POINT ( 'NONE',  ( 0.3420746716998660508, 0.1974969037888705814, -1.152887139107611425 ) ) ;
#37479 = CARTESIAN_POINT ( 'NONE',  ( -0.7677165354330699465, 0.1660481256975885056, 0.3530559997133364547 ) ) ;
#37480 = CARTESIAN_POINT ( 'NONE',  ( -3.886287458032462006, 1.724409448818898127, -0.6299212598425202314 ) ) ;
#37481 = CARTESIAN_POINT ( 'NONE',  ( 0.7611548556430451917, -0.5023911411419708095, 0.1820866141732285504 ) ) ;
#37482 = CARTESIAN_POINT ( 'NONE',  ( 0.000000000000000000, 0.000000000000000000, -2.755905511811024056 ) ) ;
#37483 = CARTESIAN_POINT ( 'NONE',  ( -0.3083989501312330295, -0.05778040916215522460, 0.4822834645669289988 ) ) ;
#37484 = CARTESIAN_POINT ( 'NONE',  ( 0.07874015748031558404, -0.1870078740157479769, 0.3641732283464567677 ) ) ;
#37485 = CARTESIAN_POINT ( 'NONE',  ( -2.759994995438131316, 1.188885443925050245, -0.3231744412229767272 ) ) ;
#37486 = CARTESIAN_POINT ( 'NONE',  ( -0.5118110236220466680, -0.6692913385826771977, 8.415575281601705876E-17 ) ) ;
#37487 = CARTESIAN_POINT ( 'NONE',  ( 0.7152230971128614723, -0.2845877964562161244, -0.3641732283464567121 ) ) ;
#37488 = CARTESIAN_POINT ( 'NONE',  ( -0.3460692066303957537, -0.1998031496062994405, -1.861548556430446366 ) ) ;
#37489 = CARTESIAN_POINT ( 'NONE',  ( 0.4658792650918641698, -0.05778040916215560624, -0.4822834645669293319 ) ) ;
#37490 = CARTESIAN_POINT ( 'NONE',  ( 1.371391076115485941, 0.1771653543307087630, 0.09757992244046791164 ) ) ;
#37491 = DIRECTION ( 'NONE',  ( 0.000000000000000000, 0.000000000000000000, 1.000000000000000000 ) ) ;
#37492 = CARTESIAN_POINT ( 'NONE',  ( -0.5577427821522301654, -0.08942795157528024563, -0.3641732283464568787 ) ) ;
#37493 = CARTESIAN_POINT ( 'NONE',  ( -0.5708661417322828946, 0.07958543189024071263, -0.2665933059059888421 ) ) ;
#37494 = CARTESIAN_POINT ( 'NONE',  ( -0.4265091863517051496, -0.6692913385826771977, 0.1292274648535927661 ) ) ;
#37495 = CARTESIAN_POINT ( 'NONE',  ( 0.1837270341207354329, 0.2306618581243848609, 0.2411417322834645549 ) ) ;
#37496 = CARTESIAN_POINT ( 'NONE',  ( 0.8595800524934390507, -0.2845877964562159024, 0.3641732283464567677 ) ) ;
#37497 = CARTESIAN_POINT ( 'NONE',  ( -1.627296587926508442, -0.5023911411419708095, -0.1820866141732282451 ) ) ;
#37498 = CARTESIAN_POINT ( 'NONE',  ( 1.450131233595801428, 0.1771653543307087630, 0.09757992244046791164 ) ) ;
#37499 = CARTESIAN_POINT ( 'NONE',  ( 0.7349081364829403995, 0.2306618581243848609, 0.2411417322834645549 ) ) ;
#37500 = CARTESIAN_POINT ( 'NONE',  ( 0.3811349131313429006, 1.253490138500162443, -2.019723589772945527 ) ) ;
#37501 = CARTESIAN_POINT ( 'NONE',  ( -0.4002624671916004129, -0.05778040916215560624, -0.4822834645669293319 ) ) ;
#37502 = CARTESIAN_POINT ( 'NONE',  ( -0.3917322834645670104, -7.196005306013484475E-17, -1.068897637795275690 ) ) ;
#37503 = CARTESIAN_POINT ( 'NONE',  ( 0.8464566929133866546, -0.5400638737290844871, 0.3530559997133364547 ) ) ;
#37504 = CARTESIAN_POINT ( 'NONE',  ( 0.5905511811023629321, 0.2952755905511811885, 0.000000000000000000 ) ) ;
#37505 = CARTESIAN_POINT ( 'NONE',  ( 5.818687728935708833E-24, 1.062992125984252745, -3.937007874015748143 ) ) ;
#37506 = CARTESIAN_POINT ( 'NONE',  ( 0.5839895013123367340, 0.1771653543307087630, 0.09757992244046791164 ) ) ;
#37507 = CARTESIAN_POINT ( 'NONE',  ( 1.292650918635171564, -0.6692913385826773087, -0.1292274648535924053 ) ) ;
#37508 = CARTESIAN_POINT ( 'NONE',  ( 0.08530183727034192087, -0.2845877964562161244, -0.3641732283464567121 ) ) ;
#37509 = CARTESIAN_POINT ( 'NONE',  ( -0.4855643044619415427, 0.05413385826771626580, -0.4176697321401330321 ) ) ;
#37510 = DIRECTION ( 'NONE',  ( 0.000000000000000000, 0.000000000000000000, 1.000000000000000000 ) ) ;
#37511 = CARTESIAN_POINT ( 'NONE',  ( 0.4199475065616803948, -0.6046776061558809534, -0.2411417322834644161 ) ) ;
#37512 = CARTESIAN_POINT ( 'NONE',  ( -0.5905511811023613777, -0.6692913385826771977, 8.415575281601705876E-17 ) ) ;
#37513 = CARTESIAN_POINT ( 'NONE',  ( -0.4330708661417315697, 0.1771653543307087630, 0.000000000000000000 ) ) ;
#37514 = CARTESIAN_POINT ( 'NONE',  ( 0.2821522309711292364, -0.6692913385826771977, 0.1292274648535927661 ) ) ;
#37515 = CARTESIAN_POINT ( 'NONE',  ( 1.141732283464567788, -0.5511811023622047445, 6.969142054262312111E-17 ) ) ;
#37516 = CARTESIAN_POINT ( 'NONE',  ( -0.4265091863517051496, -0.6692913385826771977, 0.1292274648535927661 ) ) ;
#37517 = PRESENTATION_STYLE_ASSIGNMENT (( #12685 ) ) ;
#37519 = CARTESIAN_POINT ( 'NONE',  ( 1.456692913385827515, 0.2952755905511811885, 0.000000000000000000 ) ) ;
#37518 = CARTESIAN_POINT ( 'NONE',  ( -2.118110236220477116, 0.000000000000000000, 0.4498537592782676509 ) ) ;
#37520 = FACE_OUTER_BOUND ( 'NONE', #34233, .T. ) ;
#37521 = CARTESIAN_POINT ( 'NONE',  ( -0.3392501089628019995, 0.1958661417322832277, -2.223097112860892288 ) ) ;
#37522 = CARTESIAN_POINT ( 'NONE',  ( -1.541994750656167090, -0.6692913385826773087, -0.1292274648535924053 ) ) ;
#37523 = CARTESIAN_POINT ( 'NONE',  ( -0.8989501312335946848, 0.2952755905511810774, -0.1292274648535930714 ) ) ;
#37524 = CARTESIAN_POINT ( 'NONE',  ( -0.4091458600556402980, -0.2362204724409451284, -0.2099737532808398921 ) ) ;
#37525 = CARTESIAN_POINT ( 'NONE',  ( 0.2891555358219910499, 0.2891555358219910499, -2.657480314960630530 ) ) ;
#37526 = ORIENTED_EDGE ( 'NONE', *, *, #19143, .F. ) ;
#37527 = CARTESIAN_POINT ( 'NONE',  ( 0.4658792650918641698, -0.08942795157528024563, -0.3641732283464568787 ) ) ;
#37528 = CARTESIAN_POINT ( 'NONE',  ( -0.1958661417322834220, -0.3392501089628018884, -1.317585301837270295 ) ) ;
#37529 = CARTESIAN_POINT ( 'NONE',  ( 0.6955380577427828781, 0.05413385826771626580, -0.4176697321401330321 ) ) ;
#37530 = CARTESIAN_POINT ( 'NONE',  ( 5.785732909357575061E-17, -0.4724409448818898682, -2.913385826771653697 ) ) ;
#37531 = CARTESIAN_POINT ( 'NONE',  ( -0.5618802787717172009, -5.582469467804009507E-15, -0.4118484887281986251 ) ) ;
#37532 = CARTESIAN_POINT ( 'NONE',  ( -0.3937007874015740483, -0.1870078740157479769, 0.3641732283464567677 ) ) ;
#37533 = CARTESIAN_POINT ( 'NONE',  ( -1.719160104986876103, -0.004921259842519576551, 0.3153832671262227771 ) ) ;
#37534 = CARTESIAN_POINT ( 'NONE',  ( 1.240157480314961314, 0.1660481256975883668, -0.3530559997133364547 ) ) ;
#37535 = CARTESIAN_POINT ( 'NONE',  ( 1.345144356955381593, -0.2845877964562161244, -0.3641732283464567121 ) ) ;
#37536 = CARTESIAN_POINT ( 'NONE',  ( -0.1246719160104980823, -0.6692913385826773087, -0.1292274648535924053 ) ) ;
#37537 = CARTESIAN_POINT ( 'NONE',  ( 0.3917322834645668994, 0.1049643490035304522, -0.5196657235882398140 ) ) ;
#37538 = CARTESIAN_POINT ( 'NONE',  ( -0.5905511811023613777, -0.6692913385826771977, 8.415575281601705876E-17 ) ) ;
#37539 = CARTESIAN_POINT ( 'NONE',  ( -1.305774278215222184, -0.5511811023622048555, -0.09757992244046775898 ) ) ;
#37540 = EDGE_CURVE ( 'NONE', #36844, #44871, #25061, .T. ) ;
#37541 = CARTESIAN_POINT ( 'NONE',  ( -0.4330708661417315697, 0.2952755905511811885, 0.000000000000000000 ) ) ;
#37542 = CARTESIAN_POINT ( 'NONE',  ( 1.620734908136483465, -0.6692913385826771977, 0.1292274648535927661 ) ) ;
#37543 = FACE_OUTER_BOUND ( 'NONE', #67605, .T. ) ;
#37544 = ORIENTED_EDGE ( 'NONE', *, *, #44425, .F. ) ;
#37545 = CARTESIAN_POINT ( 'NONE',  ( -0.3392501089628019995, 0.1958661417322831999, -1.912748974574490113 ) ) ;
#37546 = CARTESIAN_POINT ( 'NONE',  ( 0.5249343832021005074, -0.6046776061558807314, 0.2411417322834647770 ) ) ;
#37547 = VERTEX_POINT ( 'NONE', #60775 ) ;
#37548 = CARTESIAN_POINT ( 'NONE',  ( -0.5446194225721777693, -0.3162353388693409650, -0.4822834645669289433 ) ) ;
#37549 = CARTESIAN_POINT ( 'NONE',  ( -1.646981627296586703, -0.05778040916215522460, 0.4822834645669289988 ) ) ;
#37550 = CARTESIAN_POINT ( 'NONE',  ( 0.6955380577427828781, 0.05413385826771626580, -0.4176697321401330321 ) ) ;
#37551 = EDGE_CURVE ( 'NONE', #75751, #15414, #39876, .T. ) ;
#37552 = CARTESIAN_POINT ( 'NONE',  ( -0.006561679790025524116, -0.05778040916215560624, -0.4822834645669293319 ) ) ;
#37553 = CARTESIAN_POINT ( 'NONE',  ( -0.1958661417322836718, 0.3392501089628017219, -1.200131233595800540 ) ) ;
#37554 = CARTESIAN_POINT ( 'NONE',  ( -0.9448818897637790704, -0.1870078740157479769, 0.4822834645669291653 ) ) ;
#37555 = CARTESIAN_POINT ( 'NONE',  ( 0.3937007874015754361, -0.1870078740157479769, 0.4822834645669291653 ) ) ;
#37556 = CARTESIAN_POINT ( 'NONE',  ( -0.5511811023622038563, -0.1870078740157479769, 0.4822834645669291653 ) ) ;
#37557 = CARTESIAN_POINT ( 'NONE',  ( 0.2690288713910767848, 0.1771653543307087630, 0.09757992244046791164 ) ) ;
#37558 = LINE ( 'NONE', #19026, #3293 ) ;
#37559 = CARTESIAN_POINT ( 'NONE',  ( -0.1902887139107604098, -0.6692913385826771977, 0.1292274648535927661 ) ) ;
#37560 = CARTESIAN_POINT ( 'NONE',  ( -0.1208384647389192101, 0.3726288332213502641, 1.112018681666451222E-17 ) ) ;
#37561 = CARTESIAN_POINT ( 'NONE',  ( 1.489501312335958172, -0.05778040916215560624, -0.4822834645669293319 ) ) ;
#37562 = CARTESIAN_POINT ( 'NONE',  ( -0.3392501089628017219, -0.1958661417322836718, -2.564304461942256808 ) ) ;
#37563 = VERTEX_POINT ( 'NONE', #47307 ) ;
#37564 = ORIENTED_EDGE ( 'NONE', *, *, #28626, .F. ) ;
#37565 = CARTESIAN_POINT ( 'NONE',  ( 0.8202099737532814183, -0.6692913385826773087, -0.1292274648535924053 ) ) ;
#37566 = CARTESIAN_POINT ( 'NONE',  ( 0.1246719160104994284, -0.5511811023622046335, 0.09757992244046803654 ) ) ;
#37568 = CARTESIAN_POINT ( 'NONE',  ( -0.06873123812452887338, -2.191421614605370878E-15, 0.4445507791589071167 ) ) ;
#37567 = CARTESIAN_POINT ( 'NONE',  ( 1.509186351706037543, -0.004921259842519576551, 0.3153832671262227771 ) ) ;
#37569 = CARTESIAN_POINT ( 'NONE',  ( 0.1049643490035304938, -0.3917322834645669549, -1.272309711286089273 ) ) ;
#37570 = CARTESIAN_POINT ( 'NONE',  ( -0.3458507752293909498, 0.3458507752293907833, 0.06102362204724409017 ) ) ;
#37571 =( NAMED_UNIT ( * ) PLANE_ANGLE_UNIT ( ) SI_UNIT ( $, .RADIAN. ) );
#37572 = B_SPLINE_CURVE_WITH_KNOTS ( 'NONE', 3,
 ( #21591, #8972, #67460, #34646, #3068, #53567, #80107 ),
 .UNSPECIFIED., .F., .F.,
 ( 4, 3, 4 ),
 ( 7.703719777548943412E-34, 0.001246232571205258119, 0.002492492258783253305 ),
 .UNSPECIFIED. ) ;
#37573 = CARTESIAN_POINT ( 'NONE',  ( -0.1070741851644051862, -0.3996062992125986590, -2.826115485564304475 ) ) ;
#37574 = CARTESIAN_POINT ( 'NONE',  ( 0.2887139107611556010, -0.6046776061558807314, 0.2411417322834647770 ) ) ;
#37575 = CARTESIAN_POINT ( 'NONE',  ( -1.423884514435694859, -0.05778040916215560624, -0.4822834645669293319 ) ) ;
#37576 = CARTESIAN_POINT ( 'NONE',  ( -1.332020997375327642, -0.3162353388693409650, -0.4822834645669289433 ) ) ;
#37577 = CARTESIAN_POINT ( 'NONE',  ( 0.1706036745406830368, 0.05413385826771666132, 0.4176697321401328100 ) ) ;
#37578 = CARTESIAN_POINT ( 'NONE',  ( 0.9711286089238851948, 0.2306618581243848609, 0.2411417322834645549 ) ) ;
#37579 = CARTESIAN_POINT ( 'NONE',  ( 1.528871391076116026, 0.1771653543307087630, 0.09757992244046791164 ) ) ;
#37580 = CARTESIAN_POINT ( 'NONE',  ( 0.7480314960629927956, 0.1771653543307087630, 0.000000000000000000 ) ) ;
#37581 = CARTESIAN_POINT ( 'NONE',  ( -1.023622047244093558, -0.1870078740157479769, 0.4822834645669291653 ) ) ;
#37582 = CARTESIAN_POINT ( 'NONE',  ( -0.3996062992125985480, -7.340648628747423112E-17, -0.4311023622047244208 ) ) ;
#37583 = CARTESIAN_POINT ( 'NONE',  ( 1.561679790026247350, 0.05413385826771626580, -0.4176697321401330321 ) ) ;
#37584 = CARTESIAN_POINT ( 'NONE',  ( 0.2867679344610365999, 0.2867679344610365999, -0.1299212598425196485 ) ) ;
#37586 = CARTESIAN_POINT ( 'NONE',  ( -0.4606233198248986804, 1.422786159591911348, 2.138962479395379646 ) ) ;
#37585 = CARTESIAN_POINT ( 'NONE',  ( 1.318897637795276356, -0.5400638737290844871, 0.3530559997133364547 ) ) ;
#37587 = CARTESIAN_POINT ( 'NONE',  ( -1.633858267716534529, -0.4536011799217368745, -0.2665933059059886201 ) ) ;
#37588 = CARTESIAN_POINT ( 'NONE',  ( 0.09842519685039434474, 0.1660481256975885056, 0.3530559997133364547 ) ) ;
#37589 = CARTESIAN_POINT ( 'NONE',  ( 0.8923884514435701520, -0.5023911411419708095, -0.1820866141732282451 ) ) ;
#37590 = CARTESIAN_POINT ( 'NONE',  ( -1.509186351706035767, -0.004921259842519870586, -0.3153832671262229437 ) ) ;
#37591 = CARTESIAN_POINT ( 'NONE',  ( 0.8792650918635177559, 0.05413385826771666132, 0.4176697321401328100 ) ) ;
#37592 = CARTESIAN_POINT ( 'NONE',  ( 1.968503937007874072, 0.000000000000000000, 5.701968306260621233 ) ) ;
#37593 = CARTESIAN_POINT ( 'NONE',  ( -0.4527559055118102749, 0.07958543189024085140, 0.2665933059059887866 ) ) ;
#37594 = CARTESIAN_POINT ( 'NONE',  ( -0.4133858267716528645, 0.1660481256975883668, -0.3530559997133364547 ) ) ;
#37595 = CARTESIAN_POINT ( 'NONE',  ( 1.437007874015748810, -0.5400638737290845981, -0.3530559997133363437 ) ) ;
#37596 = CARTESIAN_POINT ( 'NONE',  ( -1.174540682414697335, -0.3162353388693409650, -0.4822834645669289433 ) ) ;
#37597 = CARTESIAN_POINT ( 'NONE',  ( 1.489501312335958172, -0.3162353388693405765, 0.4822834645669290543 ) ) ;
#37598 = CARTESIAN_POINT ( 'NONE',  ( 0.1049643490035304799, -0.3917322834645670104, -0.7119615729996870979 ) ) ;
#37599 = CARTESIAN_POINT ( 'NONE',  ( -1.161417322834644716, 0.07958543189024085140, 0.2665933059059887866 ) ) ;
#37600 =( BOUNDED_CURVE ( )  B_SPLINE_CURVE ( 2, ( #38920, #78075, #51119, #33025, #76814, #45639, #19562, #32608, #71334, #1059, #31778, #45221, #46057 ),
 .UNSPECIFIED., .F., .F. ) 
 B_SPLINE_CURVE_WITH_KNOTS ( ( 3, 2, 2, 2, 2, 2, 3 ),
 ( 0.8875000000000000666, 0.8916666666666668295, 0.8958333333333334814, 0.9000000000000001332, 0.9041666666666667851, 0.9083333333333334370, 0.9125000000000000888 ),
 .UNSPECIFIED. ) 
 CURVE ( )  GEOMETRIC_REPRESENTATION_ITEM ( )  RATIONAL_B_SPLINE_CURVE ( ( 0.9999999999999991118, 0.9659258262890692004, 1.000000000000000000, 0.9659258262890683122, 1.000000000000000000, 0.9659258262890683122, 1.000000000000000000, 0.9659258262890683122, 1.000000000000000000, 0.9659258262890683122, 1.000000000000000000, 0.9659258262890674240, 1.000000000000000888 ) ) 
 REPRESENTATION_ITEM ( '' )  );
#37601 = DIRECTION ( 'NONE',  ( 0.000000000000000000, 0.000000000000000000, 1.000000000000000000 ) ) ;
#37602 = CARTESIAN_POINT ( 'NONE',  ( 0.8005249343832027131, 0.05413385826771666132, 0.4176697321401328100 ) ) ;
#37603 = CARTESIAN_POINT ( 'NONE',  ( 0.4724409448818897572, -0.1265901696524988906, -2.393044619422572072 ) ) ;
#37604 = CARTESIAN_POINT ( 'NONE',  ( -1.509186351706035767, 0.05413385826771626580, -0.4176697321401330321 ) ) ;
#37605 = CARTESIAN_POINT ( 'NONE',  ( -1.607611548556429737, 0.1771653543307087075, -0.09757992244046823083 ) ) ;
#37606 = CARTESIAN_POINT ( 'NONE',  ( -0.9317585301837263412, -0.004921259842519576551, 0.3153832671262227771 ) ) ;
#37607 = CARTESIAN_POINT ( 'NONE',  ( 1.614173228346457378, -0.5511811023622047445, 6.969142054262312111E-17 ) ) ;
#37608 = CARTESIAN_POINT ( 'NONE',  ( -0.3937007874015740483, -0.1870078740157479769, 0.4822834645669291653 ) ) ;
#37609 = CARTESIAN_POINT ( 'NONE',  ( 0.1509186351706045259, -0.08942795157528024563, -0.3641732283464568787 ) ) ;
#37610 = CARTESIAN_POINT ( 'NONE',  ( -1.443569553805773564, -0.5023911411419708095, 0.1820866141732285504 ) ) ;
#37611 = CARTESIAN_POINT ( 'NONE',  ( 1.318897637795276356, 0.07958543189024071263, -0.2665933059059888421 ) ) ;
#37612 = CARTESIAN_POINT ( 'NONE',  ( 1.010498687664042716, -0.4281496062992124485, 0.4176697321401328655 ) ) ;
#37613 = CARTESIAN_POINT ( 'NONE',  ( 1.410761154855643795, -0.3162353388693405765, 0.4822834645669290543 ) ) ;
#37614 = CARTESIAN_POINT ( 'NONE',  ( 0.2296587926509192634, -0.2845877964562159024, 0.3641732283464567677 ) ) ;
#37615 = EDGE_CURVE ( 'NONE', #57884, #25547, #17000, .T. ) ;
#37616 = CARTESIAN_POINT ( 'NONE',  ( 0.3018372703412079971, 0.05413385826771626580, -0.4176697321401330321 ) ) ;
#37617 = CARTESIAN_POINT ( 'NONE',  ( 1.056430446194226436, -0.5511811023622048555, -0.09757992244046775898 ) ) ;
#37618 = ORIENTED_EDGE ( 'NONE', *, *, #10682, .T. ) ;
#37619 = CARTESIAN_POINT ( 'NONE',  ( 1.437007874015748810, 0.1660481256975885056, 0.3530559997133364547 ) ) ;
#37620 = CARTESIAN_POINT ( 'NONE',  ( -1.404199475065615932, -0.4281496062992127816, -0.4176697321401328100 ) ) ;
#37621 = CARTESIAN_POINT ( 'NONE',  ( -0.3018372703412066094, 0.05413385826771666132, 0.4176697321401328100 ) ) ;
#37622 = CARTESIAN_POINT ( 'NONE',  ( 0.2925321140481932369, 0.2925321140481932369, -0.2952755905511811330 ) ) ;
#37623 = CARTESIAN_POINT ( 'NONE',  ( -0.3996062992125985480, -7.340648628747423112E-17, -2.793307086614173151 ) ) ;
#37624 = CARTESIAN_POINT ( 'NONE',  ( 0.4068241469816279987, -0.4281496062992127816, -0.4176697321401328100 ) ) ;
#37625 = CARTESIAN_POINT ( 'NONE',  ( 1.076115485564305141, -0.5023911411419708095, 0.1820866141732285504 ) ) ;
#37626 = CARTESIAN_POINT ( 'NONE',  ( -0.006561679790025524116, -0.05778040916215560624, -0.4822834645669293319 ) ) ;
#37627 = CARTESIAN_POINT ( 'NONE',  ( 0.1706036745406830368, 0.05413385826771666132, 0.4176697321401328100 ) ) ;
#37628 = CARTESIAN_POINT ( 'NONE',  ( 4.893765752498283924E-17, -0.3996062992125986035, -2.283464566929133799 ) ) ;
#37629 = CARTESIAN_POINT ( 'NONE',  ( 0.2891555358219910499, 0.2891555358219910499, -1.397637795275590733 ) ) ;
#37630 = CARTESIAN_POINT ( 'NONE',  ( -0.2517570632375117912, 1.135012049176707949, 1.093517086496077262 ) ) ;
#37631 = DIRECTION ( 'NONE',  ( -1.000000000000000000, -0.000000000000000000, -0.000000000000000000 ) ) ;
#37632 = CARTESIAN_POINT ( 'NONE',  ( 0.2867679344610366554, -0.2867679344610365444, -0.5629921259842519676 ) ) ;
#37633 = CARTESIAN_POINT ( 'NONE',  ( -0.5774278215223089816, 0.1283753931104746893, -0.1820866141732285504 ) ) ;
#37634 = CARTESIAN_POINT ( 'NONE',  ( -0.9514435695538050464, -0.3162353388693405765, 0.4822834645669290543 ) ) ;
#37635 = CARTESIAN_POINT ( 'NONE',  ( 0.3420746716998660508, -0.1974969037888704149, -2.543963254593176071 ) ) ;
#37636 = CARTESIAN_POINT ( 'NONE',  ( 0.8202099737532814183, -0.6692913385826773087, -0.1292274648535924053 ) ) ;
#37637 = CARTESIAN_POINT ( 'NONE',  ( -1.601049868766403650, 0.2306618581243847221, -0.2411417322834647770 ) ) ;
#37638 = CARTESIAN_POINT ( 'NONE',  ( 0.8595800524934390507, -0.05778040916215560624, -0.4822834645669293319 ) ) ;
#37639 = CARTESIAN_POINT ( 'NONE',  ( 0.1265901696524989462, 0.4724409448818897572, -2.670603674540682260 ) ) ;
#37640 = CARTESIAN_POINT ( 'NONE',  ( -9.787531504996567848E-17, 0.3996062992125986035, -2.362204724409448620 ) ) ;
#37641 = DIRECTION ( 'NONE',  ( -0.000000000000000000, -1.000000000000000000, -0.000000000000000000 ) ) ;
#37642 = CARTESIAN_POINT ( 'NONE',  ( 0.9842519685039375910, 0.2952755905511811885, 0.000000000000000000 ) ) ;
#37643 = CARTESIAN_POINT ( 'NONE',  ( 0.7677165354330716118, -0.5400638737290844871, 0.3530559997133364547 ) ) ;
#37644 = CARTESIAN_POINT ( 'NONE',  ( 0.7020997375328090762, -0.08942795157528024563, -0.3641732283464568787 ) ) ;
#37645 = CARTESIAN_POINT ( 'NONE',  ( 1.463254593175853824, -0.6692913385826771977, 0.1292274648535927661 ) ) ;
#37646 = CARTESIAN_POINT ( 'NONE',  ( 0.1958661417322836440, -0.3392501089628017219, -0.3339895013123360679 ) ) ;
#37647 = DIRECTION ( 'NONE',  ( 0.000000000000000000, -0.000000000000000000, 1.000000000000000000 ) ) ;
#37648 = CARTESIAN_POINT ( 'NONE',  ( 0.7217847769028878924, 0.05413385826771666132, 0.4176697321401328100 ) ) ;
#37649 = CARTESIAN_POINT ( 'NONE',  ( 1.574803149606299746, -0.1870078740157480601, -0.3641732283464567677 ) ) ;
#37650 = CARTESIAN_POINT ( 'NONE',  ( -0.5183727034120726440, -0.6692913385826773087, -0.1292274648535924053 ) ) ;
#37651 = CARTESIAN_POINT ( 'NONE',  ( -1.003937007874015297, -0.5400638737290845981, -0.3530559997133363437 ) ) ;
#37652 = CARTESIAN_POINT ( 'NONE',  ( 1.292650918635171564, 0.2952755905511811885, 0.1292274648535926551 ) ) ;
#37653 = CARTESIAN_POINT ( 'NONE',  ( 0.3917322834645669549, 0.1049643490035304660, -0.5242782152230972548 ) ) ;
#37654 = CARTESIAN_POINT ( 'NONE',  ( 0.1958661417322836440, -0.3392501089628017219, -1.658792650918635259 ) ) ;
#37655 = CARTESIAN_POINT ( 'NONE',  ( -0.2867679344610365999, 0.2867679344610364889, -2.688976377952755570 ) ) ;
#37656 = CARTESIAN_POINT ( 'NONE',  ( 1.351706036745407680, 0.05413385826771666132, 0.4176697321401328100 ) ) ;
#37657 = ORIENTED_EDGE ( 'NONE', *, *, #30323, .T. ) ;
#37658 = CARTESIAN_POINT ( 'NONE',  ( 0.3996062992125986590, -0.1070741851644053111, -0.1115485564304461857 ) ) ;
#37659 = ORIENTED_EDGE ( 'NONE', *, *, #59375, .F. ) ;
#37660 = LINE ( 'NONE', #10771, #39514 ) ;
#37661 = CARTESIAN_POINT ( 'NONE',  ( 1.371391076115485719, -0.5511811023622048555, -0.09757992244046775898 ) ) ;
#37662 = CARTESIAN_POINT ( 'NONE',  ( 0.3996062992125986035, 0.1070741851644054776, -1.541994750656167978 ) ) ;
#37663 = CARTESIAN_POINT ( 'NONE',  ( 1.384514435695538559, 0.1771653543307087075, -0.09757992244046823083 ) ) ;
#37664 = DIRECTION ( 'NONE',  ( -0.000000000000000000, -1.000000000000000000, -0.000000000000000000 ) ) ;
#37665 = FACE_OUTER_BOUND ( 'NONE', #76177, .T. ) ;
#37666 = CARTESIAN_POINT ( 'NONE',  ( -0.2217488924428978880, 1.907169838053261124, 0.2213636967189943072 ) ) ;
#37667 = CARTESIAN_POINT ( 'NONE',  ( -0.1958661417322834220, -0.3392501089628018884, -0.6227034120734910028 ) ) ;
#37668 = CARTESIAN_POINT ( 'NONE',  ( -0.7677165354330699465, -0.4536011799217368745, -0.2665933059059886201 ) ) ;
#37669 = AXIS2_PLACEMENT_3D ( 'NONE', #66187, #73753, #34190 ) ;
#37670 = CARTESIAN_POINT ( 'NONE',  ( -1.397637795275589623, 0.07958543189024085140, 0.2665933059059887866 ) ) ;
#37671 = CARTESIAN_POINT ( 'NONE',  ( -1.292650918635170010, 0.2952755905511810774, -0.1292274648535930714 ) ) ;
#37672 = CARTESIAN_POINT ( 'NONE',  ( 0.09186351706036799403, -0.4281496062992127816, -0.4176697321401328100 ) ) ;
#37673 = CARTESIAN_POINT ( 'NONE',  ( 1.450131233595801428, 0.2952755905511811885, 0.1292274648535926551 ) ) ;
#37674 = EDGE_LOOP ( 'NONE', ( #13720, #67103, #4852, #44480 ) ) ;
#37675 = EDGE_CURVE ( 'NONE', #59607, #41772, #42240, .T. ) ;
#37676 = CARTESIAN_POINT ( 'NONE',  ( 1.338582677165355062, -0.1870078740157480879, -0.4822834645669291653 ) ) ;
#37677 = CARTESIAN_POINT ( 'NONE',  ( -1.154855643044618629, 0.1539470093639523085, 0.1968503937007873850 ) ) ;
#37678 = SHAPE_REPRESENTATION_RELATIONSHIP ( 'NONE' , 'NONE' ,  #48103, #60502 ) ;
#37679 = CARTESIAN_POINT ( 'NONE',  ( -0.3458507752293909498, 0.3458507752293907833, -2.224409448818897239 ) ) ;
#37680 = CARTESIAN_POINT ( 'NONE',  ( 2.129998074986495737, 1.668416680336017865, 0.4562095852119728012 ) ) ;
#37681 = CARTESIAN_POINT ( 'NONE',  ( -0.3608923884514428360, 0.1771653543307087630, 0.09757992244046791164 ) ) ;
#37682 = EDGE_CURVE ( 'NONE', #2500, #57445, #59731, .T. ) ;
#37683 = CARTESIAN_POINT ( 'NONE',  ( -1.364829396325458521, -0.6046776061558807314, 0.2411417322834647770 ) ) ;
#37684 = CARTESIAN_POINT ( 'NONE',  ( 0.8989501312335964611, 0.2952755905511811885, 0.1292274648535926551 ) ) ;
#37685 = EDGE_LOOP ( 'NONE', ( #51100, #78071, #8262, #40629 ) ) ;
#37687 = DIRECTION ( 'NONE',  ( 0.000000000000000000, 0.000000000000000000, -1.000000000000000000 ) ) ;
#37686 = CARTESIAN_POINT ( 'NONE',  ( 0.7677165354330716118, 0.1660481256975883391, -0.3530559997133364547 ) ) ;
#37688 = CARTESIAN_POINT ( 'NONE',  ( 1.108923884514436686, -0.3162353388693409650, -0.4822834645669289433 ) ) ;
#37689 = CARTESIAN_POINT ( 'NONE',  ( -1.108923884514435132, -0.3162353388693405765, 0.4822834645669290543 ) ) ;
#37690 = CARTESIAN_POINT ( 'NONE',  ( 0.1958661417322834497, 0.3392501089628018329, -0.2243901330370585701 ) ) ;
#37691 = CARTESIAN_POINT ( 'NONE',  ( -0.1771653543307080136, -0.4536011799217367080, 0.2665933059059888421 ) ) ;
#37692 = CARTESIAN_POINT ( 'NONE',  ( 0.3392501089628018884, -0.1958661417322834220, -0.9770341207349081403 ) ) ;
#37693 = CARTESIAN_POINT ( 'NONE',  ( -0.6692913385826764205, 0.1771653543307087630, 0.000000000000000000 ) ) ;
#37694 = CARTESIAN_POINT ( 'NONE',  ( 0.6955380577427828781, -0.004921259842519870586, -0.3153832671262229437 ) ) ;
#37695 = CARTESIAN_POINT ( 'NONE',  ( 0.04593175853018440641, 0.2952755905511810774, -0.1292274648535930714 ) ) ;
#37696 = CARTESIAN_POINT ( 'NONE',  ( -0.5380577427821514602, -0.004921259842519576551, 0.3153832671262227771 ) ) ;
#37697 = CARTESIAN_POINT ( 'NONE',  ( 4.797336870675656522E-17, -0.3917322834645670104, -2.905511811023621771 ) ) ;
#37698 = CARTESIAN_POINT ( 'NONE',  ( 1.240157480314961314, -0.5400638737290844871, 0.3530559997133364547 ) ) ;
#37699 = EDGE_CURVE ( 'NONE', #38952, #24575, #26033, .T. ) ;
#37700 = EDGE_CURVE ( 'NONE', #13300, #71398, #9244, .T. ) ;
#37701 = CARTESIAN_POINT ( 'NONE',  ( -0.8595800524934373854, -0.05778040916215522460, 0.4822834645669289988 ) ) ;
#37702 = CARTESIAN_POINT ( 'NONE',  ( -0.4724409448818898682, -8.678599364036362592E-17, -1.375984251968503713 ) ) ;
#37703 = CARTESIAN_POINT ( 'NONE',  ( -0.4330708661417315697, 0.2952755905511811885, 0.000000000000000000 ) ) ;
#37704 = CARTESIAN_POINT ( 'NONE',  ( -1.122047244094487306, 0.1660481256975883668, -0.3530559997133364547 ) ) ;
#37705 = CARTESIAN_POINT ( 'NONE',  ( 1.108923884514436686, -0.2845877964562161244, -0.3641732283464567121 ) ) ;
#37706 = CARTESIAN_POINT ( 'NONE',  ( 0.1771653543307093182, 0.07958543189024085140, 0.2665933059059887866 ) ) ;
#37707 = CARTESIAN_POINT ( 'NONE',  ( -0.4330708661417315697, 0.2952755905511811885, 0.000000000000000000 ) ) ;
#37708 = CARTESIAN_POINT ( 'NONE',  ( -1.233595800524933894, -0.6046776061558809534, -0.2411417322834644161 ) ) ;
#37709 = DIRECTION ( 'NONE',  ( 1.000000000000000000, 0.000000000000000000, 0.000000000000000000 ) ) ;
#37710 = CARTESIAN_POINT ( 'NONE',  ( 1.627296587926509996, -0.5023911411419708095, 0.1820866141732285504 ) ) ;
#37711 = CARTESIAN_POINT ( 'NONE',  ( -0.3674540682414689785, 0.2306618581243848609, 0.2411417322834645549 ) ) ;
#37712 = CARTESIAN_POINT ( 'NONE',  ( -1.076115485564303809, 0.2306618581243848609, 0.2411417322834645549 ) ) ;
#37713 = VERTEX_POINT ( 'NONE', #76977 ) ;
#37714 = CARTESIAN_POINT ( 'NONE',  ( 0.2925321140481932369, -0.2925321140481931814, -2.064960629921259283 ) ) ;
#37715 = CARTESIAN_POINT ( 'NONE',  ( 1.010498687664042716, 0.05413385826771626580, -0.4176697321401330321 ) ) ;
#37716 = CARTESIAN_POINT ( 'NONE',  ( -0.6496062992125976043, -0.4536011799217367080, 0.2665933059059888421 ) ) ;
#37717 = CARTESIAN_POINT ( 'NONE',  ( -0.1070741851644056997, 0.3996062992125984925, -1.343175853018372834 ) ) ;
#37718 = CARTESIAN_POINT ( 'NONE',  ( -0.8333333333333323711, -0.6692913385826773087, -0.1292274648535924053 ) ) ;
#37719 = CARTESIAN_POINT ( 'NONE',  ( 1.292650918635171564, -0.6692913385826773087, -0.1292274648535924053 ) ) ;
#37720 = CARTESIAN_POINT ( 'NONE',  ( 0.9251968503937015864, 0.1660481256975883668, -0.3530559997133364547 ) ) ;
#37721 = LINE ( 'NONE', #63395, #41193 ) ;
#37722 = CARTESIAN_POINT ( 'NONE',  ( -1.246719160104986512, -0.004921259842519576551, 0.3153832671262227771 ) ) ;
#37723 = CARTESIAN_POINT ( 'NONE',  ( 0.1998031496062994128, -0.3460692066303957537, -0.4835958005249343938 ) ) ;
#37724 = CARTESIAN_POINT ( 'NONE',  ( 0.1998031496062992740, 0.3460692066303959757, -0.9317585301837270073 ) ) ;
#37725 = CARTESIAN_POINT ( 'NONE',  ( 0.3420746716998660508, -0.1974969037888703871, -0.4199475065616798952 ) ) ;
#37726 = CARTESIAN_POINT ( 'NONE',  ( 0.4476898780826904511, 1.379730629998464631, 2.610432142638456465 ) ) ;
#37727 = CARTESIAN_POINT ( 'NONE',  ( 1.069553805774278832, 0.1771653543307087075, -0.09757992244046823083 ) ) ;
#37728 = CARTESIAN_POINT ( 'NONE',  ( 0.9186351706036751663, -0.5023911411419708095, 0.1820866141732285504 ) ) ;
#37729 = CIRCLE ( 'NONE', #6793, 0.1771653543307085410 ) ;
#37730 = CARTESIAN_POINT ( 'NONE',  ( 0.5314960629921264834, 0.1660481256975883668, -0.3530559997133364547 ) ) ;
#37731 = CARTESIAN_POINT ( 'NONE',  ( 1.574803149606299746, -0.1870078740157479769, 0.4822834645669291653 ) ) ;
#37732 = CARTESIAN_POINT ( 'NONE',  ( 0.3949938075777409408, -0.1058382717557499186, -1.448162729658792669 ) ) ;
#37733 = CARTESIAN_POINT ( 'NONE',  ( 0.7480314960629927956, 0.1771653543307087630, 0.000000000000000000 ) ) ;
#37734 = CARTESIAN_POINT ( 'NONE',  ( -0.2559055118110227234, -0.5400638737290844871, 0.3530559997133364547 ) ) ;
#37735 = CARTESIAN_POINT ( 'NONE',  ( -1.076115485564303809, -0.6046776061558809534, -0.2411417322834644161 ) ) ;
#37736 = CARTESIAN_POINT ( 'NONE',  ( 1.358267716535433323, 0.1660481256975885056, 0.3530559997133364547 ) ) ;
#37737 = CARTESIAN_POINT ( 'NONE',  ( -1.157146581871515012E-16, 0.4724409448818898682, -1.417322834645669216 ) ) ;
#37738 = CARTESIAN_POINT ( 'NONE',  ( -0.3460692066303960868, 0.1998031496062990242, -2.545931758530183497 ) ) ;
#37739 = CARTESIAN_POINT ( 'NONE',  ( -0.1968503937007867743, -0.5511811023622047445, 6.969142054262312111E-17 ) ) ;
#37740 = ORIENTED_EDGE ( 'NONE', *, *, #6951, .F. ) ;
#37741 = ORIENTED_EDGE ( 'NONE', *, *, #47486, .T. ) ;
#37742 = CARTESIAN_POINT ( 'NONE',  ( -0.6692913385826764205, -0.6692913385826771977, 8.415575281601705876E-17 ) ) ;
#37743 = CARTESIAN_POINT ( 'NONE',  ( -0.5839895013123351797, -0.6692913385826771977, 0.1292274648535927661 ) ) ;
#37744 = CARTESIAN_POINT ( 'NONE',  ( -0.7086614173228339419, -0.1870078740157479769, 0.4822834645669291653 ) ) ;
#37745 = CARTESIAN_POINT ( 'NONE',  ( 0.3477690288713918276, -0.6692913385826773087, -0.1292274648535924053 ) ) ;
#37746 = CARTESIAN_POINT ( 'NONE',  ( -0.4986876640419939388, 0.2306618581243847221, -0.2411417322834647770 ) ) ;
#37747 = CARTESIAN_POINT ( 'NONE',  ( -1.312335958005248715, 0.2306618581243848609, 0.2411417322834645549 ) ) ;
#37748 = VECTOR ( 'NONE', #34124, 39.37007874015748143 ) ;
#37749 = CARTESIAN_POINT ( 'NONE',  ( -0.8661417322834640276, -0.1870078740157480879, -0.4822834645669291653 ) ) ;
#37750 = CARTESIAN_POINT ( 'NONE',  ( 0.6824146981627303710, 0.2306618581243847221, -0.2411417322834647770 ) ) ;
#37751 = EDGE_CURVE ( 'NONE', #19878, #36616, #31938, .T. ) ;
#37752 = CARTESIAN_POINT ( 'NONE',  ( -0.1049643490035307020, 0.3917322834645669549, -1.416010498687664043 ) ) ;
#37753 = CARTESIAN_POINT ( 'NONE',  ( -0.4658792650918627265, -0.2845877964562161244, -0.3641732283464567121 ) ) ;
#37754 = VERTEX_POINT ( 'NONE', #71499 ) ;
#37755 = CARTESIAN_POINT ( 'NONE',  ( -9.674558042662121740E-17, 0.3949938075777409963, -1.574803149606299302 ) ) ;
#37756 = ORIENTED_EDGE ( 'NONE', *, *, #82229, .F. ) ;
#37757 = CARTESIAN_POINT ( 'NONE',  ( -1.384514435695537005, 0.1771653543307087630, 0.09757992244046791164 ) ) ;
#37758 = CARTESIAN_POINT ( 'NONE',  ( -1.233595800524933894, -0.6046776061558809534, -0.2411417322834644161 ) ) ;
#37759 = CARTESIAN_POINT ( 'NONE',  ( -1.062992125984250968, -0.6692913385826771977, 8.415575281601705876E-17 ) ) ;
#37760 = CARTESIAN_POINT ( 'NONE',  ( -0.1998031496062991907, -0.3460692066303959757, -0.2230971128608923715 ) ) ;
#37761 = CARTESIAN_POINT ( 'NONE',  ( -1.318897637795274802, -0.5400638737290845981, -0.3530559997133363437 ) ) ;
#37762 = CARTESIAN_POINT ( 'NONE',  ( -0.9842519685039365918, -0.6692913385826771977, 8.415575281601705876E-17 ) ) ;
#37763 = CARTESIAN_POINT ( 'NONE',  ( 2.516666435443586813, 2.742784459617114923, -0.5314960629921260393 ) ) ;
#37764 = CARTESIAN_POINT ( 'NONE',  ( -1.679790026246718693, 0.2306618581243847221, -0.2411417322834647770 ) ) ;
#37765 = CARTESIAN_POINT ( 'NONE',  ( 0.3740157480314966754, -0.4536011799217367080, 0.2665933059059888421 ) ) ;
#37766 = CARTESIAN_POINT ( 'NONE',  ( -1.646051170424378096, 0.000000000000000000, 0.3464511005275205946 ) ) ;
#37767 = CARTESIAN_POINT ( 'NONE',  ( -0.2867679344610364334, -0.2867679344610367109, 0.01377952755905502598 ) ) ;
#37768 = CARTESIAN_POINT ( 'NONE',  ( -0.1115485564304456306, 0.1771653543307087075, -0.09757992244046823083 ) ) ;
#37769 = CARTESIAN_POINT ( 'NONE',  ( -0.5380577427821514602, 0.05413385826771666132, 0.4176697321401328100 ) ) ;
#37770 = CARTESIAN_POINT ( 'NONE',  ( 1.541994750656168645, -0.6692913385826771977, 0.1292274648535927661 ) ) ;
#37771 = CARTESIAN_POINT ( 'NONE',  ( -0.4396325459317577122, -0.6692913385826773087, -0.1292274648535924053 ) ) ;
#37772 = ORIENTED_EDGE ( 'NONE', *, *, #19166, .T. ) ;
#37773 = CARTESIAN_POINT ( 'NONE',  ( -0.3996062992125986035, -7.340648628747425578E-17, -2.086614173228346303 ) ) ;
#37774 = LINE ( 'NONE', #31455, #56015 ) ;
#37775 = EDGE_LOOP ( 'NONE', ( #6196, #13015, #11078, #59096, #1634, #30188, #32492, #10222 ) ) ;
#37776 = CARTESIAN_POINT ( 'NONE',  ( 0.3996062992125984925, 0.1070741851644054637, -1.618766404199474929 ) ) ;
#37777 = CARTESIAN_POINT ( 'NONE',  ( -0.4986876640419939388, 0.2306618581243847221, -0.2411417322834647770 ) ) ;
#37778 = CARTESIAN_POINT ( 'NONE',  ( 1.509186351706037543, -0.4281496062992127816, -0.4176697321401328100 ) ) ;
#37779 = CARTESIAN_POINT ( 'NONE',  ( -1.030183727034119867, -0.08942795157528024563, -0.3641732283464568787 ) ) ;
#37780 = CARTESIAN_POINT ( 'NONE',  ( -1.364829396325458521, 0.2306618581243847221, -0.2411417322834647770 ) ) ;
#37781 = CARTESIAN_POINT ( 'NONE',  ( -0.4724409448818899238, 0.1265901696524986686, -0.8202099737532806412 ) ) ;
#37782 = CARTESIAN_POINT ( 'NONE',  ( 0.4847769261806181285, 1.968503937007873850, -0.4915354330708656128 ) ) ;
#37783 = CARTESIAN_POINT ( 'NONE',  ( -0.3917322834645671215, 0.1049643490035301469, -0.02493438320209968861 ) ) ;
#37784 = CARTESIAN_POINT ( 'NONE',  ( 1.135170603674541256, -0.6692913385826773087, -0.1292274648535924053 ) ) ;
#37785 = CARTESIAN_POINT ( 'NONE',  ( 1.220472440944881942, 0.8346805926620878280, -0.5309055118110238558 ) ) ;
#37786 = CARTESIAN_POINT ( 'NONE',  ( 0.2427821522309719648, -0.05778040916215522460, 0.4822834645669289988 ) ) ;
#37787 = CARTESIAN_POINT ( 'NONE',  ( -1.089238845144356427, -0.3690944881889765550, -0.3153832671262227771 ) ) ;
#37788 = CARTESIAN_POINT ( 'NONE',  ( -0.3215223097112853146, -0.3162353388693405765, 0.4822834645669290543 ) ) ;
#37789 = CARTESIAN_POINT ( 'NONE',  ( -0.1265901696524993347, 0.4724409448818895907, -2.603018372703412631 ) ) ;
#37790 = CARTESIAN_POINT ( 'NONE',  ( -0.9251968503937002541, 0.1660481256975885056, 0.3530559997133364547 ) ) ;
#37791 = CARTESIAN_POINT ( 'NONE',  ( 0.3949938075777409408, -0.1058382717557499186, -2.078083989501312345 ) ) ;
#37792 = CARTESIAN_POINT ( 'NONE',  ( 0.6955380577427828781, -0.004921259842519870586, -0.3153832671262229437 ) ) ;
#37793 = CARTESIAN_POINT ( 'NONE',  ( -0.3018372703412066094, -0.004921259842519576551, 0.3153832671262227771 ) ) ;
#37794 = CARTESIAN_POINT ( 'NONE',  ( 0.7611548556430454138, 0.1283753931104746893, -0.1820866141732285504 ) ) ;
#37795 = CARTESIAN_POINT ( 'NONE',  ( -1.430446194225721390, -0.4281496062992124485, 0.4176697321401328655 ) ) ;
#37796 = AXIS2_PLACEMENT_3D ( 'NONE', #65610, #7940, #40742 ) ;
#37797 = CARTESIAN_POINT ( 'NONE',  ( -3.197598486322605016, 2.742783266281798138, -0.5314960629921260393 ) ) ;
#37798 = CARTESIAN_POINT ( 'NONE',  ( 0.7283464566929143125, 0.07958543189024085140, 0.2665933059059887866 ) ) ;
#37799 = CARTESIAN_POINT ( 'NONE',  ( -0.9580052493438311334, 0.05413385826771626580, -0.4176697321401330321 ) ) ;
#37800 = CARTESIAN_POINT ( 'NONE',  ( 1.377952755905512472, -0.6692913385826771977, 8.415575281601705876E-17 ) ) ;
#37801 = CARTESIAN_POINT ( 'NONE',  ( -1.964414453380826986, 1.188885443925074004, 0.3231744412230012631 ) ) ;
#37802 = CARTESIAN_POINT ( 'NONE',  ( -0.08530183727034056085, -0.2845877964562159024, 0.3641732283464567677 ) ) ;
#37803 = CARTESIAN_POINT ( 'NONE',  ( 0.2017716535433070613, 0.2017716535433070613, -0.3937007874015748254 ) ) ;
#37804 = CARTESIAN_POINT ( 'NONE',  ( 0.5446194225721792126, -0.3162353388693405765, 0.4822834645669290543 ) ) ;
#37805 = CARTESIAN_POINT ( 'NONE',  ( 0.2199809220305531665, 0.1970133122064496867, 0.1374248322900813168 ) ) ;
#37806 = CARTESIAN_POINT ( 'NONE',  ( 1.358267716535433323, -0.4536011799217368745, -0.2665933059059886201 ) ) ;
#37807 = CARTESIAN_POINT ( 'NONE',  ( -1.227034120734907585, 0.2952755905511811885, 0.1292274648535926551 ) ) ;
#37808 = CARTESIAN_POINT ( 'NONE',  ( -0.4396325459317577122, -0.5511811023622048555, -0.09757992244046775898 ) ) ;
#37809 = CARTESIAN_POINT ( 'NONE',  ( 0.3503937007874015630, 0.3733313776025731778, -0.01968503937007957602 ) ) ;
#37810 = CARTESIAN_POINT ( 'NONE',  ( 0.4265091863517067039, -0.5511811023622048555, -0.09757992244046775898 ) ) ;
#37811 = AXIS2_PLACEMENT_3D ( 'NONE', #6676, #26869, #374 ) ;
#37812 = CARTESIAN_POINT ( 'NONE',  ( -0.9645669291338575535, -0.5400638737290844871, 0.3530559997133364547 ) ) ;
#37813 = CARTESIAN_POINT ( 'NONE',  ( -0.3083989501312330295, -0.3162353388693409650, -0.4822834645669289433 ) ) ;
#37814 = CARTESIAN_POINT ( 'NONE',  ( 0.3460692066303959202, -0.1998031496062991630, -0.8116797900262466836 ) ) ;
#37815 = CARTESIAN_POINT ( 'NONE',  ( -0.3917322834645669549, -0.1049643490035306603, -2.177821522309711266 ) ) ;
#37816 = CARTESIAN_POINT ( 'NONE',  ( 0.8202099737532813073, 0.1771653543307087630, 0.09757992244046791164 ) ) ;
#37817 = CARTESIAN_POINT ( 'NONE',  ( -0.4986876640419939388, 0.2306618581243847221, -0.2411417322834647770 ) ) ;
#37818 = CARTESIAN_POINT ( 'NONE',  ( -0.8333333333333323711, 0.2952755905511811885, 0.1292274648535926551 ) ) ;
#37819 = CARTESIAN_POINT ( 'NONE',  ( -0.8136482939632537770, 0.1283753931104746893, -0.1820866141732285504 ) ) ;
#37820 = CARTESIAN_POINT ( 'NONE',  ( -0.6272530615646277896, 0.009110075358399026199, -0.2965444001473090951 ) ) ;
#37821 = CARTESIAN_POINT ( 'NONE',  ( -0.09186351706036663400, -0.4281496062992124485, 0.4176697321401328655 ) ) ;
#37822 = EDGE_CURVE ( 'NONE', #82322, #47058, #44139, .T. ) ;
#37823 = CARTESIAN_POINT ( 'NONE',  ( -1.463254593175852492, -0.5511811023622048555, -0.09757992244046775898 ) ) ;
#37824 = CARTESIAN_POINT ( 'NONE',  ( 1.102362204724410155, -0.1870078740157479769, 0.4822834645669291653 ) ) ;
#37825 = DIRECTION ( 'NONE',  ( -3.096699300667737957E-16, 1.000000000000000000, -0.000000000000000000 ) ) ;
#37826 = CARTESIAN_POINT ( 'NONE',  ( -0.3392501089628019995, 0.1958661417322831999, -1.912748974574490113 ) ) ;
#37827 = ORIENTED_EDGE ( 'NONE', *, *, #49490, .F. ) ;
#37828 = EDGE_CURVE ( 'NONE', #41807, #57855, #31104, .T. ) ;
#37829 = LINE ( 'NONE', #57170, #44504 ) ;
#37830 = CARTESIAN_POINT ( 'NONE',  ( -1.253280839895012377, -0.05778040916215522460, 0.4822834645669289988 ) ) ;
#37831 = CARTESIAN_POINT ( 'NONE',  ( -0.7480314960629914633, 0.2952755905511811885, 0.000000000000000000 ) ) ;
#37832 = CARTESIAN_POINT ( 'NONE',  ( 1.476377952755906220, 0.1660481256975883668, -0.3530559997133364547 ) ) ;
#37833 = CARTESIAN_POINT ( 'NONE',  ( -0.3917322834645669549, -0.1049643490035306603, -2.020341207349081181 ) ) ;
#37834 = DIRECTION ( 'NONE',  ( -1.000000000000000000, -1.734723475976808080E-16, -3.491481338843132961E-15 ) ) ;
#37835 = CARTESIAN_POINT ( 'NONE',  ( 0.8202099737532814183, -0.6692913385826773087, -0.1292274648535924053 ) ) ;
#37836 = CARTESIAN_POINT ( 'NONE',  ( 0.07874015748031558404, -0.1870078740157479769, 0.4822834645669291653 ) ) ;
#37837 = CARTESIAN_POINT ( 'NONE',  ( -1.157146581871515012E-16, 0.4724409448818898682, -0.4724409448818898127 ) ) ;
#37838 = CARTESIAN_POINT ( 'NONE',  ( -0.6627296587926501115, 0.2952755905511810219, -0.1292274648535930437 ) ) ;
#37839 = CARTESIAN_POINT ( 'NONE',  ( 1.043307086614173818, -0.4536011799217368745, -0.2665933059059886201 ) ) ;
#37840 = CARTESIAN_POINT ( 'NONE',  ( 0.1070741851644053527, 0.3996062992125986590, -0.7808398950131233418 ) ) ;
#37841 = ORIENTED_EDGE ( 'NONE', *, *, #511, .F. ) ;
#37842 = CARTESIAN_POINT ( 'NONE',  ( -0.3392501089628017219, -0.1958661417322836718, -2.721784776902886893 ) ) ;
#37843 = ORIENTED_EDGE ( 'NONE', *, *, #65705, .F. ) ;
#37844 = CARTESIAN_POINT ( 'NONE',  ( 0.1968503937007881344, 0.2952755905511811885, 0.000000000000000000 ) ) ;
#37845 = CARTESIAN_POINT ( 'NONE',  ( -0.8727034120734901146, -0.05778040916215560624, -0.4822834645669293319 ) ) ;
#37846 = CARTESIAN_POINT ( 'NONE',  ( -1.640419947506561060, 0.05413385826771666132, 0.4176697321401328100 ) ) ;
#37847 = CARTESIAN_POINT ( 'NONE',  ( 0.7742782152230979209, 0.05413385826771626580, -0.4176697321401330321 ) ) ;
#37848 = CARTESIAN_POINT ( 'NONE',  ( 1.443569553805774897, -0.6046776061558809534, -0.2411417322834644161 ) ) ;
#37849 = CARTESIAN_POINT ( 'NONE',  ( 1.515748031496063186, -0.5400638737290845981, -0.3530559997133363437 ) ) ;
#37850 = CARTESIAN_POINT ( 'NONE',  ( -0.1837270341207340729, 0.2306618581243847221, -0.2411417322834647770 ) ) ;
#37851 = CIRCLE ( 'NONE', #23080, 3.582677165354330562 ) ;
#37852 = CARTESIAN_POINT ( 'NONE',  ( -1.456692913385826182, 0.2952755905511811885, 0.000000000000000000 ) ) ;
#37853 = CARTESIAN_POINT ( 'NONE',  ( 1.614173228346457378, 0.2952755905511811885, 0.000000000000000000 ) ) ;
#37854 = EDGE_CURVE ( 'NONE', #75665, #40053, #22125, .T. ) ;
#37855 = CARTESIAN_POINT ( 'NONE',  ( 1.653543307086614789, -0.1870078740157479769, 0.4822834645669291653 ) ) ;
#37856 = CARTESIAN_POINT ( 'NONE',  ( 0.1958661417322836440, -0.3392501089628017219, -0.08398950131233590133 ) ) ;
#37857 = CARTESIAN_POINT ( 'NONE',  ( 0.9776902887139113929, -0.5511811023622048555, -0.09757992244046775898 ) ) ;
#37858 = ORIENTED_EDGE ( 'NONE', *, *, #60347, .F. ) ;
#37859 = CARTESIAN_POINT ( 'NONE',  ( -0.3949938075777409963, -7.255918531996591613E-17, -0.03937007874015754222 ) ) ;
#37860 = EDGE_LOOP ( 'NONE', ( #30288, #19331, #70138, #28986, #65300, #57699 ) ) ;
#37861 = CARTESIAN_POINT ( 'NONE',  ( -0.2165354330708654795, -0.4536011799217368745, -0.2665933059059886201 ) ) ;
#37862 = DIRECTION ( 'NONE',  ( -1.000000000000000000, 0.000000000000000000, 0.000000000000000000 ) ) ;
#37863 = CARTESIAN_POINT ( 'NONE',  ( 5.463695987328526437E-16, -0.1870078740157479769, 0.4822834645669291653 ) ) ;
#37864 = CARTESIAN_POINT ( 'NONE',  ( 0.4068241469816279987, -0.4281496062992127816, -0.4176697321401328100 ) ) ;
#37865 = CARTESIAN_POINT ( 'NONE',  ( -0.6167979002624665030, 0.05413385826771666132, 0.4176697321401328100 ) ) ;
#37866 = EDGE_CURVE ( 'NONE', #27190, #79281, #7613, .T. ) ;
#37867 = CARTESIAN_POINT ( 'NONE',  ( 0.1958661417322834775, 0.3392501089628018884, -1.873378895834332258 ) ) ;
#37868 = CARTESIAN_POINT ( 'NONE',  ( -1.017060367454067249, -0.05778040916215522460, 0.4822834645669289988 ) ) ;
#37869 = CARTESIAN_POINT ( 'NONE',  ( 0.1958661417322836440, -0.3392501089628017219, -2.696194225721784576 ) ) ;
#37870 = CARTESIAN_POINT ( 'NONE',  ( 1.332020997375328974, -0.08942795157528024563, -0.3641732283464568787 ) ) ;
#37871 = CARTESIAN_POINT ( 'NONE',  ( -1.266404199475064773, -0.05778040916215560624, -0.4822834645669293319 ) ) ;
#37872 = CARTESIAN_POINT ( 'NONE',  ( 0.9120734908136490793, 0.2952755905511810774, -0.1292274648535930714 ) ) ;
#37873 = CARTESIAN_POINT ( 'NONE',  ( 1.095800524934383846, -0.05778040916215560624, -0.4822834645669293319 ) ) ;
#37874 = CARTESIAN_POINT ( 'NONE',  ( -0.3996062992125987146, 0.1070741851644051862, -0.6627296587926508886 ) ) ;
#37875 = CARTESIAN_POINT ( 'NONE',  ( -1.161417322834644716, -0.5400638737290845981, -0.3530559997133363437 ) ) ;
#37876 = CARTESIAN_POINT ( 'NONE',  ( -0.2925321140481930149, -0.2925321140481933480, -0.2933070866141732069 ) ) ;
#37877 = CARTESIAN_POINT ( 'NONE',  ( -0.1998031496062991630, -0.3460692066303959202, 0.01509186351706034469 ) ) ;
#37878 = CARTESIAN_POINT ( 'NONE',  ( -0.2755905511811018171, 0.2952755905511811885, 0.000000000000000000 ) ) ;
#37879 = CARTESIAN_POINT ( 'NONE',  ( -0.3460692066303958092, -0.1998031496062994683, -2.887139107611548461 ) ) ;
#37880 = CARTESIAN_POINT ( 'NONE',  ( -0.1958661417322836718, 0.3392501089628017219, -1.515091863517060489 ) ) ;
#37881 = CARTESIAN_POINT ( 'NONE',  ( 1.312335958005249825, 0.2306618581243847221, -0.2411417322834647770 ) ) ;
#37882 = CARTESIAN_POINT ( 'NONE',  ( 1.292650918635171564, -0.6692913385826773087, -0.1292274648535924053 ) ) ;
#37883 = CARTESIAN_POINT ( 'NONE',  ( 0.02624671916010564918, -0.5023911411419708095, -0.1820866141732282451 ) ) ;
#37884 = CARTESIAN_POINT ( 'NONE',  ( 0.9251968503937015864, -0.5400638737290844871, 0.3530559997133364547 ) ) ;
#37885 = CARTESIAN_POINT ( 'NONE',  ( -0.4091458600556402980, -0.2362204724409451284, -1.704068241469816058 ) ) ;
#37886 = CARTESIAN_POINT ( 'NONE',  ( 0.4002624671916016896, -0.08942795157527998196, 0.3641732283464567121 ) ) ;
#37887 = CARTESIAN_POINT ( 'NONE',  ( 0.2755905511811031494, -0.6692913385826771977, 8.415575281601705876E-17 ) ) ;
#37888 = CARTESIAN_POINT ( 'NONE',  ( 0.1058382717557499880, 0.3949938075777409408, -0.8576115485564304031 ) ) ;
#37889 = CARTESIAN_POINT ( 'NONE',  ( -0.9842519685039365918, -0.6692913385826771977, 8.415575281601705876E-17 ) ) ;
#37890 = CARTESIAN_POINT ( 'NONE',  ( 0.9842519685039375910, 0.1771653543307087630, 0.000000000000000000 ) ) ;
#37891 = CARTESIAN_POINT ( 'NONE',  ( 0.3812812444996376282, 2.409604939980833412E-17, -0.3464511005275205946 ) ) ;
#37892 = CARTESIAN_POINT ( 'NONE',  ( -0.4133858267716528645, 0.1660481256975883668, -0.3530559997133364547 ) ) ;
#37893 = CARTESIAN_POINT ( 'NONE',  ( 0.1312335958005257930, 0.1283753931104746893, -0.1820866141732285504 ) ) ;
#37894 = CARTESIAN_POINT ( 'NONE',  ( -2.873110008490984413, 1.063968899401426693, 0.03484477857464209766 ) ) ;
#37895 = CARTESIAN_POINT ( 'NONE',  ( -0.3018372703412066094, 0.05413385826771666132, 0.4176697321401328100 ) ) ;
#37896 = CARTESIAN_POINT ( 'NONE',  ( 0.2690288713910767848, -0.5511811023622048555, -0.09757992244046775898 ) ) ;
#37897 = CARTESIAN_POINT ( 'NONE',  ( 0.2925321140481932369, -0.2925321140481931814, -1.907480314960629642 ) ) ;
#37898 = CARTESIAN_POINT ( 'NONE',  ( 0.1640419947506569498, -0.3162353388693409650, -0.4822834645669289433 ) ) ;
#37899 = CARTESIAN_POINT ( 'NONE',  ( 1.148293963254593875, -0.5511811023622046335, 0.09757992244046803654 ) ) ;
#37900 = CARTESIAN_POINT ( 'NONE',  ( 0.3822046412494098377, 1.809133623825372073E-16, -0.3791483426435173776 ) ) ;
#37901 = CARTESIAN_POINT ( 'NONE',  ( -0.2559055118110230564, 0.07958543189024071263, -0.2665933059059888421 ) ) ;
#37902 = CARTESIAN_POINT ( 'NONE',  ( -0.7480314960629914633, 0.1771653543307087630, 0.000000000000000000 ) ) ;
#37903 = CARTESIAN_POINT ( 'NONE',  ( -0.1640419947506553400, -0.05778040916215560624, -0.4822834645669293319 ) ) ;
#37904 = CARTESIAN_POINT ( 'NONE',  ( -0.08530183727034056085, -0.05778040916215560624, -0.4822834645669293319 ) ) ;
#37905 = CARTESIAN_POINT ( 'NONE',  ( 1.135170603674541256, -0.5511811023622048555, -0.09757992244046775898 ) ) ;
#37906 = CARTESIAN_POINT ( 'NONE',  ( -1.646981627296586703, -0.2845877964562161244, -0.3641732283464567121 ) ) ;
#37907 = CARTESIAN_POINT ( 'NONE',  ( -1.706036745406823485, 0.2306618581243848609, 0.2411417322834645549 ) ) ;
#37908 = VECTOR ( 'NONE', #77916, 39.37007874015748143 ) ;
#37909 = CARTESIAN_POINT ( 'NONE',  ( 0.6299212598425204535, -0.1870078740157480879, -0.4822834645669291653 ) ) ;
#37910 = CARTESIAN_POINT ( 'NONE',  ( -0.4359958488159792478, 1.724409448818897683, 2.094141031014984389 ) ) ;
#37911 = CARTESIAN_POINT ( 'NONE',  ( -0.1640419947506555343, -0.3162353388693405765, 0.4822834645669290543 ) ) ;
#37912 = CARTESIAN_POINT ( 'NONE',  ( 0.2867679344610365999, 0.2867679344610365999, -1.009842519685039353 ) ) ;
#37913 = CARTESIAN_POINT ( 'NONE',  ( 0.9580052493438327987, -0.4281496062992127816, -0.4176697321401328100 ) ) ;
#37914 = CARTESIAN_POINT ( 'NONE',  ( 0.6692913385826778638, -0.6692913385826771977, 8.415575281601705876E-17 ) ) ;
#37915 = CARTESIAN_POINT ( 'NONE',  ( 0.000000000000000000, 2.755905511811024056, 0.000000000000000000 ) ) ;
#37916 = CARTESIAN_POINT ( 'NONE',  ( 0.4461942257217856311, 0.1283753931104746893, -0.1820866141732285504 ) ) ;
#37917 = CARTESIAN_POINT ( 'NONE',  ( 1.089238845144357759, 0.05413385826771626580, -0.4176697321401330321 ) ) ;
#37918 = ADVANCED_FACE ( 'NONE', ( #18496 ), #31522, .F. ) ;
#37919 = CARTESIAN_POINT ( 'NONE',  ( -0.1574803149606292529, -0.1870078740157479769, 0.3641732283464567677 ) ) ;
#37920 = CARTESIAN_POINT ( 'NONE',  ( -0.2230971128608915943, 0.05413385826771666132, 0.4176697321401328100 ) ) ;
#37921 = CARTESIAN_POINT ( 'NONE',  ( 0.8267716535433077274, 0.2952755905511811885, 0.000000000000000000 ) ) ;
#37922 = CARTESIAN_POINT ( 'NONE',  ( 0.4593175853018379162, -0.4281496062992124485, 0.4176697321401328655 ) ) ;
#37923 = CARTESIAN_POINT ( 'NONE',  ( -0.7283464566929126471, -0.5400638737290844871, 0.3530559997133364547 ) ) ;
#37924 = CARTESIAN_POINT ( 'NONE',  ( -0.8530183727034112984, -0.3690944881889765550, -0.3153832671262227771 ) ) ;
#37925 = CARTESIAN_POINT ( 'NONE',  ( 0.4855643044619428750, 0.05413385826771666132, 0.4176697321401328100 ) ) ;
#37926 = CARTESIAN_POINT ( 'NONE',  ( -1.397637795275589623, 0.1660481256975885056, 0.3530559997133364547 ) ) ;
#37927 = CARTESIAN_POINT ( 'NONE',  ( -0.5380577427821514602, 0.05413385826771666132, 0.4176697321401328100 ) ) ;
#37928 = CARTESIAN_POINT ( 'NONE',  ( 1.168682819302787168, 2.409604939980833412E-17, -0.3464511005275205946 ) ) ;
#37930 = CARTESIAN_POINT ( 'NONE',  ( 1.463254593175853824, 0.2952755905511810774, -0.1292274648535930714 ) ) ;
#37929 = LINE ( 'NONE', #43402, #54015 ) ;
#37931 = CARTESIAN_POINT ( 'NONE',  ( 1.312335958005250269, -0.6046776061558807314, 0.2411417322834647770 ) ) ;
#37932 = CARTESIAN_POINT ( 'NONE',  ( 0.3917322834645670104, -0.1049643490035303273, -1.993438320209973913 ) ) ;
#37933 = CARTESIAN_POINT ( 'NONE',  ( -1.522309711286088607, -0.6046776061558807314, 0.2411417322834647770 ) ) ;
#37934 = CARTESIAN_POINT ( 'NONE',  ( -0.7677165354330699465, 0.1660481256975885056, 0.3530559997133364547 ) ) ;
#37935 = CARTESIAN_POINT ( 'NONE',  ( -0.4091458600556405756, 0.2362204724409446288, -0.1837270341207349056 ) ) ;
#37936 = CARTESIAN_POINT ( 'NONE',  ( 0.1974969037888706369, -0.3420746716998659953, -2.769028871391075786 ) ) ;
#37937 = ORIENTED_EDGE ( 'NONE', *, *, #45564, .F. ) ;
#37938 = CARTESIAN_POINT ( 'NONE',  ( -0.1640419947506553400, -0.08942795157528024563, -0.3641732283464568787 ) ) ;
#37939 = CARTESIAN_POINT ( 'NONE',  ( 0.2867679344610365999, 0.2867679344610365999, -1.547244094488189115 ) ) ;
#37940 = CARTESIAN_POINT ( 'NONE',  ( 0.8595800524934390507, -0.05778040916215560624, -0.4822834645669293319 ) ) ;
#37941 = CARTESIAN_POINT ( 'NONE',  ( -0.4724409448818895907, -0.1265901696524993070, -2.723097112860892288 ) ) ;
#37942 = DIRECTION ( 'NONE',  ( 1.000000000000000000, -0.000000000000000000, -0.000000000000000000 ) ) ;
#37943 = CARTESIAN_POINT ( 'NONE',  ( -0.6430446194225712953, -0.004921259842519870586, -0.3153832671262229437 ) ) ;
#37944 = CARTESIAN_POINT ( 'NONE',  ( 1.141392835773559211, 0.000000000000000000, 1.456353465694822491 ) ) ;
#37945 = CARTESIAN_POINT ( 'NONE',  ( 1.272965879265092637, -0.4281496062992127816, -0.4176697321401328100 ) ) ;
#37946 = CARTESIAN_POINT ( 'NONE',  ( 0.7677165354330716118, -0.4536011799217367080, 0.2665933059059888421 ) ) ;
#37947 = CARTESIAN_POINT ( 'NONE',  ( 0.2034120734908144990, -0.6692913385826771977, 0.1292274648535927661 ) ) ;
#37948 = CARTESIAN_POINT ( 'NONE',  ( 0.1049643490035303689, 0.3917322834645668994, -0.5459124427483446063 ) ) ;
#37949 = CARTESIAN_POINT ( 'NONE',  ( -0.4396325459317577122, -0.6692913385826773087, -0.1292274648535924053 ) ) ;
#37950 = CARTESIAN_POINT ( 'NONE',  ( -1.430446194225721390, -0.3690944881889763329, 0.3153832671262228327 ) ) ;
#37951 = CARTESIAN_POINT ( 'NONE',  ( -0.3215223097112853146, -0.3162353388693405765, 0.4822834645669290543 ) ) ;
#37952 = CARTESIAN_POINT ( 'NONE',  ( 1.594488188976378673, -0.5400638737290845981, -0.3530559997133363437 ) ) ;
#37953 = CARTESIAN_POINT ( 'NONE',  ( 0.5314960629921395840, 2.755905511811024056, -3.900966923095588346 ) ) ;
#37954 = EDGE_LOOP ( 'NONE', ( #21092, #59381, #64170, #65004, #42844, #72213, #78059, #6086, #29289, #20507, #50458, #12117, #75667, #48304, #25513, #75254, #73491, #33064, #54216, #7091, #46954, #47506, #14170, #55044, #42906, #27945, #21914, #15548, #77827, #63222, #397, #47347, #22478, #59192, #81681, #77101 ) ) ;
#37955 = CARTESIAN_POINT ( 'NONE',  ( -0.3392501089628019995, 0.1958661417322831999, -2.070229289535120198 ) ) ;
#37956 = CARTESIAN_POINT ( 'NONE',  ( 0.3543307086614181922, -0.6692913385826771977, 8.415575281601705876E-17 ) ) ;
#37957 = ORIENTED_EDGE ( 'NONE', *, *, #24432, .F. ) ;
#37958 = CARTESIAN_POINT ( 'NONE',  ( -0.8333333333333323711, -0.6692913385826773087, -0.1292274648535924053 ) ) ;
#37959 = CARTESIAN_POINT ( 'NONE',  ( -1.482939632545930975, 0.05413385826771666132, 0.4176697321401328100 ) ) ;
#37960 = CARTESIAN_POINT ( 'NONE',  ( 0.7480314960629927956, -0.6692913385826771977, 8.415575281601705876E-17 ) ) ;
#37961 = AXIS2_PLACEMENT_3D ( 'NONE', #52472, #78180, #16698 ) ;
#37962 = CARTESIAN_POINT ( 'NONE',  ( 0.07874015748031558404, -0.1870078740157479769, 0.4822834645669291653 ) ) ;
#37963 = CARTESIAN_POINT ( 'NONE',  ( -0.3917322834645671215, 0.1049643490035301469, -1.377296587926508664 ) ) ;
#37964 = CARTESIAN_POINT ( 'NONE',  ( -0.7480314960629914633, 0.2952755905511811885, 0.000000000000000000 ) ) ;
#37965 = CARTESIAN_POINT ( 'NONE',  ( -0.06561679790026180015, 0.05413385826771666132, 0.4176697321401328100 ) ) ;
#37966 = CARTESIAN_POINT ( 'NONE',  ( -1.030183727034119867, -0.3162353388693405765, 0.4822834645669290543 ) ) ;
#37967 = CARTESIAN_POINT ( 'NONE',  ( -0.06561679790026180015, -0.004921259842519576551, 0.3153832671262227771 ) ) ;
#37968 = CARTESIAN_POINT ( 'NONE',  ( 0.4724409448818898682, 2.892866454678787531E-17, -0.03740157480314962313 ) ) ;
#37969 = CARTESIAN_POINT ( 'NONE',  ( 0.1049868766404206816, -0.6046776061558809534, -0.2411417322834644161 ) ) ;
#37970 = AXIS2_PLACEMENT_3D ( 'NONE', #55763, #37249, #50275 ) ;
#37971 = CARTESIAN_POINT ( 'NONE',  ( 0.3372635250547070807, -0.3676148930005934123, -0.006554863637384342537 ) ) ;
#37972 = CARTESIAN_POINT ( 'NONE',  ( 1.102362204724410155, -0.1870078740157479769, 0.4822834645669291653 ) ) ;
#37973 = CARTESIAN_POINT ( 'NONE',  ( -0.1958661417322834220, -0.3392501089628018884, -2.734908136482939511 ) ) ;
#37974 = VERTEX_POINT ( 'NONE', #26874 ) ;
#37975 = ORIENTED_EDGE ( 'NONE', *, *, #40988, .T. ) ;
#37976 = CARTESIAN_POINT ( 'NONE',  ( 0.2624671916010504757, 0.2306618581243848609, 0.2411417322834645549 ) ) ;
#37977 = CARTESIAN_POINT ( 'NONE',  ( 0.2952755905511816326, -0.4536011799217367080, 0.2665933059059888421 ) ) ;
#37979 = CARTESIAN_POINT ( 'NONE',  ( 0.4359958488159307310, 1.724409448818897905, 3.937007874015793885 ) ) ;
#37978 = CARTESIAN_POINT ( 'NONE',  ( 1.430446194225722500, -0.3690944881889765550, -0.3153832671262227771 ) ) ;
#37980 = CARTESIAN_POINT ( 'NONE',  ( -0.1958661417322836718, 0.3392501089628017219, -1.042650918635170676 ) ) ;
#37981 = CARTESIAN_POINT ( 'NONE',  ( 0.1265901696524990294, -0.4724409448818896462, -0.3195538057742782212 ) ) ;
#37982 = CARTESIAN_POINT ( 'NONE',  ( 1.502624671916010790, -0.08942795157527998196, 0.3641732283464567121 ) ) ;
#37983 = CARTESIAN_POINT ( 'NONE',  ( -1.640419947506561060, 0.05413385826771666132, 0.4176697321401328100 ) ) ;
#37984 = CARTESIAN_POINT ( 'NONE',  ( 0.3460692066303959202, -0.1998031496062991630, -2.858923884514435798 ) ) ;
#37985 = CARTESIAN_POINT ( 'NONE',  ( 0.5183727034120741983, 0.2952755905511810774, -0.1292274648535930714 ) ) ;
#37986 = CARTESIAN_POINT ( 'NONE',  ( -1.141732283464566011, 0.2952755905511811885, 0.000000000000000000 ) ) ;
#37987 = CARTESIAN_POINT ( 'NONE',  ( -1.115485564304461219, -0.4281496062992124485, 0.4176697321401328655 ) ) ;
#37988 = CARTESIAN_POINT ( 'NONE',  ( 0.3477690288713918276, 0.2952755905511811885, 0.1292274648535926551 ) ) ;
#37989 = CARTESIAN_POINT ( 'NONE',  ( 0.8005249343832027131, 0.05413385826771666132, 0.4176697321401328100 ) ) ;
#37990 = CARTESIAN_POINT ( 'NONE',  ( 1.338582677165355062, -0.1870078740157479769, 0.3641732283464567677 ) ) ;
#37991 = CARTESIAN_POINT ( 'NONE',  ( 1.010498687664042716, -0.3690944881889763329, 0.3153832671262228327 ) ) ;
#37992 = CARTESIAN_POINT ( 'NONE',  ( -0.9251968503937002541, -0.5400638737290845981, -0.3530559997133363437 ) ) ;
#37993 = CARTESIAN_POINT ( 'NONE',  ( 4.893765752498283308E-17, -0.3996062992125985480, -0.4704724409448819422 ) ) ;
#37994 = CARTESIAN_POINT ( 'NONE',  ( -1.574803149606298192, -0.1870078740157480601, -0.3641732283464567677 ) ) ;
#37995 = CARTESIAN_POINT ( 'NONE',  ( 0.1958661417322836440, -0.3392501089628017219, -0.08398950131233591521 ) ) ;
#37997 = CARTESIAN_POINT ( 'NONE',  ( -0.4741706889230301036, 1.520077057622760464, 2.169554232157526297 ) ) ;
#37996 = CARTESIAN_POINT ( 'NONE',  ( 0.9317585301837276734, 0.05413385826771626580, -0.4176697321401330321 ) ) ;
#37998 = CARTESIAN_POINT ( 'NONE',  ( -1.515748031496062076, 0.07958543189024071263, -0.2665933059059888421 ) ) ;
#37999 = CARTESIAN_POINT ( 'NONE',  ( -0.05905511811023545637, 0.1660481256975885056, 0.3530559997133364547 ) ) ;
#38000 = CARTESIAN_POINT ( 'NONE',  ( 0.9908136482939640111, 0.1771653543307087075, -0.09757992244046823083 ) ) ;
#38001 = CARTESIAN_POINT ( 'NONE',  ( -1.679790026246718693, 0.1283753931104746893, -0.1820866141732285504 ) ) ;
#38002 = CARTESIAN_POINT ( 'NONE',  ( 1.141732283464567788, -0.6692913385826771977, 8.415575281601705876E-17 ) ) ;
#38003 = CARTESIAN_POINT ( 'NONE',  ( -0.4855643044619415427, 0.05413385826771626580, -0.4176697321401330321 ) ) ;
#38004 = CARTESIAN_POINT ( 'NONE',  ( -0.6496062992125976043, -0.4536011799217367080, 0.2665933059059888421 ) ) ;
#38005 = CARTESIAN_POINT ( 'NONE',  ( -0.6496062992125976043, -0.5400638737290844871, 0.3530559997133364547 ) ) ;
#38006 = CARTESIAN_POINT ( 'NONE',  ( 1.640419947506562393, -0.4281496062992124485, 0.4176697321401328655 ) ) ;
#38007 = CARTESIAN_POINT ( 'NONE',  ( -1.305774278215222184, -0.6692913385826773087, -0.1292274648535924053 ) ) ;
#38008 = CARTESIAN_POINT ( 'NONE',  ( 1.574803149606299746, -0.1870078740157480879, -0.4822834645669291653 ) ) ;
#38009 = CARTESIAN_POINT ( 'NONE',  ( 0.2867679344610366554, 0.2867679344610366554, -0.9219353262805269900 ) ) ;
#38010 = CARTESIAN_POINT ( 'NONE',  ( -1.430446194225720724, -0.004921259842519870586, -0.3153832671262229437 ) ) ;
#38011 = EDGE_CURVE ( 'NONE', #10560, #14996, #45273, .T. ) ;
#38012 = CARTESIAN_POINT ( 'NONE',  ( 2.611722799339308843, 1.697109554835841916, 0.4469779880792065785 ) ) ;
#38013 = B_SPLINE_CURVE_WITH_KNOTS ( 'NONE', 3,
 ( #1663, #45415, #13454, #39964, #33644, #46677, #19341 ),
 .UNSPECIFIED., .F., .F.,
 ( 4, 3, 4 ),
 ( 1.388456241783856658E-17, 0.001246230184515585400, 0.002492489877932651567 ),
 .UNSPECIFIED. ) ;
#38014 = CARTESIAN_POINT ( 'NONE',  ( 1.148293963254593653, 0.2952755905511810774, -0.1292274648535930714 ) ) ;
#38015 = CARTESIAN_POINT ( 'NONE',  ( 0.4091458600556404646, -0.2362204724409448231, -2.386482939632545985 ) ) ;
#38016 = CARTESIAN_POINT ( 'NONE',  ( -1.712598425196849572, 0.1660481256975885056, 0.3530559997133364547 ) ) ;
#38017 = CARTESIAN_POINT ( 'NONE',  ( -1.640419947506561060, -0.004921259842519576551, 0.3153832671262227771 ) ) ;
#38018 = CARTESIAN_POINT ( 'NONE',  ( -0.8464566929133852113, -0.4536011799217368745, -0.2665933059059886201 ) ) ;
#38019 = DIRECTION ( 'NONE',  ( -0.000000000000000000, 1.000000000000000000, -0.000000000000000000 ) ) ;
#38020 = CARTESIAN_POINT ( 'NONE',  ( -0.4790026246719152336, -0.05778040916215560624, -0.4822834645669293319 ) ) ;
#38021 = CARTESIAN_POINT ( 'NONE',  ( -0.1771653543307080136, 0.07958543189024071263, -0.2665933059059888421 ) ) ;
#38022 = CARTESIAN_POINT ( 'NONE',  ( -1.489501312335957062, -0.2845877964562161244, -0.3641732283464567121 ) ) ;
#38023 = CARTESIAN_POINT ( 'NONE',  ( 1.141732283464567566, 0.1771653543307087630, 0.000000000000000000 ) ) ;
#38024 = CIRCLE ( 'NONE', #73008, 0.5118110236220472231 ) ;
#38025 = CARTESIAN_POINT ( 'NONE',  ( 0.9776902887139113929, -0.6692913385826773087, -0.1292274648535924053 ) ) ;
#38026 = CARTESIAN_POINT ( 'NONE',  ( 1.587926509186352142, 0.05413385826771666132, 0.4176697321401328100 ) ) ;
#38027 = CARTESIAN_POINT ( 'NONE',  ( 0.1115485564304470323, 0.1771653543307087630, 0.09757992244046791164 ) ) ;
#38028 = CARTESIAN_POINT ( 'NONE',  ( 0.5708661417322842269, 0.1660481256975885056, 0.3530559997133364547 ) ) ;
#38029 = CARTESIAN_POINT ( 'NONE',  ( 0.4855643044619428750, -0.004921259842519576551, 0.3153832671262227771 ) ) ;
#38030 = CARTESIAN_POINT ( 'NONE',  ( 1.607611548556431069, 0.2952755905511811885, 0.1292274648535926551 ) ) ;
#38031 = CARTESIAN_POINT ( 'NONE',  ( -1.246719160104985846, -0.4281496062992127816, -0.4176697321401328100 ) ) ;
#38032 = CARTESIAN_POINT ( 'NONE',  ( -0.3280839895013117347, -0.4281496062992124485, 0.4176697321401328655 ) ) ;
#38033 = CARTESIAN_POINT ( 'NONE',  ( -0.1998031496062991907, -0.3460692066303959757, -0.2230971128608923992 ) ) ;
#38034 = CARTESIAN_POINT ( 'NONE',  ( -0.3460692066303960313, 0.1998031496062989965, -2.465223097112860806 ) ) ;
#38035 = CARTESIAN_POINT ( 'NONE',  ( 0.2952755905511816326, -0.5400638737290844871, 0.3530559997133364547 ) ) ;
#38036 = CARTESIAN_POINT ( 'NONE',  ( 1.286089238845145033, 0.1283753931104748280, 0.1820866141732283561 ) ) ;
#38037 = CARTESIAN_POINT ( 'NONE',  ( -0.3871391076115476282, -0.05778040916215522460, 0.4822834645669289988 ) ) ;
#38038 = CARTESIAN_POINT ( 'NONE',  ( 0.5446194225721792126, -0.05778040916215560624, -0.4822834645669293319 ) ) ;
#38039 = CARTESIAN_POINT ( 'NONE',  ( 0.3996062992125986035, 2.446882876249141962E-17, -2.165354330708661568 ) ) ;
#38040 = CARTESIAN_POINT ( 'NONE',  ( -0.3949938075777409963, -7.255918531996591613E-17, -1.456692913385826627 ) ) ;
#38041 = CARTESIAN_POINT ( 'NONE',  ( -0.1070741851644056997, 0.3996062992125986035, -2.683727034120735322 ) ) ;
#38042 = CARTESIAN_POINT ( 'NONE',  ( -0.4724409448818899238, 0.1265901696524986964, -2.552493438320209140 ) ) ;
#38043 = CARTESIAN_POINT ( 'NONE',  ( 0.2867679344610366554, 0.2867679344610366554, -0.4448818897637794589 ) ) ;
#38044 = CARTESIAN_POINT ( 'NONE',  ( -0.3477690288713905509, -0.5511811023622046335, 0.09757992244046803654 ) ) ;
#38045 = CARTESIAN_POINT ( 'NONE',  ( -1.227034120734907585, 0.2952755905511811885, 0.1292274648535926551 ) ) ;
#38046 = CARTESIAN_POINT ( 'NONE',  ( 0.2891555358219910499, 0.2891555358219910499, -2.576771653543307838 ) ) ;
#38047 = CARTESIAN_POINT ( 'NONE',  ( 0.7349081364829403995, 0.2306618581243848609, 0.2411417322834645549 ) ) ;
#38048 = CARTESIAN_POINT ( 'NONE',  ( 1.227034120734908917, -0.6692913385826771977, 0.1292274648535927661 ) ) ;
#38049 = CARTESIAN_POINT ( 'NONE',  ( 0.8858267716535438430, -0.5400638737290845981, -0.3530559997133363437 ) ) ;
#38050 = CARTESIAN_POINT ( 'NONE',  ( -0.6179882174207321777, -1.177125479915915794E-15, 0.3627985898453519598 ) ) ;
#38051 = CARTESIAN_POINT ( 'NONE',  ( 0.3460692066303959202, 0.1998031496062993295, -2.335958005249343827 ) ) ;
#38052 = CARTESIAN_POINT ( 'NONE',  ( 0.000000000000000000, 0.000000000000000000, 0.000000000000000000 ) ) ;
#38053 = CARTESIAN_POINT ( 'NONE',  ( 0.3937007874015754361, -0.1870078740157480879, -0.4822834645669291653 ) ) ;
#38054 = CARTESIAN_POINT ( 'NONE',  ( 0.7545931758530188826, -0.6692913385826771977, 0.1292274648535927661 ) ) ;
#38055 = CARTESIAN_POINT ( 'NONE',  ( 0.6824146981627303710, 0.1283753931104746893, -0.1820866141732285504 ) ) ;
#38056 = CARTESIAN_POINT ( 'NONE',  ( 1.207349081364829990, 0.2306618581243848609, 0.2411417322834645549 ) ) ;
#38057 = CARTESIAN_POINT ( 'NONE',  ( -9.594673741351313045E-17, 0.3917322834645670104, -0.2421259842519686289 ) ) ;
#38058 = CARTESIAN_POINT ( 'NONE',  ( 0.4658792650918640033, -0.3162353388693405765, 0.4822834645669290543 ) ) ;
#38059 = CARTESIAN_POINT ( 'NONE',  ( 0.9973753280839902091, -0.6046776061558807314, 0.2411417322834647770 ) ) ;
#38060 = CARTESIAN_POINT ( 'NONE',  ( 0.2624671916010504757, 0.2306618581243848609, 0.2411417322834645549 ) ) ;
#38061 = VECTOR ( 'NONE', #58937, 39.37007874015748143 ) ;
#38062 = CARTESIAN_POINT ( 'NONE',  ( 1.502624671916010790, -0.08942795157527998196, 0.3641732283464567121 ) ) ;
#38063 = CARTESIAN_POINT ( 'NONE',  ( -0.8333333333333323711, -0.6692913385826773087, -0.1292274648535924053 ) ) ;
#38064 = CARTESIAN_POINT ( 'NONE',  ( -1.194225721784776262, 0.05413385826771626580, -0.4176697321401330321 ) ) ;
#38065 = CARTESIAN_POINT ( 'NONE',  ( 1.167979002624672580, 0.05413385826771626580, -0.4176697321401330321 ) ) ;
#38066 = CARTESIAN_POINT ( 'NONE',  ( -0.2867679344610364334, -0.2867679344610367109, -0.4586614173228347746 ) ) ;
#38067 = CARTESIAN_POINT ( 'NONE',  ( 0.1049643490035303689, 0.3917322834645670104, -1.560367454068241511 ) ) ;
#38068 = CARTESIAN_POINT ( 'NONE',  ( 0.3917322834645669549, 0.1049643490035304660, -2.793963254593175183 ) ) ;
#38069 = EDGE_LOOP ( 'NONE', ( #70659, #24906, #27913, #24107 ) ) ;
#38070 = CARTESIAN_POINT ( 'NONE',  ( 0.2891555358219910499, -0.2891555358219909944, -2.933070866141733291 ) ) ;
#38071 = ORIENTED_EDGE ( 'NONE', *, *, #71767, .T. ) ;
#38072 = CARTESIAN_POINT ( 'NONE',  ( 1.574803149606299746, -0.1870078740157480879, -0.4822834645669291653 ) ) ;
#38073 = CARTESIAN_POINT ( 'NONE',  ( 1.443569553805774897, 0.1283753931104748280, 0.1820866141732283561 ) ) ;
#38074 = CARTESIAN_POINT ( 'NONE',  ( -0.1998031496062994683, 0.3460692066303958092, -1.430446194225721834 ) ) ;
#38075 = CARTESIAN_POINT ( 'NONE',  ( 1.253280839895013710, -0.08942795157528024563, -0.3641732283464568787 ) ) ;
#38076 = CARTESIAN_POINT ( 'NONE',  ( -1.313877454013331780, 0.2755905511811023723, 0.7983292792091805090 ) ) ;
#38077 = CARTESIAN_POINT ( 'NONE',  ( 2.795275590551181910, 1.900312960331935086, 0.000000000000000000 ) ) ;
#38078 = CARTESIAN_POINT ( 'NONE',  ( 0.4606732211678789546, 1.763126522798926343, 0.5309055118110234117 ) ) ;
#38079 = CARTESIAN_POINT ( 'NONE',  ( -0.1958661417322836718, 0.3392501089628017219, -0.7276902887139108378 ) ) ;
#38080 = CIRCLE ( 'NONE', #16664, 1.122047244094488194 ) ;
#38081 = CARTESIAN_POINT ( 'NONE',  ( -0.7480314960629914633, -0.5511811023622047445, 6.969142054262312111E-17 ) ) ;
#38082 = CARTESIAN_POINT ( 'NONE',  ( -1.476377952755905110, -0.4536011799217368745, -0.2665933059059886201 ) ) ;
#38083 = CARTESIAN_POINT ( 'NONE',  ( -1.115485564304461219, 0.05413385826771626580, -0.4176697321401330321 ) ) ;
#38084 = CARTESIAN_POINT ( 'NONE',  ( 0.05905511811023681640, 0.1660481256975883668, -0.3530559997133364547 ) ) ;
#38085 = CARTESIAN_POINT ( 'NONE',  ( -1.640419947506561060, 0.05413385826771666132, 0.4176697321401328100 ) ) ;
#38086 = VERTEX_POINT ( 'NONE', #73162 ) ;
#38087 = CARTESIAN_POINT ( 'NONE',  ( 2.630268417803912406, 1.724409448818900570, -0.4359958488159719758 ) ) ;
#38088 = CARTESIAN_POINT ( 'NONE',  ( 0.000000000000000000, 0.000000000000000000, 0.000000000000000000 ) ) ;
#38089 = CARTESIAN_POINT ( 'NONE',  ( -0.4724409448818898682, -8.678599364036362592E-17, -2.086614173228346303 ) ) ;
#38090 = DIRECTION ( 'NONE',  ( -3.491481338843132961E-15, -0.000000000000000000, 1.000000000000000000 ) ) ;
#38091 = CARTESIAN_POINT ( 'NONE',  ( -0.2887139107611542133, -0.5023911411419708095, -0.1820866141732282451 ) ) ;
#38092 =( BOUNDED_CURVE ( )  B_SPLINE_CURVE ( 2, ( #47915, #3315, #21431, #80356, #67711, #48743, #66891, #16788, #42425, #36123, #29394, #22669, #9632 ),
 .UNSPECIFIED., .F., .F. ) 
 B_SPLINE_CURVE_WITH_KNOTS ( ( 3, 2, 2, 2, 2, 2, 3 ),
 ( 0.2624999999999999556, 0.2666666666666666075, 0.2708333333333333148, 0.2750000000000000222, 0.2791666666666666741, 0.2833333333333333814, 0.2875000000000000333 ),
 .UNSPECIFIED. ) 
 CURVE ( )  GEOMETRIC_REPRESENTATION_ITEM ( )  RATIONAL_B_SPLINE_CURVE ( ( 1.000000000000000444, 0.9659258262890678681, 1.000000000000000000, 0.9659258262890683122, 1.000000000000000000, 0.9659258262890683122, 1.000000000000000000, 0.9659258262890683122, 1.000000000000000000, 0.9659258262890683122, 1.000000000000000000, 0.9659258262890678681, 1.000000000000000444 ) ) 
 REPRESENTATION_ITEM ( '' )  );
#38093 = CARTESIAN_POINT ( 'NONE',  ( -0.9842519685039360366, 0.2952755905511811885, 0.000000000000000000 ) ) ;
#38094 = CARTESIAN_POINT ( 'NONE',  ( 0.9383202099737538715, -0.05778040916215560624, -0.4822834645669293319 ) ) ;
#38095 = ORIENTED_EDGE ( 'NONE', *, *, #45233, .F. ) ;
#38097 = FACE_OUTER_BOUND ( 'NONE', #79100, .T. ) ;
#38096 = CARTESIAN_POINT ( 'NONE',  ( -0.4724409448818898682, -8.678599364036362592E-17, -2.244094488188976388 ) ) ;
#38098 = CARTESIAN_POINT ( 'NONE',  ( 1.154855643044620184, -0.6046776061558807314, 0.2411417322834647770 ) ) ;
#38099 = CARTESIAN_POINT ( 'NONE',  ( -1.299212598425196097, -0.6692913385826771977, 8.415575281601705876E-17 ) ) ;
#38100 = CARTESIAN_POINT ( 'NONE',  ( 0.3392501089628018329, 0.1958661417322835052, -0.9986683482601557138 ) ) ;
#38101 = CARTESIAN_POINT ( 'NONE',  ( -0.4921259842519677963, -0.4536011799217367080, 0.2665933059059888421 ) ) ;
#38102 = CARTESIAN_POINT ( 'NONE',  ( 0.3917322834645670104, 2.398668435337828261E-17, -0.8326771653543307838 ) ) ;
#38103 = CARTESIAN_POINT ( 'NONE',  ( -0.6299212598425188991, -0.1870078740157480601, -0.3641732283464567677 ) ) ;
#38104 = CARTESIAN_POINT ( 'NONE',  ( -0.07874015748031421014, -0.1870078740157480601, -0.3641732283464567677 ) ) ;
#38105 = CARTESIAN_POINT ( 'NONE',  ( 0.1574803149606306130, -0.1870078740157479769, 0.4822834645669291653 ) ) ;
#38106 = CARTESIAN_POINT ( 'NONE',  ( -0.7414698162729651543, -0.5511811023622046335, 0.09757992244046803654 ) ) ;
#38107 = CARTESIAN_POINT ( 'NONE',  ( -0.2867679344610364334, -0.2867679344610367109, -2.570866141732283339 ) ) ;
#38108 = CARTESIAN_POINT ( 'NONE',  ( 1.043307086614173818, -0.5400638737290845981, -0.3530559997133363437 ) ) ;
#38109 = B_SPLINE_CURVE_WITH_KNOTS ( 'NONE', 3,
 ( #57054, #63382, #64631, #58301 ),
 .UNSPECIFIED., .F., .F.,
 ( 4, 4 ),
 ( 0.000000000000000000, 0.001421551995671108343 ),
 .UNSPECIFIED. ) ;
#38110 = EDGE_CURVE ( 'NONE', #79188, #78367, #22226, .T. ) ;
#38111 = CARTESIAN_POINT ( 'NONE',  ( -1.397637795275589623, -0.5400638737290845981, -0.3530559997133363437 ) ) ;
#38112 = CARTESIAN_POINT ( 'NONE',  ( -0.4724409448818895907, -0.1265901696524993070, -1.067585301837270517 ) ) ;
#38113 = CARTESIAN_POINT ( 'NONE',  ( -0.3018372703412066094, 0.05413385826771666132, 0.4176697321401328100 ) ) ;
#38114 = CARTESIAN_POINT ( 'NONE',  ( -1.017060367454067249, -0.05778040916215522460, 0.4822834645669289988 ) ) ;
#38115 = CARTESIAN_POINT ( 'NONE',  ( 1.266404199475066328, -0.2845877964562161244, -0.3641732283464567121 ) ) ;
#38116 = CARTESIAN_POINT ( 'NONE',  ( -0.1312335958005241554, 0.1283753931104748280, 0.1820866141732283561 ) ) ;
#38117 = CARTESIAN_POINT ( 'NONE',  ( -0.8136482939632537770, -0.6046776061558807314, 0.2411417322834647770 ) ) ;
#38118 = CARTESIAN_POINT ( 'NONE',  ( -0.9776902887139098386, 0.2952755905511810774, -0.1292274648535930714 ) ) ;
#38119 = LINE ( 'NONE', #25899, #82428 ) ;
#38120 = CARTESIAN_POINT ( 'NONE',  ( 1.345144356955381593, -0.08942795157527998196, 0.3641732283464567121 ) ) ;
#38121 = AXIS2_PLACEMENT_3D ( 'NONE', #10912, #68981, #63487 ) ;
#38122 = CARTESIAN_POINT ( 'NONE',  ( -0.3805774278215216522, 0.05413385826771666132, 0.4176697321401328100 ) ) ;
#38123 = CARTESIAN_POINT ( 'NONE',  ( -1.220472440944881054, 0.2952755905511811885, 0.000000000000000000 ) ) ;
#38124 = ORIENTED_EDGE ( 'NONE', *, *, #51676, .F. ) ;
#38125 = CARTESIAN_POINT ( 'NONE',  ( 0.2925321140481932369, -0.2925321140481931814, -2.222440944881889813 ) ) ;
#38126 = CARTESIAN_POINT ( 'NONE',  ( -0.8989501312335946848, -0.5511811023622046335, 0.09757992244046803654 ) ) ;
#38127 = CARTESIAN_POINT ( 'NONE',  ( 0.9908136482939640111, 0.2952755905511810774, -0.1292274648535930714 ) ) ;
#38128 = CARTESIAN_POINT ( 'NONE',  ( -1.010498687664041384, -0.3690944881889765550, -0.3153832671262227771 ) ) ;
#38129 = CARTESIAN_POINT ( 'NONE',  ( -9.787531504996566615E-17, 0.3996062992125985480, -1.179133858267716661 ) ) ;
#38130 = CARTESIAN_POINT ( 'NONE',  ( -0.9448818897637790704, -0.1870078740157479769, 0.4822834645669291653 ) ) ;
#38131 = CARTESIAN_POINT ( 'NONE',  ( 1.003937007874016407, -0.5400638737290844871, 0.3530559997133364547 ) ) ;
#38132 = CARTESIAN_POINT ( 'NONE',  ( 0.9514435695538062676, -0.3162353388693409650, -0.4822834645669289433 ) ) ;
#38133 = CARTESIAN_POINT ( 'NONE',  ( 1.522309711286089939, -0.6046776061558809534, -0.2411417322834644161 ) ) ;
#38134 = CARTESIAN_POINT ( 'NONE',  ( -1.509186351706035767, -0.004921259842519870586, -0.3153832671262229437 ) ) ;
#38135 = CARTESIAN_POINT ( 'NONE',  ( 0.3996062992125984925, 0.1070741851644054499, -0.8313648293963252778 ) ) ;
#38136 = CARTESIAN_POINT ( 'NONE',  ( 0.2925321140481932369, -0.2925321140481932369, -0.8858267716535430658 ) ) ;
#38137 = CIRCLE ( 'NONE', #27394, 1.220472440944883719 ) ;
#38138 = CARTESIAN_POINT ( 'NONE',  ( 0.1974969037888704704, 0.3420746716998660508, -0.1443569553805774675 ) ) ;
#38139 = CARTESIAN_POINT ( 'NONE',  ( -1.968503937007874072, 0.000000000000000000, 5.544487991299990703 ) ) ;
#38140 = CARTESIAN_POINT ( 'NONE',  ( 1.141732283464567788, -0.5511811023622047445, 6.969142054262312111E-17 ) ) ;
#38141 = EDGE_CURVE ( 'NONE', #57006, #15098, #81544, .T. ) ;
#38142 = CARTESIAN_POINT ( 'NONE',  ( 0.7020997375328090762, -0.08942795157528024563, -0.3641732283464568787 ) ) ;
#38143 = CARTESIAN_POINT ( 'NONE',  ( 0.01312335958005323398, 0.05413385826771666132, 0.4176697321401328100 ) ) ;
#38144 = CARTESIAN_POINT ( 'NONE',  ( -0.1265901696524986964, -0.4724409448818899238, -2.353674540682414662 ) ) ;
#38145 = CARTESIAN_POINT ( 'NONE',  ( 4.837279021331061486E-17, -0.3949938075777409963, -1.257874015748031260 ) ) ;
#38146 = CARTESIAN_POINT ( 'NONE',  ( 0.9973753280839902091, -0.5023911411419708095, 0.1820866141732285504 ) ) ;
#38147 = CARTESIAN_POINT ( 'NONE',  ( -0.4658792650918627265, -0.3162353388693409650, -0.4822834645669289433 ) ) ;
#38148 = CARTESIAN_POINT ( 'NONE',  ( -1.371391076115484609, -0.6692913385826771977, 0.1292274648535927661 ) ) ;
#38149 = CARTESIAN_POINT ( 'NONE',  ( 0.7742782152230979209, 0.05413385826771626580, -0.4176697321401330321 ) ) ;
#38150 = CARTESIAN_POINT ( 'NONE',  ( -0.1265901696524993347, 0.4724409448818895907, -1.423884514435695525 ) ) ;
#38151 = CARTESIAN_POINT ( 'NONE',  ( -0.7202472836732357608, 0.02791078216816347476, -0.4328096321851898631 ) ) ;
#38152 = EDGE_LOOP ( 'NONE', ( #59211, #47073, #48243, #12854 ) ) ;
#38153 = EDGE_LOOP ( 'NONE', ( #28357, #42302, #25456, #31436 ) ) ;
#38154 = CARTESIAN_POINT ( 'NONE',  ( -1.181102362204723644, -0.1870078740157480879, -0.4822834645669291653 ) ) ;
#38155 = CARTESIAN_POINT ( 'NONE',  ( -0.7874015748031489847, -0.1870078740157480879, -0.4822834645669291653 ) ) ;
#38157 = CARTESIAN_POINT ( 'NONE',  ( -0.7611548556430438595, -0.6046776061558809534, -0.2411417322834644161 ) ) ;
#38156 = CARTESIAN_POINT ( 'NONE',  ( -0.8398950131233585692, 0.1283753931104748280, 0.1820866141732283561 ) ) ;
#38158 = CARTESIAN_POINT ( 'NONE',  ( 0.1958661417322834497, 0.3392501089628018329, -2.114153912564617599 ) ) ;
#38159 = CARTESIAN_POINT ( 'NONE',  ( -0.2296587926509179312, -0.05778040916215522460, 0.4822834645669289988 ) ) ;
#38160 = CARTESIAN_POINT ( 'NONE',  ( 1.443569553805774897, 0.2306618581243848609, 0.2411417322834645549 ) ) ;
#38161 = CARTESIAN_POINT ( 'NONE',  ( -0.8267716535433065062, -0.6692913385826771977, 8.415575281601705876E-17 ) ) ;
#38162 = CARTESIAN_POINT ( 'NONE',  ( 0.2559055118110243332, -0.5400638737290845981, -0.3530559997133363437 ) ) ;
#38163 = ADVANCED_FACE ( 'NONE', ( #79082 ), #7529, .F. ) ;
#38164 = CARTESIAN_POINT ( 'NONE',  ( -0.3917322834645669549, -0.1049643490035306603, -1.297900262467191590 ) ) ;
#38165 = CARTESIAN_POINT ( 'NONE',  ( -0.7283464566929126471, -0.4536011799217367080, 0.2665933059059888421 ) ) ;
#38166 = ORIENTED_EDGE ( 'NONE', *, *, #6316, .T. ) ;
#38167 = CARTESIAN_POINT ( 'NONE',  ( -9.674558042662121740E-17, 0.3949938075777409963, -1.889763779527559029 ) ) ;
#38168 = ORIENTED_EDGE ( 'NONE', *, *, #44178, .F. ) ;
#38169 = CARTESIAN_POINT ( 'NONE',  ( -1.725721784776902190, -0.08942795157527998196, 0.3641732283464567121 ) ) ;
#38170 = CARTESIAN_POINT ( 'NONE',  ( -1.030183727034119867, -0.3162353388693405765, 0.4822834645669290543 ) ) ;
#38171 = CARTESIAN_POINT ( 'NONE',  ( -0.8333333333333323711, 0.2952755905511811885, 0.1292274648535926551 ) ) ;
#38172 = CARTESIAN_POINT ( 'NONE',  ( -0.3996062992125986035, -7.340648628747425578E-17, -0.03937007874015749365 ) ) ;
#38173 = CARTESIAN_POINT ( 'NONE',  ( -1.167979002624671470, -0.4281496062992127816, -0.4176697321401328100 ) ) ;
#38174 = CARTESIAN_POINT ( 'NONE',  ( -1.338582677165353729, -0.1870078740157480879, -0.4822834645669291653 ) ) ;
#38175 = CARTESIAN_POINT ( 'NONE',  ( -1.555118110236219930, -0.5400638737290845981, -0.3530559997133363437 ) ) ;
#38176 = CARTESIAN_POINT ( 'NONE',  ( 0.6199123404867349363, 8.471767977567108961E-16, -0.4445507791589058955 ) ) ;
#38177 = CARTESIAN_POINT ( 'NONE',  ( 0.6167979002624679463, -0.004921259842519870586, -0.3153832671262229437 ) ) ;
#38178 = CARTESIAN_POINT ( 'NONE',  ( 0.9881811337016640495, 2.755905511811024056, 0.5314960629921260393 ) ) ;
#38179 = CARTESIAN_POINT ( 'NONE',  ( -0.2867679344610364334, -0.2867679344610367109, 0.1712598425196849850 ) ) ;
#38180 = CARTESIAN_POINT ( 'NONE',  ( -0.5643044619422565855, -0.004921259842519870586, -0.3153832671262229437 ) ) ;
#38181 = CARTESIAN_POINT ( 'NONE',  ( -0.8530183727034112984, 0.05413385826771666132, 0.4176697321401328100 ) ) ;
#38182 = CARTESIAN_POINT ( 'NONE',  ( 1.384514435695538337, -0.6692913385826771977, 0.1292274648535927661 ) ) ;
#38183 = CARTESIAN_POINT ( 'NONE',  ( -0.5052493438320203589, 0.2952755905511810774, -0.1292274648535930714 ) ) ;
#38184 = VERTEX_POINT ( 'NONE', #15094 ) ;
#38185 = EDGE_LOOP ( 'NONE', ( #38686, #11781 ) ) ;
#38186 = CARTESIAN_POINT ( 'NONE',  ( -9.787531504996566615E-17, 0.3996062992125985480, -2.124015748031495843 ) ) ;
#38187 = CARTESIAN_POINT ( 'NONE',  ( -0.4658792650918627265, -0.3162353388693409650, -0.4822834645669289433 ) ) ;
#38188 = CARTESIAN_POINT ( 'NONE',  ( 1.430446194225722500, 0.05413385826771666132, 0.4176697321401328100 ) ) ;
#38189 = CARTESIAN_POINT ( 'NONE',  ( -1.253280839895012377, -0.08942795157527998196, 0.3641732283464567121 ) ) ;
#38190 = CARTESIAN_POINT ( 'NONE',  ( -1.286089238845143479, -0.6046776061558807314, 0.2411417322834647770 ) ) ;
#38191 = CARTESIAN_POINT ( 'NONE',  ( -1.157146581871515012E-16, 0.4724409448818898682, -0.7874015748031496509 ) ) ;
#38192 = CARTESIAN_POINT ( 'NONE',  ( 1.964921794496066632, 1.189595890467126882, 0.3229789317950442218 ) ) ;
#38193 = CARTESIAN_POINT ( 'NONE',  ( 0.3392501089628018884, -0.1958661417322834220, -0.09711286089238840846 ) ) ;
#38194 = CARTESIAN_POINT ( 'NONE',  ( -0.3392501089628019995, 0.1958661417322832277, -2.158136482939632561 ) ) ;
#38195 = CARTESIAN_POINT ( 'NONE',  ( 0.2362204724409456558, -0.1870078740157479769, 0.4822834645669291653 ) ) ;
#38196 = CARTESIAN_POINT ( 'NONE',  ( -0.8989501312335946848, -0.5511811023622046335, 0.09757992244046803654 ) ) ;
#38197 = CARTESIAN_POINT ( 'NONE',  ( -0.4133858267716528645, 0.1660481256975883668, -0.3530559997133364547 ) ) ;
#38198 = CARTESIAN_POINT ( 'NONE',  ( -0.2362204724409451284, 0.4091458600556402425, -2.609580052493438274 ) ) ;
#38199 = CARTESIAN_POINT ( 'NONE',  ( -0.6955380577427815458, -0.4281496062992127816, -0.4176697321401328100 ) ) ;
#38200 = CARTESIAN_POINT ( 'NONE',  ( -0.8858267716535425107, 0.1660481256975883668, -0.3530559997133364547 ) ) ;
#38201 = AXIS2_PLACEMENT_3D ( 'NONE', #53370, #28535, #28948 ) ;
#38202 = CARTESIAN_POINT ( 'NONE',  ( 0.1058382717557500852, -0.3949938075777408852, -2.366797900262467280 ) ) ;
#38203 = CARTESIAN_POINT ( 'NONE',  ( 1.017060367454068581, -0.08942795157528024563, -0.3641732283464568787 ) ) ;
#38204 = CARTESIAN_POINT ( 'NONE',  ( -0.9120734908136475250, 0.1771653543307087630, 0.09757992244046791164 ) ) ;
#38205 = CARTESIAN_POINT ( 'NONE',  ( 0.8464566929133866546, -0.4536011799217367080, 0.2665933059059888421 ) ) ;
#38206 = CARTESIAN_POINT ( 'NONE',  ( -1.679790026246718693, 0.2306618581243847221, -0.2411417322834647770 ) ) ;
#38207 = CARTESIAN_POINT ( 'NONE',  ( 1.502624671916010790, -0.3162353388693409650, -0.4822834645669289433 ) ) ;
#38208 = CARTESIAN_POINT ( 'NONE',  ( 0.6889763779527566800, -0.4536011799217367080, 0.2665933059059888421 ) ) ;
#38209 = CARTESIAN_POINT ( 'NONE',  ( -0.2867679344610365999, 0.2867679344610364889, -1.429133858267716661 ) ) ;
#38210 = CARTESIAN_POINT ( 'NONE',  ( -0.8398950131233585692, 0.2306618581243848609, 0.2411417322834645549 ) ) ;
#38211 = CARTESIAN_POINT ( 'NONE',  ( 1.148293963254593653, 0.2952755905511810774, -0.1292274648535930714 ) ) ;
#38212 = CARTESIAN_POINT ( 'NONE',  ( -0.4724409448818895907, -0.1265901696524993070, 0.1922572178477690297 ) ) ;
#38213 = CARTESIAN_POINT ( 'NONE',  ( -0.2362204724409440182, -0.1870078740157479769, 0.3641732283464567677 ) ) ;
#38214 = CARTESIAN_POINT ( 'NONE',  ( 0.6399301791983058596, -1.374501131054255944E-15, 0.4445507791589066726 ) ) ;
#38215 = CARTESIAN_POINT ( 'NONE',  ( 0.3346456692913393205, -0.5400638737290845981, -0.3530559997133363437 ) ) ;
#38216 = CARTESIAN_POINT ( 'NONE',  ( 0.6692913385826777528, 0.2952755905511811885, 0.000000000000000000 ) ) ;
#38217 = CARTESIAN_POINT ( 'NONE',  ( 0.8923884514435701520, -0.5023911411419708095, -0.1820866141732282451 ) ) ;
#38218 = CARTESIAN_POINT ( 'NONE',  ( 0.1771653543307093182, 0.07958543189024085140, 0.2665933059059887866 ) ) ;
#38219 = CARTESIAN_POINT ( 'NONE',  ( 0.1246719160104994284, 0.2952755905511810774, -0.1292274648535930714 ) ) ;
#38220 = CARTESIAN_POINT ( 'NONE',  ( -1.561679790026246017, 0.05413385826771666132, 0.4176697321401328100 ) ) ;
#38221 = CARTESIAN_POINT ( 'NONE',  ( -0.5905511811023613777, -0.5511811023622047445, 6.969142054262312111E-17 ) ) ;
#38222 = PLANE ( 'NONE',  #7190 ) ;
#38223 = CARTESIAN_POINT ( 'NONE',  ( -0.3477690288713902178, 0.2952755905511810774, -0.1292274648535930714 ) ) ;
#38224 = CARTESIAN_POINT ( 'NONE',  ( 0.1070741851644053388, 0.3996062992125986035, -1.330052493438320216 ) ) ;
#38225 = CARTESIAN_POINT ( 'NONE',  ( -0.1049643490035307020, 0.3917322834645669549, -2.295931758530183497 ) ) ;
#38226 = CARTESIAN_POINT ( 'NONE',  ( 0.07874015748031558404, -0.1870078740157480601, -0.3641732283464567677 ) ) ;
#38227 = CARTESIAN_POINT ( 'NONE',  ( -0.4593175853018364174, -0.4281496062992127816, -0.4176697321401328100 ) ) ;
#38228 = CARTESIAN_POINT ( 'NONE',  ( -1.122047244094487306, 0.1660481256975883668, -0.3530559997133364547 ) ) ;
#38229 = CARTESIAN_POINT ( 'NONE',  ( -0.7283464566929126471, -0.4536011799217367080, 0.2665933059059888421 ) ) ;
#38230 = CARTESIAN_POINT ( 'NONE',  ( -3.931483604541833987, 1.111096610303996091, 0.2104479119174702539 ) ) ;
#38231 = CARTESIAN_POINT ( 'NONE',  ( -0.1312335958005241554, -0.6046776061558809534, -0.2411417322834644161 ) ) ;
#38232 = CARTESIAN_POINT ( 'NONE',  ( -1.601049868766403650, -0.5023911411419708095, 0.1820866141732285504 ) ) ;
#38233 = CARTESIAN_POINT ( 'NONE',  ( 1.200787401574803681, -0.5400638737290845981, -0.3530559997133363437 ) ) ;
#38234 = CARTESIAN_POINT ( 'NONE',  ( -0.4678115244718906163, 1.617859111677685924, 1.019879954333916761 ) ) ;
#38235 = CARTESIAN_POINT ( 'NONE',  ( 4.797336870675656522E-17, -0.3917322834645670659, -2.280203042815959869 ) ) ;
#38236 = ORIENTED_EDGE ( 'NONE', *, *, #66367, .F. ) ;
#38237 = VECTOR ( 'NONE', #48252, 39.37007874015748143 ) ;
#38238 = FACE_BOUND ( 'NONE', #44962, .T. ) ;
#38239 = EDGE_CURVE ( 'NONE', #23562, #64782, #30721, .T. ) ;
#38240 = CARTESIAN_POINT ( 'NONE',  ( -1.200787401574802349, 0.1660481256975883668, -0.3530559997133364547 ) ) ;
#38241 = CARTESIAN_POINT ( 'NONE',  ( -0.8661417322834640276, -0.1870078740157480879, -0.4822834645669291653 ) ) ;
#38242 = CARTESIAN_POINT ( 'NONE',  ( -1.555118110236219930, -0.5400638737290845981, -0.3530559997133363437 ) ) ;
#38243 = CARTESIAN_POINT ( 'NONE',  ( 0.3392501089628018329, 0.1958661417322835607, -2.105643044619422533 ) ) ;
#38244 = CARTESIAN_POINT ( 'NONE',  ( -0.3692639355350240127, 0.1324727617108177880, -1.220472440944881720 ) ) ;
#38245 = CARTESIAN_POINT ( 'NONE',  ( 0.9251968503937015864, 0.1660481256975883668, -0.3530559997133364547 ) ) ;
#38246 = CARTESIAN_POINT ( 'NONE',  ( 0.1377952755905518800, 0.1660481256975883668, -0.3530559997133364547 ) ) ;
#38247 = CARTESIAN_POINT ( 'NONE',  ( 0.000000000000000000, 0.000000000000000000, -0.1574803149606299746 ) ) ;
#38248 = CARTESIAN_POINT ( 'NONE',  ( -0.3460692066303960313, 0.1998031496062989965, -2.622703412073490892 ) ) ;
#38249 = CARTESIAN_POINT ( 'NONE',  ( 1.286089238845145033, 0.1283753931104748280, 0.1820866141732283561 ) ) ;
#38250 = CARTESIAN_POINT ( 'NONE',  ( 0.1070741851644053527, 0.3996062992125986590, -1.253280839895013044 ) ) ;
#38251 = ORIENTED_EDGE ( 'NONE', *, *, #67725, .T. ) ;
#38253 = CARTESIAN_POINT ( 'NONE',  ( -0.1958661417322836995, 0.3392501089628017219, -0.009861835466878533449 ) ) ;
#38252 = VECTOR ( 'NONE', #799, 39.37007874015748143 ) ;
#38254 = EDGE_LOOP ( 'NONE', ( #52773, #63387, #26894, #72579, #28356, #61710, #28142 ) ) ;
#38255 = CARTESIAN_POINT ( 'NONE',  ( 0.1640419947506569498, -0.05778040916215522460, 0.4822834645669289988 ) ) ;
#38256 = CARTESIAN_POINT ( 'NONE',  ( -0.8989501312335946848, 0.2952755905511810774, -0.1292274648535930714 ) ) ;
#38257 = CARTESIAN_POINT ( 'NONE',  ( -1.594488188976377119, 0.1660481256975883668, -0.3530559997133364547 ) ) ;
#38258 = CARTESIAN_POINT ( 'NONE',  ( 0.4396325459317593221, 0.2952755905511810774, -0.1292274648535930714 ) ) ;
#38259 = CARTESIAN_POINT ( 'NONE',  ( 1.450131233595801428, -0.6692913385826773087, -0.1292274648535924053 ) ) ;
#38260 = CARTESIAN_POINT ( 'NONE',  ( -0.1574803149606292529, -0.1870078740157480879, -0.4822834645669291653 ) ) ;
#38261 = CARTESIAN_POINT ( 'NONE',  ( -1.167979002624671470, 0.05413385826771666132, 0.4176697321401328100 ) ) ;
#38262 = CARTESIAN_POINT ( 'NONE',  ( 1.128608923884514947, 0.2306618581243848609, 0.2411417322834645549 ) ) ;
#38263 = B_SPLINE_CURVE_WITH_KNOTS ( 'NONE', 3,
 ( #44241, #77510, #38775, #918, #19845, #64452, #13533 ),
 .UNSPECIFIED., .F., .F.,
 ( 4, 3, 4 ),
 ( 1.734723475976807094E-18, 0.001246232571205225159, 0.002492492258783242029 ),
 .UNSPECIFIED. ) ;
#38264 = CARTESIAN_POINT ( 'NONE',  ( 1.561679790026247350, 0.05413385826771626580, -0.4176697321401330321 ) ) ;
#38265 = CARTESIAN_POINT ( 'NONE',  ( -0.08530183727034056085, -0.05778040916215560624, -0.4822834645669293319 ) ) ;
#38266 = CARTESIAN_POINT ( 'NONE',  ( 0.1958661417322834775, 0.3392501089628018884, -0.1364829396325459021 ) ) ;
#38267 = CARTESIAN_POINT ( 'NONE',  ( 0.4068241469816281097, -0.004921259842519576551, 0.3153832671262227771 ) ) ;
#38268 = VERTEX_POINT ( 'NONE', #32252 ) ;
#38269 = CARTESIAN_POINT ( 'NONE',  ( 0.3949938075777409408, 0.1058382717557500574, -0.5971128608923886860 ) ) ;
#38270 = ORIENTED_EDGE ( 'NONE', *, *, #69485, .T. ) ;
#38271 = CARTESIAN_POINT ( 'NONE',  ( -0.03280839895013062252, -0.5511811023622046335, 0.09757992244046803654 ) ) ;
#38272 = CARTESIAN_POINT ( 'NONE',  ( -0.2362204724409451284, 0.4091458600556402425, -0.1706036745406823985 ) ) ;
#38273 = CARTESIAN_POINT ( 'NONE',  ( -0.03280839895013062252, -0.6692913385826771977, 0.1292274648535927661 ) ) ;
#38274 = CARTESIAN_POINT ( 'NONE',  ( -0.1377952755905504645, 0.1660481256975885056, 0.3530559997133364547 ) ) ;
#38275 = EDGE_CURVE ( 'NONE', #82700, #62471, #57913, .T. ) ;
#38276 = CARTESIAN_POINT ( 'NONE',  ( -0.7677165354330699465, 0.1660481256975885056, 0.3530559997133364547 ) ) ;
#38277 = CARTESIAN_POINT ( 'NONE',  ( 0.2867679344610366554, 0.2867679344610366554, -1.866817216044307060 ) ) ;
#38278 = CARTESIAN_POINT ( 'NONE',  ( -1.030183727034119867, -0.3162353388693405765, 0.4822834645669290543 ) ) ;
#38279 = PRODUCT_DEFINITION ( 'UNKNOWN', '', #53084, #77355 ) ;
#38280 = CARTESIAN_POINT ( 'NONE',  ( 0.2867679344610365999, 0.2867679344610365999, -2.742125984251967630 ) ) ;
#38281 = CARTESIAN_POINT ( 'NONE',  ( 0.7283464566929140904, -0.4536011799217368745, -0.2665933059059886201 ) ) ;
#38282 = CARTESIAN_POINT ( 'NONE',  ( 0.9580052493438327987, -0.4281496062992127816, -0.4176697321401328100 ) ) ;
#38283 = CARTESIAN_POINT ( 'NONE',  ( 0.6889763779527566800, -0.5400638737290844871, 0.3530559997133364547 ) ) ;
#38284 = CARTESIAN_POINT ( 'NONE',  ( 0.3460692066303959757, -0.1998031496062991907, -0.8923884514435694859 ) ) ;
#38285 = CARTESIAN_POINT ( 'NONE',  ( -1.384514435695537005, 0.2952755905511811885, 0.1292274648535926551 ) ) ;
#38286 = CARTESIAN_POINT ( 'NONE',  ( -0.1070741851644056997, 0.3996062992125984925, -0.2408136482939632061 ) ) ;
#38287 = CARTESIAN_POINT ( 'NONE',  ( -0.2925321140481932369, 0.2925321140481931259, 0.06102362204724406242 ) ) ;
#38288 = CARTESIAN_POINT ( 'NONE',  ( -0.2952755905511804668, 0.1660481256975885056, 0.3530559997133364547 ) ) ;
#38289 = CARTESIAN_POINT ( 'NONE',  ( 0.1998031496062992740, 0.3460692066303959757, -2.821522309711286258 ) ) ;
#38290 = CARTESIAN_POINT ( 'NONE',  ( -0.2867679344610364334, -0.2867679344610367109, -1.875984251968503935 ) ) ;
#38291 = CARTESIAN_POINT ( 'NONE',  ( 1.259842519685040019, -0.1870078740157479769, 0.4822834645669291653 ) ) ;
#38292 = CARTESIAN_POINT ( 'NONE',  ( 1.253280839895013710, -0.05778040916215560624, -0.4822834645669293319 ) ) ;
#38293 = CARTESIAN_POINT ( 'NONE',  ( 0.2690288713910767848, 0.1771653543307087630, 0.09757992244046791164 ) ) ;
#38294 = CARTESIAN_POINT ( 'NONE',  ( 0.9776902887139113929, 0.2952755905511811885, 0.1292274648535926551 ) ) ;
#38295 = CARTESIAN_POINT ( 'NONE',  ( 0.4724409448818898682, 2.892866454678787531E-17, -1.297244094488188670 ) ) ;
#38296 = CARTESIAN_POINT ( 'NONE',  ( 0.1574803149606306130, -0.1870078740157480601, -0.3641732283464567677 ) ) ;
#38297 = EDGE_CURVE ( 'NONE', #50786, #21089, #78826, .T. ) ;
#38298 = CARTESIAN_POINT ( 'NONE',  ( 0.4396325459317590445, -0.6692913385826771977, 0.1292274648535927661 ) ) ;
#38299 = CARTESIAN_POINT ( 'NONE',  ( 0.1058382717557500852, -0.3949938075777408852, -0.9494750656167980640 ) ) ;
#38300 = CARTESIAN_POINT ( 'NONE',  ( -1.154855643044618851, -0.6046776061558809534, -0.2411417322834644161 ) ) ;
#38301 = AXIS2_PLACEMENT_3D ( 'NONE', #59525, #66271, #1882 ) ;
#38302 = CARTESIAN_POINT ( 'NONE',  ( 1.069553805774278610, -0.5511811023622046335, 0.09757992244046803654 ) ) ;
#38303 = EDGE_CURVE ( 'NONE', #73526, #44157, #33921, .T. ) ;
#38304 = CARTESIAN_POINT ( 'NONE',  ( 0.3543307086614179147, 0.2066929133858268208, 0.000000000000000000 ) ) ;
#38305 = CARTESIAN_POINT ( 'NONE',  ( -0.4461942257217840213, 0.2306618581243848609, 0.2411417322834645549 ) ) ;
#38306 = CARTESIAN_POINT ( 'NONE',  ( -0.3805774278215216522, -0.004921259842519576551, 0.3153832671262227771 ) ) ;
#38307 = CARTESIAN_POINT ( 'NONE',  ( 0.4606732211678742361, 1.778019097314512686, 0.5309055118110234117 ) ) ;
#38308 = CARTESIAN_POINT ( 'NONE',  ( -0.4133858267716528645, 0.1660481256975883668, -0.3530559997133364547 ) ) ;
#38309 = CARTESIAN_POINT ( 'NONE',  ( 0.4790026246719167324, -0.08942795157527998196, 0.3641732283464567121 ) ) ;
#38310 = CARTESIAN_POINT ( 'NONE',  ( 0.3460692066303959202, -0.1998031496062991630, -2.229002624671916344 ) ) ;
#38311 = CARTESIAN_POINT ( 'NONE',  ( -0.1181102362204717315, -0.6692913385826771977, 8.415575281601705876E-17 ) ) ;
#38312 = CARTESIAN_POINT ( 'NONE',  ( 0.3392501089628018329, 0.1958661417322835052, -1.628589608102675390 ) ) ;
#38313 = CARTESIAN_POINT ( 'NONE',  ( 1.240157480314961314, 0.07958543189024071263, -0.2665933059059888421 ) ) ;
#38314 = CARTESIAN_POINT ( 'NONE',  ( 0.3812812444996376282, 2.409604939980833412E-17, -0.3464511005275205946 ) ) ;
#38315 = CARTESIAN_POINT ( 'NONE',  ( -0.6955380577427815458, -0.3690944881889765550, -0.3153832671262227771 ) ) ;
#38316 = CIRCLE ( 'NONE', #73252, 0.09842519685039351207 ) ;
#38317 = CARTESIAN_POINT ( 'NONE',  ( -0.7611548556430438595, 0.1283753931104748280, 0.1820866141732283561 ) ) ;
#38318 = CARTESIAN_POINT ( 'NONE',  ( -0.3280839895013117347, 0.05413385826771626580, -0.4176697321401330321 ) ) ;
#38319 = CARTESIAN_POINT ( 'NONE',  ( 0.07217847769028949700, -0.05778040916215560624, -0.4822834645669293319 ) ) ;
#38320 = CARTESIAN_POINT ( 'NONE',  ( 0.4002624671916016896, -0.08942795157527998196, 0.3641732283464567121 ) ) ;
#38321 = DIRECTION ( 'NONE',  ( 1.000000000000000000, 0.000000000000000000, 3.455050906509825972E-15 ) ) ;
#38322 = CARTESIAN_POINT ( 'NONE',  ( 1.404199475065617264, -0.3690944881889763329, 0.3153832671262228327 ) ) ;
#38323 = ADVANCED_FACE ( 'NONE', ( #83189 ), #69327, .F. ) ;
#38324 = CARTESIAN_POINT ( 'NONE',  ( 0.5708661417322842269, 0.1660481256975885056, 0.3530559997133364547 ) ) ;
#38325 = CARTESIAN_POINT ( 'NONE',  ( 0.4672528563079797470, 1.453807508635538870, -2.153192469889489757 ) ) ;
#38326 = CARTESIAN_POINT ( 'NONE',  ( -0.1968503937007867743, -0.6692913385826771977, 8.415575281601705876E-17 ) ) ;
#38327 = CARTESIAN_POINT ( 'NONE',  ( 4.797336870675656522E-17, -0.3917322834645670104, -0.7933070866141732624 ) ) ;
#38328 = CARTESIAN_POINT ( 'NONE',  ( -1.318897637795274802, -0.5400638737290845981, -0.3530559997133363437 ) ) ;
#38329 = CARTESIAN_POINT ( 'NONE',  ( 0.9251968503937015864, 0.1660481256975883668, -0.3530559997133364547 ) ) ;
#38330 = CARTESIAN_POINT ( 'NONE',  ( 0.4921259842519691285, -0.5400638737290845981, -0.3530559997133363437 ) ) ;
#38331 = CARTESIAN_POINT ( 'NONE',  ( 0.4199475065616805614, 0.1283753931104748280, 0.1820866141732283561 ) ) ;
#38332 = CARTESIAN_POINT ( 'NONE',  ( 1.312335958005250269, -0.6046776061558807314, 0.2411417322834647770 ) ) ;
#38333 = EDGE_CURVE ( 'NONE', #2585, #39954, #44044, .T. ) ;
#38334 = CARTESIAN_POINT ( 'NONE',  ( -0.2821522309711278487, 0.1771653543307087630, 0.09757992244046791164 ) ) ;
#38335 = CARTESIAN_POINT ( 'NONE',  ( -0.5839895013123351797, -0.6692913385826771977, 0.1292274648535927661 ) ) ;
#38336 = CARTESIAN_POINT ( 'NONE',  ( 0.3458507752293908943, -0.3458507752293908943, -2.618110236220472675 ) ) ;
#38337 = CARTESIAN_POINT ( 'NONE',  ( 0.3937007874015754361, -0.1870078740157480879, -0.4822834645669291653 ) ) ;
#38338 = CARTESIAN_POINT ( 'NONE',  ( -0.9055118110236215490, -0.6692913385826771977, 8.415575281601705876E-17 ) ) ;
#38339 = CARTESIAN_POINT ( 'NONE',  ( -0.8005249343832013809, -0.3690944881889763329, 0.3153832671262228327 ) ) ;
#38340 = CARTESIAN_POINT ( 'NONE',  ( 0.3412073490813655186, 0.2306618581243848609, 0.2411417322834645549 ) ) ;
#38341 = CARTESIAN_POINT ( 'NONE',  ( -1.115485564304461219, -0.4281496062992124485, 0.4176697321401328655 ) ) ;
#38342 = CARTESIAN_POINT ( 'NONE',  ( -0.2230971128608915943, 0.05413385826771666132, 0.4176697321401328100 ) ) ;
#38343 = EDGE_CURVE ( 'NONE', #16885, #36844, #20471, .T. ) ;
#38344 =( NAMED_UNIT ( * ) PLANE_ANGLE_UNIT ( ) SI_UNIT ( $, .RADIAN. ) );
#38346 = CARTESIAN_POINT ( 'NONE',  ( 1.174540682414699111, -0.05778040916215560624, -0.4822834645669293319 ) ) ;
#38345 = CARTESIAN_POINT ( 'NONE',  ( -1.586052503253848611, 0.7480314960629931287, 0.1653254495020559378 ) ) ;
#38347 = CARTESIAN_POINT ( 'NONE',  ( 1.128608923884515169, -0.6046776061558809534, -0.2411417322834644161 ) ) ;
#38348 = CARTESIAN_POINT ( 'NONE',  ( 0.3917322834645670104, 2.398668435337828261E-17, -2.157480314960630086 ) ) ;
#38349 = CARTESIAN_POINT ( 'NONE',  ( 0.4768059346183028957, 1.738380701482457269, -0.5050996235782325705 ) ) ;
#38350 = CARTESIAN_POINT ( 'NONE',  ( -1.108923884514435132, -0.3162353388693405765, 0.4822834645669290543 ) ) ;
#38351 = CARTESIAN_POINT ( 'NONE',  ( 0.4091458600556403535, 0.2362204724409449896, -0.4461942257217847430 ) ) ;
#38352 = CARTESIAN_POINT ( 'NONE',  ( 0.3460692066303959757, -0.1998031496062991907, -0.2624671916010499206 ) ) ;
#38353 = VERTEX_POINT ( 'NONE', #77719 ) ;
#38354 = CARTESIAN_POINT ( 'NONE',  ( -0.1902887139107604098, 0.1771653543307087075, -0.09757992244046823083 ) ) ;
#38355 = CARTESIAN_POINT ( 'NONE',  ( -0.3917322834645669549, -0.1049643490035306603, -1.927821522309711044 ) ) ;
#38356 = CARTESIAN_POINT ( 'NONE',  ( 0.6824146981627303710, 0.2306618581243847221, -0.2411417322834647770 ) ) ;
#38357 = CARTESIAN_POINT ( 'NONE',  ( 0.3458507752293908943, -0.3458507752293908943, -2.933070866141732402 ) ) ;
#38358 = CARTESIAN_POINT ( 'NONE',  ( -1.595398199321655719, 1.860919225514068298, -0.1559797534342489689 ) ) ;
#38359 = CARTESIAN_POINT ( 'NONE',  ( -0.5643044619422565855, -0.3690944881889763329, 0.3153832671262228327 ) ) ;
#38360 =( CONVERSION_BASED_UNIT ( 'INCH', #19001 ) LENGTH_UNIT ( ) NAMED_UNIT ( #37342 ) );
#38361 = CARTESIAN_POINT ( 'NONE',  ( 1.266404199475066328, -0.3162353388693409650, -0.4822834645669289433 ) ) ;
#38362 = CARTESIAN_POINT ( 'NONE',  ( 0.7545931758530188826, -0.5511811023622046335, 0.09757992244046803654 ) ) ;
#38363 = CARTESIAN_POINT ( 'NONE',  ( -0.07874015748031421014, -0.1870078740157479769, 0.4822834645669291653 ) ) ;
#38364 = CARTESIAN_POINT ( 'NONE',  ( -0.3392501089628019439, 0.1958661417322832554, -0.5787208416984759296 ) ) ;
#38365 = CARTESIAN_POINT ( 'NONE',  ( -1.010498687664041384, 0.05413385826771666132, 0.4176697321401328100 ) ) ;
#38366 = CARTESIAN_POINT ( 'NONE',  ( -1.253280839895012377, -0.08942795157527998196, 0.3641732283464567121 ) ) ;
#38367 = CARTESIAN_POINT ( 'NONE',  ( -0.5249343832020990641, -0.6046776061558809534, -0.2411417322834644161 ) ) ;
#38368 = DIRECTION ( 'NONE',  ( 0.000000000000000000, 0.000000000000000000, 1.000000000000000000 ) ) ;
#38369 = CARTESIAN_POINT ( 'NONE',  ( -0.03443470937339728616, 0.2755905511811023723, -1.537015892239756099 ) ) ;
#38370 = VERTEX_POINT ( 'NONE', #15412 ) ;
#38371 = CARTESIAN_POINT ( 'NONE',  ( -0.2867679344610367109, 0.2867679344610365444, -2.063667609745093667 ) ) ;
#38372 = CARTESIAN_POINT ( 'NONE',  ( 0.4396325459317593221, 0.2952755905511810774, -0.1292274648535930714 ) ) ;
#38373 = VERTEX_POINT ( 'NONE', #41072 ) ;
#38374 = CIRCLE ( 'NONE', #36996, 0.1968503937007874405 ) ;
#38375 = CARTESIAN_POINT ( 'NONE',  ( -0.7152230971128602510, -0.05778040916215560624, -0.4822834645669293319 ) ) ;
#38376 = CARTESIAN_POINT ( 'NONE',  ( 1.410761154855643795, -0.3162353388693405765, 0.4822834645669290543 ) ) ;
#38377 = CARTESIAN_POINT ( 'NONE',  ( 0.6889763779527563470, 0.1660481256975883668, -0.3530559997133364547 ) ) ;
#38378 = CARTESIAN_POINT ( 'NONE',  ( 0.1968503937007881344, -0.6692913385826771977, 8.415575281601705876E-17 ) ) ;
#38379 = CARTESIAN_POINT ( 'NONE',  ( 4.797336870675656522E-17, -0.3917322834645670104, -1.265748031496062964 ) ) ;
#38380 = CARTESIAN_POINT ( 'NONE',  ( -0.7349081364829390672, 0.2306618581243847221, -0.2411417322834647770 ) ) ;
#38381 = CARTESIAN_POINT ( 'NONE',  ( -0.3346456692913377662, 0.1660481256975883668, -0.3530559997133364547 ) ) ;
#38382 = CARTESIAN_POINT ( 'NONE',  ( 0.07874015748031558404, -0.1870078740157479769, 0.3641732283464567677 ) ) ;
#38383 = CARTESIAN_POINT ( 'NONE',  ( -0.01987007963502784164, 0.3948464311378730440, -1.229201863956146261E-17 ) ) ;
#38384 = CARTESIAN_POINT ( 'NONE',  ( 0.05249343832021075018, 0.2306618581243847221, -0.2411417322834647770 ) ) ;
#38385 = CARTESIAN_POINT ( 'NONE',  ( 0.3503937007874015630, -0.3733313776025731778, -0.01968503937007957602 ) ) ;
#38386 = CARTESIAN_POINT ( 'NONE',  ( 0.9514435695538062676, -0.05778040916215522460, 0.4822834645669289988 ) ) ;
#38387 = CARTESIAN_POINT ( 'NONE',  ( 4.797336870675656522E-17, -0.3917322834645670104, -2.748031496062991685 ) ) ;
#38388 = ORIENTED_EDGE ( 'NONE', *, *, #58809, .T. ) ;
#38389 = ORIENTED_EDGE ( 'NONE', *, *, #29541, .F. ) ;
#38390 = CARTESIAN_POINT ( 'NONE',  ( 0.3477690288713918276, -0.6692913385826773087, -0.1292274648535924053 ) ) ;
#38391 = CARTESIAN_POINT ( 'NONE',  ( -0.4921259842519677963, -0.4536011799217367080, 0.2665933059059888421 ) ) ;
#38393 = CARTESIAN_POINT ( 'NONE',  ( -0.03443470937339728616, 0.2755905511811023723, -1.537015892239756099 ) ) ;
#38392 = CARTESIAN_POINT ( 'NONE',  ( 1.574803149606299746, -0.1870078740157480601, -0.3641732283464567677 ) ) ;
#38394 = CARTESIAN_POINT ( 'NONE',  ( 0.1958661417322834775, 0.3392501089628018884, -1.331364829396325611 ) ) ;
#38395 = CARTESIAN_POINT ( 'NONE',  ( 0.1265901696524989462, 0.4724409448818897572, -0.07020997375328083545 ) ) ;
#38396 = CARTESIAN_POINT ( 'NONE',  ( 1.443569553805774897, -0.5023911411419708095, -0.1820866141732282451 ) ) ;
#38397 = EDGE_CURVE ( 'NONE', #33221, #34136, #25301, .T. ) ;
#38398 = CARTESIAN_POINT ( 'NONE',  ( -1.450131233595799651, 0.2952755905511810774, -0.1292274648535930714 ) ) ;
#38399 = CARTESIAN_POINT ( 'NONE',  ( -0.2925321140481930149, -0.2925321140481933480, -2.812992125984251857 ) ) ;
#38400 = CARTESIAN_POINT ( 'NONE',  ( -0.1049868766404193215, 0.2306618581243847221, -0.2411417322834647770 ) ) ;
#38401 = CARTESIAN_POINT ( 'NONE',  ( -1.384514435695537005, -0.6692913385826773087, -0.1292274648535924053 ) ) ;
#38402 = CARTESIAN_POINT ( 'NONE',  ( -1.325459317585300889, -0.4281496062992127816, -0.4176697321401328100 ) ) ;
#38403 = CARTESIAN_POINT ( 'NONE',  ( 0.4199475065616803948, -0.6046776061558809534, -0.2411417322834644161 ) ) ;
#38404 = CARTESIAN_POINT ( 'NONE',  ( -0.2891555358219909388, -0.2891555358219912164, -0.1358267716535433156 ) ) ;
#38405 = CARTESIAN_POINT ( 'NONE',  ( 1.502624671916010790, -0.05778040916215522460, 0.4822834645669289988 ) ) ;
#38406 = CARTESIAN_POINT ( 'NONE',  ( 0.7808398950131240079, -0.3162353388693405765, 0.4822834645669290543 ) ) ;
#38407 = CARTESIAN_POINT ( 'NONE',  ( 1.253280839895013710, -0.08942795157528024563, -0.3641732283464568787 ) ) ;
#38408 = CARTESIAN_POINT ( 'NONE',  ( 0.6299212598425204535, -0.1870078740157480601, -0.3641732283464567677 ) ) ;
#38409 = CARTESIAN_POINT ( 'NONE',  ( -1.443569553805773564, 0.2306618581243847221, -0.2411417322834647770 ) ) ;
#38410 = CARTESIAN_POINT ( 'NONE',  ( 0.1998031496062992463, 0.3460692066303959202, -1.008530183727034180 ) ) ;
#38411 = CARTESIAN_POINT ( 'NONE',  ( 1.062992125984252745, 0.2952755905511811885, 0.000000000000000000 ) ) ;
#38412 = CARTESIAN_POINT ( 'NONE',  ( 0.2867679344610365999, -0.2867679344610365444, -0.2480314960629920740 ) ) ;
#38413 = CONICAL_SURFACE ( 'NONE', #14294, 2.637795275590551380, 0.7853981633974500554 ) ;
#38415 = CARTESIAN_POINT ( 'NONE',  ( -0.4732338166266092383, 1.502938029856535795, 2.167264197069282528 ) ) ;
#38414 = CARTESIAN_POINT ( 'NONE',  ( 0.5577427821522316087, -0.05778040916215522460, 0.4822834645669289988 ) ) ;
#38416 = CARTESIAN_POINT ( 'NONE',  ( 0.5314960629921324786, 2.716535433070866645, -1.854472803289050509 ) ) ;
#38417 = CARTESIAN_POINT ( 'NONE',  ( 0.1509186351706045259, -0.05778040916215560624, -0.4822834645669293319 ) ) ;
#38418 = CARTESIAN_POINT ( 'NONE',  ( 0.6233595800524939223, -0.2845877964562159024, 0.3641732283464567677 ) ) ;
#38419 = CARTESIAN_POINT ( 'NONE',  ( 1.003937007874016407, -0.5400638737290844871, 0.3530559997133364547 ) ) ;
#38420 = DIRECTION ( 'NONE',  ( 0.000000000000000000, -1.000000000000000000, 0.000000000000000000 ) ) ;
#38421 = CARTESIAN_POINT ( 'NONE',  ( -0.5971128608923877978, 0.1771653543307087630, 0.09757992244046791164 ) ) ;
#38422 = CARTESIAN_POINT ( 'NONE',  ( -0.5314960629921254842, -0.5400638737290845981, -0.3530559997133363437 ) ) ;
#38423 = CARTESIAN_POINT ( 'NONE',  ( 1.646981627296588035, -0.3162353388693405765, 0.4822834645669290543 ) ) ;
#38424 = CARTESIAN_POINT ( 'NONE',  ( -0.9448818897637790704, -0.1870078740157479769, 0.4822834645669291653 ) ) ;
#38425 = CARTESIAN_POINT ( 'NONE',  ( 0.9973753280839902091, -0.6046776061558807314, 0.2411417322834647770 ) ) ;
#38426 = CARTESIAN_POINT ( 'NONE',  ( -0.3392501089628019995, 0.1958661417322831999, -0.8103867698500807348 ) ) ;
#38427 = CARTESIAN_POINT ( 'NONE',  ( -1.548556430446193399, -0.5023911411419708095, -0.1820866141732282451 ) ) ;
#38428 = DIRECTION ( 'NONE',  ( 0.000000000000000000, 0.000000000000000000, -1.000000000000000000 ) ) ;
#38429 = CARTESIAN_POINT ( 'NONE',  ( 1.036745406824147508, -0.4281496062992127816, -0.4176697321401328100 ) ) ;
#38430 = CARTESIAN_POINT ( 'NONE',  ( -0.3458507752293909498, 0.3458507752293907833, -2.301181102362204633 ) ) ;
#38431 = CARTESIAN_POINT ( 'NONE',  ( -1.633858267716534529, -0.5400638737290845981, -0.3530559997133363437 ) ) ;
#38432 = CARTESIAN_POINT ( 'NONE',  ( -1.574803149606298192, -0.1870078740157480601, -0.3641732283464567677 ) ) ;
#38433 = CARTESIAN_POINT ( 'NONE',  ( -1.148293963254592542, -0.5511811023622048555, -0.09757992244046775898 ) ) ;
#38434 = CYLINDRICAL_SURFACE ( 'NONE', #31230, 0.4724409448818898682 ) ;
#38435 = CARTESIAN_POINT ( 'NONE',  ( -0.4068241469816264999, -0.4281496062992124485, 0.4176697321401328655 ) ) ;
#38436 = CARTESIAN_POINT ( 'NONE',  ( -0.4396325459317577122, -0.5511811023622048555, -0.09757992244046775898 ) ) ;
#38437 = CARTESIAN_POINT ( 'NONE',  ( -1.404199475065615932, -0.004921259842519576551, 0.3153832671262227771 ) ) ;
#38438 = CARTESIAN_POINT ( 'NONE',  ( 0.9908136482939640111, 0.1771653543307087075, -0.09757992244046823083 ) ) ;
#38439 = CARTESIAN_POINT ( 'NONE',  ( 0.3871391076115493490, -0.3162353388693405765, 0.4822834645669290543 ) ) ;
#38440 = FACE_OUTER_BOUND ( 'NONE', #12096, .T. ) ;
#38441 = CARTESIAN_POINT ( 'NONE',  ( -0.1509186351706028884, -0.2845877964562161244, -0.3641732283464567121 ) ) ;
#38442 = CARTESIAN_POINT ( 'NONE',  ( 0.3543307086614181922, -0.6692913385826771977, 8.415575281601705876E-17 ) ) ;
#38443 = CARTESIAN_POINT ( 'NONE',  ( 0.6955380577427828781, -0.004921259842519870586, -0.3153832671262229437 ) ) ;
#38444 = CARTESIAN_POINT ( 'NONE',  ( -1.627296587926508442, 0.2306618581243848609, 0.2411417322834645549 ) ) ;
#38445 = CARTESIAN_POINT ( 'NONE',  ( -1.115485564304461219, 0.05413385826771626580, -0.4176697321401330321 ) ) ;
#38446 = CARTESIAN_POINT ( 'NONE',  ( -0.6102362204724400829, 0.1660481256975885056, 0.3530559997133364547 ) ) ;
#38447 = CARTESIAN_POINT ( 'NONE',  ( -0.3996062992125986035, -7.340648628747425578E-17, -0.3543307086614173040 ) ) ;
#38448 = CARTESIAN_POINT ( 'NONE',  ( 0.3996062992125986035, -0.1070741851644052972, -2.708005249343832688 ) ) ;
#38449 = CARTESIAN_POINT ( 'NONE',  ( 0.4527559055118117182, -0.5400638737290844871, 0.3530559997133364547 ) ) ;
#38450 = CARTESIAN_POINT ( 'NONE',  ( 1.056430446194226436, -0.5511811023622048555, -0.09757992244046775898 ) ) ;
#38451 = CARTESIAN_POINT ( 'NONE',  ( -0.3937007874015740483, -0.1870078740157479769, 0.4822834645669291653 ) ) ;
#38452 = CARTESIAN_POINT ( 'NONE',  ( 0.3477690288713918276, 0.2952755905511811885, 0.1292274648535926551 ) ) ;
#38453 = CARTESIAN_POINT ( 'NONE',  ( -0.3996062992125987146, 0.1070741851644051862, -2.237532808398950301 ) ) ;
#38454 = CARTESIAN_POINT ( 'NONE',  ( -0.1974969037888703871, -0.3420746716998661063, -1.325459317585301777 ) ) ;
#38455 = CARTESIAN_POINT ( 'NONE',  ( -0.2925321140481930704, -0.2925321140481933480, -2.893700787401574992 ) ) ;
#38456 = CARTESIAN_POINT ( 'NONE',  ( 1.348312163386739426, 1.062992125984252079, 0.8371118098809627872 ) ) ;
#38457 = CARTESIAN_POINT ( 'NONE',  ( -0.3917322834645671215, 0.1049643490035301469, -0.9698162729658791337 ) ) ;
#38458 = CARTESIAN_POINT ( 'NONE',  ( -1.148293963254592542, -0.5511811023622048555, -0.09757992244046775898 ) ) ;
#38459 = CARTESIAN_POINT ( 'NONE',  ( -1.082677165354329896, 0.1660481256975885056, 0.3530559997133364547 ) ) ;
#38460 = CARTESIAN_POINT ( 'NONE',  ( 0.2891555358219910499, -0.2891555358219909944, -2.694881889763779625 ) ) ;
#38461 = CARTESIAN_POINT ( 'NONE',  ( 0.9973753280839902091, -0.6046776061558807314, 0.2411417322834647770 ) ) ;
#38462 = CARTESIAN_POINT ( 'NONE',  ( 1.489501312335958172, -0.05778040916215560624, -0.4822834645669293319 ) ) ;
#38463 = CARTESIAN_POINT ( 'NONE',  ( 0.5839895013123367340, -0.6692913385826773087, -0.1292274648535924053 ) ) ;
#38464 = CARTESIAN_POINT ( 'NONE',  ( -0.6188235755478027622, -3.724876541855331158E-15, 0.3954974714151467396 ) ) ;
#38465 = CIRCLE ( 'NONE', #33069, 0.3051181102362204856 ) ;
#38466 = CARTESIAN_POINT ( 'NONE',  ( -0.1070741851644051862, -0.3996062992125987146, -1.961942257217847763 ) ) ;
#38467 = CARTESIAN_POINT ( 'NONE',  ( 0.1049643490035304799, -0.3917322834645670104, -0.8694418879603171835 ) ) ;
#38468 = CARTESIAN_POINT ( 'NONE',  ( -0.7461015470515853787, 2.202998601811383850, 0.5309055118110236338 ) ) ;
#38469 = AXIS2_PLACEMENT_3D ( 'NONE', #30587, #11241, #24262 ) ;
#38470 = VECTOR ( 'NONE', #76874, 39.37007874015748143 ) ;
#38471 = CARTESIAN_POINT ( 'NONE',  ( 0.3543307086614179147, 0.2952755905511811885, 0.000000000000000000 ) ) ;
#38472 = CARTESIAN_POINT ( 'NONE',  ( 0.08530183727034192087, -0.3162353388693409650, -0.4822834645669289433 ) ) ;
#38473 = CARTESIAN_POINT ( 'NONE',  ( 0.7874015748031503170, -0.1870078740157479769, 0.3641732283464567677 ) ) ;
#38474 = CARTESIAN_POINT ( 'NONE',  ( 1.200787401574803681, 0.1660481256975885056, 0.3530559997133364547 ) ) ;
#38475 = CARTESIAN_POINT ( 'NONE',  ( -0.1958661417322836718, 0.3392501089628017219, -0.2552493438320210806 ) ) ;
#38476 = CARTESIAN_POINT ( 'NONE',  ( 0.6561679790026253567, 0.2306618581243848609, 0.2411417322834645549 ) ) ;
#38477 = CARTESIAN_POINT ( 'NONE',  ( 1.233595800524935227, 0.2306618581243847221, -0.2411417322834647770 ) ) ;
#38478 = CARTESIAN_POINT ( 'NONE',  ( 0.5183727034120741983, -0.6692913385826771977, 0.1292274648535927661 ) ) ;
#38479 = CARTESIAN_POINT ( 'NONE',  ( 1.332020997375329197, -0.2845877964562159024, 0.3641732283464567677 ) ) ;
#38480 = CARTESIAN_POINT ( 'NONE',  ( -0.9842519685039365918, -0.6692913385826771977, 8.415575281601705876E-17 ) ) ;
#38481 = CARTESIAN_POINT ( 'NONE',  ( -0.8858267716535425107, 0.1660481256975883668, -0.3530559997133364547 ) ) ;
#38482 = CARTESIAN_POINT ( 'NONE',  ( 1.233595800524935227, -0.6046776061558807314, 0.2411417322834647770 ) ) ;
#38483 = CARTESIAN_POINT ( 'NONE',  ( -0.3392501089628019995, 0.1958661417322832277, -0.7408136482939633449 ) ) ;
#38484 = CARTESIAN_POINT ( 'NONE',  ( -0.3917322834645669549, -0.1049643490035306603, -1.455380577427821676 ) ) ;
#38485 = CARTESIAN_POINT ( 'NONE',  ( 0.1049643490035304938, -0.3917322834645669549, -2.754593175853017328 ) ) ;
#38486 = VERTEX_POINT ( 'NONE', #1533 ) ;
#38487 = CARTESIAN_POINT ( 'NONE',  ( 0.3996062992125986035, 0.1070741851644054776, 0.03280839895013121232 ) ) ;
#38488 = ORIENTED_EDGE ( 'NONE', *, *, #56663, .F. ) ;
#38489 = CARTESIAN_POINT ( 'NONE',  ( 1.456692913385827515, -0.6692913385826771977, 8.415575281601705876E-17 ) ) ;
#38490 = AXIS2_PLACEMENT_3D ( 'NONE', #58380, #26398, #13367 ) ;
#38491 = CARTESIAN_POINT ( 'NONE',  ( 1.010498687664042716, -0.004921259842519870586, -0.3153832671262229437 ) ) ;
#38492 = CARTESIAN_POINT ( 'NONE',  ( 0.1998031496062992740, 0.3460692066303959757, -1.561679790026246684 ) ) ;
#38493 = CARTESIAN_POINT ( 'NONE',  ( 1.266404199475066328, -0.2845877964562161244, -0.3641732283464567121 ) ) ;
#38494 = DIRECTION ( 'NONE',  ( 0.000000000000000000, 1.000000000000000000, 0.000000000000000000 ) ) ;
#38495 = CARTESIAN_POINT ( 'NONE',  ( -0.1115485564304456445, 0.2952755905511810219, -0.1292274648535930437 ) ) ;
#38496 = DIRECTION ( 'NONE',  ( 0.000000000000000000, 0.4999999999999997224, 0.8660254037844388186 ) ) ;
#38497 = CARTESIAN_POINT ( 'NONE',  ( 0.3917322834645669549, 0.1049643490035304660, -0.6817585301837268963 ) ) ;
#38498 = EDGE_CURVE ( 'NONE', #29599, #44548, #6210, .T. ) ;
#38499 = CARTESIAN_POINT ( 'NONE',  ( -0.7020997375328074108, -0.08942795157527998196, 0.3641732283464567121 ) ) ;
#38500 = CARTESIAN_POINT ( 'NONE',  ( -1.555118110236219930, 0.07958543189024085140, 0.2665933059059887866 ) ) ;
#38501 = CARTESIAN_POINT ( 'NONE',  ( -1.220472440944881054, -0.6692913385826771977, 8.415575281601705876E-17 ) ) ;
#38502 = CARTESIAN_POINT ( 'NONE',  ( 0.1443569553805781891, -0.4281496062992124485, 0.4176697321401328655 ) ) ;
#38503 = CARTESIAN_POINT ( 'NONE',  ( 1.581364829396326277, -0.05778040916215522460, 0.4822834645669289988 ) ) ;
#38504 = ORIENTED_EDGE ( 'NONE', *, *, #40133, .T. ) ;
#38505 = CARTESIAN_POINT ( 'NONE',  ( -1.609562092802257816, 0.2869345716361978438, 0.09226303723660828071 ) ) ;
#38506 = DIRECTION ( 'NONE',  ( 6.123233995736767268E-17, 1.000000000000000000, -9.948661822761038443E-18 ) ) ;
#38507 = CARTESIAN_POINT ( 'NONE',  ( -0.4091458600556402980, -0.2362204724409451284, -1.942257217847769057 ) ) ;
#38508 = DIRECTION ( 'NONE',  ( 0.000000000000000000, 0.000000000000000000, 1.000000000000000000 ) ) ;
#38509 = CARTESIAN_POINT ( 'NONE',  ( -0.2952755905511803003, -0.4536011799217368745, -0.2665933059059886201 ) ) ;
#38510 = CARTESIAN_POINT ( 'NONE',  ( -1.187664041994749731, -0.3162353388693405765, 0.4822834645669290543 ) ) ;
#38511 = CARTESIAN_POINT ( 'NONE',  ( 0.8858267716535438430, 0.1660481256975885056, 0.3530559997133364547 ) ) ;
#38512 = ORIENTED_EDGE ( 'NONE', *, *, #7858, .F. ) ;
#38514 = CARTESIAN_POINT ( 'NONE',  ( -1.646051170424378096, -0.1870078740157480046, 1.254653134982923898E-17 ) ) ;
#38513 = CARTESIAN_POINT ( 'NONE',  ( -1.603475055217291612, 0.5037964761735302943, -0.04573490813648262154 ) ) ;
#38515 = CARTESIAN_POINT ( 'NONE',  ( 1.023622047244095334, -0.1870078740157479769, 0.4822834645669291653 ) ) ;
#38516 = CARTESIAN_POINT ( 'NONE',  ( -1.233595800524933894, 0.2306618581243848609, 0.2411417322834645549 ) ) ;
#38517 = CARTESIAN_POINT ( 'NONE',  ( -0.3917322834645670659, 0.1049643490035301607, -0.7427628364491322133 ) ) ;
#38518 = CARTESIAN_POINT ( 'NONE',  ( -0.4265091863517051496, 0.1771653543307087075, -0.09757992244046823083 ) ) ;
#38519 = CARTESIAN_POINT ( 'NONE',  ( -0.3392501089628019995, 0.1958661417322832277, -0.7408136482939633449 ) ) ;
#38520 = CARTESIAN_POINT ( 'NONE',  ( -0.4330708661417315697, -0.5511811023622047445, 6.969142054262312111E-17 ) ) ;
#38521 = CARTESIAN_POINT ( 'NONE',  ( 0.1706036745406830368, -0.004921259842519576551, 0.3153832671262227771 ) ) ;
#38522 = CARTESIAN_POINT ( 'NONE',  ( 0.1312335958005255154, -0.6046776061558807314, 0.2411417322834647770 ) ) ;
#38523 = CARTESIAN_POINT ( 'NONE',  ( -0.9711286089238838626, 0.1283753931104746893, -0.1820866141732285504 ) ) ;
#38524 = CARTESIAN_POINT ( 'NONE',  ( 0.1049643490035303689, 0.3917322834645670104, -2.820209973753280419 ) ) ;
#38525 = CARTESIAN_POINT ( 'NONE',  ( 1.272965879265092637, 0.05413385826771666132, 0.4176697321401328100 ) ) ;
#38526 = AXIS2_PLACEMENT_3D ( 'NONE', #30032, #42245, #22487 ) ;
#38527 = CARTESIAN_POINT ( 'NONE',  ( -1.410761154855641575, -0.3162353388693409650, -0.4822834645669289433 ) ) ;
#38528 = AXIS2_PLACEMENT_3D ( 'NONE', #52236, #2582, #53491 ) ;
#38529 = CARTESIAN_POINT ( 'NONE',  ( 0.2362204724409449064, 0.4091458600556404646, -1.166010498687663821 ) ) ;
#38530 = CARTESIAN_POINT ( 'NONE',  ( -0.5118110236220466680, -0.6692913385826771977, 8.415575281601705876E-17 ) ) ;
#38531 = CARTESIAN_POINT ( 'NONE',  ( -0.9842519685039360366, 0.2952755905511811885, 0.000000000000000000 ) ) ;
#38532 = CARTESIAN_POINT ( 'NONE',  ( 0.6364829396325465405, -0.2845877964562161244, -0.3641732283464567121 ) ) ;
#38533 = CARTESIAN_POINT ( 'NONE',  ( -0.4921259842519677963, -0.4536011799217367080, 0.2665933059059888421 ) ) ;
#38534 = CARTESIAN_POINT ( 'NONE',  ( -0.5511811023622041894, -0.1870078740157480879, -0.4822834645669291653 ) ) ;
#38535 = CARTESIAN_POINT ( 'NONE',  ( -0.9908136482939626788, 0.2952755905511811885, 0.1292274648535926551 ) ) ;
#38536 = CARTESIAN_POINT ( 'NONE',  ( 0.000000000000000000, 0.4177165354330708569, 0.000000000000000000 ) ) ;
#38537 = CARTESIAN_POINT ( 'NONE',  ( 1.122047244094488860, -0.4536011799217368745, -0.2665933059059886201 ) ) ;
#38538 = PRODUCT ( 'MAS-416', 'MAS-416', '', ( #64600 ) ) ;
#38539 = CARTESIAN_POINT ( 'NONE',  ( -0.1574803149606292529, -0.1870078740157480879, -0.4822834645669291653 ) ) ;
#38540 = CARTESIAN_POINT ( 'NONE',  ( -1.391076115485563758, 0.2306618581243848609, 0.2411417322834645549 ) ) ;
#38541 = ORIENTED_EDGE ( 'NONE', *, *, #2416, .F. ) ;
#38542 = CARTESIAN_POINT ( 'NONE',  ( 0.3460692066303959202, -0.1998031496062991630, -2.543963254593176071 ) ) ;
#38543 = CARTESIAN_POINT ( 'NONE',  ( -1.003937007874014853, 0.07958543189024085140, 0.2665933059059887866 ) ) ;
#38544 = CARTESIAN_POINT ( 'NONE',  ( 0.8923884514435701520, -0.6046776061558809534, -0.2411417322834644161 ) ) ;
#38545 = CARTESIAN_POINT ( 'NONE',  ( -0.9711286089238838626, -0.5023911411419708095, 0.1820866141732285504 ) ) ;
#38546 = CARTESIAN_POINT ( 'NONE',  ( 0.3996062992125984925, 0.1070741851644054637, -1.303805774278215202 ) ) ;
#38547 = CARTESIAN_POINT ( 'NONE',  ( -0.8661417322834640276, -0.1870078740157480879, -0.4822834645669291653 ) ) ;
#38548 = CARTESIAN_POINT ( 'NONE',  ( 0.7283464566929143125, 0.1660481256975885056, 0.3530559997133364547 ) ) ;
#38549 = CARTESIAN_POINT ( 'NONE',  ( 0.6758530183727039509, -0.6692913385826771977, 0.1292274648535927661 ) ) ;
#38550 = CARTESIAN_POINT ( 'NONE',  ( 1.568241469816273437, -0.3162353388693405765, 0.4822834645669290543 ) ) ;
#38551 = CARTESIAN_POINT ( 'NONE',  ( -1.482939632545930975, -0.3690944881889765550, -0.3153832671262227771 ) ) ;
#38552 = CARTESIAN_POINT ( 'NONE',  ( -0.1070741851644057135, 0.3996062992125984925, -0.5557742782152230721 ) ) ;
#38553 = CARTESIAN_POINT ( 'NONE',  ( 0.2925321140481932369, -0.2925321140481932369, -1.043307086614173151 ) ) ;
#38554 = CARTESIAN_POINT ( 'NONE',  ( 0.3949938075777411073, -0.1058382717557499464, -0.1115485564304462551 ) ) ;
#38555 = CARTESIAN_POINT ( 'NONE',  ( -0.1938976377952756625, 0.1938976377952755792, 0.07874015748031495954 ) ) ;
#38556 = CARTESIAN_POINT ( 'NONE',  ( 1.062992125984252745, 0.1771653543307087630, 0.000000000000000000 ) ) ;
#38557 = CARTESIAN_POINT ( 'NONE',  ( 0.4396325459317590445, -0.5511811023622046335, 0.09757992244046803654 ) ) ;
#38558 = CARTESIAN_POINT ( 'NONE',  ( 0.09842519685039434474, -0.5400638737290845981, -0.3530559997133363437 ) ) ;
#38559 = CARTESIAN_POINT ( 'NONE',  ( 1.325459317585302665, 0.05413385826771626580, -0.4176697321401330321 ) ) ;
#38560 = CARTESIAN_POINT ( 'NONE',  ( -0.3949938075777411073, 0.1058382717557497660, -1.526902887139107934 ) ) ;
#38561 = CARTESIAN_POINT ( 'NONE',  ( 0.4396325459317593221, 0.1771653543307087075, -0.09757992244046823083 ) ) ;
#38562 = CARTESIAN_POINT ( 'NONE',  ( -0.5905511811023613777, -0.6692913385826771977, 8.415575281601705876E-17 ) ) ;
#38563 = CARTESIAN_POINT ( 'NONE',  ( -1.312335958005248715, 0.2306618581243848609, 0.2411417322834645549 ) ) ;
#38564 = CARTESIAN_POINT ( 'NONE',  ( 0.8005249343832028242, -0.4281496062992127816, -0.4176697321401328100 ) ) ;
#38565 = CARTESIAN_POINT ( 'NONE',  ( 0.3458507752293908943, -0.3458507752293908943, -1.673228346456692828 ) ) ;
#38566 = CARTESIAN_POINT ( 'NONE',  ( -0.3460692066303958092, -0.1998031496062994683, -2.729658792650918375 ) ) ;
#38567 = VERTEX_POINT ( 'NONE', #27187 ) ;
#38568 = ORIENTED_EDGE ( 'NONE', *, *, #10106, .T. ) ;
#38569 = CARTESIAN_POINT ( 'NONE',  ( -1.384514435695537005, 0.2952755905511811885, 0.1292274648535926551 ) ) ;
#38570 = CARTESIAN_POINT ( 'NONE',  ( -0.6102362204724400829, -0.5400638737290845981, -0.3530559997133363437 ) ) ;
#38572 = CARTESIAN_POINT ( 'NONE',  ( -0.7677165354330699465, -0.5400638737290845981, -0.3530559997133363437 ) ) ;
#38571 = CARTESIAN_POINT ( 'NONE',  ( -0.5905511811023613777, -0.5511811023622047445, 6.969142054262312111E-17 ) ) ;
#38573 = CARTESIAN_POINT ( 'NONE',  ( -0.3917322834645670659, 0.1049643490035301607, -2.160085671094801540 ) ) ;
#38574 = CARTESIAN_POINT ( 'NONE',  ( 0.1133856558944468795, -0.2726377952755905665, 0.1574803149606299191 ) ) ;
#38575 = CARTESIAN_POINT ( 'NONE',  ( -1.587926509186350810, -0.004921259842519870586, -0.3153832671262229437 ) ) ;
#38576 = CARTESIAN_POINT ( 'NONE',  ( -1.332020997375327642, -0.3162353388693409650, -0.4822834645669289433 ) ) ;
#38577 = CARTESIAN_POINT ( 'NONE',  ( 0.2690288713910767848, -0.6692913385826773087, -0.1292274648535924053 ) ) ;
#38578 = CARTESIAN_POINT ( 'NONE',  ( -0.9580052493438311334, 0.05413385826771626580, -0.4176697321401330321 ) ) ;
#38579 = VECTOR ( 'NONE', #58552, 39.37007874015748143 ) ;
#38580 = EDGE_CURVE ( 'NONE', #45100, #27310, #79389, .T. ) ;
#38581 = CARTESIAN_POINT ( 'NONE',  ( -0.3392501089628019995, 0.1958661417322832277, -1.435695538057742970 ) ) ;
#38582 = CARTESIAN_POINT ( 'NONE',  ( -0.9448818897637790704, -0.1870078740157480601, -0.3641732283464567677 ) ) ;
#38583 = ORIENTED_EDGE ( 'NONE', *, *, #30705, .F. ) ;
#38584 = CARTESIAN_POINT ( 'NONE',  ( 0.1974969037888706369, -0.3420746716998659953, -1.824146981627296382 ) ) ;
#38585 = VECTOR ( 'NONE', #63981, 39.37007874015748143 ) ;
#38586 = ORIENTED_EDGE ( 'NONE', *, *, #9419, .T. ) ;
#38587 = CARTESIAN_POINT ( 'NONE',  ( 0.9348729704079946634, -8.644661201599092366E-16, -0.4445507791589066171 ) ) ;
#38588 = CARTESIAN_POINT ( 'NONE',  ( -1.115485564304461219, 0.05413385826771626580, -0.4176697321401330321 ) ) ;
#38589 = CARTESIAN_POINT ( 'NONE',  ( -0.8858267716535425107, -0.5400638737290844871, 0.3530559997133364547 ) ) ;
#38590 = CARTESIAN_POINT ( 'NONE',  ( -9.787531504996567848E-17, 0.3996062992125986035, -8.919671568592925241E-18 ) ) ;
#38591 = CARTESIAN_POINT ( 'NONE',  ( -1.115485564304461219, -0.4281496062992124485, 0.4176697321401328655 ) ) ;
#38592 = CARTESIAN_POINT ( 'NONE',  ( -1.253280839895012377, -0.05778040916215522460, 0.4822834645669289988 ) ) ;
#38593 = CARTESIAN_POINT ( 'NONE',  ( 3.937007874015748143, 2.755905511811024056, 0.5314960629921260393 ) ) ;
#38594 = CARTESIAN_POINT ( 'NONE',  ( 0.5643044619422579178, -0.004921259842519576551, 0.3153832671262227771 ) ) ;
#38595 = CARTESIAN_POINT ( 'NONE',  ( -1.646051170424378096, -0.1870078740157480046, 1.254653134982923898E-17 ) ) ;
#38596 = CARTESIAN_POINT ( 'NONE',  ( 0.3917322834645669549, 0.1049643490035304660, -0.5242782152230972548 ) ) ;
#38597 = CARTESIAN_POINT ( 'NONE',  ( -0.3871391076115479057, -0.2845877964562161244, -0.3641732283464567121 ) ) ;
#38598 = CARTESIAN_POINT ( 'NONE',  ( -0.9448818897637790704, -0.1870078740157480879, -0.4822834645669291653 ) ) ;
#38599 = CARTESIAN_POINT ( 'NONE',  ( 1.443569553805774897, 0.2306618581243848609, 0.2411417322834645549 ) ) ;
#38600 = CARTESIAN_POINT ( 'NONE',  ( -0.6102362204724400829, -0.5400638737290845981, -0.3530559997133363437 ) ) ;
#38601 = EDGE_LOOP ( 'NONE', ( #24087, #21076, #33312 ) ) ;
#38602 = ORIENTED_EDGE ( 'NONE', *, *, #72224, .T. ) ;
#38603 = CARTESIAN_POINT ( 'NONE',  ( -0.3996062992125984925, -0.1070741851644056858, -2.012467191601049699 ) ) ;
#38604 = CARTESIAN_POINT ( 'NONE',  ( -1.049868766404198794, -0.6046776061558807314, 0.2411417322834647770 ) ) ;
#38605 = CARTESIAN_POINT ( 'NONE',  ( 1.194225721784777594, -0.4281496062992127816, -0.4176697321401328100 ) ) ;
#38606 = CARTESIAN_POINT ( 'NONE',  ( -0.9383202099737524282, -0.08942795157527998196, 0.3641732283464567121 ) ) ;
#38607 = CARTESIAN_POINT ( 'NONE',  ( -1.574803149606298636, -0.1870078740157479769, 0.4822834645669291653 ) ) ;
#38608 = CARTESIAN_POINT ( 'NONE',  ( 0.1265901696524990294, -0.4724409448818896462, -1.030183727034120533 ) ) ;
#38609 = CARTESIAN_POINT ( 'NONE',  ( 2.001206130748399925, 1.231544801320224369, 0.3638227417423782195 ) ) ;
#38610 = CARTESIAN_POINT ( 'NONE',  ( -0.2867679344610364334, -0.2867679344610367109, -0.2086614173228345248 ) ) ;
#38611 = CARTESIAN_POINT ( 'NONE',  ( -0.4724409448818898682, 5.785732909357575061E-17, -2.755905511811024056 ) ) ;
#38612 = CARTESIAN_POINT ( 'NONE',  ( 0.03937007874015833325, -0.6692913385826771977, 8.415575281601705876E-17 ) ) ;
#38613 = CARTESIAN_POINT ( 'NONE',  ( -0.8727034120734901146, -0.2845877964562159024, 0.3641732283464567677 ) ) ;
#38614 = CARTESIAN_POINT ( 'NONE',  ( -0.7611548556430438595, 0.2306618581243848609, 0.2411417322834645549 ) ) ;
#38615 = CARTESIAN_POINT ( 'NONE',  ( 0.4724409448818898682, 2.892866454678787531E-17, -2.872047244094488416 ) ) ;
#38616 = CARTESIAN_POINT ( 'NONE',  ( -1.135170603674539924, -0.6692913385826771977, 0.1292274648535927661 ) ) ;
#38617 = CARTESIAN_POINT ( 'NONE',  ( -0.9645669291338575535, -0.5400638737290844871, 0.3530559997133364547 ) ) ;
#38618 = CARTESIAN_POINT ( 'NONE',  ( -0.04593175853018302557, -0.6692913385826773087, -0.1292274648535924053 ) ) ;
#38619 = CARTESIAN_POINT ( 'NONE',  ( -0.1058382717557503072, 0.3949938075777408852, -2.603018372703412187 ) ) ;
#38620 = CARTESIAN_POINT ( 'NONE',  ( 0.9973753280839902091, 0.1283753931104746893, -0.1820866141732285504 ) ) ;
#38621 = CARTESIAN_POINT ( 'NONE',  ( -0.5905511811023615998, 0.1771653543307087630, 0.000000000000000000 ) ) ;
#38622 = CARTESIAN_POINT ( 'NONE',  ( -0.09709680097443590396, 1.072984620235833075, -1.483320890666278480 ) ) ;
#38623 = CARTESIAN_POINT ( 'NONE',  ( 0.5905511811023629321, 0.1771653543307087630, 0.000000000000000000 ) ) ;
#38624 = CARTESIAN_POINT ( 'NONE',  ( 1.154855643044620184, 0.1283753931104746893, -0.1820866141732285504 ) ) ;
#38625 = CARTESIAN_POINT ( 'NONE',  ( 1.377952755905512472, -0.6692913385826771977, 8.415575281601705876E-17 ) ) ;
#38626 = CARTESIAN_POINT ( 'NONE',  ( 0.4199475065616805614, 0.1283753931104748280, 0.1820866141732283561 ) ) ;
#38627 = CARTESIAN_POINT ( 'NONE',  ( -0.2867679344610364334, -0.2867679344610367109, -1.311023622047244430 ) ) ;
#38628 = CARTESIAN_POINT ( 'NONE',  ( -0.9514435695538050464, -0.05778040916215560624, -0.4822834645669293319 ) ) ;
#38629 = CARTESIAN_POINT ( 'NONE',  ( 1.259842519685040019, -0.1870078740157479769, 0.4822834645669291653 ) ) ;
#38630 = CARTESIAN_POINT ( 'NONE',  ( -0.2362204724409447953, -0.4091458600556404646, -0.1423884514435695414 ) ) ;
#38631 = CARTESIAN_POINT ( 'NONE',  ( -0.4986876640419939388, 0.1283753931104746893, -0.1820866141732285504 ) ) ;
#38632 = CARTESIAN_POINT ( 'NONE',  ( -0.7137454485294950635, 2.362204724409448620, -0.4917280318828581298 ) ) ;
#38633 = CARTESIAN_POINT ( 'NONE',  ( 0.3740157480314966754, -0.5400638737290844871, 0.3530559997133364547 ) ) ;
#38634 = CARTESIAN_POINT ( 'NONE',  ( 0.2362204724409449064, 2.410722045565656378E-17, -0.1968503937007874405 ) ) ;
#38635 = CARTESIAN_POINT ( 'NONE',  ( 1.023622047244095112, -0.1870078740157480601, -0.3641732283464567677 ) ) ;
#38636 = CARTESIAN_POINT ( 'NONE',  ( 0.2296587926509192634, -0.08942795157528024563, -0.3641732283464568787 ) ) ;
#38637 = CARTESIAN_POINT ( 'NONE',  ( 0.1049868766404206816, 0.2306618581243848609, 0.2411417322834645549 ) ) ;
#38638 = CARTESIAN_POINT ( 'NONE',  ( -1.568241469816272105, -0.05778040916215522460, 0.4822834645669289988 ) ) ;
#38639 = CARTESIAN_POINT ( 'NONE',  ( -0.7414698162729651543, -0.5511811023622046335, 0.09757992244046803654 ) ) ;
#38640 = CYLINDRICAL_SURFACE ( 'NONE', #36747, 0.3937007874015748254 ) ;
#38641 = CARTESIAN_POINT ( 'NONE',  ( -0.4133858267716528645, -0.5400638737290844871, 0.3530559997133364547 ) ) ;
#38642 = CARTESIAN_POINT ( 'NONE',  ( 0.3460692066303958092, 0.1998031496062993018, -0.9954068241469815614 ) ) ;
#38643 = CARTESIAN_POINT ( 'NONE',  ( -0.3917322834645671215, 0.1049643490035301469, -2.479658792650918375 ) ) ;
#38644 = CARTESIAN_POINT ( 'NONE',  ( 0.3412073490813655186, 0.1283753931104748280, 0.1820866141732283561 ) ) ;
#38646 = AXIS2_PLACEMENT_3D ( 'NONE', #13126, #32047, #7648 ) ;
#38645 = CARTESIAN_POINT ( 'NONE',  ( -0.9580052493438311334, 0.05413385826771626580, -0.4176697321401330321 ) ) ;
#38647 = CARTESIAN_POINT ( 'NONE',  ( -1.030183727034119867, -0.3162353388693405765, 0.4822834645669290543 ) ) ;
#38648 = CARTESIAN_POINT ( 'NONE',  ( -1.325459317585300889, -0.004921259842519576551, 0.3153832671262227771 ) ) ;
#38649 = DIRECTION ( 'NONE',  ( -1.000000000000000000, 0.000000000000000000, 0.000000000000000000 ) ) ;
#38650 = CARTESIAN_POINT ( 'NONE',  ( -0.5052493438320203589, 0.2952755905511810774, -0.1292274648535930714 ) ) ;
#38651 = CARTESIAN_POINT ( 'NONE',  ( -0.7742782152230962556, -0.3690944881889765550, -0.3153832671262227771 ) ) ;
#38652 = CARTESIAN_POINT ( 'NONE',  ( -1.706036745406823485, 0.1283753931104748280, 0.1820866141732283561 ) ) ;
#38653 = CARTESIAN_POINT ( 'NONE',  ( 1.469816272965879911, 0.2306618581243847221, -0.2411417322834647770 ) ) ;
#38654 = CARTESIAN_POINT ( 'NONE',  ( -0.4744094488189005143, 1.537401574803149984, 1.016821367227982220 ) ) ;
#38655 = CARTESIAN_POINT ( 'NONE',  ( -0.2867679344610365444, -0.2867679344610367664, -2.103037688485251522 ) ) ;
#38656 = VERTEX_POINT ( 'NONE', #14169 ) ;
#38657 = CARTESIAN_POINT ( 'NONE',  ( 0.4061203303035133549, 3.421639014772782816E-16, 0.3464511005275203726 ) ) ;
#38658 = CARTESIAN_POINT ( 'NONE',  ( -1.292650918635170010, -0.6692913385826771977, 0.1292274648535927661 ) ) ;
#38659 = CARTESIAN_POINT ( 'NONE',  ( -0.8398950131233589023, -0.6046776061558809534, -0.2411417322834644161 ) ) ;
#38660 = CARTESIAN_POINT ( 'NONE',  ( -1.548556430446193399, -0.6046776061558809534, -0.2411417322834644161 ) ) ;
#38661 = CARTESIAN_POINT ( 'NONE',  ( -0.3917322834645669549, -0.1049643490035306603, -2.177821522309711266 ) ) ;
#38662 = CARTESIAN_POINT ( 'NONE',  ( 1.443569553805774897, -0.5023911411419708095, -0.1820866141732282451 ) ) ;
#38663 = CARTESIAN_POINT ( 'NONE',  ( 0.6758530183727039509, -0.6692913385826771977, 0.1292274648535927661 ) ) ;
#38664 = CARTESIAN_POINT ( 'NONE',  ( -0.07874015748031421014, -0.1870078740157479769, 0.4822834645669291653 ) ) ;
#38665 = CARTESIAN_POINT ( 'NONE',  ( -0.3492006680983059108, -0.3045572308828553565, -0.01849200668098333403 ) ) ;
#38666 = CARTESIAN_POINT ( 'NONE',  ( 1.614173228346456712, 2.401574803149606474, 0.1372047244094478646 ) ) ;
#38667 = CARTESIAN_POINT ( 'NONE',  ( 0.7020997375328090762, -0.08942795157528024563, -0.3641732283464568787 ) ) ;
#38668 = CARTESIAN_POINT ( 'NONE',  ( 0.1998031496062994405, -0.3460692066303958092, -1.351706036745406792 ) ) ;
#38669 = ORIENTED_EDGE ( 'NONE', *, *, #61343, .T. ) ;
#38670 = CARTESIAN_POINT ( 'NONE',  ( -0.3392501089628017219, -0.1958661417322836995, 0.1082484007535938902 ) ) ;
#38671 = ORIENTED_EDGE ( 'NONE', *, *, #53241, .T. ) ;
#38672 = CARTESIAN_POINT ( 'NONE',  ( -0.1115485564304456306, 0.2952755905511810774, -0.1292274648535930714 ) ) ;
#38673 = CARTESIAN_POINT ( 'NONE',  ( -0.8464566929133852113, -0.5400638737290845981, -0.3530559997133363437 ) ) ;
#38674 = CARTESIAN_POINT ( 'NONE',  ( -1.620734908136482577, 0.2952755905511811885, 0.1292274648535926551 ) ) ;
#38675 = CARTESIAN_POINT ( 'NONE',  ( 0.6496062992125991586, -0.5400638737290845981, -0.3530559997133363437 ) ) ;
#38676 = CARTESIAN_POINT ( 'NONE',  ( -1.594488188976377119, 0.07958543189024071263, -0.2665933059059888421 ) ) ;
#38677 = CARTESIAN_POINT ( 'NONE',  ( 1.332020997375328974, -0.05778040916215560624, -0.4822834645669293319 ) ) ;
#38678 = CARTESIAN_POINT ( 'NONE',  ( -0.5052493438320203589, 0.2952755905511810774, -0.1292274648535930714 ) ) ;
#38679 = CARTESIAN_POINT ( 'NONE',  ( 0.6299212598425204535, -0.1870078740157479769, 0.4822834645669291653 ) ) ;
#38680 = CARTESIAN_POINT ( 'NONE',  ( 1.581364829396326277, -0.05778040916215522460, 0.4822834645669289988 ) ) ;
#38681 = CARTESIAN_POINT ( 'NONE',  ( 1.115485564304462551, 0.05413385826771666132, 0.4176697321401328100 ) ) ;
#38682 = CARTESIAN_POINT ( 'NONE',  ( 0.4698620426710066744, 1.469755830210690117, -2.565186897544956324 ) ) ;
#38683 = CARTESIAN_POINT ( 'NONE',  ( -0.2034120734908131112, -0.6692913385826773087, -0.1292274648535924053 ) ) ;
#38684 = CARTESIAN_POINT ( 'NONE',  ( 0.1049643490035303689, 0.3917322834645670104, 0.01443569553805778768 ) ) ;
#38685 = CARTESIAN_POINT ( 'NONE',  ( 0.3215223097112867578, -0.2845877964562161244, -0.3641732283464567121 ) ) ;
#38686 = ORIENTED_EDGE ( 'NONE', *, *, #74544, .T. ) ;
#38687 = CARTESIAN_POINT ( 'NONE',  ( -0.2891555358219911054, 0.2891555358219909388, -0.4921259842519685179 ) ) ;
#38688 = ORIENTED_EDGE ( 'NONE', *, *, #79768, .T. ) ;
#38689 = CARTESIAN_POINT ( 'NONE',  ( -0.4986876640419942164, -0.5023911411419708095, 0.1820866141732285504 ) ) ;
#38690 = FACE_OUTER_BOUND ( 'NONE', #30930, .T. ) ;
#38691 = CARTESIAN_POINT ( 'NONE',  ( 0.1771653543307093182, 0.1660481256975885056, 0.3530559997133364547 ) ) ;
#38692 = CARTESIAN_POINT ( 'NONE',  ( 0.1377952755905518800, -0.5400638737290844871, 0.3530559997133364547 ) ) ;
#38693 = CARTESIAN_POINT ( 'NONE',  ( -0.8070866141732276899, -0.5400638737290844871, 0.3530559997133364547 ) ) ;
#38694 = CARTESIAN_POINT ( 'NONE',  ( 0.3392501089628018884, -0.1958661417322833942, -1.834008817094174848 ) ) ;
#38695 = CARTESIAN_POINT ( 'NONE',  ( -1.194225721784776262, -0.4281496062992124485, 0.4176697321401328655 ) ) ;
#38696 = CARTESIAN_POINT ( 'NONE',  ( -0.1341536278048623410, 1.446850393700787274, 0.2827841492639507903 ) ) ;
#38697 = CARTESIAN_POINT ( 'NONE',  ( 0.7742782152230978099, -0.3690944881889763329, 0.3153832671262228327 ) ) ;
#38698 = CARTESIAN_POINT ( 'NONE',  ( 0.3674540682414705883, -0.6046776061558807314, 0.2411417322834647770 ) ) ;
#38699 = CARTESIAN_POINT ( 'NONE',  ( 0.7742782152230979209, 0.05413385826771626580, -0.4176697321401330321 ) ) ;
#38700 = CARTESIAN_POINT ( 'NONE',  ( 0.1070741851644053527, 0.3996062992125986590, -1.253280839895013044 ) ) ;
#38701 = CARTESIAN_POINT ( 'NONE',  ( -1.725721784776902190, -0.05778040916215522460, 0.4822834645669289988 ) ) ;
#38702 = CARTESIAN_POINT ( 'NONE',  ( 0.1070741851644054776, -0.3996062992125984925, -0.6345144356955381149 ) ) ;
#38703 = CARTESIAN_POINT ( 'NONE',  ( -0.3996062992125985480, -7.340648628747423112E-17, -0.1161417322834645965 ) ) ;
#38704 = CARTESIAN_POINT ( 'NONE',  ( -0.2230971128608915943, -0.4281496062992127816, -0.4176697321401328100 ) ) ;
#38705 = CARTESIAN_POINT ( 'NONE',  ( -0.2925321140481930704, -0.2925321140481933480, -2.736220472440944018 ) ) ;
#38706 = CARTESIAN_POINT ( 'NONE',  ( -9.594673741351313045E-17, 0.3917322834645670104, -1.501968503937008093 ) ) ;
#38707 = CARTESIAN_POINT ( 'NONE',  ( -1.312335958005248715, 0.1283753931104748280, 0.1820866141732283561 ) ) ;
#38708 = CARTESIAN_POINT ( 'NONE',  ( 1.161417322834646271, 0.1660481256975883668, -0.3530559997133364547 ) ) ;
#38709 = VECTOR ( 'NONE', #34010, 39.37007874015748143 ) ;
#38710 = CARTESIAN_POINT ( 'NONE',  ( 1.489501312335958172, -0.3162353388693405765, 0.4822834645669290543 ) ) ;
#38711 = CARTESIAN_POINT ( 'NONE',  ( 0.3937007874015754361, -0.1870078740157479769, 0.3641732283464567677 ) ) ;
#38712 = CARTESIAN_POINT ( 'NONE',  ( 0.4068241469816279987, -0.4281496062992127816, -0.4176697321401328100 ) ) ;
#38713 = CARTESIAN_POINT ( 'NONE',  ( 0.2362204724409449064, 0.4091458600556404646, -1.480971128608923548 ) ) ;
#38714 = CARTESIAN_POINT ( 'NONE',  ( 0.3543307086614181922, -0.5511811023622047445, 6.969142054262312111E-17 ) ) ;
#38715 = CARTESIAN_POINT ( 'NONE',  ( 0.4068241469816279987, -0.4281496062992127816, -0.4176697321401328100 ) ) ;
#38716 = CARTESIAN_POINT ( 'NONE',  ( 0.3949938075777408852, 0.1058382717557500435, -1.461286089238844843 ) ) ;
#38717 = CARTESIAN_POINT ( 'NONE',  ( -1.023622047244094002, -0.1870078740157480879, -0.4822834645669291653 ) ) ;
#38718 = CARTESIAN_POINT ( 'NONE',  ( 0.5774278215223103139, -0.5023911411419708095, -0.1820866141732282451 ) ) ;
#38719 = LINE ( 'NONE', #13901, #68912 ) ;
#38721 = EDGE_CURVE ( 'NONE', #71398, #18593, #59175, .T. ) ;
#38720 = CARTESIAN_POINT ( 'NONE',  ( -0.6496062992125976043, -0.5400638737290844871, 0.3530559997133364547 ) ) ;
#38722 = CARTESIAN_POINT ( 'NONE',  ( -0.4527559055118102749, -0.4536011799217368745, -0.2665933059059886201 ) ) ;
#38723 = DIRECTION ( 'NONE',  ( 1.000000000000000000, 0.000000000000000000, 0.000000000000000000 ) ) ;
#38724 = CARTESIAN_POINT ( 'NONE',  ( -0.2821522309711278487, 0.2952755905511811885, 0.1292274648535926551 ) ) ;
#38725 = CARTESIAN_POINT ( 'NONE',  ( -0.2362204724409440182, -0.1870078740157479769, 0.4822834645669291653 ) ) ;
#38726 = CARTESIAN_POINT ( 'NONE',  ( 0.1246719160104994284, -0.5511811023622046335, 0.09757992244046803654 ) ) ;
#38727 = CARTESIAN_POINT ( 'NONE',  ( 0.3460692066303958092, 0.1998031496062993018, -2.255249343832021136 ) ) ;
#38728 = CARTESIAN_POINT ( 'NONE',  ( -0.1377952755905504645, -0.5400638737290845981, -0.3530559997133363437 ) ) ;
#38729 = EDGE_CURVE ( 'NONE', #39936, #57846, #5197, .T. ) ;
#38730 = CARTESIAN_POINT ( 'NONE',  ( -0.3917322834645668994, -0.1049643490035306742, -1.858248400753593987 ) ) ;
#38731 = CARTESIAN_POINT ( 'NONE',  ( 1.089238845144357759, -0.004921259842519870586, -0.3153832671262229437 ) ) ;
#38732 = CARTESIAN_POINT ( 'NONE',  ( 1.509186351706037543, -0.4281496062992127816, -0.4176697321401328100 ) ) ;
#38733 = CARTESIAN_POINT ( 'NONE',  ( -0.6561679790026240244, -0.5023911411419708095, 0.1820866141732285504 ) ) ;
#38734 = CARTESIAN_POINT ( 'NONE',  ( -0.5905511811023615998, 0.1771653543307087630, 0.000000000000000000 ) ) ;
#38735 = CARTESIAN_POINT ( 'NONE',  ( -0.5577427821522301654, -0.3162353388693405765, 0.4822834645669290543 ) ) ;
#38736 = CARTESIAN_POINT ( 'NONE',  ( 0.05249343832021075018, 0.2306618581243847221, -0.2411417322834647770 ) ) ;
#38737 = CARTESIAN_POINT ( 'NONE',  ( 0.4921259842519691285, -0.4536011799217368745, -0.2665933059059886201 ) ) ;
#38738 = CARTESIAN_POINT ( 'NONE',  ( 0.4091458600556403535, 0.2362204724409449896, -2.335958005249343827 ) ) ;
#38739 = CARTESIAN_POINT ( 'NONE',  ( 1.213910761154856299, -0.5511811023622048555, -0.09757992244046775898 ) ) ;
#38740 = CARTESIAN_POINT ( 'NONE',  ( 0.6364829396325465405, -0.3162353388693409650, -0.4822834645669289433 ) ) ;
#38741 = EDGE_CURVE ( 'NONE', #27293, #10557, #47928, .T. ) ;
#38742 = CARTESIAN_POINT ( 'NONE',  ( 0.3460692066303959202, -0.1998031496062991630, 0.1332020997375328031 ) ) ;
#38743 = CARTESIAN_POINT ( 'NONE',  ( -0.1574803149606292529, -0.1870078740157479769, 0.4822834645669291653 ) ) ;
#38744 = CARTESIAN_POINT ( 'NONE',  ( 0.3917322834645670104, -0.1049643490035303411, -1.141076115485564202 ) ) ;
#38745 = CARTESIAN_POINT ( 'NONE',  ( 1.391076115485564868, -0.5023911411419708095, 0.1820866141732285504 ) ) ;
#38746 = CARTESIAN_POINT ( 'NONE',  ( 1.043307086614173818, 0.1660481256975885056, 0.3530559997133364547 ) ) ;
#38747 = CARTESIAN_POINT ( 'NONE',  ( 0.1968503937007881344, -0.6692913385826771977, 8.415575281601705876E-17 ) ) ;
#38748 = CARTESIAN_POINT ( 'NONE',  ( -0.4029448339610336438, 1.286526487772640115, -3.916342797992894198 ) ) ;
#38749 = CARTESIAN_POINT ( 'NONE',  ( 0.4002624671916016896, -0.08942795157527998196, 0.3641732283464567121 ) ) ;
#38750 = CARTESIAN_POINT ( 'NONE',  ( 0.6036745406824154392, 0.2306618581243847221, -0.2411417322834647770 ) ) ;
#38751 = CARTESIAN_POINT ( 'NONE',  ( -0.2493438320209966919, -0.004921259842519870586, -0.3153832671262229437 ) ) ;
#38752 = CARTESIAN_POINT ( 'NONE',  ( -0.8661417322834640276, -0.1870078740157479769, 0.4822834645669291653 ) ) ;
#38753 = DIRECTION ( 'NONE',  ( 0.000000000000000000, -1.734723475976805862E-16, -1.000000000000000000 ) ) ;
#38754 = CARTESIAN_POINT ( 'NONE',  ( -0.1968503937007867743, -0.6692913385826771977, 8.415575281601705876E-17 ) ) ;
#38755 = CARTESIAN_POINT ( 'NONE',  ( -1.397637795275589623, -0.5400638737290845981, -0.3530559997133363437 ) ) ;
#38756 = CARTESIAN_POINT ( 'NONE',  ( -0.6167979002624665030, -0.004921259842519576551, 0.3153832671262227771 ) ) ;
#38757 = CARTESIAN_POINT ( 'NONE',  ( 0.2296587926509192634, -0.05778040916215560624, -0.4822834645669293319 ) ) ;
#38758 = CARTESIAN_POINT ( 'NONE',  ( -1.128608923884513837, -0.6046776061558807314, 0.2411417322834647770 ) ) ;
#38759 = CARTESIAN_POINT ( 'NONE',  ( -0.4199475065616791736, -0.6046776061558807314, 0.2411417322834647770 ) ) ;
#38761 = CARTESIAN_POINT ( 'NONE',  ( 1.469816272965879911, 0.2306618581243847221, -0.2411417322834647770 ) ) ;
#38760 = DIRECTION ( 'NONE',  ( 1.000000000000000000, 0.000000000000000000, -0.000000000000000000 ) ) ;
#38762 = CARTESIAN_POINT ( 'NONE',  ( 1.437007874015748810, -0.5400638737290845981, -0.3530559997133363437 ) ) ;
#38763 = CARTESIAN_POINT ( 'NONE',  ( 0.1958661417322834775, 0.3392501089628018884, -2.498687664041994605 ) ) ;
#38764 = DIRECTION ( 'NONE',  ( -0.000000000000000000, -1.000000000000000000, -0.000000000000000000 ) ) ;
#38765 = CARTESIAN_POINT ( 'NONE',  ( -1.082677165354329896, 0.1660481256975885056, 0.3530559997133364547 ) ) ;
#38766 = CARTESIAN_POINT ( 'NONE',  ( 0.1265901696524989462, 0.4724409448818897572, -0.7808398950131233418 ) ) ;
#38767 = CARTESIAN_POINT ( 'NONE',  ( 0.1998031496062992740, 0.3460692066303959757, -0.1443569553805774397 ) ) ;
#38768 = VERTEX_POINT ( 'NONE', #4425 ) ;
#38769 = CARTESIAN_POINT ( 'NONE',  ( -0.2362204724409440182, -0.1870078740157479769, 0.3641732283464567677 ) ) ;
#38770 = CARTESIAN_POINT ( 'NONE',  ( 0.3917322834645669549, 0.1049643490035304660, -1.691601049868766360 ) ) ;
#38771 = VERTEX_POINT ( 'NONE', #3605 ) ;
#38772 = CARTESIAN_POINT ( 'NONE',  ( 0.2034120734908142214, 0.2952755905511810774, -0.1292274648535930714 ) ) ;
#38773 = CARTESIAN_POINT ( 'NONE',  ( 0.6233595800524939223, -0.3162353388693405765, 0.4822834645669290543 ) ) ;
#38774 = CARTESIAN_POINT ( 'NONE',  ( -0.2362204724409451284, 0.4091458600556402425, -2.847769028871391050 ) ) ;
#38775 = CARTESIAN_POINT ( 'NONE',  ( -0.5404819259526909558, -4.992347309556208597E-15, 0.4118484887281982920 ) ) ;
#38776 = CARTESIAN_POINT ( 'NONE',  ( -0.3280839895013117347, -0.004921259842519870586, -0.3153832671262229437 ) ) ;
#38777 = CARTESIAN_POINT ( 'NONE',  ( 0.3821149210511736727, 0.02791078216816508459, -0.4328096321851889194 ) ) ;
#38778 = CARTESIAN_POINT ( 'NONE',  ( 0.6627296587926517768, -0.6692913385826773087, -0.1292274648535924053 ) ) ;
#38779 = CARTESIAN_POINT ( 'NONE',  ( 0.9514435695538062676, -0.08942795157527998196, 0.3641732283464567121 ) ) ;
#38780 = CARTESIAN_POINT ( 'NONE',  ( -0.5971128608923877978, -0.6692913385826773087, -0.1292274648535924053 ) ) ;
#38781 = CARTESIAN_POINT ( 'NONE',  ( 0.2867679344610365999, 0.2867679344610365999, -1.005230028050182245 ) ) ;
#38782 = CARTESIAN_POINT ( 'NONE',  ( -0.6299212598425188991, -0.1870078740157480879, -0.4822834645669291653 ) ) ;
#38783 = CARTESIAN_POINT ( 'NONE',  ( -1.318897637795274802, -0.4536011799217368745, -0.2665933059059886201 ) ) ;
#38784 = CARTESIAN_POINT ( 'NONE',  ( -0.8267716535433065062, -0.6692913385826771977, 8.415575281601705876E-17 ) ) ;
#38785 = CARTESIAN_POINT ( 'NONE',  ( 1.640419947506562393, -0.4281496062992124485, 0.4176697321401328655 ) ) ;
#38786 = DIRECTION ( 'NONE',  ( 0.000000000000000000, 0.000000000000000000, -1.000000000000000000 ) ) ;
#38787 = VERTEX_POINT ( 'NONE', #28853 ) ;
#38788 = CARTESIAN_POINT ( 'NONE',  ( -0.2867679344610365444, -0.2867679344610367664, -2.260518003445880719 ) ) ;
#38789 = CARTESIAN_POINT ( 'NONE',  ( 0.2034120734908144990, -0.6692913385826771977, 0.1292274648535927661 ) ) ;
#38790 = EDGE_LOOP ( 'NONE', ( #77079, #50185, #31340, #78141, #67792, #32876, #69963, #18092 ) ) ;
#38791 = CARTESIAN_POINT ( 'NONE',  ( -0.8661417322834640276, -0.1870078740157480879, -0.4822834645669291653 ) ) ;
#38792 = EDGE_CURVE ( 'NONE', #400, #25602, #16661, .T. ) ;
#38793 = CARTESIAN_POINT ( 'NONE',  ( 1.325459317585302665, 0.05413385826771626580, -0.4176697321401330321 ) ) ;
#38794 = CARTESIAN_POINT ( 'NONE',  ( 1.128608923884514947, 0.2306618581243848609, 0.2411417322834645549 ) ) ;
#38795 = CARTESIAN_POINT ( 'NONE',  ( 0.6102362204724416372, -0.5400638737290844871, 0.3530559997133364547 ) ) ;
#38796 = CARTESIAN_POINT ( 'NONE',  ( 0.2296587926509192634, -0.3162353388693405765, 0.4822834645669290543 ) ) ;
#38797 = CARTESIAN_POINT ( 'NONE',  ( -0.2867679344610364334, -0.2867679344610367109, -1.718503937007874072 ) ) ;
#38798 = CARTESIAN_POINT ( 'NONE',  ( -1.122047244094487306, -0.5400638737290844871, 0.3530559997133364547 ) ) ;
#38799 = CARTESIAN_POINT ( 'NONE',  ( -0.02624671916010428221, 0.2306618581243847221, -0.2411417322834647770 ) ) ;
#38800 = CARTESIAN_POINT ( 'NONE',  ( -0.2165354330708654795, 0.07958543189024085140, 0.2665933059059887866 ) ) ;
#38801 = FACE_OUTER_BOUND ( 'NONE', #82349, .T. ) ;
#38802 = CARTESIAN_POINT ( 'NONE',  ( -0.05249343832020938322, -0.6046776061558809534, -0.2411417322834644161 ) ) ;
#38803 = LINE ( 'NONE', #14824, #27858 ) ;
#38804 = EDGE_CURVE ( 'NONE', #69251, #11040, #36409, .T. ) ;
#38805 = CARTESIAN_POINT ( 'NONE',  ( 1.332020997375328974, -0.05778040916215560624, -0.4822834645669293319 ) ) ;
#38806 = FACE_OUTER_BOUND ( 'NONE', #27955, .T. ) ;
#38807 = ORIENTED_EDGE ( 'NONE', *, *, #63898, .F. ) ;
#38808 = ORIENTED_EDGE ( 'NONE', *, *, #27035, .T. ) ;
#38809 = CARTESIAN_POINT ( 'NONE',  ( 0.4461942257217856311, 0.2306618581243847221, -0.2411417322834647770 ) ) ;
#38810 = CARTESIAN_POINT ( 'NONE',  ( -0.3083989501312330295, -0.08942795157527998196, 0.3641732283464567121 ) ) ;
#38812 = DIRECTION ( 'NONE',  ( 1.047444401652940007E-14, -0.000000000000000000, -1.000000000000000000 ) ) ;
#38811 = CARTESIAN_POINT ( 'NONE',  ( 1.633858267716535639, -0.4536011799217367080, 0.2665933059059888421 ) ) ;
#38813 = CARTESIAN_POINT ( 'NONE',  ( -0.1265901696524993347, 0.4724409448818895907, -0.08333333333333335646 ) ) ;
#38814 = CARTESIAN_POINT ( 'NONE',  ( 1.614173228346457378, 0.2952755905511811885, 0.000000000000000000 ) ) ;
#38815 = CARTESIAN_POINT ( 'NONE',  ( 0.3996062992125984925, 0.1070741851644054637, -2.721128608923884418 ) ) ;
#38816 = CARTESIAN_POINT ( 'NONE',  ( -0.1509186351706028884, -0.05778040916215522460, 0.4822834645669289988 ) ) ;
#38817 = CARTESIAN_POINT ( 'NONE',  ( 0.4359958488159610956, 1.724409448818897461, 1.033875059083681158 ) ) ;
#38818 = CARTESIAN_POINT ( 'NONE',  ( -1.397637795275589623, 0.1660481256975885056, 0.3530559997133364547 ) ) ;
#38819 = CARTESIAN_POINT ( 'NONE',  ( 0.3543307086614179147, 0.2952755905511811885, 0.000000000000000000 ) ) ;
#38820 = CARTESIAN_POINT ( 'NONE',  ( -0.3420746716998660508, -0.1974969037888706924, 0.02821522309711286050 ) ) ;
#38821 = CARTESIAN_POINT ( 'NONE',  ( 1.535433070866142558, 0.2952755905511811885, 0.000000000000000000 ) ) ;
#38822 = CARTESIAN_POINT ( 'NONE',  ( 0.8333333333333340365, 0.2952755905511810774, -0.1292274648535930714 ) ) ;
#38823 = CARTESIAN_POINT ( 'NONE',  ( 0.9908136482939640111, -0.5511811023622046335, 0.09757992244046803654 ) ) ;
#38824 = CARTESIAN_POINT ( 'NONE',  ( -0.02624671916010428221, 0.2306618581243847221, -0.2411417322834647770 ) ) ;
#38825 = CARTESIAN_POINT ( 'NONE',  ( 0.7874015748031503170, -0.1870078740157480601, -0.3641732283464567677 ) ) ;
#38826 = CARTESIAN_POINT ( 'NONE',  ( -1.384514435695537005, -0.6692913385826773087, -0.1292274648535924053 ) ) ;
#38827 = CARTESIAN_POINT ( 'NONE',  ( -0.1998031496062994405, 0.3460692066303957537, -0.7198162729658792447 ) ) ;
#38828 = CARTESIAN_POINT ( 'NONE',  ( 1.003937007874016407, -0.5400638737290844871, 0.3530559997133364547 ) ) ;
#38829 =( BOUNDED_SURFACE ( )  B_SPLINE_SURFACE ( 1, 2, ( 
 ( #60772, #61185, #15347, #54451, #27957, #80163, #22480, #48141, #74668, #3539, #36344, #47304, #72994, #41008, #68349, #66692, #9027, #30440, #83032, #68752, #18238, #24936, #69978, #75898, #11513, #37579, #50606, #63666, #11094, #24535, #51017, #4764, #37169, #63252, #62849, #69162, #5592, #36751, #6006, #17424, #49790, #12333, #24121, #62427, #82620, #25355, #44288, #31258, #69576, #76716, #76313, #50201, #57336, #31675, #37990, #56105, #19049, #56926, #43878, #11924, #81809, #75492, #18644, #17831, #44696, #70393, #12748, #38407, #4355, #30023, #43465, #5185, #55687, #30849, #56514, #81394, #23710, #49381, #75077, #82217, #43055, #46802, #65356, #52693, #70826, #64501, #46383, #26622, #27031, #7694, #13173, #6839, #26194, #78400, #20310, #52276, #32510, #40087, #45543, #32934, #64924, #33361, #71241, #59024, #19468, #58172, #77980, #38823, #45961, #71657, #13585, #39240, #65774, #1788, #45118, #19896, #14009, #25771, #7262, #51855, #20732, #968, #541, #1380, #59434, #72076, #27448, #53109, #21147, #77562, #14435, #58599, #33772, #39666, #8106, #78818, #72493, #51432, #14842, #64087, #6424, #32093, #57754, #116, #77135, #29520, #74156, #74574, #2203, #59851, #28698, #53942, #9759, #48874, #15257, #2624, #60274, #73750, #73327, #41335, #35846, #8520, #67425, #28280, #27871, #79655, #16086, #3033, #15674, #79239, #40916, #29110, #35019, #40502, #22389, #34609, #53531, #21554, #55181, #54780, #3446, #67015, #47215, #10181, #66184, #34187, #54360, #72905, #35430, #66598, #9348, #8932, #80072, #21971, #61515, #47633, #48049, #61095, #22796, #41731, #60683, #80483, #48456, #16504, #42147, #67842, #3860, #80890, #23203, #75799, #49694, #81716, #18141, #49284, #76212, #29926, #62329, #82523, #36654, #23615, #11831, #12237, #56826, #50102, #82120, #5904, #5497, #62754, #69883, #44193, #24841, #17332, #50508, #43775, #56420, #24435, #74987, #18548, #37893, #69478, #55589, #50919, #63569, #30758, #24026, #4666, #37484, #30339, #31576, #5090, #56005, #42962, #57232, #36252, #82933, #25255, #16919, #68656, #75389, #42556, #68260, #10994, #4263, #10596, #61922, #81301, #17735, #43364, #69064, #11414, #37069, #63158, #31159, #52590, #46280, #70292, #64816, #12644, #7157, #45016, #1280, #59331, #16, #435, #1688, #71976, #57654, #33669, #19366, #13478, #25670, #26929, #65678, #13903, #18950, #65250, #14330, #26090, #78297, #32828, #77453, #77034, #6317, #20629, #13067, #58496, #63980, #51750, #76619, #19788, #45440, #71136, #33259, #860, #27346, #44597, #38306, #39988, #8005, #31994, #6735, #51330, #39136, #70716, #52172, #26517, #58921, #38722, #64399, #7587, #32406, #77875, #20206, #45856, #58069, #71554, #39561, #3342, #3756, #14744, #72394, #41230, #66493, #22284, #61407, #27765, #15151, #72802, #2934, #2522, #53838, #48355, #21042, #79971, #40808, #40398, #8827, #28598, #15571, #28180, #8415, #53430, #41636, #47529, #53004, #34921, #47113, #66079, #34083, #42046, #67327, #15989, #79551, #59746, #22696, #78717, #46701, #66917, #2100, #47945, #79138, #60584, #21455, #67742, #9660, #29006, #35330, #54255, #74053, #34504, #21864, #10075, #60168, #73220, #60993, #54672, #73647, #9249, #80384, #16400, #35739, #30664, #18048, #36151, #29828, #11738, #75294, #75707, #56327, #61824, #55491, #74888, #43681, #68967, #17638, #81201, #5402, #10900, #81619, #30244, #82026, #36558, #24340, #68153, #23516, #43270, #4164, #11316, #36975, #62235, #4573, #31065, #51542, #10497, #68557, #62655, #74470, #55907, #17234, #69384, #49600, #49185, #50009, #25881, #37393, #42864, #63065, #4996, #56733, #230, #23933, #77245, #19575, #45235, #70935, #64612, #13280, #38932, #29421, #55079, #80788, #23103, #48771, #16817, #42453, #33038, #40603, #26305, #53631, #47319, #2312, #13693, #52379, #72598, #14944, #58707, #77670, #73010, #58282, #27973, #39348, #647, #26725, #46903, #79339, #1072, #14117, #66286, #59957, #51963, #78511, #20000, #20834, #78088, #8625, #15361, #65033, #39770, #41022, #21659, #71346, #6949, #20419, #27137, #7368, #34296, #32620, #27556, #45651, #78926, #46072 ),
 ( #53215, #65465, #71764, #7799, #33464, #59126, #52802, #1483, #1896, #46487, #72182, #14540, #40192, #21248, #65875, #8210, #33875, #59540, #41435, #41839, #55701, #47735, #73852, #74681, #48982, #10288, #29220, #60786, #9041, #49397, #67946, #55289, #73433, #67118, #17027, #54887, #29629, #35955, #15783, #9449, #28802, #80999, #22900, #80592, #35120, #42666, #48157, #68365, #23313, #74265, #4370, #3139, #67529, #81409, #54466, #16193, #10703, #36359, #61624, #48567, #80179, #34715, #75091, #3966, #62034, #22494, #9867, #30039, #16608, #23726, #17439, #35536, #61198, #3555, #66708, #42251, #60376, #2724, #28385, #54045, #79759, #22076, #69991, #24550, #38002, #81825, #69175, #56938, #17845, #5605, #82635, #75912, #18251, #44709, #64101, #24135, #82231, #24948, #4779, #69590, #30863, #31690, #63264, #49805, #63680, #38419, #57348, #6436, #32107, #128, #56528, #51030, #50216, #12762, #18656, #76326, #25367, #75506, #30455, #83044, #76729, #11936, #31273, #43893, #37591, #50621, #57766, #19061, #77148, #56119, #62443, #44300, #12346, #6018, #51444, #43479, #5199, #62862, #70406, #25783, #43069, #68766, #11110, #36767, #11526, #37183, #39252, #52704, #65370, #77993, #58183, #19906, #8118, #38835, #33372, #6851, #52288, #19480, #45974, #71669, #20321, #59447, #7705, #2215, #70837, #13186, #53541, #14021, #64514, #59036, #45556, #14853, #553, #1390, #40097, #64934, #7274, #78415, #39678, #27044, #40514, #32521, #46394, #32945, #26206, #58611, #20744, #72088, #14446, #51868, #21157, #77574, #979, #71252, #65785, #13598, #26634, #33783, #8531, #1799, #27462, #53120, #78831, #72504, #45133, #46813, #66194, #34198, #59862, #27881, #61106, #47644, #10607, #42159, #55194, #10192, #3458, #16930, #53952, #54372, #68272, #60284, #3043, #3872, #61526, #22810, #41741, #73339, #21564, #61933, #80494, #67854, #2634, #79665, #29531, #67435, #35861, #48467, #28290, #21982, #41345, #80901, #35440, #9769, #15687, #23215, #60693, #48059, #80082, #74168, #28708, #16515, #34620, #67025, #29123, #9358, #54791, #48885, #22402, #73761, #74586, #42570, #35029, #16096, #36264, #40928, #4276, #29937, #79249, #47226, #72916, #15267, #66608, #8944, #18960, #44608, #12657, #69077, #63580, #62768, #25265, #31170, #5507, #37903, #36666, #42972, #69893, #5914, #82132, #18154, #30769, #11427, #11841, #70304, #31588, #6333, #17344, #74998, #43786, #37082, #24852, #63992, #30351, #12247, #63169, #76629, #56020, #56430, #38318, #62341, #5102, #57243, #82947, #82534, #69492, #49707, #81313, #55601, #56836, #44203, #4680, #81728, #50931, #37494, #18559, #50520, #24037, #75402, #17748, #23626, #76226, #49297, #43377, #68668, #24446, #50114, #75811, #11007, #77466, #13918, #45029, #6747, #873, #38735, #32841, #26532, #45452, #71150, #78310, #71989, #70728, #51764, #52185, #51341, #13491, #26102, #7600, #7170, #13082, #39574, #14342, #33274, #40002, #65690, #8018, #19803, #1292, #39147, #20641, #20220, #77889, #58934, #64412, #77045, #26942, #52603, #64832, #58510, #45869, #71567, #65264, #33681, #46294, #59343, #19377, #25681, #32006, #57666, #28, #32419, #58081, #447, #43643, #57101, #56694, #24711, #19225, #75256, #50790, #69346, #11278, #11700, #82796, #69754, #82393, #62615, #25532, #81987, #37354, #49971, #5769, #18009, #68929, #36937, #12928, #38170, #70156, #50379, #4957, #76895, #23896, #17600, #12100, #30625, #18818, #56290, #31438, #75669, #38588, #12509, #83210, #24301, #63027, #25120, #5365, #76077, #31026, #63844, #44062, #18421, #44465, #44875, #6182, #70574, #64266, #6600, #37758, #31860, #63433, #32272, #76491, #57519, #51197, #57932, #49562, #43232, #59563, #65489, #21272, #14968, #38950, #33488, #64634, #59150, #13718, #53238, #27996, #51986, #52401, #53655, #40626, #26324, #2339, #71368, #7821, #77691, #78954, #34319, #65897, #70953, #33898, #66308, #78110, #46927, #1507, #46096, #52823, #39371, #13298, #6969, #27160, #32640, #20442, #45257, #71788, #14142, #39794, #1919, #78535, #79363, #58304, #669, #20021, #20858, #45672, #46510, #65057, #8648, #7394, #72211, #8233 ) ),
 .UNSPECIFIED., .F., .F., .F. ) 
 B_SPLINE_SURFACE_WITH_KNOTS ( ( 2, 2 ),
 ( 3, 2, 2, 2, 2, 2, 2, 2, 2, 2, 2, 2, 2, 2, 2, 2, 2, 2, 2, 2, 2, 2, 2, 2, 2, 2, 2, 2, 2, 2, 2, 2, 2, 2, 2, 2, 2, 2, 2, 2, 2, 2, 2, 2, 2, 2, 2, 2, 2, 2, 2, 2, 2, 2, 2, 2, 2, 2, 2, 2, 2, 2, 2, 2, 2, 2, 2, 2, 2, 2, 2, 2, 2, 2, 2, 2, 2, 2, 2, 2, 2, 2, 2, 2, 2, 2, 2, 2, 2, 2, 2, 2, 2, 2, 2, 2, 2, 2, 2, 2, 2, 2, 2, 2, 2, 2, 2, 2, 2, 2, 2, 2, 2, 2, 2, 2, 2, 2, 2, 2, 2, 2, 2, 2, 2, 2, 2, 2, 2, 2, 2, 2, 2, 2, 2, 2, 2, 2, 2, 2, 2, 2, 2, 2, 2, 2, 2, 2, 2, 2, 2, 2, 2, 2, 2, 2, 2, 2, 2, 2, 2, 2, 2, 2, 2, 2, 2, 2, 2, 2, 2, 2, 2, 2, 2, 2, 2, 2, 2, 2, 2, 2, 2, 2, 2, 2, 2, 2, 2, 2, 2, 2, 2, 2, 2, 2, 2, 2, 2, 2, 2, 2, 2, 2, 2, 2, 2, 2, 2, 2, 2, 2, 2, 2, 2, 2, 2, 2, 2, 2, 2, 2, 2, 2, 2, 2, 2, 2, 2, 2, 2, 2, 2, 2, 2, 2, 2, 2, 2, 2, 2, 2, 2, 2, 2, 2, 2, 2, 2, 2, 2, 2, 2, 2, 2, 3 ),
 ( 0.000000000000000000, 1.000000000000000000 ),
 ( 0.000000000000000000, 0.003787878787878787984, 0.007575757575757575968, 0.01136363636363636395, 0.01515151515151515194, 0.01893939393939393992, 0.02272727272727272790, 0.02651515151515151589, 0.03030303030303030387, 0.03409090909090908839, 0.03787878787878787984, 0.04166666666666666435, 0.04545454545454545581, 0.04924242424242424032, 0.05303030303030303177, 0.05681818181818181629, 0.06060606060606060774, 0.06439393939393939226, 0.06818181818181817677, 0.07196969696969697516, 0.07575757575757575968, 0.07954545454545454419, 0.08333333333333332871, 0.08712121212121212710, 0.09090909090909091161, 0.09469696969696969613, 0.09848484848484848064, 0.1022727272727272790, 0.1060606060606060635, 0.1098484848484848481, 0.1136363636363636326, 0.1174242424242424310, 0.1212121212121212155, 0.1250000000000000000, 0.1287878787878787845, 0.1325757575757575690, 0.1363636363636363535, 0.1401515151515151381, 0.1439393939393939503, 0.1477272727272727348, 0.1515151515151515194, 0.1553030303030303039, 0.1590909090909090884, 0.1628787878787878729, 0.1666666666666666574, 0.1704545454545454419, 0.1742424242424242542, 0.1780303030303030387, 0.1818181818181818232, 0.1856060606060606077, 0.1893939393939393923, 0.1931818181818181768, 0.1969696969696969613, 0.2007575757575757458, 0.2045454545454545581, 0.2083333333333333426, 0.2121212121212121271, 0.2159090909090909116, 0.2196969696969696961, 0.2234848484848484806, 0.2272727272727272652, 0.2310606060606060497, 0.2348484848484848619, 0.2386363636363636465, 0.2424242424242424310, 0.2462121212121212155, 0.2500000000000000000, 0.2537878787878787845, 0.2575757575757575690, 0.2613636363636363535, 0.2651515151515151381, 0.2689393939393939226, 0.2727272727272727071, 0.2765151515151514916, 0.2803030303030302761, 0.2840909090909091161, 0.2878787878787879007, 0.2916666666666666852, 0.2954545454545454697, 0.2992424242424242542, 0.3030303030303030387, 0.3068181818181818232, 0.3106060606060606077, 0.3143939393939393923, 0.3181818181818181768, 0.3219696969696969613, 0.3257575757575757458, 0.3295454545454545303, 0.3333333333333333148, 0.3371212121212120993, 0.3409090909090908839, 0.3446969696969697239, 0.3484848484848485084, 0.3522727272727272929, 0.3560606060606060774, 0.3598484848484848619, 0.3636363636363636465, 0.3674242424242424310, 0.3712121212121212155, 0.3750000000000000000, 0.3787878787878787845, 0.3825757575757575690, 0.3863636363636363535, 0.3901515151515151381, 0.3939393939393939226, 0.3977272727272727071, 0.4015151515151514916, 0.4053030303030302761, 0.4090909090909091161, 0.4128787878787879007, 0.4166666666666666852, 0.4204545454545454697, 0.4242424242424242542, 0.4280303030303030387, 0.4318181818181818232, 0.4356060606060606077, 0.4393939393939393923, 0.4431818181818181768, 0.4469696969696969613, 0.4507575757575757458, 0.4545454545454545303, 0.4583333333333333148, 0.4621212121212120993, 0.4659090909090908839, 0.4696969696969697239, 0.4734848484848485084, 0.4772727272727272929, 0.4810606060606060774, 0.4848484848484848619, 0.4886363636363636465, 0.4924242424242424310, 0.4962121212121212155, 0.5000000000000000000, 0.5037878787878787845, 0.5075757575757575690, 0.5113636363636363535, 0.5151515151515151381, 0.5189393939393939226, 0.5227272727272727071, 0.5265151515151514916, 0.5303030303030302761, 0.5340909090909090606, 0.5378787878787878451, 0.5416666666666666297, 0.5454545454545454142, 0.5492424242424241987, 0.5530303030303029832, 0.5568181818181817677, 0.5606060606060605522, 0.5643939393939394478, 0.5681818181818182323, 0.5719696969696970168, 0.5757575757575758013, 0.5795454545454545858, 0.5833333333333333703, 0.5871212121212121549, 0.5909090909090909394, 0.5946969696969697239, 0.5984848484848485084, 0.6022727272727272929, 0.6060606060606060774, 0.6098484848484848619, 0.6136363636363636465, 0.6174242424242424310, 0.6212121212121212155, 0.6250000000000000000, 0.6287878787878787845, 0.6325757575757575690, 0.6363636363636363535, 0.6401515151515151381, 0.6439393939393939226, 0.6477272727272727071, 0.6515151515151514916, 0.6553030303030302761, 0.6590909090909090606, 0.6628787878787878451, 0.6666666666666666297, 0.6704545454545454142, 0.6742424242424241987, 0.6780303030303029832, 0.6818181818181817677, 0.6856060606060605522, 0.6893939393939394478, 0.6931818181818182323, 0.6969696969696970168, 0.7007575757575758013, 0.7045454545454545858, 0.7083333333333333703, 0.7121212121212121549, 0.7159090909090909394, 0.7196969696969697239, 0.7234848484848485084, 0.7272727272727272929, 0.7310606060606060774, 0.7348484848484848619, 0.7386363636363636465, 0.7424242424242424310, 0.7462121212121212155, 0.7500000000000000000, 0.7537878787878787845, 0.7575757575757575690, 0.7613636363636363535, 0.7651515151515151381, 0.7689393939393939226, 0.7727272727272727071, 0.7765151515151514916, 0.7803030303030302761, 0.7840909090909090606, 0.7878787878787878451, 0.7916666666666666297, 0.7954545454545454142, 0.7992424242424241987, 0.8030303030303029832, 0.8068181818181817677, 0.8106060606060605522, 0.8143939393939394478, 0.8181818181818182323, 0.8219696969696970168, 0.8257575757575758013, 0.8295454545454545858, 0.8333333333333333703, 0.8371212121212121549, 0.8409090909090909394, 0.8446969696969697239, 0.8484848484848485084, 0.8522727272727272929, 0.8560606060606060774, 0.8598484848484848619, 0.8636363636363636465, 0.8674242424242424310, 0.8712121212121212155, 0.8750000000000000000, 0.8787878787878787845, 0.8825757575757575690, 0.8863636363636363535, 0.8901515151515151381, 0.8939393939393939226, 0.8977272727272727071, 0.9015151515151514916, 0.9053030303030302761, 0.9090909090909090606, 0.9128787878787878451, 0.9166666666666666297, 0.9204545454545454142, 0.9242424242424241987, 0.9280303030303029832, 0.9318181818181817677, 0.9356060606060605522, 0.9393939393939394478, 0.9431818181818182323, 0.9469696969696970168, 0.9507575757575758013, 0.9545454545454545858, 0.9583333333333333703, 0.9621212121212121549, 0.9659090909090909394 ),
 .UNSPECIFIED. ) 
 GEOMETRIC_REPRESENTATION_ITEM ( )  RATIONAL_B_SPLINE_SURFACE ( (
 ( 1.000000000000000000, 0.9659258262890683122, 1.000000000000000000, 0.9659258262890683122, 1.000000000000000000, 0.9659258262890683122, 1.000000000000000000, 0.9659258262890683122, 1.000000000000000000, 0.9659258262890683122, 1.000000000000000000, 0.9659258262890683122, 1.000000000000000000, 0.9659258262890683122, 1.000000000000000000, 0.9659258262890683122, 1.000000000000000000, 0.9659258262890683122, 1.000000000000000000, 0.9659258262890683122, 1.000000000000000000, 0.9659258262890683122, 1.000000000000000000, 0.9659258262890683122, 1.000000000000000000, 0.9659258262890683122, 1.000000000000000000, 0.9659258262890683122, 1.000000000000000000, 0.9659258262890683122, 1.000000000000000000, 0.9659258262890683122, 1.000000000000000000, 0.9659258262890683122, 1.000000000000000000, 0.9659258262890683122, 1.000000000000000000, 0.9659258262890683122, 1.000000000000000000, 0.9659258262890683122, 1.000000000000000000, 0.9659258262890683122, 1.000000000000000000, 0.9659258262890683122, 1.000000000000000000, 0.9659258262890683122, 1.000000000000000000, 0.9659258262890683122, 1.000000000000000000, 0.9659258262890683122, 1.000000000000000000, 0.9659258262890683122, 1.000000000000000000, 0.9659258262890683122, 1.000000000000000000, 0.9659258262890683122, 1.000000000000000000, 0.9659258262890683122, 1.000000000000000000, 0.9659258262890683122, 1.000000000000000000, 0.9659258262890683122, 1.000000000000000000, 0.9659258262890683122, 1.000000000000000000, 0.9659258262890683122, 1.000000000000000000, 0.9659258262890683122, 1.000000000000000000, 0.9659258262890683122, 1.000000000000000000, 0.9659258262890683122, 1.000000000000000000, 0.9659258262890683122, 1.000000000000000000, 0.9659258262890683122, 1.000000000000000000, 0.9659258262890683122, 1.000000000000000000, 0.9659258262890683122, 1.000000000000000000, 0.9659258262890683122, 1.000000000000000000, 0.9659258262890683122, 1.000000000000000000, 0.9659258262890683122, 1.000000000000000000, 0.9659258262890683122, 1.000000000000000000, 0.9659258262890683122, 1.000000000000000000, 0.9659258262890683122, 1.000000000000000000, 0.9659258262890683122, 1.000000000000000000, 0.9659258262890683122, 1.000000000000000000, 0.9659258262890683122, 1.000000000000000000, 0.9659258262890683122, 1.000000000000000000, 0.9659258262890683122, 1.000000000000000000, 0.9659258262890683122, 1.000000000000000000, 0.9659258262890683122, 1.000000000000000000, 0.9659258262890683122, 1.000000000000000000, 0.9659258262890683122, 1.000000000000000000, 0.9659258262890683122, 1.000000000000000000, 0.9659258262890683122, 1.000000000000000000, 0.9659258262890683122, 1.000000000000000000, 0.9659258262890683122, 1.000000000000000000, 0.9659258262890683122, 1.000000000000000000, 0.9659258262890683122, 1.000000000000000000, 0.9659258262890683122, 1.000000000000000000, 0.9659258262890683122, 1.000000000000000000, 0.9659258262890683122, 1.000000000000000000, 0.9659258262890683122, 1.000000000000000000, 0.9659258262890683122, 1.000000000000000000, 0.9659258262890683122, 1.000000000000000000, 0.9659258262890683122, 1.000000000000000000, 0.9659258262890683122, 1.000000000000000000, 0.9659258262890683122, 1.000000000000000000, 0.9659258262890683122, 1.000000000000000000, 0.9659258262890683122, 1.000000000000000000, 0.9659258262890683122, 1.000000000000000000, 0.9659258262890683122, 1.000000000000000000, 0.9659258262890683122, 1.000000000000000000, 0.9659258262890683122, 1.000000000000000000, 0.9659258262890683122, 1.000000000000000000, 0.9659258262890683122, 1.000000000000000000, 0.9659258262890683122, 1.000000000000000000, 0.9659258262890683122, 1.000000000000000000, 0.9659258262890683122, 1.000000000000000000, 0.9659258262890683122, 1.000000000000000000, 0.9659258262890683122, 1.000000000000000000, 0.9659258262890683122, 1.000000000000000000, 0.9659258262890683122, 1.000000000000000000, 0.9659258262890683122, 1.000000000000000000, 0.9659258262890683122, 1.000000000000000000, 0.9659258262890683122, 1.000000000000000000, 0.9659258262890683122, 1.000000000000000000, 0.9659258262890683122, 1.000000000000000000, 0.9659258262890683122, 1.000000000000000000, 0.9659258262890683122, 1.000000000000000000, 0.9659258262890683122, 1.000000000000000000, 0.9659258262890683122, 1.000000000000000000, 0.9659258262890683122, 1.000000000000000000, 0.9659258262890683122, 1.000000000000000000, 0.9659258262890683122, 1.000000000000000000, 0.9659258262890683122, 1.000000000000000000, 0.9659258262890683122, 1.000000000000000000, 0.9659258262890683122, 1.000000000000000000, 0.9659258262890683122, 1.000000000000000000, 0.9659258262890683122, 1.000000000000000000, 0.9659258262890683122, 1.000000000000000000, 0.9659258262890683122, 1.000000000000000000, 0.9659258262890683122, 1.000000000000000000, 0.9659258262890683122, 1.000000000000000000, 0.9659258262890683122, 1.000000000000000000, 0.9659258262890683122, 1.000000000000000000, 0.9659258262890683122, 1.000000000000000000, 0.9659258262890683122, 1.000000000000000000, 0.9659258262890683122, 1.000000000000000000, 0.9659258262890683122, 1.000000000000000000, 0.9659258262890683122, 1.000000000000000000, 0.9659258262890683122, 1.000000000000000000, 0.9659258262890683122, 1.000000000000000000, 0.9659258262890683122, 1.000000000000000000, 0.9659258262890683122, 1.000000000000000000, 0.9659258262890683122, 1.000000000000000000, 0.9659258262890683122, 1.000000000000000000, 0.9659258262890683122, 1.000000000000000000, 0.9659258262890683122, 1.000000000000000000, 0.9659258262890683122, 1.000000000000000000, 0.9659258262890683122, 1.000000000000000000, 0.9659258262890683122, 1.000000000000000000, 0.9659258262890683122, 1.000000000000000000, 0.9659258262890683122, 1.000000000000000000, 0.9659258262890683122, 1.000000000000000000, 0.9659258262890683122, 1.000000000000000000, 0.9659258262890683122, 1.000000000000000000, 0.9659258262890683122, 1.000000000000000000, 0.9659258262890683122, 1.000000000000000000, 0.9659258262890683122, 1.000000000000000000, 0.9659258262890683122, 1.000000000000000000, 0.9659258262890683122, 1.000000000000000000, 0.9659258262890683122, 1.000000000000000000, 0.9659258262890683122, 1.000000000000000000, 0.9659258262890683122, 1.000000000000000000, 0.9659258262890683122, 1.000000000000000000, 0.9659258262890683122, 1.000000000000000000, 0.9659258262890683122, 1.000000000000000000, 0.9659258262890683122, 1.000000000000000000, 0.9659258262890683122, 1.000000000000000000, 0.9659258262890683122, 1.000000000000000000, 0.9659258262890683122, 1.000000000000000000, 0.9659258262890683122, 1.000000000000000000, 0.9659258262890683122, 1.000000000000000000, 0.9659258262890683122, 1.000000000000000000, 0.9659258262890683122, 1.000000000000000000, 0.9659258262890683122, 1.000000000000000000, 0.9659258262890683122, 1.000000000000000000, 0.9659258262890683122, 1.000000000000000000, 0.9659258262890683122, 1.000000000000000000, 0.9659258262890683122, 1.000000000000000000, 0.9659258262890683122, 1.000000000000000000, 0.9659258262890683122, 1.000000000000000000, 0.9659258262890683122, 1.000000000000000000, 0.9659258262890683122, 1.000000000000000000, 0.9659258262890683122, 1.000000000000000000, 0.9659258262890683122, 1.000000000000000000, 0.9659258262890683122, 1.000000000000000000, 0.9659258262890683122, 1.000000000000000000, 0.9659258262890683122, 1.000000000000000000, 0.9659258262890683122, 1.000000000000000000, 0.9659258262890683122, 1.000000000000000000, 0.9659258262890683122, 1.000000000000000000, 0.9659258262890683122, 1.000000000000000000, 0.9659258262890683122, 1.000000000000000000, 0.9659258262890683122, 1.000000000000000000, 0.9659258262890683122, 1.000000000000000000, 0.9659258262890683122, 1.000000000000000000, 0.9659258262890683122, 1.000000000000000000, 0.9659258262890683122, 1.000000000000000000, 0.9659258262890683122, 1.000000000000000000, 0.9659258262890683122, 1.000000000000000000, 0.9659258262890683122, 1.000000000000000000, 0.9659258262890683122, 1.000000000000000000, 0.9659258262890683122, 1.000000000000000000, 0.9659258262890683122, 1.000000000000000000, 0.9659258262890683122, 1.000000000000000000, 0.9659258262890683122, 1.000000000000000000, 0.9659258262890683122, 1.000000000000000000, 0.9659258262890683122, 1.000000000000000000, 0.9659258262890683122, 1.000000000000000000, 0.9659258262890683122, 1.000000000000000000, 0.9659258262890683122, 1.000000000000000000, 0.9659258262890683122, 1.000000000000000000, 0.9659258262890683122, 1.000000000000000000, 0.9659258262890683122, 1.000000000000000000, 0.9659258262890683122, 1.000000000000000000, 0.9659258262890683122, 1.000000000000000000, 0.9659258262890683122, 1.000000000000000000, 0.9659258262890683122, 1.000000000000000000, 0.9659258262890683122, 1.000000000000000000, 0.9659258262890683122, 1.000000000000000000, 0.9659258262890683122, 1.000000000000000000, 0.9659258262890683122, 1.000000000000000000, 0.9659258262890683122, 1.000000000000000000, 0.9659258262890683122, 1.000000000000000000, 0.9659258262890683122, 1.000000000000000000, 0.9659258262890683122, 1.000000000000000000, 0.9659258262890683122, 1.000000000000000000, 0.9659258262890683122, 1.000000000000000000, 0.9659258262890683122, 1.000000000000000000, 0.9659258262890683122, 1.000000000000000000, 0.9659258262890683122, 1.000000000000000000, 0.9659258262890683122, 1.000000000000000000, 0.9659258262890683122, 1.000000000000000000, 0.9659258262890683122, 1.000000000000000000, 0.9659258262890683122, 1.000000000000000000, 0.9659258262890683122, 1.000000000000000000, 0.9659258262890683122, 1.000000000000000000, 0.9659258262890683122, 1.000000000000000000, 0.9659258262890683122, 1.000000000000000000, 0.9659258262890683122, 1.000000000000000000, 0.9659258262890683122, 1.000000000000000000, 0.9659258262890683122, 1.000000000000000000, 0.9659258262890683122, 1.000000000000000000, 0.9659258262890683122, 1.000000000000000000, 0.9659258262890683122, 1.000000000000000000, 0.9659258262890683122, 1.000000000000000000, 0.9659258262890683122, 1.000000000000000000, 0.9659258262890683122, 1.000000000000000000, 0.9659258262890683122, 1.000000000000000000, 0.9659258262890683122, 1.000000000000000000, 0.9659258262890683122, 1.000000000000000000, 0.9659258262890683122, 1.000000000000000000, 0.9659258262890683122, 1.000000000000000000, 0.9659258262890683122, 1.000000000000000000, 0.9659258262890683122, 1.000000000000000000, 0.9659258262890683122, 1.000000000000000000, 0.9659258262890683122, 1.000000000000000000, 0.9659258262890683122, 1.000000000000000000, 0.9659258262890683122, 1.000000000000000000, 0.9659258262890683122, 1.000000000000000000, 0.9659258262890683122, 1.000000000000000000, 0.9659258262890683122, 1.000000000000000000, 0.9659258262890683122, 1.000000000000000000, 0.9659258262890683122, 1.000000000000000000, 0.9659258262890683122, 1.000000000000000000, 0.9659258262890683122, 1.000000000000000000, 0.9659258262890683122, 1.000000000000000000, 0.9659258262890683122, 1.000000000000000000, 0.9659258262890683122, 1.000000000000000000, 0.9659258262890683122, 1.000000000000000000, 0.9659258262890683122, 1.000000000000000000, 0.9659258262890683122, 1.000000000000000000, 0.9659258262890683122, 1.000000000000000000, 0.9659258262890683122, 1.000000000000000000, 0.9659258262890683122, 1.000000000000000000, 0.9659258262890683122, 1.000000000000000000, 0.9659258262890683122, 1.000000000000000000, 0.9659258262890683122, 1.000000000000000000, 0.9659258262890683122, 1.000000000000000000, 0.9659258262890683122, 1.000000000000000000, 0.9659258262890683122, 1.000000000000000000),
 ( 1.000000000000000000, 0.9659258262890683122, 1.000000000000000000, 0.9659258262890683122, 1.000000000000000000, 0.9659258262890683122, 1.000000000000000000, 0.9659258262890683122, 1.000000000000000000, 0.9659258262890683122, 1.000000000000000000, 0.9659258262890683122, 1.000000000000000000, 0.9659258262890683122, 1.000000000000000000, 0.9659258262890683122, 1.000000000000000000, 0.9659258262890683122, 1.000000000000000000, 0.9659258262890683122, 1.000000000000000000, 0.9659258262890683122, 1.000000000000000000, 0.9659258262890683122, 1.000000000000000000, 0.9659258262890683122, 1.000000000000000000, 0.9659258262890683122, 1.000000000000000000, 0.9659258262890683122, 1.000000000000000000, 0.9659258262890683122, 1.000000000000000000, 0.9659258262890683122, 1.000000000000000000, 0.9659258262890683122, 1.000000000000000000, 0.9659258262890683122, 1.000000000000000000, 0.9659258262890683122, 1.000000000000000000, 0.9659258262890683122, 1.000000000000000000, 0.9659258262890683122, 1.000000000000000000, 0.9659258262890683122, 1.000000000000000000, 0.9659258262890683122, 1.000000000000000000, 0.9659258262890683122, 1.000000000000000000, 0.9659258262890683122, 1.000000000000000000, 0.9659258262890683122, 1.000000000000000000, 0.9659258262890683122, 1.000000000000000000, 0.9659258262890683122, 1.000000000000000000, 0.9659258262890683122, 1.000000000000000000, 0.9659258262890683122, 1.000000000000000000, 0.9659258262890683122, 1.000000000000000000, 0.9659258262890683122, 1.000000000000000000, 0.9659258262890683122, 1.000000000000000000, 0.9659258262890683122, 1.000000000000000000, 0.9659258262890683122, 1.000000000000000000, 0.9659258262890683122, 1.000000000000000000, 0.9659258262890683122, 1.000000000000000000, 0.9659258262890683122, 1.000000000000000000, 0.9659258262890683122, 1.000000000000000000, 0.9659258262890683122, 1.000000000000000000, 0.9659258262890683122, 1.000000000000000000, 0.9659258262890683122, 1.000000000000000000, 0.9659258262890683122, 1.000000000000000000, 0.9659258262890683122, 1.000000000000000000, 0.9659258262890683122, 1.000000000000000000, 0.9659258262890683122, 1.000000000000000000, 0.9659258262890683122, 1.000000000000000000, 0.9659258262890683122, 1.000000000000000000, 0.9659258262890683122, 1.000000000000000000, 0.9659258262890683122, 1.000000000000000000, 0.9659258262890683122, 1.000000000000000000, 0.9659258262890683122, 1.000000000000000000, 0.9659258262890683122, 1.000000000000000000, 0.9659258262890683122, 1.000000000000000000, 0.9659258262890683122, 1.000000000000000000, 0.9659258262890683122, 1.000000000000000000, 0.9659258262890683122, 1.000000000000000000, 0.9659258262890683122, 1.000000000000000000, 0.9659258262890683122, 1.000000000000000000, 0.9659258262890683122, 1.000000000000000000, 0.9659258262890683122, 1.000000000000000000, 0.9659258262890683122, 1.000000000000000000, 0.9659258262890683122, 1.000000000000000000, 0.9659258262890683122, 1.000000000000000000, 0.9659258262890683122, 1.000000000000000000, 0.9659258262890683122, 1.000000000000000000, 0.9659258262890683122, 1.000000000000000000, 0.9659258262890683122, 1.000000000000000000, 0.9659258262890683122, 1.000000000000000000, 0.9659258262890683122, 1.000000000000000000, 0.9659258262890683122, 1.000000000000000000, 0.9659258262890683122, 1.000000000000000000, 0.9659258262890683122, 1.000000000000000000, 0.9659258262890683122, 1.000000000000000000, 0.9659258262890683122, 1.000000000000000000, 0.9659258262890683122, 1.000000000000000000, 0.9659258262890683122, 1.000000000000000000, 0.9659258262890683122, 1.000000000000000000, 0.9659258262890683122, 1.000000000000000000, 0.9659258262890683122, 1.000000000000000000, 0.9659258262890683122, 1.000000000000000000, 0.9659258262890683122, 1.000000000000000000, 0.9659258262890683122, 1.000000000000000000, 0.9659258262890683122, 1.000000000000000000, 0.9659258262890683122, 1.000000000000000000, 0.9659258262890683122, 1.000000000000000000, 0.9659258262890683122, 1.000000000000000000, 0.9659258262890683122, 1.000000000000000000, 0.9659258262890683122, 1.000000000000000000, 0.9659258262890683122, 1.000000000000000000, 0.9659258262890683122, 1.000000000000000000, 0.9659258262890683122, 1.000000000000000000, 0.9659258262890683122, 1.000000000000000000, 0.9659258262890683122, 1.000000000000000000, 0.9659258262890683122, 1.000000000000000000, 0.9659258262890683122, 1.000000000000000000, 0.9659258262890683122, 1.000000000000000000, 0.9659258262890683122, 1.000000000000000000, 0.9659258262890683122, 1.000000000000000000, 0.9659258262890683122, 1.000000000000000000, 0.9659258262890683122, 1.000000000000000000, 0.9659258262890683122, 1.000000000000000000, 0.9659258262890683122, 1.000000000000000000, 0.9659258262890683122, 1.000000000000000000, 0.9659258262890683122, 1.000000000000000000, 0.9659258262890683122, 1.000000000000000000, 0.9659258262890683122, 1.000000000000000000, 0.9659258262890683122, 1.000000000000000000, 0.9659258262890683122, 1.000000000000000000, 0.9659258262890683122, 1.000000000000000000, 0.9659258262890683122, 1.000000000000000000, 0.9659258262890683122, 1.000000000000000000, 0.9659258262890683122, 1.000000000000000000, 0.9659258262890683122, 1.000000000000000000, 0.9659258262890683122, 1.000000000000000000, 0.9659258262890683122, 1.000000000000000000, 0.9659258262890683122, 1.000000000000000000, 0.9659258262890683122, 1.000000000000000000, 0.9659258262890683122, 1.000000000000000000, 0.9659258262890683122, 1.000000000000000000, 0.9659258262890683122, 1.000000000000000000, 0.9659258262890683122, 1.000000000000000000, 0.9659258262890683122, 1.000000000000000000, 0.9659258262890683122, 1.000000000000000000, 0.9659258262890683122, 1.000000000000000000, 0.9659258262890683122, 1.000000000000000000, 0.9659258262890683122, 1.000000000000000000, 0.9659258262890683122, 1.000000000000000000, 0.9659258262890683122, 1.000000000000000000, 0.9659258262890683122, 1.000000000000000000, 0.9659258262890683122, 1.000000000000000000, 0.9659258262890683122, 1.000000000000000000, 0.9659258262890683122, 1.000000000000000000, 0.9659258262890683122, 1.000000000000000000, 0.9659258262890683122, 1.000000000000000000, 0.9659258262890683122, 1.000000000000000000, 0.9659258262890683122, 1.000000000000000000, 0.9659258262890683122, 1.000000000000000000, 0.9659258262890683122, 1.000000000000000000, 0.9659258262890683122, 1.000000000000000000, 0.9659258262890683122, 1.000000000000000000, 0.9659258262890683122, 1.000000000000000000, 0.9659258262890683122, 1.000000000000000000, 0.9659258262890683122, 1.000000000000000000, 0.9659258262890683122, 1.000000000000000000, 0.9659258262890683122, 1.000000000000000000, 0.9659258262890683122, 1.000000000000000000, 0.9659258262890683122, 1.000000000000000000, 0.9659258262890683122, 1.000000000000000000, 0.9659258262890683122, 1.000000000000000000, 0.9659258262890683122, 1.000000000000000000, 0.9659258262890683122, 1.000000000000000000, 0.9659258262890683122, 1.000000000000000000, 0.9659258262890683122, 1.000000000000000000, 0.9659258262890683122, 1.000000000000000000, 0.9659258262890683122, 1.000000000000000000, 0.9659258262890683122, 1.000000000000000000, 0.9659258262890683122, 1.000000000000000000, 0.9659258262890683122, 1.000000000000000000, 0.9659258262890683122, 1.000000000000000000, 0.9659258262890683122, 1.000000000000000000, 0.9659258262890683122, 1.000000000000000000, 0.9659258262890683122, 1.000000000000000000, 0.9659258262890683122, 1.000000000000000000, 0.9659258262890683122, 1.000000000000000000, 0.9659258262890683122, 1.000000000000000000, 0.9659258262890683122, 1.000000000000000000, 0.9659258262890683122, 1.000000000000000000, 0.9659258262890683122, 1.000000000000000000, 0.9659258262890683122, 1.000000000000000000, 0.9659258262890683122, 1.000000000000000000, 0.9659258262890683122, 1.000000000000000000, 0.9659258262890683122, 1.000000000000000000, 0.9659258262890683122, 1.000000000000000000, 0.9659258262890683122, 1.000000000000000000, 0.9659258262890683122, 1.000000000000000000, 0.9659258262890683122, 1.000000000000000000, 0.9659258262890683122, 1.000000000000000000, 0.9659258262890683122, 1.000000000000000000, 0.9659258262890683122, 1.000000000000000000, 0.9659258262890683122, 1.000000000000000000, 0.9659258262890683122, 1.000000000000000000, 0.9659258262890683122, 1.000000000000000000, 0.9659258262890683122, 1.000000000000000000, 0.9659258262890683122, 1.000000000000000000, 0.9659258262890683122, 1.000000000000000000, 0.9659258262890683122, 1.000000000000000000, 0.9659258262890683122, 1.000000000000000000, 0.9659258262890683122, 1.000000000000000000, 0.9659258262890683122, 1.000000000000000000, 0.9659258262890683122, 1.000000000000000000, 0.9659258262890683122, 1.000000000000000000, 0.9659258262890683122, 1.000000000000000000, 0.9659258262890683122, 1.000000000000000000, 0.9659258262890683122, 1.000000000000000000, 0.9659258262890683122, 1.000000000000000000, 0.9659258262890683122, 1.000000000000000000, 0.9659258262890683122, 1.000000000000000000, 0.9659258262890683122, 1.000000000000000000, 0.9659258262890683122, 1.000000000000000000, 0.9659258262890683122, 1.000000000000000000, 0.9659258262890683122, 1.000000000000000000, 0.9659258262890683122, 1.000000000000000000, 0.9659258262890683122, 1.000000000000000000, 0.9659258262890683122, 1.000000000000000000, 0.9659258262890683122, 1.000000000000000000, 0.9659258262890683122, 1.000000000000000000, 0.9659258262890683122, 1.000000000000000000, 0.9659258262890683122, 1.000000000000000000, 0.9659258262890683122, 1.000000000000000000, 0.9659258262890683122, 1.000000000000000000, 0.9659258262890683122, 1.000000000000000000, 0.9659258262890683122, 1.000000000000000000, 0.9659258262890683122, 1.000000000000000000, 0.9659258262890683122, 1.000000000000000000, 0.9659258262890683122, 1.000000000000000000, 0.9659258262890683122, 1.000000000000000000, 0.9659258262890683122, 1.000000000000000000, 0.9659258262890683122, 1.000000000000000000, 0.9659258262890683122, 1.000000000000000000, 0.9659258262890683122, 1.000000000000000000, 0.9659258262890683122, 1.000000000000000000, 0.9659258262890683122, 1.000000000000000000, 0.9659258262890683122, 1.000000000000000000, 0.9659258262890683122, 1.000000000000000000, 0.9659258262890683122, 1.000000000000000000, 0.9659258262890683122, 1.000000000000000000, 0.9659258262890683122, 1.000000000000000000, 0.9659258262890683122, 1.000000000000000000, 0.9659258262890683122, 1.000000000000000000, 0.9659258262890683122, 1.000000000000000000, 0.9659258262890683122, 1.000000000000000000, 0.9659258262890683122, 1.000000000000000000, 0.9659258262890683122, 1.000000000000000000, 0.9659258262890683122, 1.000000000000000000, 0.9659258262890683122, 1.000000000000000000, 0.9659258262890683122, 1.000000000000000000, 0.9659258262890683122, 1.000000000000000000, 0.9659258262890683122, 1.000000000000000000, 0.9659258262890683122, 1.000000000000000000, 0.9659258262890683122, 1.000000000000000000, 0.9659258262890683122, 1.000000000000000000, 0.9659258262890683122, 1.000000000000000000, 0.9659258262890683122, 1.000000000000000000, 0.9659258262890683122, 1.000000000000000000, 0.9659258262890683122, 1.000000000000000000, 0.9659258262890683122, 1.000000000000000000, 0.9659258262890683122, 1.000000000000000000, 0.9659258262890683122, 1.000000000000000000, 0.9659258262890683122, 1.000000000000000000, 0.9659258262890683122, 1.000000000000000000, 0.9659258262890683122, 1.000000000000000000, 0.9659258262890683122, 1.000000000000000000, 0.9659258262890683122, 1.000000000000000000) ) ) 
 REPRESENTATION_ITEM ( '' )  SURFACE ( )  );
#38830 = CARTESIAN_POINT ( 'NONE',  ( -0.1049643490035302024, -0.3917322834645671215, -0.6942257217847765949 ) ) ;
#38832 = CARTESIAN_POINT ( 'NONE',  ( -0.3227188174119199338, 1.189353863002643896, 1.964709871421637555 ) ) ;
#38831 = CARTESIAN_POINT ( 'NONE',  ( 0.8661417322834653598, -0.1870078740157479769, 0.4822834645669291653 ) ) ;
#38833 = CARTESIAN_POINT ( 'NONE',  ( -1.699475065616797398, 0.1771653543307087630, 0.09757992244046791164 ) ) ;
#38834 = CARTESIAN_POINT ( 'NONE',  ( 0.3871391076115492380, -0.08942795157528024563, -0.3641732283464568787 ) ) ;
#38835 = CARTESIAN_POINT ( 'NONE',  ( 0.6889763779527566800, -0.5400638737290844871, 0.3530559997133364547 ) ) ;
#38836 = CARTESIAN_POINT ( 'NONE',  ( -0.2318981092368783692, 0.1830245018656607436, 0.1465342031617538066 ) ) ;
#38837 = CARTESIAN_POINT ( 'NONE',  ( -1.010498687664041384, -0.3690944881889765550, -0.3153832671262227771 ) ) ;
#38838 = CARTESIAN_POINT ( 'NONE',  ( -0.5905511811023615998, 0.2952755905511811885, 0.000000000000000000 ) ) ;
#38839 = CARTESIAN_POINT ( 'NONE',  ( -1.653543307086613234, -0.1870078740157479769, 0.3641732283464567677 ) ) ;
#38840 = CARTESIAN_POINT ( 'NONE',  ( -1.227034120734907585, 0.2952755905511811885, 0.1292274648535926551 ) ) ;
#38841 = CARTESIAN_POINT ( 'NONE',  ( 0.9645669291338591078, -0.5400638737290845981, -0.3530559997133363437 ) ) ;
#38842 = CARTESIAN_POINT ( 'NONE',  ( -1.148293963254592542, 0.1771653543307087630, 0.09757992244046791164 ) ) ;
#38843 = LINE ( 'NONE', #58193, #11480 ) ;
#38844 = CARTESIAN_POINT ( 'NONE',  ( 1.194225721784777594, -0.4281496062992127816, -0.4176697321401328100 ) ) ;
#38845 = CARTESIAN_POINT ( 'NONE',  ( -0.4091458600556402980, -0.2362204724409451284, -2.648950131233595684 ) ) ;
#38846 = CARTESIAN_POINT ( 'NONE',  ( 0.000000000000000000, 2.755905511811024056, 0.000000000000000000 ) ) ;
#38847 = CARTESIAN_POINT ( 'NONE',  ( 1.377952755905512472, 0.2952755905511811885, 0.000000000000000000 ) ) ;
#38848 = CARTESIAN_POINT ( 'NONE',  ( -1.108923884514435132, -0.2845877964562159024, 0.3641732283464567677 ) ) ;
#38849 = CARTESIAN_POINT ( 'NONE',  ( 1.169169330835494014, -5.140490538625777863E-17, -0.3627989612356145588 ) ) ;
#38850 = CARTESIAN_POINT ( 'NONE',  ( -1.423884514435694859, -0.08942795157528024563, -0.3641732283464568787 ) ) ;
#38851 = CARTESIAN_POINT ( 'NONE',  ( -0.4790026246719152336, -0.08942795157528024563, -0.3641732283464568787 ) ) ;
#38852 = CARTESIAN_POINT ( 'NONE',  ( -1.587926509186350810, -0.3690944881889763329, 0.3153832671262228327 ) ) ;
#38853 = CARTESIAN_POINT ( 'NONE',  ( 0.7808398950131240079, -0.2845877964562159024, 0.3641732283464567677 ) ) ;
#38854 = CARTESIAN_POINT ( 'NONE',  ( 0.3608923884514443348, -0.6692913385826771977, 0.1292274648535927661 ) ) ;
#38855 = CARTESIAN_POINT ( 'NONE',  ( 1.318897637795276356, 0.1660481256975883668, -0.3530559997133364547 ) ) ;
#38856 = CARTESIAN_POINT ( 'NONE',  ( 0.5511811023622055217, -0.1870078740157479769, 0.4822834645669291653 ) ) ;
#38857 = CARTESIAN_POINT ( 'NONE',  ( 0.3608923884514443348, 0.1771653543307087075, -0.09757992244046823083 ) ) ;
#38858 = CARTESIAN_POINT ( 'NONE',  ( -1.423884514435694859, -0.05778040916215560624, -0.4822834645669293319 ) ) ;
#38859 = CARTESIAN_POINT ( 'NONE',  ( -1.305774278215222184, 0.2952755905511811885, 0.1292274648535926551 ) ) ;
#38860 = CARTESIAN_POINT ( 'NONE',  ( -0.6561679790026240244, -0.6046776061558807314, 0.2411417322834647770 ) ) ;
#38861 = CARTESIAN_POINT ( 'NONE',  ( -0.3460692066303958092, -0.1998031496062994683, -0.2099737532808399199 ) ) ;
#38862 = CARTESIAN_POINT ( 'NONE',  ( -0.3034767870060118278, 1.228735513192457551, 0.07815720285223907993 ) ) ;
#38863 = CARTESIAN_POINT ( 'NONE',  ( -0.07874015748031421014, -0.1870078740157480879, -0.4822834645669291653 ) ) ;
#38864 = CARTESIAN_POINT ( 'NONE',  ( 1.122047244094488860, 0.07958543189024085140, 0.2665933059059887866 ) ) ;
#38865 = CARTESIAN_POINT ( 'NONE',  ( -0.2230971128608915943, 0.05413385826771666132, 0.4176697321401328100 ) ) ;
#38867 = VECTOR ( 'NONE', #948, 39.37007874015748143 ) ;
#38866 = CARTESIAN_POINT ( 'NONE',  ( 0.3608923884514443348, 0.2952755905511810774, -0.1292274648535930714 ) ) ;
#38868 = EDGE_CURVE ( 'NONE', #41210, #39595, #47906, .T. ) ;
#38869 = CARTESIAN_POINT ( 'NONE',  ( 4.893765752498283924E-17, -0.3996062992125986035, -2.755905511811023612 ) ) ;
#38870 = CARTESIAN_POINT ( 'NONE',  ( -0.2891555358219908833, -0.2891555358219912164, -1.791338582677165725 ) ) ;
#38871 = CARTESIAN_POINT ( 'NONE',  ( 0.1958661417322836440, -0.3392501089628017219, -0.3989501312335957950 ) ) ;
#38872 = CARTESIAN_POINT ( 'NONE',  ( 0.2710150415003133029, -0.1175404812240907343, 5.835005246025582792 ) ) ;
#38873 = CARTESIAN_POINT ( 'NONE',  ( -0.3392501089628019995, 0.1958661417322832277, -1.120734908136482799 ) ) ;
#38874 = ADVANCED_FACE ( 'NONE', ( #67998 ), #73903, .F. ) ;
#38875 = CARTESIAN_POINT ( 'NONE',  ( -1.023622047244094002, -0.1870078740157480601, -0.3641732283464567677 ) ) ;
#38876 = CARTESIAN_POINT ( 'NONE',  ( -0.3917322834645669549, -0.1049643490035306603, -1.140419947506561282 ) ) ;
#38877 = CARTESIAN_POINT ( 'NONE',  ( -1.174540682414697335, -0.3162353388693409650, -0.4822834645669289433 ) ) ;
#38878 = CARTESIAN_POINT ( 'NONE',  ( -0.2867679344610366554, 0.2867679344610365444, 0.2152424128947000026 ) ) ;
#38879 = CARTESIAN_POINT ( 'NONE',  ( 0.6036745406824154392, 0.2306618581243847221, -0.2411417322834647770 ) ) ;
#38880 = CARTESIAN_POINT ( 'NONE',  ( 1.154855643044620184, 0.2306618581243847221, -0.2411417322834647770 ) ) ;
#38881 = CARTESIAN_POINT ( 'NONE',  ( 0.8136482939632553313, 0.2306618581243848609, 0.2411417322834645549 ) ) ;
#38882 = CARTESIAN_POINT ( 'NONE',  ( -0.4091458600556402980, -0.2362204724409451284, -2.729658792650918375 ) ) ;
#38883 = CARTESIAN_POINT ( 'NONE',  ( 0.2925321140481932369, -0.2925321140481932369, -2.618110236220472675 ) ) ;
#38884 = CARTESIAN_POINT ( 'NONE',  ( -0.2867679344610367109, 0.2867679344610365444, -1.276266034941944127 ) ) ;
#38885 = FACE_OUTER_BOUND ( 'NONE', #20564, .T. ) ;
#38886 = CARTESIAN_POINT ( 'NONE',  ( 0.4461942257217855201, -0.6046776061558807314, 0.2411417322834647770 ) ) ;
#38887 = CARTESIAN_POINT ( 'NONE',  ( 0.3083989501312343062, -0.3162353388693405765, 0.4822834645669290543 ) ) ;
#38888 = CARTESIAN_POINT ( 'NONE',  ( 0.9973753280839902091, 0.1283753931104746893, -0.1820866141732285504 ) ) ;
#38889 = CARTESIAN_POINT ( 'NONE',  ( 1.161417322834646493, -0.5400638737290844871, 0.3530559997133364547 ) ) ;
#38890 = CARTESIAN_POINT ( 'NONE',  ( 0.1958661417322836440, -0.3392501089628017219, -0.01902887139107619849 ) ) ;
#38891 = CARTESIAN_POINT ( 'NONE',  ( 0.1837270341207354329, 0.2306618581243848609, 0.2411417322834645549 ) ) ;
#38892 = CARTESIAN_POINT ( 'NONE',  ( 0.9317585301837276734, 0.05413385826771626580, -0.4176697321401330321 ) ) ;
#38893 = CARTESIAN_POINT ( 'NONE',  ( 0.3215223097112867578, -0.3162353388693409650, -0.4822834645669289433 ) ) ;
#38894 = CARTESIAN_POINT ( 'NONE',  ( 1.312335958005250269, -0.5023911411419708095, 0.1820866141732285504 ) ) ;
#38895 = CARTESIAN_POINT ( 'NONE',  ( -1.095800524934382292, -0.05778040916215522460, 0.4822834645669289988 ) ) ;
#38896 = CARTESIAN_POINT ( 'NONE',  ( -1.010498687664041384, -0.4281496062992127816, -0.4176697321401328100 ) ) ;
#38897 = CARTESIAN_POINT ( 'NONE',  ( 1.220472440944882386, -0.6692913385826771977, 8.415575281601705876E-17 ) ) ;
#38898 = CARTESIAN_POINT ( 'NONE',  ( -0.2867679344610364334, -0.2867679344610367109, -0.6161417322834646937 ) ) ;
#38899 = CARTESIAN_POINT ( 'NONE',  ( -0.3392501089628017219, -0.1958661417322836718, -2.091863517060367439 ) ) ;
#38900 = CARTESIAN_POINT ( 'NONE',  ( -0.1049643490035307020, 0.3917322834645669549, -2.518372703412073754 ) ) ;
#38901 = ORIENTED_EDGE ( 'NONE', *, *, #65412, .T. ) ;
#38902 = CARTESIAN_POINT ( 'NONE',  ( 0.1070741851644053527, 0.3996062992125986590, 0.006561679790026227546 ) ) ;
#38903 = VERTEX_POINT ( 'NONE', #60837 ) ;
#38904 = CARTESIAN_POINT ( 'NONE',  ( 1.601049868766404982, -0.6046776061558809534, -0.2411417322834644161 ) ) ;
#38905 = CARTESIAN_POINT ( 'NONE',  ( 1.049868766404200127, -0.5023911411419708095, -0.1820866141732282451 ) ) ;
#38906 = CARTESIAN_POINT ( 'NONE',  ( -0.1998031496062991907, -0.3460692066303959757, -1.640419947506561726 ) ) ;
#38907 = CARTESIAN_POINT ( 'NONE',  ( 1.174540682414699111, -0.2845877964562159024, 0.3641732283464567677 ) ) ;
#38908 = CARTESIAN_POINT ( 'NONE',  ( 2.795275590551181466, 2.001539355558160871, 0.000000000000000000 ) ) ;
#38909 = LINE ( 'NONE', #33012, #34251 ) ;
#38910 = CARTESIAN_POINT ( 'NONE',  ( 0.4091458600556404646, -0.2362204724409448231, -1.207349081364829324 ) ) ;
#38911 = CARTESIAN_POINT ( 'NONE',  ( 0.3917322834645669549, 0.1049643490035304660, -0.8392388451443569819 ) ) ;
#38912 = CARTESIAN_POINT ( 'NONE',  ( -1.076115485564303809, -0.5023911411419708095, -0.1820866141732282451 ) ) ;
#38913 = CARTESIAN_POINT ( 'NONE',  ( 1.601049868766404982, 0.2306618581243848609, 0.2411417322834645549 ) ) ;
#38914 = CARTESIAN_POINT ( 'NONE',  ( -1.318897637795274802, 0.1660481256975885056, 0.3530559997133364547 ) ) ;
#38915 = CARTESIAN_POINT ( 'NONE',  ( 0.2362204724409456558, -0.1870078740157480879, -0.4822834645669291653 ) ) ;
#38916 = CARTESIAN_POINT ( 'NONE',  ( 1.332020997375328974, -0.05778040916215560624, -0.4822834645669293319 ) ) ;
#38917 = ORIENTED_EDGE ( 'NONE', *, *, #59271, .F. ) ;
#38918 = CARTESIAN_POINT ( 'NONE',  ( -1.119414574269209650, 1.069244457019925765, -0.07832840781635802552 ) ) ;
#38919 = DIRECTION ( 'NONE',  ( 1.000000000000000000, 0.000000000000000000, 0.000000000000000000 ) ) ;
#38920 = CARTESIAN_POINT ( 'NONE',  ( 0.4724409448818898682, 2.892866454678787531E-17, -2.637795275590551380 ) ) ;
#38921 = DIRECTION ( 'NONE',  ( 0.000000000000000000, -1.000000000000000000, 0.000000000000000000 ) ) ;
#38922 = CARTESIAN_POINT ( 'NONE',  ( -1.023622047244093558, -0.1870078740157479769, 0.3641732283464567677 ) ) ;
#38923 = DIRECTION ( 'NONE',  ( 3.096699300667737957E-16, -1.000000000000000000, 0.000000000000000000 ) ) ;
#38924 = CARTESIAN_POINT ( 'NONE',  ( 0.6824146981627303710, -0.6046776061558807314, 0.2411417322834647770 ) ) ;
#38925 = ORIENTED_EDGE ( 'NONE', *, *, #82772, .F. ) ;
#38927 = CYLINDRICAL_SURFACE ( 'NONE', #80147, 0.07874015748031495954 ) ;
#38926 = CARTESIAN_POINT ( 'NONE',  ( -1.603475055217291612, 0.5037964761735302943, 0.04573490813648253134 ) ) ;
#38928 = CARTESIAN_POINT ( 'NONE',  ( 1.391076115485564868, 0.2306618581243847221, -0.2411417322834647770 ) ) ;
#38929 = CARTESIAN_POINT ( 'NONE',  ( -1.528871391076114250, 0.2952755905511810774, -0.1292274648535930714 ) ) ;
#38930 = CARTESIAN_POINT ( 'NONE',  ( 0.3917322834645668994, 0.1049643490035304522, -0.8346263535094994301 ) ) ;
#38931 = CARTESIAN_POINT ( 'NONE',  ( -0.2362204724409442680, -0.1870078740157480601, -0.3641732283464567677 ) ) ;
#38932 = CARTESIAN_POINT ( 'NONE',  ( -1.305774278215222184, 0.1771653543307087630, 0.09757992244046791164 ) ) ;
#38933 = CARTESIAN_POINT ( 'NONE',  ( -0.3503937007874015630, 0.3733313776025732333, -0.01968503937007903132 ) ) ;
#38934 = CARTESIAN_POINT ( 'NONE',  ( -0.5183727034120726440, 0.1771653543307087630, 0.09757992244046791164 ) ) ;
#38935 = CARTESIAN_POINT ( 'NONE',  ( 0.2690288713910767848, -0.5511811023622048555, -0.09757992244046775898 ) ) ;
#38936 = CARTESIAN_POINT ( 'NONE',  ( 0.1246719160104994284, -0.6692913385826771977, 0.1292274648535927661 ) ) ;
#38937 = CARTESIAN_POINT ( 'NONE',  ( -1.049868766404198794, -0.5023911411419708095, 0.1820866141732285504 ) ) ;
#38938 = CARTESIAN_POINT ( 'NONE',  ( -0.1049643490035307020, 0.3917322834645669549, -2.833333333333333037 ) ) ;
#38939 = CARTESIAN_POINT ( 'NONE',  ( 0.9973753280839902091, 0.2306618581243847221, -0.2411417322834647770 ) ) ;
#38940 = CARTESIAN_POINT ( 'NONE',  ( -1.240157480314959759, -0.5400638737290845981, -0.3530559997133363437 ) ) ;
#38941 = CARTESIAN_POINT ( 'NONE',  ( -0.4091458600556405756, 0.2362204724409446288, -1.047900262467191590 ) ) ;
#38942 = CARTESIAN_POINT ( 'NONE',  ( -0.3937007874015740483, -0.1870078740157480879, -0.4822834645669291653 ) ) ;
#38943 = CARTESIAN_POINT ( 'NONE',  ( -0.9120734908136475250, -0.6692913385826773087, -0.1292274648535924053 ) ) ;
#38944 = CARTESIAN_POINT ( 'NONE',  ( 0.7480314960629927956, 0.1771653543307087630, 0.000000000000000000 ) ) ;
#38945 = CARTESIAN_POINT ( 'NONE',  ( -0.3083989501312330295, -0.08942795157527998196, 0.3641732283464567121 ) ) ;
#38946 = CARTESIAN_POINT ( 'NONE',  ( -0.4658792650918627265, -0.05778040916215522460, 0.4822834645669289988 ) ) ;
#38947 = CARTESIAN_POINT ( 'NONE',  ( -1.515748031496062076, -0.5400638737290844871, 0.3530559997133364547 ) ) ;
#38948 = DIRECTION ( 'NONE',  ( 0.6236670536615140925, 0.6323634944239162614, 0.4595169388576875180 ) ) ;
#38949 = CARTESIAN_POINT ( 'NONE',  ( 1.476377952755906442, -0.4536011799217367080, 0.2665933059059888421 ) ) ;
#38950 = CARTESIAN_POINT ( 'NONE',  ( -1.325459317585300889, 0.05413385826771666132, 0.4176697321401328100 ) ) ;
#38951 = CARTESIAN_POINT ( 'NONE',  ( -1.318897637795274802, -0.5400638737290845981, -0.3530559997133363437 ) ) ;
#38952 = VERTEX_POINT ( 'NONE', #48620 ) ;
#38953 = CARTESIAN_POINT ( 'NONE',  ( -0.2925321140481930149, -0.2925321140481933480, -2.498031496062992574 ) ) ;
#38954 = CARTESIAN_POINT ( 'NONE',  ( -1.030183727034119867, -0.2845877964562159024, 0.3641732283464567677 ) ) ;
#38955 = CARTESIAN_POINT ( 'NONE',  ( 0.8202099737532813073, 0.2952755905511811885, 0.1292274648535926551 ) ) ;
#38956 = CARTESIAN_POINT ( 'NONE',  ( -0.8923884514435688198, 0.1283753931104746893, -0.1820866141732285504 ) ) ;
#38957 = CARTESIAN_POINT ( 'NONE',  ( 0.3996062992125985480, 2.446882876249141654E-17, -1.297244094488189115 ) ) ;
#38958 = CARTESIAN_POINT ( 'NONE',  ( -0.9842519685039365918, -0.6692913385826771977, 8.415575281601705876E-17 ) ) ;
#38959 = CARTESIAN_POINT ( 'NONE',  ( 0.7874015748031503170, -0.1870078740157480879, -0.4822834645669291653 ) ) ;
#38960 = CARTESIAN_POINT ( 'NONE',  ( 0.6889763779527566800, -0.5400638737290844871, 0.3530559997133364547 ) ) ;
#38961 = DIRECTION ( 'NONE',  ( -0.7071067811865472397, 0.000000000000000000, -0.7071067811865476838 ) ) ;
#38962 = CARTESIAN_POINT ( 'NONE',  ( -1.640419947506561060, -0.3690944881889765550, -0.3153832671262227771 ) ) ;
#38964 = EDGE_CURVE ( 'NONE', #73460, #28061, #34469, .T. ) ;
#38963 = CARTESIAN_POINT ( 'NONE',  ( 0.1070741851644054637, -0.3996062992125984925, -0.4770341207349080848 ) ) ;
#38965 = CARTESIAN_POINT ( 'NONE',  ( -0.1998031496062994683, 0.3460692066303958092, -0.9580052493438320216 ) ) ;
#38966 = CARTESIAN_POINT ( 'NONE',  ( -0.2891555358219908833, -0.2891555358219912164, -0.8464566929133858775 ) ) ;
#38967 = DIRECTION ( 'NONE',  ( -1.734723475976806848E-16, -1.000000000000000000, 0.000000000000000000 ) ) ;
#38968 = CARTESIAN_POINT ( 'NONE',  ( 0.9908136482939640111, -0.5511811023622046335, 0.09757992244046803654 ) ) ;
#38969 = CARTESIAN_POINT ( 'NONE',  ( 0.3740157480314966754, 0.07958543189024071263, -0.2665933059059888421 ) ) ;
#38970 = CARTESIAN_POINT ( 'NONE',  ( 0.2887139107611556010, -0.6046776061558807314, 0.2411417322834647770 ) ) ;
#38971 = CARTESIAN_POINT ( 'NONE',  ( 1.266404199475066328, -0.05778040916215522460, 0.4822834645669289988 ) ) ;
#38972 = CARTESIAN_POINT ( 'NONE',  ( 0.1974969037888704704, 0.3420746716998660508, -1.323490813648294129 ) ) ;
#38973 = CARTESIAN_POINT ( 'NONE',  ( 0.4921259842519691285, -0.4536011799217368745, -0.2665933059059886201 ) ) ;
#38974 = CARTESIAN_POINT ( 'NONE',  ( -0.6889763779527552368, 0.1660481256975885056, 0.3530559997133364547 ) ) ;
#38975 = CARTESIAN_POINT ( 'NONE',  ( -1.279527559055116948, 0.1660481256975883668, -0.3530559997133364547 ) ) ;
#38976 = CARTESIAN_POINT ( 'NONE',  ( 0.6430446194225729606, -0.4281496062992127816, -0.4176697321401328100 ) ) ;
#38977 = CARTESIAN_POINT ( 'NONE',  ( -0.3458507752293909498, 0.3458507752293907833, -1.594488188976378229 ) ) ;
#38978 = CARTESIAN_POINT ( 'NONE',  ( 0.3996062992125986035, -0.1070741851644053111, -2.631233595800524405 ) ) ;
#38979 = ORIENTED_EDGE ( 'NONE', *, *, #25459, .T. ) ;
#38980 = VERTEX_POINT ( 'NONE', #80229 ) ;
#38981 = CARTESIAN_POINT ( 'NONE',  ( -1.246719160104986512, 0.05413385826771666132, 0.4176697321401328100 ) ) ;
#38982 = CARTESIAN_POINT ( 'NONE',  ( -0.6430446194225712953, 0.05413385826771626580, -0.4176697321401330321 ) ) ;
#38984 = CARTESIAN_POINT ( 'NONE',  ( -0.9251968503937002541, -0.5400638737290845981, -0.3530559997133363437 ) ) ;
#38983 = CARTESIAN_POINT ( 'NONE',  ( -0.8989501312335946848, -0.5511811023622046335, 0.09757992244046803654 ) ) ;
#38985 = CARTESIAN_POINT ( 'NONE',  ( -0.1958661417322834497, -0.3392501089628018884, -2.035413755084302778 ) ) ;
#38986 = CARTESIAN_POINT ( 'NONE',  ( 0.2925321140481932369, 0.2925321140481932369, -2.734251968503936148 ) ) ;
#38987 = CARTESIAN_POINT ( 'NONE',  ( 1.607611548556431069, -0.6692913385826773087, -0.1292274648535924053 ) ) ;
#38988 = CARTESIAN_POINT ( 'NONE',  ( -1.115485564304461219, -0.4281496062992124485, 0.4176697321401328655 ) ) ;
#38989 = CARTESIAN_POINT ( 'NONE',  ( 0.1706036745406830368, 0.05413385826771666132, 0.4176697321401328100 ) ) ;
#38990 = CARTESIAN_POINT ( 'NONE',  ( -0.6430446194225712953, 0.05413385826771626580, -0.4176697321401330321 ) ) ;
#38991 =( BOUNDED_CURVE ( )  B_SPLINE_CURVE ( 2, ( #74335, #17917, #30530, #31341, #69662, #23798, #25022, #49877, #57007, #68020, #4036, #17100, #36024 ),
 .UNSPECIFIED., .F., .F. ) 
 B_SPLINE_CURVE_WITH_KNOTS ( ( 3, 2, 2, 2, 2, 2, 3 ),
 ( 0.4922150842069599741, 0.4924242424242424310, 0.4962121212121212155, 0.5000000000000000000, 0.5037878787878787845, 0.5075757575757575690, 0.5077849157930400814 ),
 .UNSPECIFIED. ) 
 CURVE ( )  GEOMETRIC_REPRESENTATION_ITEM ( )  RATIONAL_B_SPLINE_CURVE ( ( 0.9964447847208428577, 0.9981185001348096275, 1.000000000000000000, 0.9659258262890683122, 1.000000000000000000, 0.9659258262890683122, 1.000000000000000000, 0.9659258262890683122, 1.000000000000000000, 0.9659258262890683122, 1.000000000000000000, 0.9981185001348091834, 0.9964447847208420805 ) ) 
 REPRESENTATION_ITEM ( '' )  );
#38992 = CARTESIAN_POINT ( 'NONE',  ( 0.1049643490035304938, -0.3917322834645669549, -1.337270341207349000 ) ) ;
#38993 = CARTESIAN_POINT ( 'NONE',  ( -0.9383202099737524282, -0.2845877964562161244, -0.3641732283464567121 ) ) ;
#38994 = VERTEX_POINT ( 'NONE', #22545 ) ;
#38995 = CARTESIAN_POINT ( 'NONE',  ( -0.1974969037888703871, -0.3420746716998661063, -1.797900262467191590 ) ) ;
#38996 = ORIENTED_EDGE ( 'NONE', *, *, #66014, .T. ) ;
#38997 = CARTESIAN_POINT ( 'NONE',  ( -1.548556430446193399, 0.1283753931104748280, 0.1820866141732283561 ) ) ;
#38998 = CARTESIAN_POINT ( 'NONE',  ( -1.095800524934382292, -0.05778040916215522460, 0.4822834645669289988 ) ) ;
#38999 = CARTESIAN_POINT ( 'NONE',  ( -1.364829396325458521, -0.6046776061558807314, 0.2411417322834647770 ) ) ;
#39000 = CARTESIAN_POINT ( 'NONE',  ( -0.3996062992125986035, -7.340648628747425578E-17, -0.3543307086614173040 ) ) ;
#39001 = CARTESIAN_POINT ( 'NONE',  ( -1.246719160104986512, 0.05413385826771666132, 0.4176697321401328100 ) ) ;
#39002 = CARTESIAN_POINT ( 'NONE',  ( -1.259842519685038686, -0.1870078740157479769, 0.4822834645669291653 ) ) ;
#39003 = CARTESIAN_POINT ( 'NONE',  ( -0.6986524979670485358, -2.191421614605370878E-15, 0.4445507791589071167 ) ) ;
#39004 = CARTESIAN_POINT ( 'NONE',  ( -0.8005249343832011588, 0.05413385826771626580, -0.4176697321401330321 ) ) ;
#39005 = CARTESIAN_POINT ( 'NONE',  ( 0.09842519685039434474, 0.07958543189024085140, 0.2665933059059887866 ) ) ;
#39006 = CARTESIAN_POINT ( 'NONE',  ( 0.4724409448818898682, 2.892866454678787531E-17, -0.9055118110236221041 ) ) ;
#39007 = CARTESIAN_POINT ( 'NONE',  ( 0.3917322834645670104, 2.398668435337828261E-17, -0.2027559055118111353 ) ) ;
#39008 = CARTESIAN_POINT ( 'NONE',  ( -0.2690288713910754526, 0.1771653543307087075, -0.09757992244046823083 ) ) ;
#39009 = CARTESIAN_POINT ( 'NONE',  ( -0.8858267716535425107, -0.5400638737290844871, 0.3530559997133364547 ) ) ;
#39010 = CARTESIAN_POINT ( 'NONE',  ( 1.437007874015748810, 0.1660481256975885056, 0.3530559997133364547 ) ) ;
#39011 = CARTESIAN_POINT ( 'NONE',  ( -0.3740157480314953431, 0.1660481256975885056, 0.3530559997133364547 ) ) ;
#39012 = ORIENTED_EDGE ( 'NONE', *, *, #16262, .T. ) ;
#39013 = ORIENTED_EDGE ( 'NONE', *, *, #34666, .F. ) ;
#39014 = CARTESIAN_POINT ( 'NONE',  ( -0.1998031496062991630, -0.3460692066303959202, -2.189632545931758489 ) ) ;
#39015 = CARTESIAN_POINT ( 'NONE',  ( -1.167979002624671470, 0.05413385826771666132, 0.4176697321401328100 ) ) ;
#39016 = CARTESIAN_POINT ( 'NONE',  ( 1.391076115485564868, -0.6046776061558807314, 0.2411417322834647770 ) ) ;
#39017 = CARTESIAN_POINT ( 'NONE',  ( -1.515748031496062076, 0.07958543189024071263, -0.2665933059059888421 ) ) ;
#39018 = CARTESIAN_POINT ( 'NONE',  ( -1.496062992125983815, -0.1870078740157480879, -0.4822834645669291653 ) ) ;
#39019 = CARTESIAN_POINT ( 'NONE',  ( -0.3458507752293906723, -0.3458507752293910609, -0.6889763779527556808 ) ) ;
#39020 = CARTESIAN_POINT ( 'NONE',  ( 2.105021046755494396, 1.366082762360720348, 0.4426340671871338284 ) ) ;
#39021 = CARTESIAN_POINT ( 'NONE',  ( 0.3392501089628018329, 0.1958661417322835607, -0.2808398950131232863 ) ) ;
#39022 = CARTESIAN_POINT ( 'NONE',  ( -0.1958661417322834220, -0.3392501089628018884, -2.197506561679789971 ) ) ;
#39023 = CARTESIAN_POINT ( 'NONE',  ( -0.06561679790026180015, 0.05413385826771666132, 0.4176697321401328100 ) ) ;
#39024 = CARTESIAN_POINT ( 'NONE',  ( -1.535433070866141225, -0.5511811023622047445, 6.969142054262312111E-17 ) ) ;
#39025 = CARTESIAN_POINT ( 'NONE',  ( -0.6758530183727028406, -0.6692913385826773087, -0.1292274648535924053 ) ) ;
#39026 = CARTESIAN_POINT ( 'NONE',  ( -0.4091458600556405756, 0.2362204724409446288, -2.780183727034120977 ) ) ;
#39028 = CARTESIAN_POINT ( 'NONE',  ( -0.2246346060905426156, 0.02791078216816064370, 0.4328096321851915285 ) ) ;
#39027 = CARTESIAN_POINT ( 'NONE',  ( -1.174540682414697335, -0.3162353388693409650, -0.4822834645669289433 ) ) ;
#39029 = CARTESIAN_POINT ( 'NONE',  ( -1.017060367454067249, -0.3162353388693409650, -0.4822834645669289433 ) ) ;
#39030 = CARTESIAN_POINT ( 'NONE',  ( -0.2296587926509179312, -0.3162353388693409650, -0.4822834645669289433 ) ) ;
#39031 = CARTESIAN_POINT ( 'NONE',  ( -0.3420746716998662729, 0.1974969037888702206, -2.622703412073491336 ) ) ;
#39032 = CARTESIAN_POINT ( 'NONE',  ( 0.9842519685039375910, 0.1771653543307087630, 0.000000000000000000 ) ) ;
#39033 = CARTESIAN_POINT ( 'NONE',  ( -0.7086614173228339419, -0.1870078740157480601, -0.3641732283464567677 ) ) ;
#39034 = DIRECTION ( 'NONE',  ( 1.000000000000000000, 0.000000000000000000, 0.000000000000000000 ) ) ;
#39035 = CARTESIAN_POINT ( 'NONE',  ( 0.7939632545931766261, -0.2845877964562161244, -0.3641732283464567121 ) ) ;
#39036 = CARTESIAN_POINT ( 'NONE',  ( 1.332020997375328974, -0.08942795157528024563, -0.3641732283464568787 ) ) ;
#39037 = CARTESIAN_POINT ( 'NONE',  ( 1.522309711286089939, -0.6046776061558809534, -0.2411417322834644161 ) ) ;
#39038 = CARTESIAN_POINT ( 'NONE',  ( 0.2624671916010504757, 0.1283753931104748280, 0.1820866141732283561 ) ) ;
#39039 = CARTESIAN_POINT ( 'NONE',  ( 0.2867679344610365999, -0.2867679344610365444, -1.507874015748031260 ) ) ;
#39040 = CARTESIAN_POINT ( 'NONE',  ( -0.8727034120734901146, -0.3162353388693405765, 0.4822834645669290543 ) ) ;
#39041 = CARTESIAN_POINT ( 'NONE',  ( 1.397637795275591177, -0.5400638737290844871, 0.3530559997133364547 ) ) ;
#39042 = B_SPLINE_CURVE_WITH_KNOTS ( 'NONE', 3,
 ( #2786, #59598, #21716, #1953 ),
 .UNSPECIFIED., .F., .F.,
 ( 4, 4 ),
 ( 1.999999999897049408E-07, 0.006970199999999935128 ),
 .UNSPECIFIED. ) ;
#39043 = CARTESIAN_POINT ( 'NONE',  ( -0.2362204724409447953, -0.4091458600556404646, 0.1725721784776902690 ) ) ;
#39044 = CARTESIAN_POINT ( 'NONE',  ( -0.4461942257217840213, -0.5023911411419708095, -0.1820866141732282451 ) ) ;
#39045 = CARTESIAN_POINT ( 'NONE',  ( 0.06561679790026316017, 0.05413385826771626580, -0.4176697321401330321 ) ) ;
#39046 = CARTESIAN_POINT ( 'NONE',  ( 0.3608923884514443348, -0.6692913385826771977, 0.1292274648535927661 ) ) ;
#39047 = FACE_OUTER_BOUND ( 'NONE', #63519, .T. ) ;
#39048 = CARTESIAN_POINT ( 'NONE',  ( 0.9055118110236227702, -0.5511811023622047445, 6.969142054262312111E-17 ) ) ;
#39049 = CARTESIAN_POINT ( 'NONE',  ( 0.2755905511811031494, -0.5511811023622047445, 6.969142054262312111E-17 ) ) ;
#39050 = CARTESIAN_POINT ( 'NONE',  ( -0.1968503937007867743, 0.2952755905511811885, 0.000000000000000000 ) ) ;
#39051 = CARTESIAN_POINT ( 'NONE',  ( -1.515748031496062076, 0.1660481256975883668, -0.3530559997133364547 ) ) ;
#39052 = CARTESIAN_POINT ( 'NONE',  ( -0.8398950131233585692, 0.1283753931104748280, 0.1820866141732283561 ) ) ;
#39053 = DIRECTION ( 'NONE',  ( 1.000000000000000000, -0.000000000000000000, -0.000000000000000000 ) ) ;
#39054 = AXIS2_PLACEMENT_3D ( 'NONE', #65547, #305, #59204 ) ;
#39055 = CARTESIAN_POINT ( 'NONE',  ( -0.8464566929133852113, 0.1660481256975885056, 0.3530559997133364547 ) ) ;
#39056 = CARTESIAN_POINT ( 'NONE',  ( 0.1998031496062992463, 0.3460692066303959202, -1.166010498687663821 ) ) ;
#39057 = EDGE_CURVE ( 'NONE', #80363, #60118, #41194, .T. ) ;
#39058 = CARTESIAN_POINT ( 'NONE',  ( 4.797336870675656522E-17, -0.3917322834645670104, -2.525590551181102317 ) ) ;
#39059 = CARTESIAN_POINT ( 'NONE',  ( 5.463695987328526437E-16, -0.1870078740157479769, 0.3641732283464567677 ) ) ;
#39060 = CARTESIAN_POINT ( 'NONE',  ( -0.8595800524934373854, -0.05778040916215522460, 0.4822834645669289988 ) ) ;
#39061 = CARTESIAN_POINT ( 'NONE',  ( -1.246719160104985846, -0.4281496062992127816, -0.4176697321401328100 ) ) ;
#39062 = CARTESIAN_POINT ( 'NONE',  ( -1.089238845144356427, -0.3690944881889765550, -0.3153832671262227771 ) ) ;
#39063 = CARTESIAN_POINT ( 'NONE',  ( -3.910145899155770710, 1.414046480882519941, -0.4591600588675787686 ) ) ;
#39064 = CARTESIAN_POINT ( 'NONE',  ( -1.017060367454067249, -0.08942795157527998196, 0.3641732283464567121 ) ) ;
#39065 = CARTESIAN_POINT ( 'NONE',  ( -1.535433070866141225, 0.1771653543307087630, 0.000000000000000000 ) ) ;
#39066 = CARTESIAN_POINT ( 'NONE',  ( 1.194225721784777594, -0.4281496062992127816, -0.4176697321401328100 ) ) ;
#39067 = CARTESIAN_POINT ( 'NONE',  ( 0.2362204724409451007, -0.4091458600556402980, -0.7217847769028871152 ) ) ;
#39068 = ADVANCED_FACE ( 'NONE', ( #35588 ), #16244, .F. ) ;
#39069 = CARTESIAN_POINT ( 'NONE',  ( 0.2867679344610366554, 0.2867679344610366554, -2.496738475886826070 ) ) ;
#39070 = ORIENTED_EDGE ( 'NONE', *, *, #15443, .F. ) ;
#39071 = CIRCLE ( 'NONE', #21664, 2.204724409448819422 ) ;
#39072 = CYLINDRICAL_SURFACE ( 'NONE', #56591, 0.5118110236220471121 ) ;
#39073 = CARTESIAN_POINT ( 'NONE',  ( -1.732283464566928277, -0.1870078740157479769, 0.4822834645669291653 ) ) ;
#39074 = CARTESIAN_POINT ( 'NONE',  ( -1.476377952755905110, -0.5400638737290845981, -0.3530559997133363437 ) ) ;
#39075 = CARTESIAN_POINT ( 'NONE',  ( 1.154855643044620184, 0.2306618581243847221, -0.2411417322834647770 ) ) ;
#39076 = CARTESIAN_POINT ( 'NONE',  ( -0.1049643490035307020, 0.3917322834645669549, -1.980971128608924214 ) ) ;
#39077 = DIRECTION ( 'NONE',  ( 1.000000000000000000, -1.445602896647338917E-16, 0.000000000000000000 ) ) ;
#39078 = CARTESIAN_POINT ( 'NONE',  ( 0.4133858267716541968, 0.1660481256975885056, 0.3530559997133364547 ) ) ;
#39079 = CARTESIAN_POINT ( 'NONE',  ( -0.1706036745406816491, 0.05413385826771626580, -0.4176697321401330321 ) ) ;
#39080 = CARTESIAN_POINT ( 'NONE',  ( -0.3273801728231969244, -2.609869883881465018E-15, -0.3464511005275220379 ) ) ;
#39081 = CARTESIAN_POINT ( 'NONE',  ( -0.6399301791983041943, -2.567464376874931580E-15, -0.4445507791589072832 ) ) ;
#39082 = CARTESIAN_POINT ( 'NONE',  ( 0.9317585301837276734, -0.3690944881889763329, 0.3153832671262228327 ) ) ;
#39083 = CARTESIAN_POINT ( 'NONE',  ( 0.3460692066303959757, -0.1998031496062991907, -1.364829396325459188 ) ) ;
#39084 = VERTEX_POINT ( 'NONE', #55343 ) ;
#39085 = CARTESIAN_POINT ( 'NONE',  ( -0.1958661417322836995, 0.3392501089628017219, 0.1476184794937513700 ) ) ;
#39086 = ORIENTED_EDGE ( 'NONE', *, *, #27581, .T. ) ;
#39087 = CARTESIAN_POINT ( 'NONE',  ( 0.09186351706036799403, -0.4281496062992127816, -0.4176697321401328100 ) ) ;
#39088 = CARTESIAN_POINT ( 'NONE',  ( -1.653543307086613234, -0.1870078740157479769, 0.4822834645669291653 ) ) ;
#39089 = CARTESIAN_POINT ( 'NONE',  ( 0.7677165354330716118, 0.1660481256975883668, -0.3530559997133364547 ) ) ;
#39090 = CARTESIAN_POINT ( 'NONE',  ( 1.010498687664042716, -0.4281496062992124485, 0.4176697321401328655 ) ) ;
#39091 = CARTESIAN_POINT ( 'NONE',  ( 1.220472440944882386, -0.6692913385826771977, 8.415575281601705876E-17 ) ) ;
#39092 = CARTESIAN_POINT ( 'NONE',  ( -0.6692913385826764205, 0.2952755905511811885, 0.000000000000000000 ) ) ;
#39093 = CARTESIAN_POINT ( 'NONE',  ( -0.02624671916010428221, -0.6046776061558807314, 0.2411417322834647770 ) ) ;
#39094 = CARTESIAN_POINT ( 'NONE',  ( 1.404199475065617264, -0.4281496062992124485, 0.4176697321401328655 ) ) ;
#39095 = CARTESIAN_POINT ( 'NONE',  ( 1.430446194225722500, 0.05413385826771666132, 0.4176697321401328100 ) ) ;
#39096 = CARTESIAN_POINT ( 'NONE',  ( 1.174540682414699111, -0.3162353388693405765, 0.4822834645669290543 ) ) ;
#39097 = CARTESIAN_POINT ( 'NONE',  ( -0.3215223097112853146, -0.3162353388693405765, 0.4822834645669290543 ) ) ;
#39098 = CARTESIAN_POINT ( 'NONE',  ( -0.3392501089628017219, -0.1958661417322836718, -0.3595800524934382736 ) ) ;
#39099 = CARTESIAN_POINT ( 'NONE',  ( 0.2493438320209980519, -0.004921259842519576551, 0.3153832671262227771 ) ) ;
#39100 = ORIENTED_EDGE ( 'NONE', *, *, #76855, .T. ) ;
#39101 = CARTESIAN_POINT ( 'NONE',  ( 0.3420746716998660508, -0.1974969037888703871, -0.5774278215223097588 ) ) ;
#39102 = VERTEX_POINT ( 'NONE', #41891 ) ;
#39103 = CARTESIAN_POINT ( 'NONE',  ( -0.6496062992125976043, -0.4536011799217367080, 0.2665933059059888421 ) ) ;
#39104 = DIRECTION ( 'NONE',  ( -1.692413147294446216E-16, 0.000000000000000000, -1.000000000000000000 ) ) ;
#39105 = CARTESIAN_POINT ( 'NONE',  ( 0.06561679790026316017, 0.05413385826771626580, -0.4176697321401330321 ) ) ;
#39106 = CARTESIAN_POINT ( 'NONE',  ( -0.1312335958005241554, 0.2306618581243848609, 0.2411417322834645549 ) ) ;
#39107 = CARTESIAN_POINT ( 'NONE',  ( -1.036745406824146176, 0.05413385826771626580, -0.4176697321401330321 ) ) ;
#39108 = CARTESIAN_POINT ( 'NONE',  ( -0.3392501089628019995, 0.1958661417322831999, -1.597788344653229720 ) ) ;
#39109 = CARTESIAN_POINT ( 'NONE',  ( -1.423884514435694859, -0.05778040916215560624, -0.4822834645669293319 ) ) ;
#39110 = DIRECTION ( 'NONE',  ( -0.000000000000000000, -0.000000000000000000, -1.000000000000000000 ) ) ;
#39111 = CARTESIAN_POINT ( 'NONE',  ( 0.8005249343832027131, -0.004921259842519576551, 0.3153832671262227771 ) ) ;
#39112 = CARTESIAN_POINT ( 'NONE',  ( 0.3412073490813655186, -0.6046776061558809534, -0.2411417322834644161 ) ) ;
#39113 = CARTESIAN_POINT ( 'NONE',  ( 0.9120734908136490793, 0.2952755905511810774, -0.1292274648535930714 ) ) ;
#39114 = AXIS2_PLACEMENT_3D ( 'NONE', #41569, #49113, #35260 ) ;
#39115 = CARTESIAN_POINT ( 'NONE',  ( -0.1998031496062991907, -0.3460692066303959757, -1.167979002624671914 ) ) ;
#39116 = CARTESIAN_POINT ( 'NONE',  ( -2.554860351194724544, 1.554815631980118740, 0.4741686481756392513 ) ) ;
#39117 = CARTESIAN_POINT ( 'NONE',  ( 4.893765752498283308E-17, -0.3996062992125985480, -0.6279527559055118058 ) ) ;
#39118 = CARTESIAN_POINT ( 'NONE',  ( -0.2925321140481932369, 0.2925321140481931259, -0.2539370078740156855 ) ) ;
#39119 = CARTESIAN_POINT ( 'NONE',  ( 0.01312335958005323398, 0.05413385826771666132, 0.4176697321401328100 ) ) ;
#39120 = CARTESIAN_POINT ( 'NONE',  ( -0.2925321140481930704, -0.2925321140481933480, -2.578740157480315265 ) ) ;
#39121 = CARTESIAN_POINT ( 'NONE',  ( 0.3392501089628018884, -0.1958661417322834220, -1.921916010498687877 ) ) ;
#39122 = CARTESIAN_POINT ( 'NONE',  ( -1.141732283464566011, 0.1771653543307087630, 0.000000000000000000 ) ) ;
#39123 = CARTESIAN_POINT ( 'NONE',  ( 1.154855643044620184, 0.2306618581243847221, -0.2411417322834647770 ) ) ;
#39124 = CARTESIAN_POINT ( 'NONE',  ( 1.207349081364829990, 0.2306618581243848609, 0.2411417322834645549 ) ) ;
#39125 = CARTESIAN_POINT ( 'NONE',  ( 0.2230971128608932319, -0.3690944881889763329, 0.3153832671262228327 ) ) ;
#39126 = CARTESIAN_POINT ( 'NONE',  ( 0.4658792650918640033, -0.3162353388693405765, 0.4822834645669290543 ) ) ;
#39127 = CARTESIAN_POINT ( 'NONE',  ( 0.1265901696524990294, -0.4724409448818896462, -1.579396325459317296 ) ) ;
#39128 = CARTESIAN_POINT ( 'NONE',  ( 0.2952755905511819101, 0.07958543189024071263, -0.2665933059059888421 ) ) ;
#39129 = CARTESIAN_POINT ( 'NONE',  ( -0.1312335958005241554, 0.2306618581243848609, 0.2411417322834645549 ) ) ;
#39130 = CARTESIAN_POINT ( 'NONE',  ( 0.1058382717557499880, 0.3949938075777409408, -1.487532808398950523 ) ) ;
#39131 = CARTESIAN_POINT ( 'NONE',  ( -1.417322834645668772, -0.1870078740157479769, 0.4822834645669291653 ) ) ;
#39132 = CARTESIAN_POINT ( 'NONE',  ( 0.3871391076115492380, -0.08942795157528024563, -0.3641732283464568787 ) ) ;
#39133 = AXIS2_PLACEMENT_3D ( 'NONE', #74150, #79648, #55175 ) ;
#39134 = CARTESIAN_POINT ( 'NONE',  ( -0.4724409448818898682, 5.785732909357575061E-17, -2.755905511811024056 ) ) ;
#39135 = CARTESIAN_POINT ( 'NONE',  ( -0.6824146981627291497, -0.6046776061558809534, -0.2411417322834644161 ) ) ;
#39136 = CARTESIAN_POINT ( 'NONE',  ( -0.4199475065616791736, -0.5023911411419708095, 0.1820866141732285504 ) ) ;
#39137 = CARTESIAN_POINT ( 'NONE',  ( -0.9317585301837263412, 0.05413385826771666132, 0.4176697321401328100 ) ) ;
#39138 = CARTESIAN_POINT ( 'NONE',  ( -0.1706036745406816491, 0.05413385826771626580, -0.4176697321401330321 ) ) ;
#39139 = CARTESIAN_POINT ( 'NONE',  ( 0.2493438320209980519, -0.3690944881889765550, -0.3153832671262227771 ) ) ;
#39140 = CARTESIAN_POINT ( 'NONE',  ( -0.3460692066303960313, 0.1998031496062989965, -2.307742782152231165 ) ) ;
#39141 = CARTESIAN_POINT ( 'NONE',  ( 0.006561679790026889343, -0.3162353388693409650, -0.4822834645669289433 ) ) ;
#39142 = CARTESIAN_POINT ( 'NONE',  ( 0.3917322834645668994, 0.1049643490035304522, -2.251949188155168979 ) ) ;
#39143 = CARTESIAN_POINT ( 'NONE',  ( 0.6824146981627303710, -0.5023911411419708095, 0.1820866141732285504 ) ) ;
#39144 = CARTESIAN_POINT ( 'NONE',  ( 1.502624671916010790, -0.3162353388693409650, -0.4822834645669289433 ) ) ;
#39145 = CARTESIAN_POINT ( 'NONE',  ( -0.7611548556430438595, 0.1283753931104748280, 0.1820866141732283561 ) ) ;
#39146 = CARTESIAN_POINT ( 'NONE',  ( -1.345144356955379816, -0.08942795157528024563, -0.3641732283464568787 ) ) ;
#39147 = CARTESIAN_POINT ( 'NONE',  ( -0.7152230971128602510, -0.3162353388693405765, 0.4822834645669290543 ) ) ;
#39148 = CARTESIAN_POINT ( 'NONE',  ( -0.05905511811023545637, -0.5400638737290845981, -0.3530559997133363437 ) ) ;
#39149 = CARTESIAN_POINT ( 'NONE',  ( 0.5511811023622055217, -0.1870078740157479769, 0.3641732283464567677 ) ) ;
#39150 = CARTESIAN_POINT ( 'NONE',  ( -0.2917579853797115930, 0.04689358074580359664, 5.530719428720964892 ) ) ;
#39151 = CARTESIAN_POINT ( 'NONE',  ( 1.010498687664042716, -0.004921259842519870586, -0.3153832671262229437 ) ) ;
#39152 = CARTESIAN_POINT ( 'NONE',  ( 0.2493438320209980519, 0.05413385826771666132, 0.4176697321401328100 ) ) ;
#39153 = CARTESIAN_POINT ( 'NONE',  ( 0.1070741851644053388, 0.3996062992125986035, 0.08727034120734905587 ) ) ;
#39154 = CARTESIAN_POINT ( 'NONE',  ( -0.2099737532808391705, -0.6046776061558809534, -0.2411417322834644161 ) ) ;
#39155 = CARTESIAN_POINT ( 'NONE',  ( -0.3917322834645671215, 0.1049643490035301469, -1.377296587926508664 ) ) ;
#39156 = CARTESIAN_POINT ( 'NONE',  ( 1.509186351706037543, -0.3690944881889765550, -0.3153832671262227771 ) ) ;
#39157 = CARTESIAN_POINT ( 'NONE',  ( 0.4265091863517067594, 0.2952755905511811885, 0.1292274648535926551 ) ) ;
#39158 = CARTESIAN_POINT ( 'NONE',  ( 0.03937007874015833325, -0.6692913385826771977, 8.415575281601705876E-17 ) ) ;
#39159 = CARTESIAN_POINT ( 'NONE',  ( 0.6167979002624679463, 0.009842519685039147898, -0.3409548833797004797 ) ) ;
#39160 = CARTESIAN_POINT ( 'NONE',  ( 0.1049868766404206816, 0.1283753931104748280, 0.1820866141732283561 ) ) ;
#39161 = CARTESIAN_POINT ( 'NONE',  ( 0.6299212598425204535, -0.1870078740157480879, -0.4822834645669291653 ) ) ;
#39162 = CARTESIAN_POINT ( 'NONE',  ( -0.4265091863517051496, 0.1771653543307087075, -0.09757992244046823083 ) ) ;
#39163 = CARTESIAN_POINT ( 'NONE',  ( -0.7086614173228339419, -0.1870078740157479769, 0.4822834645669291653 ) ) ;
#39164 = CARTESIAN_POINT ( 'NONE',  ( -0.6299212598425228959, 1.724409448818897905, 0.9285414500055694242 ) ) ;
#39165 = CARTESIAN_POINT ( 'NONE',  ( -0.3083989501312330295, -0.05778040916215522460, 0.4822834645669289988 ) ) ;
#39166 = VERTEX_POINT ( 'NONE', #73489 ) ;
#39167 = CARTESIAN_POINT ( 'NONE',  ( -1.115485564304461219, 0.05413385826771626580, -0.4176697321401330321 ) ) ;
#39168 = CARTESIAN_POINT ( 'NONE',  ( -0.6561679790026240244, -0.5023911411419708095, 0.1820866141732285504 ) ) ;
#39169 = VECTOR ( 'NONE', #6829, 39.37007874015748143 ) ;
#39170 = CARTESIAN_POINT ( 'NONE',  ( 0.1312335958005255154, -0.6046776061558807314, 0.2411417322834647770 ) ) ;
#39171 = CARTESIAN_POINT ( 'NONE',  ( -1.076115485564303809, 0.2306618581243848609, 0.2411417322834645549 ) ) ;
#39172 = CARTESIAN_POINT ( 'NONE',  ( -0.9120734908136475250, -0.6692913385826773087, -0.1292274648535924053 ) ) ;
#39173 = FACE_OUTER_BOUND ( 'NONE', #734, .T. ) ;
#39175 = CARTESIAN_POINT ( 'NONE',  ( 1.423884514435696191, -0.05778040916215522460, 0.4822834645669289988 ) ) ;
#39174 = DIRECTION ( 'NONE',  ( -0.000000000000000000, 1.000000000000000000, -0.000000000000000000 ) ) ;
#39176 = CARTESIAN_POINT ( 'NONE',  ( 1.161417322834646493, -0.5400638737290844871, 0.3530559997133364547 ) ) ;
#39177 = CARTESIAN_POINT ( 'NONE',  ( 0.3917322834645670104, 2.398668435337828261E-17, -2.472440944881889813 ) ) ;
#39178 = CARTESIAN_POINT ( 'NONE',  ( 2.795275590551181466, 2.244094488188977277, 0.000000000000000000 ) ) ;
#39179 = CARTESIAN_POINT ( 'NONE',  ( -1.489501312335957062, -0.3162353388693409650, -0.4822834645669289433 ) ) ;
#39180 = CARTESIAN_POINT ( 'NONE',  ( -0.3458507752293909498, 0.3458507752293907833, -0.9645669291338579976 ) ) ;
#39181 = CARTESIAN_POINT ( 'NONE',  ( -0.3460692066303960868, 0.1998031496062990242, -0.1837270341207349333 ) ) ;
#39182 = ORIENTED_EDGE ( 'NONE', *, *, #33290, .F. ) ;
#39183 = CARTESIAN_POINT ( 'NONE',  ( -0.02624671916010428221, 0.1283753931104746893, -0.1820866141732285504 ) ) ;
#39184 = CARTESIAN_POINT ( 'NONE',  ( -0.1049643490035302024, -0.3917322834645671215, -1.954068241469816503 ) ) ;
#39185 = EDGE_LOOP ( 'NONE', ( #27815, #10877, #40575 ) ) ;
#39186 = CARTESIAN_POINT ( 'NONE',  ( 0.3018372703412079971, -0.4281496062992124485, 0.4176697321401328655 ) ) ;
#39187 = CARTESIAN_POINT ( 'NONE',  ( 0.3412073490813655186, 0.2306618581243848609, 0.2411417322834645549 ) ) ;
#39188 = CARTESIAN_POINT ( 'NONE',  ( -1.614173228346456712, 2.401574803149606474, -0.1372047244094478091 ) ) ;
#39189 = FACE_OUTER_BOUND ( 'NONE', #18994, .T. ) ;
#39190 = CARTESIAN_POINT ( 'NONE',  ( -0.9580052493438311334, -0.004921259842519870586, -0.3153832671262229437 ) ) ;
#39191 =( NAMED_UNIT ( * ) SI_UNIT ( $, .STERADIAN. ) SOLID_ANGLE_UNIT ( ) );
#39192 = CARTESIAN_POINT ( 'NONE',  ( 0.6889763779527566800, -0.5400638737290844871, 0.3530559997133364547 ) ) ;
#39193 = EDGE_CURVE ( 'NONE', #21404, #14171, #42031, .T. ) ;
#39194 = CARTESIAN_POINT ( 'NONE',  ( 0.9842519685039375910, 0.1771653543307087630, 0.000000000000000000 ) ) ;
#39195 = CARTESIAN_POINT ( 'NONE',  ( -0.2755905511811015396, -0.6692913385826771977, 8.415575281601705876E-17 ) ) ;
#39196 = CARTESIAN_POINT ( 'NONE',  ( 0.3392501089628018329, 0.1958661417322835052, -1.156148663220785799 ) ) ;
#39197 = CARTESIAN_POINT ( 'NONE',  ( -0.8661417322834640276, -0.1870078740157479769, 0.4822834645669291653 ) ) ;
#39198 = CARTESIAN_POINT ( 'NONE',  ( 0.5314960629921350321, 2.755905511811024056, -2.583694225513478937 ) ) ;
#39199 = CARTESIAN_POINT ( 'NONE',  ( -0.8464566929133852113, -0.5400638737290845981, -0.3530559997133363437 ) ) ;
#39200 = CARTESIAN_POINT ( 'NONE',  ( 1.332020997375329197, -0.3162353388693405765, 0.4822834645669290543 ) ) ;
#39201 = CARTESIAN_POINT ( 'NONE',  ( 1.607611548556431069, -0.5511811023622048555, -0.09757992244046775898 ) ) ;
#39202 = EDGE_LOOP ( 'NONE', ( #53378, #45526, #38095, #28854 ) ) ;
#39203 = CARTESIAN_POINT ( 'NONE',  ( 0.1049643490035303967, 0.3917322834645670659, -2.352381520506248602 ) ) ;
#39204 = CARTESIAN_POINT ( 'NONE',  ( -0.08530183727034056085, -0.3162353388693405765, 0.4822834645669290543 ) ) ;
#39205 = EDGE_LOOP ( 'NONE', ( #52352, #26863, #46541, #32491 ) ) ;
#39206 = CARTESIAN_POINT ( 'NONE',  ( -0.7217847769028863381, 0.05413385826771626580, -0.4176697321401330321 ) ) ;
#39207 = CARTESIAN_POINT ( 'NONE',  ( 1.430446194225722500, 0.05413385826771666132, 0.4176697321401328100 ) ) ;
#39208 = CARTESIAN_POINT ( 'NONE',  ( 1.141732283464567566, 0.2952755905511811885, 0.000000000000000000 ) ) ;
#39209 = CARTESIAN_POINT ( 'NONE',  ( 0.3346456692913390985, 0.1660481256975885056, 0.3530559997133364547 ) ) ;
#39210 = CARTESIAN_POINT ( 'NONE',  ( 0.2230971128608932319, -0.4281496062992124485, 0.4176697321401328655 ) ) ;
#39211 = CARTESIAN_POINT ( 'NONE',  ( -0.2867679344610365999, 0.2867679344610364889, -1.679133858267716661 ) ) ;
#39212 = CARTESIAN_POINT ( 'NONE',  ( -1.338582677165353729, -0.1870078740157480879, -0.4822834645669291653 ) ) ;
#39213 = CARTESIAN_POINT ( 'NONE',  ( -0.3937007874015740483, -0.1870078740157479769, 0.4822834645669291653 ) ) ;
#39214 = CARTESIAN_POINT ( 'NONE',  ( -0.2493438320209966919, -0.3690944881889763329, 0.3153832671262228327 ) ) ;
#39215 = CARTESIAN_POINT ( 'NONE',  ( 1.607611548556431069, -0.6692913385826773087, -0.1292274648535924053 ) ) ;
#39216 = CARTESIAN_POINT ( 'NONE',  ( 1.345144356955381593, -0.05778040916215522460, 0.4822834645669289988 ) ) ;
#39217 = CARTESIAN_POINT ( 'NONE',  ( -0.4527559055118102749, 0.1660481256975885056, 0.3530559997133364547 ) ) ;
#39218 = DIRECTION ( 'NONE',  ( -1.000000000000000000, 0.000000000000000000, 0.000000000000000000 ) ) ;
#39219 = CARTESIAN_POINT ( 'NONE',  ( 1.003937007874016185, 0.1660481256975883668, -0.3530559997133364547 ) ) ;
#39220 = CARTESIAN_POINT ( 'NONE',  ( 0.3149606299212736604, 2.559055118110236560, -3.937007874015761022 ) ) ;
#39221 = VERTEX_POINT ( 'NONE', #55754 ) ;
#39222 = EDGE_CURVE ( 'NONE', #32899, #53885, #53822, .T. ) ;
#39223 = ORIENTED_EDGE ( 'NONE', *, *, #21721, .T. ) ;
#39224 = CARTESIAN_POINT ( 'NONE',  ( 0.1509186351706045259, -0.05778040916215560624, -0.4822834645669293319 ) ) ;
#39225 = CARTESIAN_POINT ( 'NONE',  ( -0.2165354330708654795, -0.4536011799217368745, -0.2665933059059886201 ) ) ;
#39227 = CARTESIAN_POINT ( 'NONE',  ( 1.603475055217291612, 0.5037964761735347352, 0.04573490813648269093 ) ) ;
#39226 = CARTESIAN_POINT ( 'NONE',  ( 1.351706036745407680, -0.004921259842519576551, 0.3153832671262227771 ) ) ;
#39228 = CARTESIAN_POINT ( 'NONE',  ( -0.4724409448818895907, -0.1265901696524993070, -0.4376640419947506744 ) ) ;
#39229 = CARTESIAN_POINT ( 'NONE',  ( 1.528871391076116026, 0.1771653543307087630, 0.09757992244046791164 ) ) ;
#39230 = CARTESIAN_POINT ( 'NONE',  ( 1.154855643044620184, 0.2306618581243847221, -0.2411417322834647770 ) ) ;
#39231 = CARTESIAN_POINT ( 'NONE',  ( 4.837279021331061486E-17, -0.3949938075777409963, -0.1555118110236220486 ) ) ;
#39232 = CARTESIAN_POINT ( 'NONE',  ( 0.1049868766404206816, -0.6046776061558809534, -0.2411417322834644161 ) ) ;
#39233 = CARTESIAN_POINT ( 'NONE',  ( -1.522309711286088607, -0.6046776061558807314, 0.2411417322834647770 ) ) ;
#39234 = CARTESIAN_POINT ( 'NONE',  ( -1.725721784776902190, -0.05778040916215522460, 0.4822834645669289988 ) ) ;
#39235 = CARTESIAN_POINT ( 'NONE',  ( -0.2427821522309703550, -0.05778040916215560624, -0.4822834645669293319 ) ) ;
#39236 = CARTESIAN_POINT ( 'NONE',  ( 0.1058382717557499880, 0.3949938075777409408, -0.07020997375328083545 ) ) ;
#39237 = CARTESIAN_POINT ( 'NONE',  ( -1.640419947506561060, -0.004921259842519576551, 0.3153832671262227771 ) ) ;
#39238 = CARTESIAN_POINT ( 'NONE',  ( 0.4986876640419954376, 0.2306618581243848609, 0.2411417322834645549 ) ) ;
#39239 = AXIS2_PLACEMENT_3D ( 'NONE', #66606, #8942, #34617 ) ;
#39240 = CARTESIAN_POINT ( 'NONE',  ( 0.9645669291338591078, -0.4536011799217368745, -0.2665933059059886201 ) ) ;
#39241 = CARTESIAN_POINT ( 'NONE',  ( 0.1565873217565743603, 1.056201437308684321, 0.2712946218330505865 ) ) ;
#39242 = ADVANCED_FACE ( 'NONE', ( #36822 ), #41487, .F. ) ;
#39243 = CARTESIAN_POINT ( 'NONE',  ( 0.7020997375328090762, -0.2845877964562159024, 0.3641732283464567677 ) ) ;
#39244 = CARTESIAN_POINT ( 'NONE',  ( -1.207349081364828436, -0.6046776061558807314, 0.2411417322834647770 ) ) ;
#39245 = CARTESIAN_POINT ( 'NONE',  ( -0.3996062992125986590, 0.1070741851644051723, -0.7395013123359580609 ) ) ;
#39246 = CARTESIAN_POINT ( 'NONE',  ( 1.102362204724410155, -0.1870078740157480879, -0.4822834645669291653 ) ) ;
#39247 = CARTESIAN_POINT ( 'NONE',  ( 0.2867679344610365999, 0.2867679344610365999, -0.6023622047244093780 ) ) ;
#39249 = PLANE ( 'NONE',  #76156 ) ;
#39248 = CARTESIAN_POINT ( 'NONE',  ( 0.7545931758530189937, 0.2952755905511810774, -0.1292274648535930714 ) ) ;
#39250 = CARTESIAN_POINT ( 'NONE',  ( -0.3805774278215216522, 0.009842519685039467087, 0.3409548833797002021 ) ) ;
#39251 = CARTESIAN_POINT ( 'NONE',  ( 0.5511811023622054106, -0.1870078740157480601, -0.3641732283464567677 ) ) ;
#39252 = CARTESIAN_POINT ( 'NONE',  ( 0.7349081364829403995, 0.2306618581243848609, 0.2411417322834645549 ) ) ;
#39253 = CARTESIAN_POINT ( 'NONE',  ( -0.03443470937339728616, 0.2755905511811023723, -1.537015892239756099 ) ) ;
#39254 = CARTESIAN_POINT ( 'NONE',  ( -1.128608923884513837, -0.5023911411419708095, 0.1820866141732285504 ) ) ;
#39255 = CARTESIAN_POINT ( 'NONE',  ( -0.9383202099737524282, -0.05778040916215522460, 0.4822834645669289988 ) ) ;
#39256 = CARTESIAN_POINT ( 'NONE',  ( 0.9580052493438327987, -0.4281496062992127816, -0.4176697321401328100 ) ) ;
#39257 = CARTESIAN_POINT ( 'NONE',  ( -0.9383202099737524282, -0.05778040916215522460, 0.4822834645669289988 ) ) ;
#39258 = CARTESIAN_POINT ( 'NONE',  ( 0.9908136482939640111, -0.6692913385826771977, 0.1292274648535927661 ) ) ;
#39259 = CARTESIAN_POINT ( 'NONE',  ( -1.443569553805773564, 0.1283753931104746893, -0.1820866141732285504 ) ) ;
#39260 = CARTESIAN_POINT ( 'NONE',  ( 1.028050040965491130, 1.383304877436015490, -0.4497434709457576729 ) ) ;
#39261 = CARTESIAN_POINT ( 'NONE',  ( 0.9776902887139113929, 0.2952755905511811885, 0.1292274648535926551 ) ) ;
#39262 = CARTESIAN_POINT ( 'NONE',  ( 0.2362204724409449064, 0.4091458600556404646, -2.268372703412073310 ) ) ;
#39263 = CARTESIAN_POINT ( 'NONE',  ( 0.2506648432407165838, 1.134319890641129813, 3.929041500980708701 ) ) ;
#39264 = CARTESIAN_POINT ( 'NONE',  ( 1.194225721784777594, 0.05413385826771666132, 0.4176697321401328100 ) ) ;
#39265 = CARTESIAN_POINT ( 'NONE',  ( -1.627296587926508442, -0.5023911411419708095, -0.1820866141732282451 ) ) ;
#39266 = CARTESIAN_POINT ( 'NONE',  ( 1.168682819302787168, 2.409604939980833412E-17, -0.3464511005275205946 ) ) ;
#39267 = CARTESIAN_POINT ( 'NONE',  ( -1.272965879265091305, -0.004921259842519870586, -0.3153832671262229437 ) ) ;
#39268 = CARTESIAN_POINT ( 'NONE',  ( -0.5577427821522301654, -0.2845877964562159024, 0.3641732283464567677 ) ) ;
#39269 = CARTESIAN_POINT ( 'NONE',  ( -1.397637795275589623, 0.07958543189024085140, 0.2665933059059887866 ) ) ;
#39270 = CARTESIAN_POINT ( 'NONE',  ( 0.8727034120734912248, -0.2845877964562161244, -0.3641732283464567121 ) ) ;
#39271 = CARTESIAN_POINT ( 'NONE',  ( 0.5839895013123367340, 0.2952755905511811885, 0.1292274648535926551 ) ) ;
#39272 = CARTESIAN_POINT ( 'NONE',  ( 1.200787401574803681, -0.5400638737290845981, -0.3530559997133363437 ) ) ;
#39273 = CARTESIAN_POINT ( 'NONE',  ( -0.05905511811023545637, 0.1660481256975885056, 0.3530559997133364547 ) ) ;
#39274 = CARTESIAN_POINT ( 'NONE',  ( 0.5380577427821529035, -0.004921259842519870586, -0.3153832671262229437 ) ) ;
#39275 = CARTESIAN_POINT ( 'NONE',  ( 1.555118110236221041, -0.5400638737290844871, 0.3530559997133364547 ) ) ;
#39276 = DIRECTION ( 'NONE',  ( 1.000000000000000000, 0.000000000000000000, 3.455050906509825972E-15 ) ) ;
#39277 = CARTESIAN_POINT ( 'NONE',  ( -0.5708661417322828946, 0.1660481256975883668, -0.3530559997133364547 ) ) ;
#39278 = CARTESIAN_POINT ( 'NONE',  ( 0.1998031496062994405, -0.3460692066303958092, -0.5643044619422572516 ) ) ;
#39279 = CARTESIAN_POINT ( 'NONE',  ( -0.2362204724409451284, 0.4091458600556402425, -1.192257217847769057 ) ) ;
#39280 = CARTESIAN_POINT ( 'NONE',  ( 0.1312335958005255154, -0.6046776061558807314, 0.2411417322834647770 ) ) ;
#39281 = CARTESIAN_POINT ( 'NONE',  ( -0.5774278215223089816, -0.6046776061558807314, 0.2411417322834647770 ) ) ;
#39282 = CARTESIAN_POINT ( 'NONE',  ( 0.06561679790026316017, 0.05413385826771626580, -0.4176697321401330321 ) ) ;
#39283 = CARTESIAN_POINT ( 'NONE',  ( -0.2925321140481932924, 0.2925321140481931814, -2.539370078740157410 ) ) ;
#39284 = CARTESIAN_POINT ( 'NONE',  ( -0.1974969037888706647, 0.3420746716998658843, -1.745406824146981339 ) ) ;
#39285 = CARTESIAN_POINT ( 'NONE',  ( 0.3917322834645670104, -0.1049643490035303411, -0.5761154855643042527 ) ) ;
#39286 = CARTESIAN_POINT ( 'NONE',  ( 1.363814626685859954, 0.1354692512615922884, 0.3875633260700433458 ) ) ;
#39287 = CARTESIAN_POINT ( 'NONE',  ( 0.1958661417322836440, -0.3392501089628017219, -1.186351706036745446 ) ) ;
#39288 = ADVANCED_FACE ( 'NONE', ( #38885 ), #44759, .T. ) ;
#39289 = CARTESIAN_POINT ( 'NONE',  ( -0.7874015748031489847, -0.1870078740157479769, 0.3641732283464567677 ) ) ;
#39290 = CARTESIAN_POINT ( 'NONE',  ( -0.3917322834645670104, -7.196005306013484475E-17, -0.9763779527559053317 ) ) ;
#39291 = CARTESIAN_POINT ( 'NONE',  ( -1.253280839895012377, -0.05778040916215522460, 0.4822834645669289988 ) ) ;
#39292 = CONICAL_SURFACE ( 'NONE', #54071, 1.181102362204724310, 0.7853981633974621568 ) ;
#39293 = CARTESIAN_POINT ( 'NONE',  ( 0.3917322834645668994, -0.1049643490035303134, 0.1233788958343325359 ) ) ;
#39294 = CARTESIAN_POINT ( 'NONE',  ( 0.5249343832021005074, -0.6046776061558807314, 0.2411417322834647770 ) ) ;
#39295 = CARTESIAN_POINT ( 'NONE',  ( -0.05905511811023545637, -0.4536011799217368745, -0.2665933059059886201 ) ) ;
#39296 = CARTESIAN_POINT ( 'NONE',  ( 1.476377952755906220, 0.1660481256975883668, -0.3530559997133364547 ) ) ;
#39297 = CARTESIAN_POINT ( 'NONE',  ( 0.2427821522309716595, -0.3162353388693409650, -0.4822834645669289433 ) ) ;
#39298 = CARTESIAN_POINT ( 'NONE',  ( -0.4091458600556405756, 0.2362204724409446288, -0.1030183727034120617 ) ) ;
#39299 = CARTESIAN_POINT ( 'NONE',  ( -0.2925321140481932924, 0.2925321140481931814, -2.381889763779527325 ) ) ;
#39300 = CARTESIAN_POINT ( 'NONE',  ( 0.3392501089628018329, 0.1958661417322835607, -1.387814591372390272 ) ) ;
#39301 = CARTESIAN_POINT ( 'NONE',  ( 1.089238845144357759, 0.05413385826771626580, -0.4176697321401330321 ) ) ;
#39302 = CARTESIAN_POINT ( 'NONE',  ( 0.3280839895013130669, 0.05413385826771666132, 0.4176697321401328100 ) ) ;
#39303 = CARTESIAN_POINT ( 'NONE',  ( 0.1443569553805781891, -0.4281496062992124485, 0.4176697321401328655 ) ) ;
#39304 = CARTESIAN_POINT ( 'NONE',  ( 1.456692913385827515, -0.6692913385826771977, 8.415575281601705876E-17 ) ) ;
#39305 = CARTESIAN_POINT ( 'NONE',  ( -0.3917322834645669549, -0.1049643490035306603, -0.6030183727034120755 ) ) ;
#39306 = CARTESIAN_POINT ( 'NONE',  ( -0.06561679790026180015, -0.4281496062992127816, -0.4176697321401328100 ) ) ;
#39307 = CARTESIAN_POINT ( 'NONE',  ( 1.272965879265092637, -0.4281496062992127816, -0.4176697321401328100 ) ) ;
#39308 = CARTESIAN_POINT ( 'NONE',  ( 0.5118110236220480003, -0.6692913385826771977, 8.415575281601705876E-17 ) ) ;
#39309 = CARTESIAN_POINT ( 'NONE',  ( 0.9973753280839902091, -0.5023911411419708095, 0.1820866141732285504 ) ) ;
#39310 = CARTESIAN_POINT ( 'NONE',  ( -0.8923884514435688198, 0.2306618581243847221, -0.2411417322834647770 ) ) ;
#39311 = CARTESIAN_POINT ( 'NONE',  ( -1.364829396325458521, 0.2306618581243847221, -0.2411417322834647770 ) ) ;
#39312 = CARTESIAN_POINT ( 'NONE',  ( 0.9186351706036751663, -0.6046776061558807314, 0.2411417322834647770 ) ) ;
#39313 = CARTESIAN_POINT ( 'NONE',  ( 0.1778467755342286460, -0.3496712940250776835, -1.929133858267715329 ) ) ;
#39314 = CARTESIAN_POINT ( 'NONE',  ( 0.3917322834645670104, -0.1049643490035303411, -1.993438320209974135 ) ) ;
#39315 =( BOUNDED_CURVE ( )  B_SPLINE_CURVE ( 2, ( #8808, #47092, #72782, #15132, #40788, #34484, #28161, #60562, #2913, #23495, #49161, #25135, #11295 ),
 .UNSPECIFIED., .F., .F. ) 
 B_SPLINE_CURVE_WITH_KNOTS ( ( 3, 2, 2, 2, 2, 2, 3 ),
 ( 0.3217605387524145044, 0.3219696969696970168, 0.3257575757575758013, 0.3295454545454545858, 0.3333333333333333703, 0.3371212121212121549, 0.3373303703384946672 ),
 .UNSPECIFIED. ) 
 CURVE ( )  GEOMETRIC_REPRESENTATION_ITEM ( )  RATIONAL_B_SPLINE_CURVE ( ( 0.9964447847208419695, 0.9981185001348091834, 1.000000000000000000, 0.9659258262890683122, 1.000000000000000000, 0.9659258262890683122, 1.000000000000000000, 0.9659258262890683122, 1.000000000000000000, 0.9659258262890683122, 1.000000000000000000, 0.9981185001348091834, 0.9964447847208420805 ) ) 
 REPRESENTATION_ITEM ( '' )  );
#39316 = CARTESIAN_POINT ( 'NONE',  ( 1.574803149606299746, -0.1870078740157480879, -0.4822834645669291653 ) ) ;
#39317 = ORIENTED_EDGE ( 'NONE', *, *, #5285, .F. ) ;
#39318 = CARTESIAN_POINT ( 'NONE',  ( -0.3460692066303960868, 0.1998031496062990242, -0.02624671916010500733 ) ) ;
#39319 = ORIENTED_EDGE ( 'NONE', *, *, #10205, .F. ) ;
#39320 = CARTESIAN_POINT ( 'NONE',  ( 1.555118110236221041, 0.1660481256975883668, -0.3530559997133364547 ) ) ;
#39321 = CARTESIAN_POINT ( 'NONE',  ( 0.9120734908136489683, -0.5511811023622046335, 0.09757992244046803654 ) ) ;
#39322 = CLOSED_SHELL ( 'NONE', ( #52359, #70250, #36189, #55647, #62473, #59591, #34236, #69083, #6324, #37918, #22780, #9537, #77338, #25998, #77464, #2342, #22947, #26530, #18831, #64507, #29619, #39555, #4835, #22460, #11345, #7398, #72318, #14954, #70511, #69203, #20079, #43389 ) ) ;
#39323 = CARTESIAN_POINT ( 'NONE',  ( -0.1458944486102277671, 0.02791078216816064370, 0.4328096321851915285 ) ) ;
#39324 = CARTESIAN_POINT ( 'NONE',  ( 2.795275590551181466, 2.204724409448820310, 0.000000000000000000 ) ) ;
#39325 = CARTESIAN_POINT ( 'NONE',  ( -0.1958661417322834220, -0.3392501089628018884, -0.7801837270341208663 ) ) ;
#39326 = CARTESIAN_POINT ( 'NONE',  ( -1.082677165354329896, -0.4536011799217368745, -0.2665933059059886201 ) ) ;
#39327 = CARTESIAN_POINT ( 'NONE',  ( -1.725721784776902190, -0.08942795157527998196, 0.3641732283464567121 ) ) ;
#39328 = CARTESIAN_POINT ( 'NONE',  ( -0.3900885325446892815, -0.05060072268104446463, -1.929133858267718216 ) ) ;
#39329 = CARTESIAN_POINT ( 'NONE',  ( -0.2690288713910754526, 0.2952755905511810774, -0.1292274648535930714 ) ) ;
#39330 = CARTESIAN_POINT ( 'NONE',  ( -1.568241469816272105, -0.3162353388693409650, -0.4822834645669289433 ) ) ;
#39331 = ORIENTED_EDGE ( 'NONE', *, *, #40826, .T. ) ;
#39332 = CARTESIAN_POINT ( 'NONE',  ( -1.391076115485563758, 0.2306618581243848609, 0.2411417322834645549 ) ) ;
#39333 = DIRECTION ( 'NONE',  ( 0.000000000000000000, 1.000000000000000000, -8.673617379884024625E-16 ) ) ;
#39334 = CARTESIAN_POINT ( 'NONE',  ( -0.3273801728231969244, -2.609869883881465018E-15, -0.3464511005275220379 ) ) ;
#39335 = CARTESIAN_POINT ( 'NONE',  ( -0.3046215029598641766, -4.378520898609941727E-15, 0.4281989832122466977 ) ) ;
#39336 = CARTESIAN_POINT ( 'NONE',  ( -0.7086614173228339419, -0.1870078740157479769, 0.3641732283464567677 ) ) ;
#39337 = CARTESIAN_POINT ( 'NONE',  ( -1.627296587926508442, 0.2306618581243848609, 0.2411417322834645549 ) ) ;
#39338 = CARTESIAN_POINT ( 'NONE',  ( 0.5118110236220480003, -0.6692913385826771977, 8.415575281601705876E-17 ) ) ;
#39339 = EDGE_LOOP ( 'NONE', ( #55027, #22744, #80448, #4340 ) ) ;
#39341 = CARTESIAN_POINT ( 'NONE',  ( 0.7998211177050879028, 0.000000000000000000, 0.3464511005275205946 ) ) ;
#39340 = CARTESIAN_POINT ( 'NONE',  ( -1.881759047730065859, 2.742776634745604625, -0.5314960629921260393 ) ) ;
#39342 = EDGE_CURVE ( 'NONE', #46748, #30815, #69424, .T. ) ;
#39343 = CARTESIAN_POINT ( 'NONE',  ( 1.404199475065617708, 0.05413385826771626580, -0.4176697321401330321 ) ) ;
#39344 = CARTESIAN_POINT ( 'NONE',  ( 1.614173228346457378, 0.1771653543307087630, 0.000000000000000000 ) ) ;
#39345 = CARTESIAN_POINT ( 'NONE',  ( -0.2867679344610364334, -0.2867679344610368219, -0.7690095556092370055 ) ) ;
#39346 = AXIS2_PLACEMENT_3D ( 'NONE', #19494, #12777, #26220 ) ;
#39347 = CARTESIAN_POINT ( 'NONE',  ( -0.4527559055118102749, 0.07958543189024085140, 0.2665933059059887866 ) ) ;
#39348 = CARTESIAN_POINT ( 'NONE',  ( -1.456692913385826182, 0.1771653543307087630, 0.000000000000000000 ) ) ;
#39349 = CARTESIAN_POINT ( 'NONE',  ( -0.4091458600556405756, 0.2362204724409446288, -0.8136482939632546652 ) ) ;
#39351 = ADVANCED_FACE ( 'NONE', ( #77195 ), #78882, .F. ) ;
#39350 = CARTESIAN_POINT ( 'NONE',  ( 0.3018372703412079971, -0.4281496062992124485, 0.4176697321401328655 ) ) ;
#39352 = CARTESIAN_POINT ( 'NONE',  ( -0.7939632545931750718, -0.08942795157528024563, -0.3641732283464568787 ) ) ;
#39353 = CARTESIAN_POINT ( 'NONE',  ( -0.006561679790025524116, -0.2845877964562159024, 0.3641732283464567677 ) ) ;
#39354 = CARTESIAN_POINT ( 'NONE',  ( 0.3018372703412079971, -0.4281496062992124485, 0.4176697321401328655 ) ) ;
#39355 = CARTESIAN_POINT ( 'NONE',  ( -1.056430446194224881, -0.5511811023622046335, 0.09757992244046803654 ) ) ;
#39356 = CARTESIAN_POINT ( 'NONE',  ( 0.1958661417322836718, -0.3392501089628017219, -0.08860199294719349472 ) ) ;
#39357 = CARTESIAN_POINT ( 'NONE',  ( 0.7677165354330716118, -0.5400638737290844871, 0.3530559997133364547 ) ) ;
#39358 = CARTESIAN_POINT ( 'NONE',  ( -1.620734908136482577, 0.2952755905511811885, 0.1292274648535926551 ) ) ;
#39359 = CARTESIAN_POINT ( 'NONE',  ( -0.2362204724409447953, -0.4091458600556404646, -1.244750656167979086 ) ) ;
#39360 = CARTESIAN_POINT ( 'NONE',  ( -0.4790026246719154557, -0.3162353388693405765, 0.4822834645669290543 ) ) ;
#39361 = CARTESIAN_POINT ( 'NONE',  ( 0.1771653543307093182, 0.07958543189024085140, 0.2665933059059887866 ) ) ;
#39362 = CARTESIAN_POINT ( 'NONE',  ( -0.9383202099737524282, -0.3162353388693409650, -0.4822834645669289433 ) ) ;
#39363 = CARTESIAN_POINT ( 'NONE',  ( 0.8792650918635177559, -0.004921259842519576551, 0.3153832671262227771 ) ) ;
#39364 = CARTESIAN_POINT ( 'NONE',  ( -0.1837270341207343505, -0.5023911411419708095, 0.1820866141732285504 ) ) ;
#39365 = CARTESIAN_POINT ( 'NONE',  ( -0.4724409448818890911, -0.1870078740157479769, 0.4822834645669291653 ) ) ;
#39366 = CARTESIAN_POINT ( 'NONE',  ( -1.312335958005248715, -0.6046776061558809534, -0.2411417322834644161 ) ) ;
#39367 = CARTESIAN_POINT ( 'NONE',  ( -1.574803149606298192, -0.1870078740157480879, -0.4822834645669291653 ) ) ;
#39368 = LINE ( 'NONE', #60396, #23294 ) ;
#39369 = CARTESIAN_POINT ( 'NONE',  ( 1.463254593175853824, -0.5511811023622046335, 0.09757992244046803654 ) ) ;
#39370 = CARTESIAN_POINT ( 'NONE',  ( 0.3149606299212606708, -0.1870078740157480879, -0.4822834645669291653 ) ) ;
#39371 = CARTESIAN_POINT ( 'NONE',  ( -1.502624671916009680, -0.3162353388693405765, 0.4822834645669290543 ) ) ;
#39372 = CARTESIAN_POINT ( 'NONE',  ( -1.548556430446193399, 0.2306618581243848609, 0.2411417322834645549 ) ) ;
#39373 = ORIENTED_EDGE ( 'NONE', *, *, #21410, .T. ) ;
#39374 = EDGE_CURVE ( 'NONE', #29467, #21709, #29174, .T. ) ;
#39375 = CARTESIAN_POINT ( 'NONE',  ( 0.1998031496062992463, 0.3460692066303959202, -2.268372703412073310 ) ) ;
#39376 = CARTESIAN_POINT ( 'NONE',  ( -1.056430446194224881, -0.5511811023622046335, 0.09757992244046803654 ) ) ;
#39377 = CARTESIAN_POINT ( 'NONE',  ( 0.6692913385826777528, 0.2952755905511811885, 0.000000000000000000 ) ) ;
#39378 = CARTESIAN_POINT ( 'NONE',  ( -0.9776902887139098386, -0.5511811023622046335, 0.09757992244046803654 ) ) ;
#39379 = CARTESIAN_POINT ( 'NONE',  ( 0.2925321140481932369, -0.2925321140481931814, -1.750000000000000222 ) ) ;
#39380 = CARTESIAN_POINT ( 'NONE',  ( -1.010498687664041384, -0.4281496062992127816, -0.4176697321401328100 ) ) ;
#39381 = CARTESIAN_POINT ( 'NONE',  ( 0.8267716535433078384, -0.6692913385826771977, 8.415575281601705876E-17 ) ) ;
#39382 = CARTESIAN_POINT ( 'NONE',  ( 0.4330708661417329575, 0.2952755905511811885, 0.000000000000000000 ) ) ;
#39383 = LINE ( 'NONE', #51997, #72136 ) ;
#39384 = CARTESIAN_POINT ( 'NONE',  ( -1.706036745406823485, 0.1283753931104748280, 0.1820866141732283561 ) ) ;
#39385 = CARTESIAN_POINT ( 'NONE',  ( -0.1070741851644051862, -0.3996062992125986035, -1.093832020997375309 ) ) ;
#39387 = ADVANCED_FACE ( 'NONE', ( #18303 ), #69642, .T. ) ;
#39386 = CARTESIAN_POINT ( 'NONE',  ( -0.2925321140481932924, 0.2925321140481931814, -1.437007874015747921 ) ) ;
#39388 = CARTESIAN_POINT ( 'NONE',  ( -0.1974969037888706647, 0.3420746716998658843, -0.6430446194225721834 ) ) ;
#39389 = AXIS2_PLACEMENT_3D ( 'NONE', #25480, #63794, #18769 ) ;
#39390 = DIRECTION ( 'NONE',  ( -1.000000000000000000, -3.096699300667737957E-16, 1.692413147294446216E-16 ) ) ;
#39391 = CARTESIAN_POINT ( 'NONE',  ( 0.5446194225721792126, -0.2845877964562159024, 0.3641732283464567677 ) ) ;
#39392 = CARTESIAN_POINT ( 'NONE',  ( 0.2362204724409456558, -0.1870078740157480601, -0.3641732283464567677 ) ) ;
#39393 = CARTESIAN_POINT ( 'NONE',  ( -0.03280839895013062252, -0.6692913385826771977, 0.1292274648535927661 ) ) ;
#39394 = CARTESIAN_POINT ( 'NONE',  ( 1.122047244094488860, 0.1660481256975885056, 0.3530559997133364547 ) ) ;
#39395 = CARTESIAN_POINT ( 'NONE',  ( -0.1058382717557497660, -0.3949938075777411073, -1.723753280839894986 ) ) ;
#39396 = CARTESIAN_POINT ( 'NONE',  ( 0.5249343832021005074, -0.5023911411419708095, 0.1820866141732285504 ) ) ;
#39397 = EDGE_CURVE ( 'NONE', #7338, #78564, #78414, .T. ) ;
#39398 = CARTESIAN_POINT ( 'NONE',  ( -0.9120734908136475250, -0.6692913385826773087, -0.1292274648535924053 ) ) ;
#39399 = CARTESIAN_POINT ( 'NONE',  ( 1.437007874015748810, 0.1660481256975885056, 0.3530559997133364547 ) ) ;
#39400 = CARTESIAN_POINT ( 'NONE',  ( 1.043307086614173818, 0.1660481256975885056, 0.3530559997133364547 ) ) ;
#39401 = CARTESIAN_POINT ( 'NONE',  ( -0.4724409448818898682, -8.678599364036362592E-17, -2.086614173228346303 ) ) ;
#39402 = ORIENTED_EDGE ( 'NONE', *, *, #79045, .T. ) ;
#39403 = ORIENTED_EDGE ( 'NONE', *, *, #3774, .F. ) ;
#39404 = VECTOR ( 'NONE', #9890, 39.37007874015748143 ) ;
#39405 = CARTESIAN_POINT ( 'NONE',  ( -1.227034120734907585, 0.2952755905511811885, 0.1292274648535926551 ) ) ;
#39406 = CARTESIAN_POINT ( 'NONE',  ( -0.8464566929133852113, 0.1660481256975885056, 0.3530559997133364547 ) ) ;
#39408 = CARTESIAN_POINT ( 'NONE',  ( -0.5643044619422565855, -0.4281496062992124485, 0.4176697321401328655 ) ) ;
#39407 = CARTESIAN_POINT ( 'NONE',  ( -0.7152230971128602510, -0.2845877964562159024, 0.3641732283464567677 ) ) ;
#39409 = CARTESIAN_POINT ( 'NONE',  ( -0.2867679344610364334, -0.2867679344610368219, -2.343812705215535974 ) ) ;
#39410 = CARTESIAN_POINT ( 'NONE',  ( 0.5314960629920847390, 2.755905511811024056, 3.937007874015794773 ) ) ;
#39411 = CARTESIAN_POINT ( 'NONE',  ( 1.528871391076116026, 0.2952755905511811885, 0.1292274648535926551 ) ) ;
#39412 = CARTESIAN_POINT ( 'NONE',  ( -1.430446194225721390, -0.4281496062992124485, 0.4176697321401328655 ) ) ;
#39413 = CARTESIAN_POINT ( 'NONE',  ( 0.4790026246719167324, -0.05778040916215522460, 0.4822834645669289988 ) ) ;
#39414 = CARTESIAN_POINT ( 'NONE',  ( -0.9645669291338575535, 0.1660481256975883668, -0.3530559997133364547 ) ) ;
#39415 = CARTESIAN_POINT ( 'NONE',  ( -0.3392501089628017219, -0.1958661417322836718, 0.1778215223097112108 ) ) ;
#39416 = CARTESIAN_POINT ( 'NONE',  ( 0.5183727034120741983, 0.2952755905511810774, -0.1292274648535930714 ) ) ;
#39417 = CARTESIAN_POINT ( 'NONE',  ( 0.1958661417322836440, -0.3392501089628017219, -1.816272965879265122 ) ) ;
#39418 = CARTESIAN_POINT ( 'NONE',  ( -0.7939632545931750718, -0.08942795157528024563, -0.3641732283464568787 ) ) ;
#39419 = VERTEX_POINT ( 'NONE', #30913 ) ;
#39420 = CARTESIAN_POINT ( 'NONE',  ( -0.1058382717557497937, -0.3949938075777411628, -1.961942257217847763 ) ) ;
#39421 = ORIENTED_EDGE ( 'NONE', *, *, #32070, .F. ) ;
#39422 = CARTESIAN_POINT ( 'NONE',  ( -1.541994750656167090, 0.1771653543307087630, 0.09757992244046791164 ) ) ;
#39423 = CARTESIAN_POINT ( 'NONE',  ( -1.161417322834644716, -0.5400638737290845981, -0.3530559997133363437 ) ) ;
#39424 = CARTESIAN_POINT ( 'NONE',  ( -1.141732283464566011, 0.2952755905511811885, 0.000000000000000000 ) ) ;
#39425 = CARTESIAN_POINT ( 'NONE',  ( 0.3460692066303959202, 0.1998031496062993295, -0.6036745406824146620 ) ) ;
#39426 = CARTESIAN_POINT ( 'NONE',  ( -1.069553805774277722, 0.2952755905511811885, 0.1292274648535926551 ) ) ;
#39427 = CARTESIAN_POINT ( 'NONE',  ( -1.076115485564303809, 0.2306618581243848609, 0.2411417322834645549 ) ) ;
#39428 = CARTESIAN_POINT ( 'NONE',  ( -1.620734908136482577, 0.2952755905511811885, 0.1292274648535926551 ) ) ;
#39429 = CARTESIAN_POINT ( 'NONE',  ( -1.595398199321656829, 0.7375059713363286695, -0.1559797534342474701 ) ) ;
#39430 = CARTESIAN_POINT ( 'NONE',  ( 0.2165354330708668673, -0.4536011799217367080, 0.2665933059059888421 ) ) ;
#39431 = CARTESIAN_POINT ( 'NONE',  ( 1.595398199321655497, 0.4829664696085563258, 0.1559797534342492742 ) ) ;
#39432 = CARTESIAN_POINT ( 'NONE',  ( -0.1049643490035307020, 0.3917322834645669549, -0.2486876640419948270 ) ) ;
#39433 = CARTESIAN_POINT ( 'NONE',  ( -0.3083989501312330295, -0.08942795157527998196, 0.3641732283464567121 ) ) ;
#39434 = CARTESIAN_POINT ( 'NONE',  ( -0.6561679790026240244, 0.2306618581243847221, -0.2411417322834647770 ) ) ;
#39435 = CARTESIAN_POINT ( 'NONE',  ( 0.7742782152230978099, -0.4281496062992124485, 0.4176697321401328655 ) ) ;
#39436 = CARTESIAN_POINT ( 'NONE',  ( -0.5249343832020990641, 0.2306618581243848609, 0.2411417322834645549 ) ) ;
#39437 = ORIENTED_EDGE ( 'NONE', *, *, #52610, .T. ) ;
#39438 = EDGE_LOOP ( 'NONE', ( #18224, #33867, #79331, #47472, #73713 ) ) ;
#39439 = CARTESIAN_POINT ( 'NONE',  ( -0.1070741851644056997, 0.3996062992125984925, -2.130577427821522374 ) ) ;
#39440 = CARTESIAN_POINT ( 'NONE',  ( -0.8989501312335946848, -0.6692913385826771977, 0.1292274648535927661 ) ) ;
#39441 = CARTESIAN_POINT ( 'NONE',  ( 1.213910761154856299, -0.6692913385826773087, -0.1292274648535924053 ) ) ;
#39442 = CARTESIAN_POINT ( 'NONE',  ( -1.469816272965878357, -0.5023911411419708095, -0.1820866141732282451 ) ) ;
#39443 = CARTESIAN_POINT ( 'NONE',  ( -0.09423411257991823331, 1.063451938596666979, 0.2574397322871235794 ) ) ;
#39444 = CARTESIAN_POINT ( 'NONE',  ( 0.3458507752293908943, -0.3458507752293908943, -0.8858267716535430658 ) ) ;
#39445 = CARTESIAN_POINT ( 'NONE',  ( -0.4744094488189105063, 1.521916954317726667, 3.908320185825789217 ) ) ;
#39446 = CARTESIAN_POINT ( 'NONE',  ( -0.2867679344610365999, 0.2867679344610364889, -0.3267716535433070613 ) ) ;
#39447 = CARTESIAN_POINT ( 'NONE',  ( -0.1958661417322834220, -0.3392501089628018884, -2.040026246719160330 ) ) ;
#39448 = CARTESIAN_POINT ( 'NONE',  ( -0.1509186351706028884, -0.3162353388693409650, -0.4822834645669289433 ) ) ;
#39449 = CARTESIAN_POINT ( 'NONE',  ( -1.522309711286088607, -0.5023911411419708095, 0.1820866141732285504 ) ) ;
#39450 = CARTESIAN_POINT ( 'NONE',  ( -0.8923884514435688198, 0.2306618581243847221, -0.2411417322834647770 ) ) ;
#39451 = CARTESIAN_POINT ( 'NONE',  ( -0.3460692066303960313, 0.1998031496062989965, -0.2604986876640419946 ) ) ;
#39453 = CARTESIAN_POINT ( 'NONE',  ( -0.1265901696524986964, -0.4724409448818899238, -1.093832020997375309 ) ) ;
#39452 = CARTESIAN_POINT ( 'NONE',  ( -1.095800524934382292, -0.05778040916215522460, 0.4822834645669289988 ) ) ;
#39454 = ADVANCED_FACE ( 'NONE', ( #49856 ), #27525, .F. ) ;
#39455 = CARTESIAN_POINT ( 'NONE',  ( -0.9711286089238838626, -0.6046776061558807314, 0.2411417322834647770 ) ) ;
#39456 = CARTESIAN_POINT ( 'NONE',  ( -0.3346456692913377662, -0.5400638737290844871, 0.3530559997133364547 ) ) ;
#39457 = CARTESIAN_POINT ( 'NONE',  ( 0.2891555358219910499, -0.2891555358219909944, -2.694881889763779625 ) ) ;
#39458 = CARTESIAN_POINT ( 'NONE',  ( 0.8267716535433077274, 0.1771653543307087630, 0.000000000000000000 ) ) ;
#39459 = CARTESIAN_POINT ( 'NONE',  ( 0.3392501089628018884, -0.1958661417322834220, -0.1896325459317586282 ) ) ;
#39460 = CIRCLE ( 'NONE', #70387, 1.220472440944881942 ) ;
#39461 = CARTESIAN_POINT ( 'NONE',  ( 0.6561679790026253567, -0.5023911411419708095, -0.1820866141732282451 ) ) ;
#39462 = CARTESIAN_POINT ( 'NONE',  ( 1.384514435695538337, -0.5511811023622046335, 0.09757992244046803654 ) ) ;
#39463 = CARTESIAN_POINT ( 'NONE',  ( 1.541994750656168645, -0.6692913385826771977, 0.1292274648535927661 ) ) ;
#39464 = UNCERTAINTY_MEASURE_WITH_UNIT (LENGTH_MEASURE( 1.000000000000000082E-05 ), #73830, 'distance_accuracy_value', 'NONE');
#39465 = CARTESIAN_POINT ( 'NONE',  ( 0.1640419947506569498, -0.2845877964562161244, -0.3641732283464567121 ) ) ;
#39466 = CARTESIAN_POINT ( 'NONE',  ( -9.594673741351313045E-17, 0.3917322834645670104, -1.881889763779527769 ) ) ;
#39467 = CARTESIAN_POINT ( 'NONE',  ( -1.377952755905511140, -0.6692913385826771977, 8.415575281601705876E-17 ) ) ;
#39468 = CARTESIAN_POINT ( 'NONE',  ( 1.417322834645670104, -0.1870078740157479769, 0.4822834645669291653 ) ) ;
#39469 = CARTESIAN_POINT ( 'NONE',  ( 0.1265901696524990294, -0.4724409448818896462, -0.004593175853018378711 ) ) ;
#39470 = CARTESIAN_POINT ( 'NONE',  ( -0.6233595800524928121, -0.2845877964562161244, -0.3641732283464567121 ) ) ;
#39471 = CARTESIAN_POINT ( 'NONE',  ( -0.4527559055118102749, 0.1660481256975885056, 0.3530559997133364547 ) ) ;
#39472 = CARTESIAN_POINT ( 'NONE',  ( 0.5118110236220480003, -0.6692913385826771977, 8.415575281601705876E-17 ) ) ;
#39473 = FACE_OUTER_BOUND ( 'NONE', #78112, .T. ) ;
#39474 = CIRCLE ( 'NONE', #12618, 1.122047244094488194 ) ;
#39475 = CARTESIAN_POINT ( 'NONE',  ( 0.7939632545931766261, -0.08942795157527998196, 0.3641732283464567121 ) ) ;
#39476 = CARTESIAN_POINT ( 'NONE',  ( -0.03937007874015669567, -0.5511811023622047445, 6.969142054262312111E-17 ) ) ;
#39477 = CARTESIAN_POINT ( 'NONE',  ( -0.4527559055118102749, -0.5400638737290845981, -0.3530559997133363437 ) ) ;
#39478 = CARTESIAN_POINT ( 'NONE',  ( -1.423884514435694859, -0.3162353388693405765, 0.4822834645669290543 ) ) ;
#39479 = CARTESIAN_POINT ( 'NONE',  ( -0.5971128608923877978, -0.5511811023622048555, -0.09757992244046775898 ) ) ;
#39480 = CARTESIAN_POINT ( 'NONE',  ( -1.559171609364246924, 0.3937007874015747699, 0.4177787735906735578 ) ) ;
#39481 = CARTESIAN_POINT ( 'NONE',  ( 0.6299212598425204535, -0.1870078740157480879, -0.4822834645669291653 ) ) ;
#39482 = CARTESIAN_POINT ( 'NONE',  ( -0.8661417322834640276, -0.1870078740157479769, 0.4822834645669291653 ) ) ;
#39483 = CARTESIAN_POINT ( 'NONE',  ( 0.2925321140481932369, -0.2925321140481931814, -1.120078740157480324 ) ) ;
#39484 = CARTESIAN_POINT ( 'NONE',  ( -0.1958661417322834220, -0.3392501089628018884, -2.669947506561679784 ) ) ;
#39485 = CARTESIAN_POINT ( 'NONE',  ( 0.2493438320209980519, -0.3690944881889765550, -0.3153832671262227771 ) ) ;
#39486 = CARTESIAN_POINT ( 'NONE',  ( -0.9711286089238838626, 0.2306618581243847221, -0.2411417322834647770 ) ) ;
#39487 = CARTESIAN_POINT ( 'NONE',  ( -1.279527559055116948, 0.1660481256975883668, -0.3530559997133364547 ) ) ;
#39488 = CARTESIAN_POINT ( 'NONE',  ( -1.292650918635170010, 0.1771653543307087075, -0.09757992244046823083 ) ) ;
#39489 = DIRECTION ( 'NONE',  ( 1.000000000000000000, -0.000000000000000000, -0.000000000000000000 ) ) ;
#39490 = CARTESIAN_POINT ( 'NONE',  ( -0.8530183727034112984, -0.004921259842519576551, 0.3153832671262227771 ) ) ;
#39491 = CARTESIAN_POINT ( 'NONE',  ( 0.4563452811745912219, 0.01305114060239447211, 2.130073781772667374 ) ) ;
#39492 = CARTESIAN_POINT ( 'NONE',  ( 1.430446194225722500, 0.05413385826771666132, 0.4176697321401328100 ) ) ;
#39493 = CARTESIAN_POINT ( 'NONE',  ( 0.3996062992125986035, 0.1070741851644054776, 0.03280839895013121926 ) ) ;
#39494 = CARTESIAN_POINT ( 'NONE',  ( 0.2867679344610366554, -0.2867679344610365999, -2.614848712107298745 ) ) ;
#39495 = EDGE_LOOP ( 'NONE', ( #79987, #58306, #42841, #67716 ) ) ;
#39496 = CARTESIAN_POINT ( 'NONE',  ( 0.02190130575838795945, -0.3959418824714272533, -2.713666019654406154E-16 ) ) ;
#39497 = CARTESIAN_POINT ( 'NONE',  ( -1.574803149606298636, -0.1870078740157479769, 0.4822834645669291653 ) ) ;
#39498 = CARTESIAN_POINT ( 'NONE',  ( -1.502624671916009680, -0.05778040916215560624, -0.4822834645669293319 ) ) ;
#39499 = CARTESIAN_POINT ( 'NONE',  ( 1.076115485564305141, -0.6046776061558807314, 0.2411417322834647770 ) ) ;
#39500 = CARTESIAN_POINT ( 'NONE',  ( -0.3917322834645670104, -7.196005306013484475E-17, -2.328740157480315265 ) ) ;
#39501 = PLANE ( 'NONE',  #6874 ) ;
#39502 = CARTESIAN_POINT ( 'NONE',  ( 0.3674540682414705883, -0.6046776061558807314, 0.2411417322834647770 ) ) ;
#39503 = CARTESIAN_POINT ( 'NONE',  ( 8.195543980992789655E-16, -0.1870078740157480879, -0.4822834645669291653 ) ) ;
#39504 = CARTESIAN_POINT ( 'NONE',  ( 0.3765731398154819609, 1.248435479399690573, -3.918969628814140904 ) ) ;
#39505 = CARTESIAN_POINT ( 'NONE',  ( -0.3996062992125985480, -0.1070741851644057135, -2.093175853018372834 ) ) ;
#39506 = CARTESIAN_POINT ( 'NONE',  ( 0.7939632545931766261, -0.08942795157527998196, 0.3641732283464567121 ) ) ;
#39507 = CARTESIAN_POINT ( 'NONE',  ( -0.2925321140481932924, 0.2925321140481931814, -1.437007874015747921 ) ) ;
#39508 = ORIENTED_EDGE ( 'NONE', *, *, #82082, .T. ) ;
#39509 = CARTESIAN_POINT ( 'NONE',  ( 0.1958661417322836440, -0.3392501089628017219, -2.918635170603674389 ) ) ;
#39510 = EDGE_LOOP ( 'NONE', ( #6684, #18089 ) ) ;
#39511 = CARTESIAN_POINT ( 'NONE',  ( -0.01968503937007793844, -0.5400638737290844871, 0.3530559997133364547 ) ) ;
#39512 = CARTESIAN_POINT ( 'NONE',  ( 1.259842519685040019, -0.1870078740157479769, 0.4822834645669291653 ) ) ;
#39513 = CARTESIAN_POINT ( 'NONE',  ( 0.5249343832021005074, -0.6046776061558807314, 0.2411417322834647770 ) ) ;
#39514 = VECTOR ( 'NONE', #74751, 39.37007874015748143 ) ;
#39515 = CARTESIAN_POINT ( 'NONE',  ( 1.246719160104987623, 0.05413385826771626580, -0.4176697321401330321 ) ) ;
#39516 = CARTESIAN_POINT ( 'NONE',  ( -0.5183727034120726440, 0.2952755905511811885, 0.1292274648535926551 ) ) ;
#39517 = CARTESIAN_POINT ( 'NONE',  ( -0.05905511811023545637, -0.5400638737290845981, -0.3530559997133363437 ) ) ;
#39518 = CARTESIAN_POINT ( 'NONE',  ( 1.450131233595801428, 0.2952755905511811885, 0.1292274648535926551 ) ) ;
#39519 = CARTESIAN_POINT ( 'NONE',  ( 1.482939632545932307, 0.05413385826771626580, -0.4176697321401330321 ) ) ;
#39520 = CARTESIAN_POINT ( 'NONE',  ( 1.292650918635171564, -0.6692913385826773087, -0.1292274648535924053 ) ) ;
#39521 = CARTESIAN_POINT ( 'NONE',  ( 4.797336870675656522E-17, -0.3917322834645670104, -0.07086614173228342195 ) ) ;
#39522 = CARTESIAN_POINT ( 'NONE',  ( 0.2952755905511819101, 0.07958543189024071263, -0.2665933059059888421 ) ) ;
#39523 = ORIENTED_EDGE ( 'NONE', *, *, #25084, .F. ) ;
#39524 = CARTESIAN_POINT ( 'NONE',  ( 0.1974969037888706369, -0.3420746716998659953, -0.4068241469816273326 ) ) ;
#39525 = ORIENTED_EDGE ( 'NONE', *, *, #6951, .T. ) ;
#39526 = CARTESIAN_POINT ( 'NONE',  ( -0.2887139107611542133, 0.1283753931104748280, 0.1820866141732283561 ) ) ;
#39527 = CARTESIAN_POINT ( 'NONE',  ( -0.1640419947506553400, -0.05778040916215560624, -0.4822834645669293319 ) ) ;
#39528 = CARTESIAN_POINT ( 'NONE',  ( 2.585342365690415978, 1.422987107291905362, 0.4606739315415591673 ) ) ;
#39529 = CARTESIAN_POINT ( 'NONE',  ( -0.03937007874015669567, -0.6692913385826771977, 8.415575281601705876E-17 ) ) ;
#39530 = CARTESIAN_POINT ( 'NONE',  ( 0.01312335958005323398, 0.05413385826771666132, 0.4176697321401328100 ) ) ;
#39531 = CARTESIAN_POINT ( 'NONE',  ( -0.9842519685039360366, 0.2952755905511811885, 0.000000000000000000 ) ) ;
#39532 = CARTESIAN_POINT ( 'NONE',  ( -1.135170603674539924, -0.6692913385826771977, 0.1292274648535927661 ) ) ;
#39533 = VECTOR ( 'NONE', #9290, 39.37007874015748143 ) ;
#39534 = CARTESIAN_POINT ( 'NONE',  ( 1.463254593175853824, -0.5511811023622046335, 0.09757992244046803654 ) ) ;
#39535 = CARTESIAN_POINT ( 'NONE',  ( -1.430446194225720724, 0.05413385826771626580, -0.4176697321401330321 ) ) ;
#39536 = CARTESIAN_POINT ( 'NONE',  ( -0.3503937007874015630, -0.3733313776025731778, -1.512162153811850596 ) ) ;
#39537 = CARTESIAN_POINT ( 'NONE',  ( 1.095800524934383846, -0.2845877964562159024, 0.3641732283464567677 ) ) ;
#39538 = CARTESIAN_POINT ( 'NONE',  ( 0.2887139107611556010, 0.2306618581243847221, -0.2411417322834647770 ) ) ;
#39539 = CARTESIAN_POINT ( 'NONE',  ( 0.7874015748031503170, -0.1870078740157480879, -0.4822834645669291653 ) ) ;
#39540 = CARTESIAN_POINT ( 'NONE',  ( -0.3996062992125986035, -0.1070741851644056997, -1.463254593175853158 ) ) ;
#39541 = CARTESIAN_POINT ( 'NONE',  ( -1.712598425196849572, 0.1660481256975885056, 0.3530559997133364547 ) ) ;
#39542 = CARTESIAN_POINT ( 'NONE',  ( 0.1070741851644053388, 0.3996062992125986035, -0.5426509186351704539 ) ) ;
#39543 = CARTESIAN_POINT ( 'NONE',  ( 0.1998031496062994128, -0.3460692066303957537, -0.01115485564304463835 ) ) ;
#39544 = CARTESIAN_POINT ( 'NONE',  ( -0.6692913385826764205, -0.6692913385826771977, 8.415575281601705876E-17 ) ) ;
#39545 = CARTESIAN_POINT ( 'NONE',  ( 0.1070741851644054915, -0.3996062992125986035, -2.604986876640420057 ) ) ;
#39546 = CARTESIAN_POINT ( 'NONE',  ( 4.797336870675656522E-17, -0.3917322834645670104, -2.210629921259842590 ) ) ;
#39547 = CARTESIAN_POINT ( 'NONE',  ( -1.076115485564303809, -0.5023911411419708095, -0.1820866141732282451 ) ) ;
#39548 = CARTESIAN_POINT ( 'NONE',  ( 1.108923884514436242, -0.05778040916215522460, 0.4822834645669289988 ) ) ;
#39549 = CARTESIAN_POINT ( 'NONE',  ( 0.8858267716535438430, 0.1660481256975885056, 0.3530559997133364547 ) ) ;
#39550 = CARTESIAN_POINT ( 'NONE',  ( -0.1771653543307080136, 0.07958543189024071263, -0.2665933059059888421 ) ) ;
#39551 = CARTESIAN_POINT ( 'NONE',  ( 0.5183727034120741983, 0.2952755905511810774, -0.1292274648535930714 ) ) ;
#39552 = CARTESIAN_POINT ( 'NONE',  ( -0.4091458600556405756, 0.2362204724409446288, -1.362860892388451539 ) ) ;
#39553 = CARTESIAN_POINT ( 'NONE',  ( 0.3937007874015754361, -0.1870078740157479769, 0.3641732283464567677 ) ) ;
#39554 = CARTESIAN_POINT ( 'NONE',  ( 0.1312335958005255154, -0.6046776061558807314, 0.2411417322834647770 ) ) ;
#39555 = ADVANCED_FACE ( 'NONE', ( #39969 ), #58476, .F. ) ;
#39556 = CARTESIAN_POINT ( 'NONE',  ( 0.3949938075777409408, -0.1058382717557499186, -1.290682414698162583 ) ) ;
#39557 = CARTESIAN_POINT ( 'NONE',  ( -1.240157480314959759, 0.1660481256975885056, 0.3530559997133364547 ) ) ;
#39558 = CARTESIAN_POINT ( 'NONE',  ( 0.3280839895013130669, -0.004921259842519576551, 0.3153832671262227771 ) ) ;
#39559 = LINE ( 'NONE', #39134, #47403 ) ;
#39560 = CARTESIAN_POINT ( 'NONE',  ( -0.8005249343832013809, -0.4281496062992124485, 0.4176697321401328655 ) ) ;
#39561 = CARTESIAN_POINT ( 'NONE',  ( -0.5118110236220466680, 0.1771653543307087630, 0.000000000000000000 ) ) ;
#39562 = CARTESIAN_POINT ( 'NONE',  ( 1.150409065943327480, 0.1377952755905511861, 0.8265612839971842041 ) ) ;
#39563 = CARTESIAN_POINT ( 'NONE',  ( -0.7874015748031489847, -0.1870078740157479769, 0.4822834645669291653 ) ) ;
#39564 = CARTESIAN_POINT ( 'NONE',  ( -0.7283464566929126471, -0.5400638737290844871, 0.3530559997133364547 ) ) ;
#39565 = CARTESIAN_POINT ( 'NONE',  ( 0.4330708661417329575, -0.5511811023622047445, 6.969142054262312111E-17 ) ) ;
#39566 = CARTESIAN_POINT ( 'NONE',  ( -0.3996062992125984925, -0.1070741851644056858, -2.012467191601049699 ) ) ;
#39567 = CARTESIAN_POINT ( 'NONE',  ( -0.1574803149606292529, -0.1870078740157480879, -0.4822834645669291653 ) ) ;
#39568 = CARTESIAN_POINT ( 'NONE',  ( -0.1958661417322836440, 0.3392501089628016664, -2.140400631724722835 ) ) ;
#39569 = CARTESIAN_POINT ( 'NONE',  ( -1.437007874015747477, -0.4536011799217367080, 0.2665933059059888421 ) ) ;
#39570 = CARTESIAN_POINT ( 'NONE',  ( 0.8398950131233602345, -0.5023911411419708095, 0.1820866141732285504 ) ) ;
#39571 = CARTESIAN_POINT ( 'NONE',  ( 1.272965879265092637, 0.05413385826771666132, 0.4176697321401328100 ) ) ;
#39572 = CARTESIAN_POINT ( 'NONE',  ( -0.6889763779527552368, -0.4536011799217368745, -0.2665933059059886201 ) ) ;
#39573 = CARTESIAN_POINT ( 'NONE',  ( -1.364829396325458521, 0.1283753931104746893, -0.1820866141732285504 ) ) ;
#39574 = CARTESIAN_POINT ( 'NONE',  ( -0.6627296587926501115, 0.2952755905511810774, -0.1292274648535930714 ) ) ;
#39575 = CARTESIAN_POINT ( 'NONE',  ( -0.2887139107611542133, 0.2306618581243848609, 0.2411417322834645549 ) ) ;
#39576 = CARTESIAN_POINT ( 'NONE',  ( 0.7217847769028878924, -0.004921259842519576551, 0.3153832671262227771 ) ) ;
#39577 = CARTESIAN_POINT ( 'NONE',  ( -0.2845256677560919489, 0.07972153265861246785, 5.543321648279010638 ) ) ;
#39578 = CARTESIAN_POINT ( 'NONE',  ( 1.161417322834646271, 0.07958543189024071263, -0.2665933059059888421 ) ) ;
#39579 = CIRCLE ( 'NONE', #81295, 0.5118110236220472231 ) ;
#39580 = CARTESIAN_POINT ( 'NONE',  ( 0.5118110236220480003, -0.6692913385826771977, 8.415575281601705876E-17 ) ) ;
#39581 = CARTESIAN_POINT ( 'NONE',  ( -0.1998031496062994405, 0.3460692066303957537, 0.06758530183727033680 ) ) ;
#39582 = CARTESIAN_POINT ( 'NONE',  ( -0.7086614173228339419, -0.1870078740157480879, -0.4822834645669291653 ) ) ;
#39583 = CARTESIAN_POINT ( 'NONE',  ( -9.594673741351313045E-17, 0.3917322834645670104, -1.344488188976378007 ) ) ;
#39584 = CARTESIAN_POINT ( 'NONE',  ( 1.292650918635171564, 0.1771653543307087630, 0.09757992244046791164 ) ) ;
#39585 = CARTESIAN_POINT ( 'NONE',  ( 0.6364829396325465405, -0.3162353388693409650, -0.4822834645669289433 ) ) ;
#39586 = CARTESIAN_POINT ( 'NONE',  ( 0.3018372703412079971, 0.05413385826771626580, -0.4176697321401330321 ) ) ;
#39587 = FACE_OUTER_BOUND ( 'NONE', #11796, .T. ) ;
#39588 = CARTESIAN_POINT ( 'NONE',  ( 0.1312335958005257930, 0.1283753931104746893, -0.1820866141732285504 ) ) ;
#39589 = CARTESIAN_POINT ( 'NONE',  ( 0.8070866141732289112, -0.5400638737290845981, -0.3530559997133363437 ) ) ;
#39590 = CARTESIAN_POINT ( 'NONE',  ( -0.2034120734908131112, -0.5511811023622048555, -0.09757992244046775898 ) ) ;
#39591 = AXIS2_PLACEMENT_3D ( 'NONE', #10369, #3217, #72674 ) ;
#39592 = CARTESIAN_POINT ( 'NONE',  ( -0.5905511811023613777, -0.6692913385826771977, 8.415575281601705876E-17 ) ) ;
#39593 = DIRECTION ( 'NONE',  ( 0.000000000000000000, -1.601283208593976204E-15, -1.000000000000000000 ) ) ;
#39594 = CARTESIAN_POINT ( 'NONE',  ( -0.3477690288713905509, -0.6692913385826771977, 0.1292274648535927661 ) ) ;
#39595 = VERTEX_POINT ( 'NONE', #13882 ) ;
#39596 = CARTESIAN_POINT ( 'NONE',  ( -1.167979002624671470, 0.05413385826771666132, 0.4176697321401328100 ) ) ;
#39597 = CARTESIAN_POINT ( 'NONE',  ( -0.5905511811023615998, 0.1771653543307087630, 0.000000000000000000 ) ) ;
#39598 = CARTESIAN_POINT ( 'NONE',  ( -0.1181102362204717315, 0.2952755905511811885, 0.000000000000000000 ) ) ;
#39599 = CARTESIAN_POINT ( 'NONE',  ( -1.069553805774277722, 0.2952755905511811885, 0.1292274648535926551 ) ) ;
#39600 = CARTESIAN_POINT ( 'NONE',  ( -0.5839895013123351797, -0.6692913385826771977, 0.1292274648535927661 ) ) ;
#39601 = LINE ( 'NONE', #8453, #37748 ) ;
#39603 = CARTESIAN_POINT ( 'NONE',  ( 0.7349081364829402885, -0.6046776061558809534, -0.2411417322834644161 ) ) ;
#39602 = CARTESIAN_POINT ( 'NONE',  ( -0.8989501312335947958, 0.2952755905511810219, -0.1292274648535930437 ) ) ;
#39604 = CARTESIAN_POINT ( 'NONE',  ( 1.469816272965879911, -0.6046776061558807314, 0.2411417322834647770 ) ) ;
#39605 = CARTESIAN_POINT ( 'NONE',  ( -9.594673741351313045E-17, 0.3917322834645670104, -2.354330708661417138 ) ) ;
#39606 = B_SPLINE_CURVE_WITH_KNOTS ( 'NONE', 3,
 ( #32103, #76321, #44295, #549 ),
 .UNSPECIFIED., .F., .F.,
 ( 4, 4 ),
 ( 3.210432057656183116E-07, 0.001287787053612148448 ),
 .UNSPECIFIED. ) ;
#39607 = DIRECTION ( 'NONE',  ( -1.000000000000000000, 1.445602896647338917E-16, -0.000000000000000000 ) ) ;
#39608 = CARTESIAN_POINT ( 'NONE',  ( -1.312335958005248715, -0.6046776061558809534, -0.2411417322834644161 ) ) ;
#39609 = CARTESIAN_POINT ( 'NONE',  ( -1.157146581871515012E-16, 0.4724409448818898682, -0.6299212598425196763 ) ) ;
#39610 = CARTESIAN_POINT ( 'NONE',  ( -0.2925321140481932924, 0.2925321140481931814, -0.01968503937007875723 ) ) ;
#39611 = ORIENTED_EDGE ( 'NONE', *, *, #1240, .F. ) ;
#39612 = CARTESIAN_POINT ( 'NONE',  ( -0.1509186351706028884, -0.2845877964562161244, -0.3641732283464567121 ) ) ;
#39613 = CARTESIAN_POINT ( 'NONE',  ( 0.3392501089628018884, -0.1958661417322834220, -1.986876640419947604 ) ) ;
#39614 = EDGE_LOOP ( 'NONE', ( #31782, #38071, #60148, #48139 ) ) ;
#39615 = CARTESIAN_POINT ( 'NONE',  ( 0.1968503937007881344, 0.2952755905511811885, 0.000000000000000000 ) ) ;
#39616 = CARTESIAN_POINT ( 'NONE',  ( -0.1377952755905504645, 0.1660481256975885056, 0.3530559997133364547 ) ) ;
#39617 = CARTESIAN_POINT ( 'NONE',  ( -0.5839895013123351797, -0.6692913385826771977, 0.1292274648535927661 ) ) ;
#39618 = DIRECTION ( 'NONE',  ( 0.000000000000000000, 0.000000000000000000, -1.000000000000000000 ) ) ;
#39619 = CARTESIAN_POINT ( 'NONE',  ( -0.6955380577427815458, -0.004921259842519576551, 0.3153832671262227771 ) ) ;
#39620 = CARTESIAN_POINT ( 'NONE',  ( 0.5839895013123367340, 0.2952755905511811885, 0.1292274648535926551 ) ) ;
#39621 = CARTESIAN_POINT ( 'NONE',  ( 0.5905511811023629321, -0.5511811023622047445, 6.969142054262312111E-17 ) ) ;
#39622 = CARTESIAN_POINT ( 'NONE',  ( -0.4658792650918627265, -0.3162353388693409650, -0.4822834645669289433 ) ) ;
#39623 = B_SPLINE_CURVE_WITH_KNOTS ( 'NONE', 3,
 ( #23252, #56056, #81350, #10643 ),
 .UNSPECIFIED., .F., .F.,
 ( 4, 4 ),
 ( 1.999999999910059834E-07, 0.006970199999999935996 ),
 .UNSPECIFIED. ) ;
#39624 = CARTESIAN_POINT ( 'NONE',  ( -0.1049643490035306742, 0.3917322834645668994, -1.031476747210287037 ) ) ;
#39625 = CARTESIAN_POINT ( 'NONE',  ( -0.7283464566929126471, -0.5400638737290844871, 0.3530559997133364547 ) ) ;
#39626 = CARTESIAN_POINT ( 'NONE',  ( -0.3149606299212459048, 2.165354330708661568, -3.924389226575469625 ) ) ;
#39627 = CARTESIAN_POINT ( 'NONE',  ( 1.417322834645670104, -0.1870078740157480879, -0.4822834645669291653 ) ) ;
#39628 = CARTESIAN_POINT ( 'NONE',  ( 1.968503937007874072, 0.000000000000000000, 5.701968306260621233 ) ) ;
#39629 = ORIENTED_EDGE ( 'NONE', *, *, #46415, .T. ) ;
#39630 = CARTESIAN_POINT ( 'NONE',  ( 0.2867679344610366554, 0.2867679344610366554, -2.339258160926195984 ) ) ;
#39631 = CARTESIAN_POINT ( 'NONE',  ( 0.1377952755905518800, 0.1660481256975883668, -0.3530559997133364547 ) ) ;
#39632 = ORIENTED_EDGE ( 'NONE', *, *, #8988, .T. ) ;
#39633 = CARTESIAN_POINT ( 'NONE',  ( -0.7677165354330699465, 0.1660481256975885056, 0.3530559997133364547 ) ) ;
#39634 = CARTESIAN_POINT ( 'NONE',  ( 1.515748031496063186, -0.5400638737290845981, -0.3530559997133363437 ) ) ;
#39635 = CARTESIAN_POINT ( 'NONE',  ( 1.450131233595801428, 0.2952755905511811885, 0.1292274648535926551 ) ) ;
#39636 = CARTESIAN_POINT ( 'NONE',  ( 0.1574803149606306130, -0.1870078740157479769, 0.4822834645669291653 ) ) ;
#39637 = CARTESIAN_POINT ( 'NONE',  ( -0.1706036745406816491, 0.05413385826771626580, -0.4176697321401330321 ) ) ;
#39638 = CARTESIAN_POINT ( 'NONE',  ( 0.2867679344610365999, 0.2867679344610365999, -1.797244094488188892 ) ) ;
#39639 = CARTESIAN_POINT ( 'NONE',  ( -1.371391076115484831, 0.2952755905511810774, -0.1292274648535930714 ) ) ;
#39640 = CARTESIAN_POINT ( 'NONE',  ( -0.1640419947506553400, -0.05778040916215560624, -0.4822834645669293319 ) ) ;
#39641 = CARTESIAN_POINT ( 'NONE',  ( -0.3149606299212590610, -0.1870078740157480601, -0.3641732283464567677 ) ) ;
#39642 = CARTESIAN_POINT ( 'NONE',  ( 1.548556430446194954, 0.2306618581243847221, -0.2411417322834647770 ) ) ;
#39643 = CARTESIAN_POINT ( 'NONE',  ( 1.423884514435696413, -0.3162353388693409650, -0.4822834645669289433 ) ) ;
#39644 = CARTESIAN_POINT ( 'NONE',  ( -0.3740157480314953431, -0.5400638737290845981, -0.3530559997133363437 ) ) ;
#39645 = CARTESIAN_POINT ( 'NONE',  ( -0.6299212598425201204, 1.968503937007873628, 0.4915354330708656128 ) ) ;
#39646 = CARTESIAN_POINT ( 'NONE',  ( 1.167979002624672580, 0.05413385826771626580, -0.4176697321401330321 ) ) ;
#39647 = CARTESIAN_POINT ( 'NONE',  ( 0.4177787735907000366, 0.3937007874015748254, -1.736336963694947944 ) ) ;
#39648 = EDGE_CURVE ( 'NONE', #71206, #29072, #73539, .T. ) ;
#39649 = VERTEX_POINT ( 'NONE', #58901 ) ;
#39650 = CARTESIAN_POINT ( 'NONE',  ( 0.02624671916010564918, -0.6046776061558809534, -0.2411417322834644161 ) ) ;
#39651 = CARTESIAN_POINT ( 'NONE',  ( -0.2034120734908131112, -0.5511811023622048555, -0.09757992244046775898 ) ) ;
#39653 = CARTESIAN_POINT ( 'NONE',  ( -0.7137454485294948414, 2.165354330708661124, 0.4917280318828577412 ) ) ;
#39652 = CARTESIAN_POINT ( 'NONE',  ( 0.8923884514435703741, 0.1283753931104748280, 0.1820866141732283561 ) ) ;
#39654 = CARTESIAN_POINT ( 'NONE',  ( 0.4091458600556403535, 0.2362204724409449896, -0.05052493438320210251 ) ) ;
#39655 = CARTESIAN_POINT ( 'NONE',  ( 1.587926509186352586, -0.3690944881889765550, -0.3153832671262227771 ) ) ;
#39656 = CARTESIAN_POINT ( 'NONE',  ( 1.043307086614173818, -0.5400638737290845981, -0.3530559997133363437 ) ) ;
#39657 = AXIS2_PLACEMENT_3D ( 'NONE', #70909, #71739, #65008 ) ;
#39658 = CARTESIAN_POINT ( 'NONE',  ( -0.3420746716998662729, 0.1974969037888702206, -0.1030183727034120894 ) ) ;
#39659 = CARTESIAN_POINT ( 'NONE',  ( 0.2362204724409456558, -0.1870078740157480879, -0.4822834645669291653 ) ) ;
#39660 = CARTESIAN_POINT ( 'NONE',  ( -1.614173228346455824, 0.2952755905511811885, 0.000000000000000000 ) ) ;
#39661 = CARTESIAN_POINT ( 'NONE',  ( -1.509186351706035767, 0.05413385826771626580, -0.4176697321401330321 ) ) ;
#39662 = CARTESIAN_POINT ( 'NONE',  ( -0.2821522309711278487, 0.2952755905511811885, 0.1292274648535926551 ) ) ;
#39663 = CARTESIAN_POINT ( 'NONE',  ( -0.1974969037888706924, 0.3420746716998658843, 0.06758530183727033680 ) ) ;
#39664 = CARTESIAN_POINT ( 'NONE',  ( 1.489501312335958172, -0.3162353388693405765, 0.4822834645669290543 ) ) ;
#39665 = CARTESIAN_POINT ( 'NONE',  ( 0.5643044619422579178, -0.4281496062992127816, -0.4176697321401328100 ) ) ;
#39666 = CARTESIAN_POINT ( 'NONE',  ( 0.8202099737532814183, -0.5511811023622048555, -0.09757992244046775898 ) ) ;
#39667 = CARTESIAN_POINT ( 'NONE',  ( 0.1777261984983631582, 1.063163173673139505, 0.2579413877952805856 ) ) ;
#39668 = CARTESIAN_POINT ( 'NONE',  ( 0.2296587926509192634, -0.2845877964562159024, 0.3641732283464567677 ) ) ;
#39669 = CARTESIAN_POINT ( 'NONE',  ( -1.187664041994749731, -0.3162353388693405765, 0.4822834645669290543 ) ) ;
#39670 = CARTESIAN_POINT ( 'NONE',  ( -0.2925321140481932369, 0.2925321140481931259, -0.7263779527559056648 ) ) ;
#39671 = CARTESIAN_POINT ( 'NONE',  ( 0.9973753280839902091, -0.6046776061558807314, 0.2411417322834647770 ) ) ;
#39672 = CARTESIAN_POINT ( 'NONE',  ( 0.1958661417322834775, 0.3392501089628018884, -0.6089238845144356871 ) ) ;
#39674 = CARTESIAN_POINT ( 'NONE',  ( 0.4091458600556404646, -0.2362204724409448231, -0.4967191601049869010 ) ) ;
#39673 = CARTESIAN_POINT ( 'NONE',  ( 0.9251968503937015864, 0.1660481256975883668, -0.3530559997133364547 ) ) ;
#39675 = CARTESIAN_POINT ( 'NONE',  ( -0.3740157480314952876, 0.1012011053420777407, 0.2882089793578256898 ) ) ;
#39676 = B_SPLINE_CURVE_WITH_KNOTS ( 'NONE', 3,
 ( #23263, #9815, #74633, #42616 ),
 .UNSPECIFIED., .F., .F.,
 ( 4, 4 ),
 ( 1.999999999897049408E-07, 0.006970199999999935128 ),
 .UNSPECIFIED. ) ;
#39677 = CARTESIAN_POINT ( 'NONE',  ( 0.4986876640419954376, 0.1283753931104748280, 0.1820866141732283561 ) ) ;
#39678 = CARTESIAN_POINT ( 'NONE',  ( 0.5249343832021005074, -0.6046776061558807314, 0.2411417322834647770 ) ) ;
#39679 = CARTESIAN_POINT ( 'NONE',  ( -0.4744094488189043446, 1.546132656481028933, 2.170146923806632433 ) ) ;
#39680 = CARTESIAN_POINT ( 'NONE',  ( -1.089238845144356427, -0.004921259842519576551, 0.3153832671262227771 ) ) ;
#39681 = CARTESIAN_POINT ( 'NONE',  ( -1.207349081364828880, 0.2306618581243847221, -0.2411417322834647770 ) ) ;
#39682 = CARTESIAN_POINT ( 'NONE',  ( -1.581364829396324945, -0.3162353388693405765, 0.4822834645669290543 ) ) ;
#39683 = CARTESIAN_POINT ( 'NONE',  ( 1.161417322834646493, -0.5400638737290844871, 0.3530559997133364547 ) ) ;
#39684 = CARTESIAN_POINT ( 'NONE',  ( 1.528871391076116026, 0.2952755905511811885, 0.1292274648535926551 ) ) ;
#39685 = CARTESIAN_POINT ( 'NONE',  ( 1.016821367227983997, 1.521771543437157481, -0.4744094488188971281 ) ) ;
#39686 = CARTESIAN_POINT ( 'NONE',  ( 0.5314960629921264834, 0.1660481256975883668, -0.3530559997133364547 ) ) ;
#39687 = CARTESIAN_POINT ( 'NONE',  ( 0.1998031496062992463, 0.3460692066303959202, 0.09383202099737530943 ) ) ;
#39688 = DIRECTION ( 'NONE',  ( -0.000000000000000000, -1.000000000000000000, -0.000000000000000000 ) ) ;
#39689 = CARTESIAN_POINT ( 'NONE',  ( 1.456692913385827515, -0.6692913385826771977, 8.415575281601705876E-17 ) ) ;
#39690 = CARTESIAN_POINT ( 'NONE',  ( -1.509186351706035767, -0.004921259842519870586, -0.3153832671262229437 ) ) ;
#39692 = CARTESIAN_POINT ( 'NONE',  ( 1.377952755905512472, 0.1771653543307087630, 0.000000000000000000 ) ) ;
#39691 =( BOUNDED_CURVE ( )  B_SPLINE_CURVE ( 2, ( #53608, #22472, #27532, #16169, #53189, #48131, #21223 ),
 .UNSPECIFIED., .F., .F. ) 
 B_SPLINE_CURVE_WITH_KNOTS ( ( 3, 2, 2, 3 ),
 ( 0.07563788552403438725, 0.07916666666666666297, 0.08333333333333334259, 0.08750000000000000833 ),
 .UNSPECIFIED. ) 
 CURVE ( )  GEOMETRIC_REPRESENTATION_ITEM ( )  RATIONAL_B_SPLINE_CURVE ( ( 0.9911642120908014109, 0.9711423276059411025, 1.000000000000000000, 0.9659258262890683122, 1.000000000000000000, 0.9659258262890682012, 1.000000000000000222 ) ) 
 REPRESENTATION_ITEM ( '' )  );
#39693 = CARTESIAN_POINT ( 'NONE',  ( -1.325459317585300889, -0.004921259842519576551, 0.3153832671262227771 ) ) ;
#39694 = CARTESIAN_POINT ( 'NONE',  ( -0.3280839895013117347, -0.004921259842519870586, -0.3153832671262229437 ) ) ;
#39695 = CARTESIAN_POINT ( 'NONE',  ( -0.3458507752293909498, 0.3458507752293908388, -2.066929133858267598 ) ) ;
#39696 = CARTESIAN_POINT ( 'NONE',  ( 1.043307086614173818, -0.4536011799217368745, -0.2665933059059886201 ) ) ;
#39697 = CARTESIAN_POINT ( 'NONE',  ( 0.6364829396325465405, -0.3162353388693409650, -0.4822834645669289433 ) ) ;
#39698 = CARTESIAN_POINT ( 'NONE',  ( 0.9186351706036751663, -0.6046776061558807314, 0.2411417322834647770 ) ) ;
#39699 = CARTESIAN_POINT ( 'NONE',  ( 0.1902887139107617975, -0.6692913385826773087, -0.1292274648535924053 ) ) ;
#39700 = CARTESIAN_POINT ( 'NONE',  ( 0.5511811023622054106, -0.1870078740157480601, -0.3641732283464567677 ) ) ;
#39701 = CARTESIAN_POINT ( 'NONE',  ( 1.141732283464567566, 0.2952755905511811885, 0.000000000000000000 ) ) ;
#39702 = CYLINDRICAL_SURFACE ( 'NONE', #11073, 0.4744094488188972947 ) ;
#39703 = CARTESIAN_POINT ( 'NONE',  ( -0.5643044619422565855, 0.05413385826771626580, -0.4176697321401330321 ) ) ;
#39704 = CARTESIAN_POINT ( 'NONE',  ( 0.1070741851644053666, 0.3996062992125986035, -0.9383202099737532054 ) ) ;
#39705 = CARTESIAN_POINT ( 'NONE',  ( -0.4091458600556405756, 0.2362204724409446288, -1.205380577427821454 ) ) ;
#39706 = CARTESIAN_POINT ( 'NONE',  ( 0.1377952755905518800, -0.5400638737290844871, 0.3530559997133364547 ) ) ;
#39708 = VECTOR ( 'NONE', #39110, 39.37007874015748143 ) ;
#39707 = CARTESIAN_POINT ( 'NONE',  ( -0.3215223097112853146, -0.05778040916215560624, -0.4822834645669293319 ) ) ;
#39709 = CARTESIAN_POINT ( 'NONE',  ( -0.06561679790026180015, -0.4281496062992127816, -0.4176697321401328100 ) ) ;
#39710 = CARTESIAN_POINT ( 'NONE',  ( 0.3460692066303959757, -0.1998031496062991907, -2.782152230971128848 ) ) ;
#39711 = CARTESIAN_POINT ( 'NONE',  ( 0.1058382717557500713, -0.3949938075777409408, -2.132545931758530244 ) ) ;
#39712 = CARTESIAN_POINT ( 'NONE',  ( -0.2867679344610364334, -0.2867679344610367109, -0.5236220472440944462 ) ) ;
#39713 = CARTESIAN_POINT ( 'NONE',  ( 0.1958661417322836440, -0.3392501089628017219, -0.8713910761154854967 ) ) ;
#39714 = CARTESIAN_POINT ( 'NONE',  ( -0.7742782152230965886, -0.004921259842519576551, 0.3153832671262227771 ) ) ;
#39715 = CARTESIAN_POINT ( 'NONE',  ( -0.2867679344610365999, 0.2867679344610364889, -1.271653543307086798 ) ) ;
#39716 = CARTESIAN_POINT ( 'NONE',  ( -1.194225721784776262, 0.05413385826771626580, -0.4176697321401330321 ) ) ;
#39717 = CARTESIAN_POINT ( 'NONE',  ( -0.1958661417322834497, -0.3392501089628018884, 0.01183033940388633805 ) ) ;
#39718 = CARTESIAN_POINT ( 'NONE',  ( 0.4724409448818904789, -0.1870078740157480879, -0.4822834645669291653 ) ) ;
#39719 = CARTESIAN_POINT ( 'NONE',  ( -0.6299212598425188991, -0.1870078740157479769, 0.3641732283464567677 ) ) ;
#39720 = CARTESIAN_POINT ( 'NONE',  ( 1.076115485564305141, -0.6046776061558807314, 0.2411417322834647770 ) ) ;
#39721 = CARTESIAN_POINT ( 'NONE',  ( 0.1837270341207354329, 0.2306618581243848609, 0.2411417322834645549 ) ) ;
#39722 = CARTESIAN_POINT ( 'NONE',  ( 0.4114485906785895208, 1.299212774617487076, 1.044049266805401999 ) ) ;
#39723 = CARTESIAN_POINT ( 'NONE',  ( -0.3996062992125986035, -0.1070741851644056997, -2.408136482939632561 ) ) ;
#39724 = CARTESIAN_POINT ( 'NONE',  ( -0.2867679344610367109, 0.2867679344610365444, -1.118785719981314264 ) ) ;
#39725 = CARTESIAN_POINT ( 'NONE',  ( 1.463254593175853824, -0.6692913385826771977, 0.1292274648535927661 ) ) ;
#39726 = CARTESIAN_POINT ( 'NONE',  ( 0.4593175853018379162, -0.4281496062992124485, 0.4176697321401328655 ) ) ;
#39727 = CARTESIAN_POINT ( 'NONE',  ( 0.1246719160104994284, -0.6692913385826771977, 0.1292274648535927661 ) ) ;
#39728 = CARTESIAN_POINT ( 'NONE',  ( 1.541994750656168645, -0.6692913385826771977, 0.1292274648535927661 ) ) ;
#39729 = CARTESIAN_POINT ( 'NONE',  ( 1.069553805774278832, 0.2952755905511810774, -0.1292274648535930714 ) ) ;
#39730 = CARTESIAN_POINT ( 'NONE',  ( 0.3917322834645670104, 2.398668435337828261E-17, -0.3602362204724410266 ) ) ;
#39731 = CARTESIAN_POINT ( 'NONE',  ( -0.1312335958005241554, 0.2306618581243848609, 0.2411417322834645549 ) ) ;
#39732 = CARTESIAN_POINT ( 'NONE',  ( 1.122047244094488860, -0.5400638737290845981, -0.3530559997133363437 ) ) ;
#39733 = CARTESIAN_POINT ( 'NONE',  ( 0.5380577427821529035, -0.4281496062992124485, 0.4176697321401328655 ) ) ;
#39734 = CARTESIAN_POINT ( 'NONE',  ( 1.167979002624672580, -0.3690944881889763329, 0.3153832671262228327 ) ) ;
#39735 = CARTESIAN_POINT ( 'NONE',  ( -1.115485564304461219, -0.4281496062992124485, 0.4176697321401328655 ) ) ;
#39736 = CARTESIAN_POINT ( 'NONE',  ( -1.450131233595799651, -0.6692913385826771977, 0.1292274648535927661 ) ) ;
#39737 = CARTESIAN_POINT ( 'NONE',  ( 0.8727034120734912248, -0.3162353388693409650, -0.4822834645669289433 ) ) ;
#39738 = CARTESIAN_POINT ( 'NONE',  ( -0.4724409448818898682, -8.678599364036362592E-17, -0.5885826771653542844 ) ) ;
#39739 = CARTESIAN_POINT ( 'NONE',  ( 4.797336870675656522E-17, -0.3917322834645670104, -2.118110236220472675 ) ) ;
#39740 = ORIENTED_EDGE ( 'NONE', *, *, #38741, .T. ) ;
#39741 = CARTESIAN_POINT ( 'NONE',  ( 0.3996062992125986590, -0.1070741851644053111, -0.2690288713910760632 ) ) ;
#39742 = VERTEX_POINT ( 'NONE', #26909 ) ;
#39743 = CARTESIAN_POINT ( 'NONE',  ( 1.443569553805774897, -0.6046776061558809534, -0.2411417322834644161 ) ) ;
#39744 = CARTESIAN_POINT ( 'NONE',  ( 0.7939632545931766261, -0.08942795157527998196, 0.3641732283464567121 ) ) ;
#39745 = CARTESIAN_POINT ( 'NONE',  ( 2.118110236220474007, 0.000000000000000000, -0.4498537592782824723 ) ) ;
#39746 = CARTESIAN_POINT ( 'NONE',  ( -0.1312335958005241554, 0.2306618581243848609, 0.2411417322834645549 ) ) ;
#39747 = DIRECTION ( 'NONE',  ( 0.000000000000000000, 0.000000000000000000, -1.000000000000000000 ) ) ;
#39748 = CARTESIAN_POINT ( 'NONE',  ( -0.1049643490035302024, -0.3917322834645671215, -0.7867454068241470644 ) ) ;
#39749 = CARTESIAN_POINT ( 'NONE',  ( 1.384514435695538337, -0.6692913385826771977, 0.1292274648535927661 ) ) ;
#39750 = CARTESIAN_POINT ( 'NONE',  ( 1.141392835773559211, 0.3937007874015748254, 1.141392835773562764 ) ) ;
#39751 = CARTESIAN_POINT ( 'NONE',  ( -0.1968503937007867743, -0.6692913385826771977, 8.415575281601705876E-17 ) ) ;
#39752 = CARTESIAN_POINT ( 'NONE',  ( 0.9973753280839902091, 0.2306618581243847221, -0.2411417322834647770 ) ) ;
#39753 = ORIENTED_EDGE ( 'NONE', *, *, #9731, .F. ) ;
#39754 = CARTESIAN_POINT ( 'NONE',  ( -1.541994750656167090, 0.2952755905511811885, 0.1292274648535926551 ) ) ;
#39755 = CARTESIAN_POINT ( 'NONE',  ( 0.000000000000000000, 0.4201155382560080032, -1.198416298106748767 ) ) ;
#39756 = CARTESIAN_POINT ( 'NONE',  ( 4.665011981514467720, 3.481290980825508807, 7.114705915355106214 ) ) ;
#39757 = CARTESIAN_POINT ( 'NONE',  ( -3.937007874015748143, 1.724409448818898127, -0.6299212598425202314 ) ) ;
#39758 = DIRECTION ( 'NONE',  ( 1.000000000000000000, -0.000000000000000000, -0.000000000000000000 ) ) ;
#39759 = CARTESIAN_POINT ( 'NONE',  ( -0.9383202099737524282, -0.2845877964562161244, -0.3641732283464567121 ) ) ;
#39760 = CARTESIAN_POINT ( 'NONE',  ( 0.9324623468618423727, 2.784432375088962958E-17, -0.3464511005275205946 ) ) ;
#39761 = CARTESIAN_POINT ( 'NONE',  ( 0.4199475065616805614, 0.2306618581243848609, 0.2411417322834645549 ) ) ;
#39762 = CIRCLE ( 'NONE', #26296, 0.1771653543307085410 ) ;
#39763 = EDGE_LOOP ( 'NONE', ( #19223, #15433, #83192, #9505 ) ) ;
#39765 = DIRECTION ( 'NONE',  ( 0.000000000000000000, -1.000000000000000000, 0.000000000000000000 ) ) ;
#39764 = CARTESIAN_POINT ( 'NONE',  ( -0.5314960629921194890, 2.716535433070866645, -1.854472803289054283 ) ) ;
#39766 = CARTESIAN_POINT ( 'NONE',  ( 0.7808398950131241190, -0.05778040916215560624, -0.4822834645669293319 ) ) ;
#39767 = CARTESIAN_POINT ( 'NONE',  ( -1.489501312335957062, -0.3162353388693409650, -0.4822834645669289433 ) ) ;
#39768 = CARTESIAN_POINT ( 'NONE',  ( -0.1049643490035301746, -0.3917322834645670659, -0.9396132301499194872 ) ) ;
#39769 = CARTESIAN_POINT ( 'NONE',  ( -0.8005249343832013809, -0.3690944881889763329, 0.3153832671262228327 ) ) ;
#39770 = CARTESIAN_POINT ( 'NONE',  ( -1.568241469816272105, -0.2845877964562161244, -0.3641732283464567121 ) ) ;
#39771 = CARTESIAN_POINT ( 'NONE',  ( -0.3392501089628017219, -0.1958661417322836718, -1.082020997375328086 ) ) ;
#39772 = CARTESIAN_POINT ( 'NONE',  ( 0.4002624671916016896, -0.3162353388693409650, -0.4822834645669289433 ) ) ;
#39773 = CARTESIAN_POINT ( 'NONE',  ( -0.7545931758530176614, -0.5511811023622048555, -0.09757992244046775898 ) ) ;
#39774 = CARTESIAN_POINT ( 'NONE',  ( 0.2952755905511816326, -0.4536011799217367080, 0.2665933059059888421 ) ) ;
#39775 = EDGE_CURVE ( 'NONE', #20676, #24808, #24114, .T. ) ;
#39776 = CARTESIAN_POINT ( 'NONE',  ( -0.1771653543307080136, -0.5400638737290844871, 0.3530559997133364547 ) ) ;
#39777 = CARTESIAN_POINT ( 'NONE',  ( -1.292650918635170010, 0.1771653543307087075, -0.09757992244046823083 ) ) ;
#39778 = CARTESIAN_POINT ( 'NONE',  ( -0.3392501089628017219, -0.1958661417322836995, -0.2067122291676659340 ) ) ;
#39779 = CARTESIAN_POINT ( 'NONE',  ( 0.9055118110236227702, -0.6692913385826771977, 8.415575281601705876E-17 ) ) ;
#39780 = EDGE_CURVE ( 'NONE', #14171, #17097, #51730, .T. ) ;
#39781 = CARTESIAN_POINT ( 'NONE',  ( -1.535433070866141225, -0.6692913385826771977, 8.415575281601705876E-17 ) ) ;
#39782 = CARTESIAN_POINT ( 'NONE',  ( 0.1265901696524989462, 0.4724409448818897572, -1.645013123359579943 ) ) ;
#39783 = CARTESIAN_POINT ( 'NONE',  ( -0.7217847769028863381, 0.05413385826771626580, -0.4176697321401330321 ) ) ;
#39784 = CARTESIAN_POINT ( 'NONE',  ( -0.2690288713910754526, 0.1771653543307087075, -0.09757992244046823083 ) ) ;
#39785 = CARTESIAN_POINT ( 'NONE',  ( -1.181102362204723644, -0.1870078740157479769, 0.4822834645669291653 ) ) ;
#39786 = CARTESIAN_POINT ( 'NONE',  ( 0.9842519685039378130, -0.5511811023622047445, 6.969142054262312111E-17 ) ) ;
#39787 = CARTESIAN_POINT ( 'NONE',  ( -0.4199475065616791736, 0.1283753931104746893, -0.1820866141732285504 ) ) ;
#39788 = CARTESIAN_POINT ( 'NONE',  ( -1.181102362204723644, -0.1870078740157480879, -0.4822834645669291653 ) ) ;
#39789 = CARTESIAN_POINT ( 'NONE',  ( -1.148293963254592542, -0.6692913385826773087, -0.1292274648535924053 ) ) ;
#39790 = CARTESIAN_POINT ( 'NONE',  ( 1.692913385826772421, 0.2952755905511811885, 0.000000000000000000 ) ) ;
#39791 = CARTESIAN_POINT ( 'NONE',  ( 1.403614904275686858E-14, 1.537401574803149984, -3.937007874015761910 ) ) ;
#39792 = CARTESIAN_POINT ( 'NONE',  ( 1.437007874015748810, -0.4536011799217368745, -0.2665933059059886201 ) ) ;
#39793 = CARTESIAN_POINT ( 'NONE',  ( 0.2165354330708668673, -0.5400638737290844871, 0.3530559997133364547 ) ) ;
#39794 = CARTESIAN_POINT ( 'NONE',  ( -1.561679790026246017, -0.4281496062992127816, -0.4176697321401328100 ) ) ;
#39795 = CARTESIAN_POINT ( 'NONE',  ( -1.469816272965878357, -0.6046776061558809534, -0.2411417322834644161 ) ) ;
#39796 = ORIENTED_EDGE ( 'NONE', *, *, #12583, .T. ) ;
#39797 = CARTESIAN_POINT ( 'NONE',  ( 4.893765752498283308E-17, -0.3996062992125985480, -2.517716535433071279 ) ) ;
#39798 = EDGE_CURVE ( 'NONE', #19015, #53614, #22199, .T. ) ;
#39799 = CARTESIAN_POINT ( 'NONE',  ( -0.7939632545931750718, -0.08942795157528024563, -0.3641732283464568787 ) ) ;
#39800 = CARTESIAN_POINT ( 'NONE',  ( 0.8858267716535438430, -0.5400638737290845981, -0.3530559997133363437 ) ) ;
#39801 = AXIS2_PLACEMENT_3D ( 'NONE', #70930, #45646, #19152 ) ;
#39802 = CARTESIAN_POINT ( 'NONE',  ( -1.253280839895012377, -0.08942795157527998196, 0.3641732283464567121 ) ) ;
#39803 = CARTESIAN_POINT ( 'NONE',  ( -9.787531504996566615E-17, 0.3996062992125985480, -1.966535433070866201 ) ) ;
#39804 = CARTESIAN_POINT ( 'NONE',  ( -1.568241469816272105, -0.05778040916215522460, 0.4822834645669289988 ) ) ;
#39805 = CIRCLE ( 'NONE', #50529, 1.220472440944881942 ) ;
#39806 = AXIS2_PLACEMENT_3D ( 'NONE', #65572, #8315, #47426 ) ;
#39807 = CARTESIAN_POINT ( 'NONE',  ( 0.8858267716535438430, 0.1660481256975885056, 0.3530559997133364547 ) ) ;
#39808 = CARTESIAN_POINT ( 'NONE',  ( 0.4461942257217856311, 0.2306618581243847221, -0.2411417322834647770 ) ) ;
#39809 = EDGE_CURVE ( 'NONE', #78537, #31856, #79176, .T. ) ;
#39810 = CARTESIAN_POINT ( 'NONE',  ( 1.069553805774278610, -0.6692913385826771977, 0.1292274648535927661 ) ) ;
#39811 = CARTESIAN_POINT ( 'NONE',  ( -0.3460692066303960313, 0.1998031496062989965, -1.205380577427821454 ) ) ;
#39812 = CARTESIAN_POINT ( 'NONE',  ( 0.2925321140481932369, -0.2925321140481932369, -1.515748031496062742 ) ) ;
#39813 = CARTESIAN_POINT ( 'NONE',  ( 0.2891555358219910499, -0.2891555358219909944, -0.5708661417322835607 ) ) ;
#39814 = CARTESIAN_POINT ( 'NONE',  ( 0.4744094488188886904, 1.537401574803149984, 2.554262525012303886 ) ) ;
#39815 = CARTESIAN_POINT ( 'NONE',  ( 0.9055118110236227702, 0.1771653543307087630, 0.000000000000000000 ) ) ;
#39816 = CARTESIAN_POINT ( 'NONE',  ( 0.1968503937007881344, 0.1771653543307087630, 0.000000000000000000 ) ) ;
#39817 = CARTESIAN_POINT ( 'NONE',  ( 5.463695987328526437E-16, -0.1870078740157479769, 0.4822834645669291653 ) ) ;
#39818 = CARTESIAN_POINT ( 'NONE',  ( 1.095800524934383846, -0.3162353388693405765, 0.4822834645669290543 ) ) ;
#39819 = CARTESIAN_POINT ( 'NONE',  ( 0.3949938075777409963, 2.418639510665530743E-17, -1.612204724409448842 ) ) ;
#39820 = CARTESIAN_POINT ( 'NONE',  ( 0.4068241469816281097, -0.004921259842519576551, 0.3153832671262227771 ) ) ;
#39821 =( BOUNDED_SURFACE ( )  B_SPLINE_SURFACE ( 1, 2, ( 
 ( #40515, #32946, #26635, #26207, #58612, #66195, #52289, #33373, #129, #51445, #1391, #52705, #70838, #79666, #28292, #53953, #41742, #22811, #72917, #74169, #54373, #54792, #35441, #15268, #34621, #21983, #80495, #73340, #47227, #22403, #10193, #15688, #60694, #9359, #61107, #16516, #3873, #34200, #42160, #48060, #66609, #80083, #73762, #41346, #67027, #35862, #29532, #55195, #42571, #28709, #2216, #35030, #47645, #48468, #16097, #3459, #59863, #40929, #3044, #67855, #61527, #80902, #53542, #67436, #9770, #29124, #23216, #21565, #48886, #74587, #16931, #2635, #8532, #27882, #79250, #8945, #60285, #4277, #56432, #36667, #76228, #36265, #75403, #24448, #29938, #37905, #49298, #25267, #11008, #5104, #17345, #18562, #57245, #50933, #43378, #12249, #31590, #17749, #44205, #50116, #69078, #74999, #63582, #5916, #11429, #82134, #55602, #37084, #68273, #62770, #30771, #75813, #24854, #18156, #76631, #61934, #81314, #18962, #43788, #23627, #69494, #62342, #82949, #42973, #11843, #69895, #4681, #37496, #63171, #5509, #31172, #10608, #68669, #56838, #30352, #56021, #82536, #81729, #50522, #24038, #49708, #77468, #19379, #44610, #26104, #26944, #64414, #51343, #39576, #40004, #1294, #77891, #26534, #78733, #58936, #70730, #25683, #71991, #52605, #45031, #78312, #19805, #32008, #59345, #58083, #20643, #14344, #45871, #30, #70306, #46296, #58512, #51766, #32843, #39149, #65266, #27359, #875, #6749, #13084, #65692, #52187, #7602, #38737, #63994, #8020, #20222, #32421, #6335, #57668, #33683, #1702, #33276, #45454, #77047, #53018, #12659, #38320, #7172, #449, #71152, #13493, #71569, #64834, #13920, #67341, #34935, #80398, #79565, #15585, #79153, #21880, #10090, #2115, #28194, #29021, #3356, #47958, #21469, #60598, #8842, #40823, #66508, #54269, #35345, #27781, #54687, #66931, #9674, #73662, #53444, #47127, #34518, #61007, #2536, #59760, #2947, #22711, #53852, #73234, #47544, #16003, #48369, #16414, #46716, #74068, #28612, #72817, #9264, #79984, #41244, #22297, #42061, #67756, #35755, #55094, #41650, #14757, #61421, #60184, #3771, #29435, #21056, #72408, #40412, #66093, #8429, #34097, #15167, #10911, #68167, #5007, #61837, #63077, #30677, #55505, #43692, #18469, #31076, #80802, #36163, #82037, #55919, #36569, #36988, #69804, #56744, #31491, #42467, #16831, #17649, #42876, #69397, #18059, #81213, #68569, #17247, #56338, #30255, #81632, #76127, #48787, #75305, #24351, #74484, #50020, #75719, #43281, #23943, #4178, #49610, #37405, #11328, #82442, #62247, #68980, #62667, #11749, #5415, #44112, #23119, #24759, #50427, #23528, #12152, #37808, #63486, #5820, #10510, #29841, #49198, #74899, #4584, #50841, #351, #44930, #45773, #77369, #26433, #19701, #14244, #57152, #20546, #46198, #39902, #70627, #44518, #64737, #38221, #39479, #7075, #31910, #20126, #78214, #7502, #82851, #12563, #58412, #32324, #12983, #13399, #71893, #33171, #7923, #18869, #76541, #45358, #19279, #71472, #77793, #57571, #38639, #76951, #32745, #6651, #57986, #52505, #25172, #51665, #771, #70206, #52084, #13820, #71055, #26008, #63896, #39052, #65166, #6234, #58839, #1197, #51249, #83263, #25585, #65590, #26846, #64317, #8747, #72313, #4384, #33584, #27262, #79464, #20960, #29642, #14660, #15487, #2018, #49412, #81011, #47443, #10716, #34418, #28098, #8334, #60086, #23739, #40317, #40724, #42679, #17039, #61637, #34000, #73137, #21374, #53347, #79057, #67959, #48995, #65996, #68377, #21781, #23325, #3978, #59662, #27682, #47029, #74694, #15068, #72721, #36373, #62047, #35967, #66410, #68779, #30052, #41144, #2440, #10301, #53754, #55303, #17452, #55714, #81424, #75105, #43082, #59247, #1606, #52922, #78636, #46618, #56543, #76744, #19074, #57778, #56133, #82244, #69604, #76339, #50634, #24149, #82648, #75925, #12359, #5212, #51457, #70420, #64115, #4792, #24963, #30469, #18669, #62877, #44722, #62456, #18265, #44314, #81838, #6450, #75519, #77160, #37196, #31286, #43493, #12775, #141, #19492, #11950, #38432, #25797, #43906, #32120, #70004, #37605, #17858, #45146, #11123, #63279, #38017, #49819, #5620 ),
 ( #30876, #36780, #57362, #63693, #69189, #56951, #6032, #11540, #31704, #24563, #50229, #83058, #25380, #51043, #14457, #45569, #27057, #58623, #7286, #32956, #20755, #1811, #51881, #53131, #33384, #33795, #40109, #77586, #13610, #990, #59460, #52299, #26218, #1401, #72515, #78005, #39689, #71681, #65796, #78842, #66205, #13200, #20333, #65381, #14033, #8130, #21168, #8544, #38847, #46824, #52716, #71263, #59047, #78427, #45985, #7716, #14864, #34210, #59873, #21575, #46405, #64527, #72099, #26645, #27473, #40526, #2227, #27892, #53552, #70849, #79260, #6864, #32533, #58197, #565, #19920, #39264, #64946, #54800, #21992, #10201, #68281, #80911, #47237, #2644, #48477, #22412, #3052, #3467, #36273, #23224, #81322, #8956, #66618, #67445, #9367, #35870, #67864, #47653, #35038, #67035, #80503, #80091, #48068, #42580, #15278, #41750, #22819, #40939, #16524, #74178, #9778, #73771, #28301, #16105, #3881, #34630, #48894, #29133, #41354, #60294, #53963, #61944, #61536, #29540, #35450, #79675, #16939, #72926, #73349, #61115, #15697, #42169, #60703, #55203, #28718, #4285, #74596, #10616, #29947, #55611, #54381, #81738, #82143, #12670, #4689, #30779, #31598, #5926, #50532, #24047, #63179, #11437, #43388, #69089, #56847, #37914, #30363, #57257, #69502, #69903, #76236, #56030, #49718, #37093, #12257, #5112, #62351, #37504, #25275, #18570, #82545, #11851, #24458, #75414, #50124, #63591, #42982, #50943, #5517, #17758, #68677, #11018, #38330, #82957, #76640, #75823, #62778, #18971, #23636, #17354, #31182, #36675, #44213, #56440, #24863, #18165, #64005, #44620, #70315, #6345, #43798, #32017, #57677, #49306, #75007, #64424, #7181, #8030, #65700, #26953, #58093, #39586, #71162, #19815, #45464, #33285, #14356, #6758, #33693, #45880, #46306, #52616, #32430, #26114, #13502, #72000, #64843, #38747, #13929, #1713, #32852, #52197, #887, #78322, #59354, #78742, #25692, #27368, #65275, #458, #71578, #7614, #58521, #26544, #53029, #21067, #46725, #34109, #20232, #77056, #77901, #39158, #40013, #58946, #20653, #1304, #40422, #39, #72417, #14766, #66103, #8439, #70742, #51353, #51775, #19389, #45041, #77480, #13094, #80813, #10101, #59770, #15177, #61016, #34944, #15595, #16013, #48796, #35765, #10519, #21478, #79161, #79995, #21890, #48379, #80408, #34530, #47554, #79574, #9683, #9273, #60607, #55104, #27793, #54279, #35354, #53453, #3782, #3367, #40834, #2125, #61435, #73671, #66941, #47972, #22309, #22720, #42475, #41659, #73246, #2545, #29445, #67350, #54702, #60194, #47136, #66519, #41255, #42070, #67765, #23128, #72827, #2956, #28621, #29031, #74078, #8851, #16424, #74494, #16841, #53862, #68180, #28203, #5828, #29850, #24361, #55513, #50031, #4592, #44121, #4187, #43291, #75728, #81221, #31501, #17256, #76549, #62256, #56347, #68579, #69813, #25182, #18877, #11337, #63494, #82860, #68988, #12162, #18068, #36997, #42884, #57161, #50849, #62676, #43703, #23537, #5018, #36173, #30686, #82048, #69406, #76138, #11760, #44526, #49206, #74910, #70214, #37414, #10920, #63086, #30263, #61846, #36577, #5424, #37818, #55927, #31086, #56753, #82453, #24768, #81643, #23951, #50437, #49619, #75313, #18479, #17660, #64744, #7082, #77802, #45367, #70635, #12570, #77377, #78222, #32332, #19286, #7511, #7931, #52514, #45782, #20134, #46625, #26855, #38647, #76958, #39911, #20555, #12991, #46207, #71062, #83270, #27270, #26015, #71901, #58848, #33592, #14253, #38228, #51256, #13828, #13406, #51673, #52094, #1614, #65599, #63905, #57579, #31918, #32753, #57994, #1205, #33179, #64324, #358, #19708, #71481, #39061, #58420, #59257, #6241, #780, #39487, #25593, #65174, #52931, #26441, #78643, #44937, #20966, #6660, #8342, #35252, #66840, #72729, #34008, #59670, #80306, #73569, #22208, #28107, #2025, #60916, #72321, #27691, #15494, #53354, #79890, #79065, #9174, #15075, #48280, #47865, #41152, #3267, #53761, #47450, #21381, #79472, #22621, #47035, #2449, #67251, #9583, #54176, #40733, #34845, #8753, #66417, #34429, #60508, #15914, #60094, #28928, #2856, #41562, #28520, #21788, #73145, #54597 ) ),
 .UNSPECIFIED., .F., .F., .F. ) 
 B_SPLINE_SURFACE_WITH_KNOTS ( ( 2, 2 ),
 ( 3, 2, 2, 2, 2, 2, 2, 2, 2, 2, 2, 2, 2, 2, 2, 2, 2, 2, 2, 2, 2, 2, 2, 2, 2, 2, 2, 2, 2, 2, 2, 2, 2, 2, 2, 2, 2, 2, 2, 2, 2, 2, 2, 2, 2, 2, 2, 2, 2, 2, 2, 2, 2, 2, 2, 2, 2, 2, 2, 2, 2, 2, 2, 2, 2, 2, 2, 2, 2, 2, 2, 2, 2, 2, 2, 2, 2, 2, 2, 2, 2, 2, 2, 2, 2, 2, 2, 2, 2, 2, 2, 2, 2, 2, 2, 2, 2, 2, 2, 2, 2, 2, 2, 2, 2, 2, 2, 2, 2, 2, 2, 2, 2, 2, 2, 2, 2, 2, 2, 2, 2, 2, 2, 2, 2, 2, 2, 2, 2, 2, 2, 2, 2, 2, 2, 2, 2, 2, 2, 2, 2, 2, 2, 2, 2, 2, 2, 2, 2, 2, 2, 2, 2, 2, 2, 2, 2, 2, 2, 2, 2, 2, 2, 2, 2, 2, 2, 2, 2, 2, 2, 2, 2, 2, 2, 2, 2, 2, 2, 2, 2, 2, 2, 2, 2, 2, 2, 2, 2, 2, 2, 2, 2, 2, 2, 2, 2, 2, 2, 2, 2, 2, 2, 2, 2, 2, 2, 2, 2, 2, 2, 2, 2, 2, 2, 2, 2, 2, 2, 2, 2, 2, 2, 2, 2, 2, 2, 2, 2, 2, 2, 2, 2, 2, 2, 2, 2, 2, 2, 2, 2, 2, 2, 2, 2, 2, 2, 2, 2, 2, 2, 2, 2, 2, 2, 3 ),
 ( 0.000000000000000000, 1.000000000000000000 ),
 ( 0.000000000000000000, 0.003787878787878787984, 0.007575757575757575968, 0.01136363636363636395, 0.01515151515151515194, 0.01893939393939393992, 0.02272727272727272790, 0.02651515151515151589, 0.03030303030303030387, 0.03409090909090908839, 0.03787878787878787984, 0.04166666666666666435, 0.04545454545454545581, 0.04924242424242424032, 0.05303030303030303177, 0.05681818181818181629, 0.06060606060606060774, 0.06439393939393939226, 0.06818181818181817677, 0.07196969696969697516, 0.07575757575757575968, 0.07954545454545454419, 0.08333333333333332871, 0.08712121212121212710, 0.09090909090909091161, 0.09469696969696969613, 0.09848484848484848064, 0.1022727272727272790, 0.1060606060606060635, 0.1098484848484848481, 0.1136363636363636326, 0.1174242424242424310, 0.1212121212121212155, 0.1250000000000000000, 0.1287878787878787845, 0.1325757575757575690, 0.1363636363636363535, 0.1401515151515151381, 0.1439393939393939503, 0.1477272727272727348, 0.1515151515151515194, 0.1553030303030303039, 0.1590909090909090884, 0.1628787878787878729, 0.1666666666666666574, 0.1704545454545454419, 0.1742424242424242542, 0.1780303030303030387, 0.1818181818181818232, 0.1856060606060606077, 0.1893939393939393923, 0.1931818181818181768, 0.1969696969696969613, 0.2007575757575757458, 0.2045454545454545581, 0.2083333333333333426, 0.2121212121212121271, 0.2159090909090909116, 0.2196969696969696961, 0.2234848484848484806, 0.2272727272727272652, 0.2310606060606060497, 0.2348484848484848619, 0.2386363636363636465, 0.2424242424242424310, 0.2462121212121212155, 0.2500000000000000000, 0.2537878787878787845, 0.2575757575757575690, 0.2613636363636363535, 0.2651515151515151381, 0.2689393939393939226, 0.2727272727272727071, 0.2765151515151514916, 0.2803030303030302761, 0.2840909090909091161, 0.2878787878787879007, 0.2916666666666666852, 0.2954545454545454697, 0.2992424242424242542, 0.3030303030303030387, 0.3068181818181818232, 0.3106060606060606077, 0.3143939393939393923, 0.3181818181818181768, 0.3219696969696969613, 0.3257575757575757458, 0.3295454545454545303, 0.3333333333333333148, 0.3371212121212120993, 0.3409090909090908839, 0.3446969696969697239, 0.3484848484848485084, 0.3522727272727272929, 0.3560606060606060774, 0.3598484848484848619, 0.3636363636363636465, 0.3674242424242424310, 0.3712121212121212155, 0.3750000000000000000, 0.3787878787878787845, 0.3825757575757575690, 0.3863636363636363535, 0.3901515151515151381, 0.3939393939393939226, 0.3977272727272727071, 0.4015151515151514916, 0.4053030303030302761, 0.4090909090909091161, 0.4128787878787879007, 0.4166666666666666852, 0.4204545454545454697, 0.4242424242424242542, 0.4280303030303030387, 0.4318181818181818232, 0.4356060606060606077, 0.4393939393939393923, 0.4431818181818181768, 0.4469696969696969613, 0.4507575757575757458, 0.4545454545454545303, 0.4583333333333333148, 0.4621212121212120993, 0.4659090909090908839, 0.4696969696969697239, 0.4734848484848485084, 0.4772727272727272929, 0.4810606060606060774, 0.4848484848484848619, 0.4886363636363636465, 0.4924242424242424310, 0.4962121212121212155, 0.5000000000000000000, 0.5037878787878787845, 0.5075757575757575690, 0.5113636363636363535, 0.5151515151515151381, 0.5189393939393939226, 0.5227272727272727071, 0.5265151515151514916, 0.5303030303030302761, 0.5340909090909090606, 0.5378787878787878451, 0.5416666666666666297, 0.5454545454545454142, 0.5492424242424241987, 0.5530303030303029832, 0.5568181818181817677, 0.5606060606060605522, 0.5643939393939394478, 0.5681818181818182323, 0.5719696969696970168, 0.5757575757575758013, 0.5795454545454545858, 0.5833333333333333703, 0.5871212121212121549, 0.5909090909090909394, 0.5946969696969697239, 0.5984848484848485084, 0.6022727272727272929, 0.6060606060606060774, 0.6098484848484848619, 0.6136363636363636465, 0.6174242424242424310, 0.6212121212121212155, 0.6250000000000000000, 0.6287878787878787845, 0.6325757575757575690, 0.6363636363636363535, 0.6401515151515151381, 0.6439393939393939226, 0.6477272727272727071, 0.6515151515151514916, 0.6553030303030302761, 0.6590909090909090606, 0.6628787878787878451, 0.6666666666666666297, 0.6704545454545454142, 0.6742424242424241987, 0.6780303030303029832, 0.6818181818181817677, 0.6856060606060605522, 0.6893939393939394478, 0.6931818181818182323, 0.6969696969696970168, 0.7007575757575758013, 0.7045454545454545858, 0.7083333333333333703, 0.7121212121212121549, 0.7159090909090909394, 0.7196969696969697239, 0.7234848484848485084, 0.7272727272727272929, 0.7310606060606060774, 0.7348484848484848619, 0.7386363636363636465, 0.7424242424242424310, 0.7462121212121212155, 0.7500000000000000000, 0.7537878787878787845, 0.7575757575757575690, 0.7613636363636363535, 0.7651515151515151381, 0.7689393939393939226, 0.7727272727272727071, 0.7765151515151514916, 0.7803030303030302761, 0.7840909090909090606, 0.7878787878787878451, 0.7916666666666666297, 0.7954545454545454142, 0.7992424242424241987, 0.8030303030303029832, 0.8068181818181817677, 0.8106060606060605522, 0.8143939393939394478, 0.8181818181818182323, 0.8219696969696970168, 0.8257575757575758013, 0.8295454545454545858, 0.8333333333333333703, 0.8371212121212121549, 0.8409090909090909394, 0.8446969696969697239, 0.8484848484848485084, 0.8522727272727272929, 0.8560606060606060774, 0.8598484848484848619, 0.8636363636363636465, 0.8674242424242424310, 0.8712121212121212155, 0.8750000000000000000, 0.8787878787878787845, 0.8825757575757575690, 0.8863636363636363535, 0.8901515151515151381, 0.8939393939393939226, 0.8977272727272727071, 0.9015151515151514916, 0.9053030303030302761, 0.9090909090909090606, 0.9128787878787878451, 0.9166666666666666297, 0.9204545454545454142, 0.9242424242424241987, 0.9280303030303029832, 0.9318181818181817677, 0.9356060606060605522, 0.9393939393939394478, 0.9431818181818182323, 0.9469696969696970168, 0.9507575757575758013, 0.9545454545454545858, 0.9583333333333333703, 0.9621212121212121549, 0.9659090909090909394 ),
 .UNSPECIFIED. ) 
 GEOMETRIC_REPRESENTATION_ITEM ( )  RATIONAL_B_SPLINE_SURFACE ( (
 ( 1.000000000000000000, 0.9659258262890683122, 1.000000000000000000, 0.9659258262890683122, 1.000000000000000000, 0.9659258262890683122, 1.000000000000000000, 0.9659258262890683122, 1.000000000000000000, 0.9659258262890683122, 1.000000000000000000, 0.9659258262890683122, 1.000000000000000000, 0.9659258262890683122, 1.000000000000000000, 0.9659258262890683122, 1.000000000000000000, 0.9659258262890683122, 1.000000000000000000, 0.9659258262890683122, 1.000000000000000000, 0.9659258262890683122, 1.000000000000000000, 0.9659258262890683122, 1.000000000000000000, 0.9659258262890683122, 1.000000000000000000, 0.9659258262890683122, 1.000000000000000000, 0.9659258262890683122, 1.000000000000000000, 0.9659258262890683122, 1.000000000000000000, 0.9659258262890683122, 1.000000000000000000, 0.9659258262890683122, 1.000000000000000000, 0.9659258262890683122, 1.000000000000000000, 0.9659258262890683122, 1.000000000000000000, 0.9659258262890683122, 1.000000000000000000, 0.9659258262890683122, 1.000000000000000000, 0.9659258262890683122, 1.000000000000000000, 0.9659258262890683122, 1.000000000000000000, 0.9659258262890683122, 1.000000000000000000, 0.9659258262890683122, 1.000000000000000000, 0.9659258262890683122, 1.000000000000000000, 0.9659258262890683122, 1.000000000000000000, 0.9659258262890683122, 1.000000000000000000, 0.9659258262890683122, 1.000000000000000000, 0.9659258262890683122, 1.000000000000000000, 0.9659258262890683122, 1.000000000000000000, 0.9659258262890683122, 1.000000000000000000, 0.9659258262890683122, 1.000000000000000000, 0.9659258262890683122, 1.000000000000000000, 0.9659258262890683122, 1.000000000000000000, 0.9659258262890683122, 1.000000000000000000, 0.9659258262890683122, 1.000000000000000000, 0.9659258262890683122, 1.000000000000000000, 0.9659258262890683122, 1.000000000000000000, 0.9659258262890683122, 1.000000000000000000, 0.9659258262890683122, 1.000000000000000000, 0.9659258262890683122, 1.000000000000000000, 0.9659258262890683122, 1.000000000000000000, 0.9659258262890683122, 1.000000000000000000, 0.9659258262890683122, 1.000000000000000000, 0.9659258262890683122, 1.000000000000000000, 0.9659258262890683122, 1.000000000000000000, 0.9659258262890683122, 1.000000000000000000, 0.9659258262890683122, 1.000000000000000000, 0.9659258262890683122, 1.000000000000000000, 0.9659258262890683122, 1.000000000000000000, 0.9659258262890683122, 1.000000000000000000, 0.9659258262890683122, 1.000000000000000000, 0.9659258262890683122, 1.000000000000000000, 0.9659258262890683122, 1.000000000000000000, 0.9659258262890683122, 1.000000000000000000, 0.9659258262890683122, 1.000000000000000000, 0.9659258262890683122, 1.000000000000000000, 0.9659258262890683122, 1.000000000000000000, 0.9659258262890683122, 1.000000000000000000, 0.9659258262890683122, 1.000000000000000000, 0.9659258262890683122, 1.000000000000000000, 0.9659258262890683122, 1.000000000000000000, 0.9659258262890683122, 1.000000000000000000, 0.9659258262890683122, 1.000000000000000000, 0.9659258262890683122, 1.000000000000000000, 0.9659258262890683122, 1.000000000000000000, 0.9659258262890683122, 1.000000000000000000, 0.9659258262890683122, 1.000000000000000000, 0.9659258262890683122, 1.000000000000000000, 0.9659258262890683122, 1.000000000000000000, 0.9659258262890683122, 1.000000000000000000, 0.9659258262890683122, 1.000000000000000000, 0.9659258262890683122, 1.000000000000000000, 0.9659258262890683122, 1.000000000000000000, 0.9659258262890683122, 1.000000000000000000, 0.9659258262890683122, 1.000000000000000000, 0.9659258262890683122, 1.000000000000000000, 0.9659258262890683122, 1.000000000000000000, 0.9659258262890683122, 1.000000000000000000, 0.9659258262890683122, 1.000000000000000000, 0.9659258262890683122, 1.000000000000000000, 0.9659258262890683122, 1.000000000000000000, 0.9659258262890683122, 1.000000000000000000, 0.9659258262890683122, 1.000000000000000000, 0.9659258262890683122, 1.000000000000000000, 0.9659258262890683122, 1.000000000000000000, 0.9659258262890683122, 1.000000000000000000, 0.9659258262890683122, 1.000000000000000000, 0.9659258262890683122, 1.000000000000000000, 0.9659258262890683122, 1.000000000000000000, 0.9659258262890683122, 1.000000000000000000, 0.9659258262890683122, 1.000000000000000000, 0.9659258262890683122, 1.000000000000000000, 0.9659258262890683122, 1.000000000000000000, 0.9659258262890683122, 1.000000000000000000, 0.9659258262890683122, 1.000000000000000000, 0.9659258262890683122, 1.000000000000000000, 0.9659258262890683122, 1.000000000000000000, 0.9659258262890683122, 1.000000000000000000, 0.9659258262890683122, 1.000000000000000000, 0.9659258262890683122, 1.000000000000000000, 0.9659258262890683122, 1.000000000000000000, 0.9659258262890683122, 1.000000000000000000, 0.9659258262890683122, 1.000000000000000000, 0.9659258262890683122, 1.000000000000000000, 0.9659258262890683122, 1.000000000000000000, 0.9659258262890683122, 1.000000000000000000, 0.9659258262890683122, 1.000000000000000000, 0.9659258262890683122, 1.000000000000000000, 0.9659258262890683122, 1.000000000000000000, 0.9659258262890683122, 1.000000000000000000, 0.9659258262890683122, 1.000000000000000000, 0.9659258262890683122, 1.000000000000000000, 0.9659258262890683122, 1.000000000000000000, 0.9659258262890683122, 1.000000000000000000, 0.9659258262890683122, 1.000000000000000000, 0.9659258262890683122, 1.000000000000000000, 0.9659258262890683122, 1.000000000000000000, 0.9659258262890683122, 1.000000000000000000, 0.9659258262890683122, 1.000000000000000000, 0.9659258262890683122, 1.000000000000000000, 0.9659258262890683122, 1.000000000000000000, 0.9659258262890683122, 1.000000000000000000, 0.9659258262890683122, 1.000000000000000000, 0.9659258262890683122, 1.000000000000000000, 0.9659258262890683122, 1.000000000000000000, 0.9659258262890683122, 1.000000000000000000, 0.9659258262890683122, 1.000000000000000000, 0.9659258262890683122, 1.000000000000000000, 0.9659258262890683122, 1.000000000000000000, 0.9659258262890683122, 1.000000000000000000, 0.9659258262890683122, 1.000000000000000000, 0.9659258262890683122, 1.000000000000000000, 0.9659258262890683122, 1.000000000000000000, 0.9659258262890683122, 1.000000000000000000, 0.9659258262890683122, 1.000000000000000000, 0.9659258262890683122, 1.000000000000000000, 0.9659258262890683122, 1.000000000000000000, 0.9659258262890683122, 1.000000000000000000, 0.9659258262890683122, 1.000000000000000000, 0.9659258262890683122, 1.000000000000000000, 0.9659258262890683122, 1.000000000000000000, 0.9659258262890683122, 1.000000000000000000, 0.9659258262890683122, 1.000000000000000000, 0.9659258262890683122, 1.000000000000000000, 0.9659258262890683122, 1.000000000000000000, 0.9659258262890683122, 1.000000000000000000, 0.9659258262890683122, 1.000000000000000000, 0.9659258262890683122, 1.000000000000000000, 0.9659258262890683122, 1.000000000000000000, 0.9659258262890683122, 1.000000000000000000, 0.9659258262890683122, 1.000000000000000000, 0.9659258262890683122, 1.000000000000000000, 0.9659258262890683122, 1.000000000000000000, 0.9659258262890683122, 1.000000000000000000, 0.9659258262890683122, 1.000000000000000000, 0.9659258262890683122, 1.000000000000000000, 0.9659258262890683122, 1.000000000000000000, 0.9659258262890683122, 1.000000000000000000, 0.9659258262890683122, 1.000000000000000000, 0.9659258262890683122, 1.000000000000000000, 0.9659258262890683122, 1.000000000000000000, 0.9659258262890683122, 1.000000000000000000, 0.9659258262890683122, 1.000000000000000000, 0.9659258262890683122, 1.000000000000000000, 0.9659258262890683122, 1.000000000000000000, 0.9659258262890683122, 1.000000000000000000, 0.9659258262890683122, 1.000000000000000000, 0.9659258262890683122, 1.000000000000000000, 0.9659258262890683122, 1.000000000000000000, 0.9659258262890683122, 1.000000000000000000, 0.9659258262890683122, 1.000000000000000000, 0.9659258262890683122, 1.000000000000000000, 0.9659258262890683122, 1.000000000000000000, 0.9659258262890683122, 1.000000000000000000, 0.9659258262890683122, 1.000000000000000000, 0.9659258262890683122, 1.000000000000000000, 0.9659258262890683122, 1.000000000000000000, 0.9659258262890683122, 1.000000000000000000, 0.9659258262890683122, 1.000000000000000000, 0.9659258262890683122, 1.000000000000000000, 0.9659258262890683122, 1.000000000000000000, 0.9659258262890683122, 1.000000000000000000, 0.9659258262890683122, 1.000000000000000000, 0.9659258262890683122, 1.000000000000000000, 0.9659258262890683122, 1.000000000000000000, 0.9659258262890683122, 1.000000000000000000, 0.9659258262890683122, 1.000000000000000000, 0.9659258262890683122, 1.000000000000000000, 0.9659258262890683122, 1.000000000000000000, 0.9659258262890683122, 1.000000000000000000, 0.9659258262890683122, 1.000000000000000000, 0.9659258262890683122, 1.000000000000000000, 0.9659258262890683122, 1.000000000000000000, 0.9659258262890683122, 1.000000000000000000, 0.9659258262890683122, 1.000000000000000000, 0.9659258262890683122, 1.000000000000000000, 0.9659258262890683122, 1.000000000000000000, 0.9659258262890683122, 1.000000000000000000, 0.9659258262890683122, 1.000000000000000000, 0.9659258262890683122, 1.000000000000000000, 0.9659258262890683122, 1.000000000000000000, 0.9659258262890683122, 1.000000000000000000, 0.9659258262890683122, 1.000000000000000000, 0.9659258262890683122, 1.000000000000000000, 0.9659258262890683122, 1.000000000000000000, 0.9659258262890683122, 1.000000000000000000, 0.9659258262890683122, 1.000000000000000000, 0.9659258262890683122, 1.000000000000000000, 0.9659258262890683122, 1.000000000000000000, 0.9659258262890683122, 1.000000000000000000, 0.9659258262890683122, 1.000000000000000000, 0.9659258262890683122, 1.000000000000000000, 0.9659258262890683122, 1.000000000000000000, 0.9659258262890683122, 1.000000000000000000, 0.9659258262890683122, 1.000000000000000000, 0.9659258262890683122, 1.000000000000000000, 0.9659258262890683122, 1.000000000000000000, 0.9659258262890683122, 1.000000000000000000, 0.9659258262890683122, 1.000000000000000000, 0.9659258262890683122, 1.000000000000000000, 0.9659258262890683122, 1.000000000000000000, 0.9659258262890683122, 1.000000000000000000, 0.9659258262890683122, 1.000000000000000000, 0.9659258262890683122, 1.000000000000000000, 0.9659258262890683122, 1.000000000000000000, 0.9659258262890683122, 1.000000000000000000, 0.9659258262890683122, 1.000000000000000000, 0.9659258262890683122, 1.000000000000000000, 0.9659258262890683122, 1.000000000000000000, 0.9659258262890683122, 1.000000000000000000, 0.9659258262890683122, 1.000000000000000000, 0.9659258262890683122, 1.000000000000000000, 0.9659258262890683122, 1.000000000000000000, 0.9659258262890683122, 1.000000000000000000, 0.9659258262890683122, 1.000000000000000000, 0.9659258262890683122, 1.000000000000000000, 0.9659258262890683122, 1.000000000000000000, 0.9659258262890683122, 1.000000000000000000, 0.9659258262890683122, 1.000000000000000000, 0.9659258262890683122, 1.000000000000000000, 0.9659258262890683122, 1.000000000000000000, 0.9659258262890683122, 1.000000000000000000, 0.9659258262890683122, 1.000000000000000000, 0.9659258262890683122, 1.000000000000000000, 0.9659258262890683122, 1.000000000000000000, 0.9659258262890683122, 1.000000000000000000, 0.9659258262890683122, 1.000000000000000000, 0.9659258262890683122, 1.000000000000000000, 0.9659258262890683122, 1.000000000000000000, 0.9659258262890683122, 1.000000000000000000, 0.9659258262890683122, 1.000000000000000000, 0.9659258262890683122, 1.000000000000000000),
 ( 1.000000000000000000, 0.9659258262890683122, 1.000000000000000000, 0.9659258262890683122, 1.000000000000000000, 0.9659258262890683122, 1.000000000000000000, 0.9659258262890683122, 1.000000000000000000, 0.9659258262890683122, 1.000000000000000000, 0.9659258262890683122, 1.000000000000000000, 0.9659258262890683122, 1.000000000000000000, 0.9659258262890683122, 1.000000000000000000, 0.9659258262890683122, 1.000000000000000000, 0.9659258262890683122, 1.000000000000000000, 0.9659258262890683122, 1.000000000000000000, 0.9659258262890683122, 1.000000000000000000, 0.9659258262890683122, 1.000000000000000000, 0.9659258262890683122, 1.000000000000000000, 0.9659258262890683122, 1.000000000000000000, 0.9659258262890683122, 1.000000000000000000, 0.9659258262890683122, 1.000000000000000000, 0.9659258262890683122, 1.000000000000000000, 0.9659258262890683122, 1.000000000000000000, 0.9659258262890683122, 1.000000000000000000, 0.9659258262890683122, 1.000000000000000000, 0.9659258262890683122, 1.000000000000000000, 0.9659258262890683122, 1.000000000000000000, 0.9659258262890683122, 1.000000000000000000, 0.9659258262890683122, 1.000000000000000000, 0.9659258262890683122, 1.000000000000000000, 0.9659258262890683122, 1.000000000000000000, 0.9659258262890683122, 1.000000000000000000, 0.9659258262890683122, 1.000000000000000000, 0.9659258262890683122, 1.000000000000000000, 0.9659258262890683122, 1.000000000000000000, 0.9659258262890683122, 1.000000000000000000, 0.9659258262890683122, 1.000000000000000000, 0.9659258262890683122, 1.000000000000000000, 0.9659258262890683122, 1.000000000000000000, 0.9659258262890683122, 1.000000000000000000, 0.9659258262890683122, 1.000000000000000000, 0.9659258262890683122, 1.000000000000000000, 0.9659258262890683122, 1.000000000000000000, 0.9659258262890683122, 1.000000000000000000, 0.9659258262890683122, 1.000000000000000000, 0.9659258262890683122, 1.000000000000000000, 0.9659258262890683122, 1.000000000000000000, 0.9659258262890683122, 1.000000000000000000, 0.9659258262890683122, 1.000000000000000000, 0.9659258262890683122, 1.000000000000000000, 0.9659258262890683122, 1.000000000000000000, 0.9659258262890683122, 1.000000000000000000, 0.9659258262890683122, 1.000000000000000000, 0.9659258262890683122, 1.000000000000000000, 0.9659258262890683122, 1.000000000000000000, 0.9659258262890683122, 1.000000000000000000, 0.9659258262890683122, 1.000000000000000000, 0.9659258262890683122, 1.000000000000000000, 0.9659258262890683122, 1.000000000000000000, 0.9659258262890683122, 1.000000000000000000, 0.9659258262890683122, 1.000000000000000000, 0.9659258262890683122, 1.000000000000000000, 0.9659258262890683122, 1.000000000000000000, 0.9659258262890683122, 1.000000000000000000, 0.9659258262890683122, 1.000000000000000000, 0.9659258262890683122, 1.000000000000000000, 0.9659258262890683122, 1.000000000000000000, 0.9659258262890683122, 1.000000000000000000, 0.9659258262890683122, 1.000000000000000000, 0.9659258262890683122, 1.000000000000000000, 0.9659258262890683122, 1.000000000000000000, 0.9659258262890683122, 1.000000000000000000, 0.9659258262890683122, 1.000000000000000000, 0.9659258262890683122, 1.000000000000000000, 0.9659258262890683122, 1.000000000000000000, 0.9659258262890683122, 1.000000000000000000, 0.9659258262890683122, 1.000000000000000000, 0.9659258262890683122, 1.000000000000000000, 0.9659258262890683122, 1.000000000000000000, 0.9659258262890683122, 1.000000000000000000, 0.9659258262890683122, 1.000000000000000000, 0.9659258262890683122, 1.000000000000000000, 0.9659258262890683122, 1.000000000000000000, 0.9659258262890683122, 1.000000000000000000, 0.9659258262890683122, 1.000000000000000000, 0.9659258262890683122, 1.000000000000000000, 0.9659258262890683122, 1.000000000000000000, 0.9659258262890683122, 1.000000000000000000, 0.9659258262890683122, 1.000000000000000000, 0.9659258262890683122, 1.000000000000000000, 0.9659258262890683122, 1.000000000000000000, 0.9659258262890683122, 1.000000000000000000, 0.9659258262890683122, 1.000000000000000000, 0.9659258262890683122, 1.000000000000000000, 0.9659258262890683122, 1.000000000000000000, 0.9659258262890683122, 1.000000000000000000, 0.9659258262890683122, 1.000000000000000000, 0.9659258262890683122, 1.000000000000000000, 0.9659258262890683122, 1.000000000000000000, 0.9659258262890683122, 1.000000000000000000, 0.9659258262890683122, 1.000000000000000000, 0.9659258262890683122, 1.000000000000000000, 0.9659258262890683122, 1.000000000000000000, 0.9659258262890683122, 1.000000000000000000, 0.9659258262890683122, 1.000000000000000000, 0.9659258262890683122, 1.000000000000000000, 0.9659258262890683122, 1.000000000000000000, 0.9659258262890683122, 1.000000000000000000, 0.9659258262890683122, 1.000000000000000000, 0.9659258262890683122, 1.000000000000000000, 0.9659258262890683122, 1.000000000000000000, 0.9659258262890683122, 1.000000000000000000, 0.9659258262890683122, 1.000000000000000000, 0.9659258262890683122, 1.000000000000000000, 0.9659258262890683122, 1.000000000000000000, 0.9659258262890683122, 1.000000000000000000, 0.9659258262890683122, 1.000000000000000000, 0.9659258262890683122, 1.000000000000000000, 0.9659258262890683122, 1.000000000000000000, 0.9659258262890683122, 1.000000000000000000, 0.9659258262890683122, 1.000000000000000000, 0.9659258262890683122, 1.000000000000000000, 0.9659258262890683122, 1.000000000000000000, 0.9659258262890683122, 1.000000000000000000, 0.9659258262890683122, 1.000000000000000000, 0.9659258262890683122, 1.000000000000000000, 0.9659258262890683122, 1.000000000000000000, 0.9659258262890683122, 1.000000000000000000, 0.9659258262890683122, 1.000000000000000000, 0.9659258262890683122, 1.000000000000000000, 0.9659258262890683122, 1.000000000000000000, 0.9659258262890683122, 1.000000000000000000, 0.9659258262890683122, 1.000000000000000000, 0.9659258262890683122, 1.000000000000000000, 0.9659258262890683122, 1.000000000000000000, 0.9659258262890683122, 1.000000000000000000, 0.9659258262890683122, 1.000000000000000000, 0.9659258262890683122, 1.000000000000000000, 0.9659258262890683122, 1.000000000000000000, 0.9659258262890683122, 1.000000000000000000, 0.9659258262890683122, 1.000000000000000000, 0.9659258262890683122, 1.000000000000000000, 0.9659258262890683122, 1.000000000000000000, 0.9659258262890683122, 1.000000000000000000, 0.9659258262890683122, 1.000000000000000000, 0.9659258262890683122, 1.000000000000000000, 0.9659258262890683122, 1.000000000000000000, 0.9659258262890683122, 1.000000000000000000, 0.9659258262890683122, 1.000000000000000000, 0.9659258262890683122, 1.000000000000000000, 0.9659258262890683122, 1.000000000000000000, 0.9659258262890683122, 1.000000000000000000, 0.9659258262890683122, 1.000000000000000000, 0.9659258262890683122, 1.000000000000000000, 0.9659258262890683122, 1.000000000000000000, 0.9659258262890683122, 1.000000000000000000, 0.9659258262890683122, 1.000000000000000000, 0.9659258262890683122, 1.000000000000000000, 0.9659258262890683122, 1.000000000000000000, 0.9659258262890683122, 1.000000000000000000, 0.9659258262890683122, 1.000000000000000000, 0.9659258262890683122, 1.000000000000000000, 0.9659258262890683122, 1.000000000000000000, 0.9659258262890683122, 1.000000000000000000, 0.9659258262890683122, 1.000000000000000000, 0.9659258262890683122, 1.000000000000000000, 0.9659258262890683122, 1.000000000000000000, 0.9659258262890683122, 1.000000000000000000, 0.9659258262890683122, 1.000000000000000000, 0.9659258262890683122, 1.000000000000000000, 0.9659258262890683122, 1.000000000000000000, 0.9659258262890683122, 1.000000000000000000, 0.9659258262890683122, 1.000000000000000000, 0.9659258262890683122, 1.000000000000000000, 0.9659258262890683122, 1.000000000000000000, 0.9659258262890683122, 1.000000000000000000, 0.9659258262890683122, 1.000000000000000000, 0.9659258262890683122, 1.000000000000000000, 0.9659258262890683122, 1.000000000000000000, 0.9659258262890683122, 1.000000000000000000, 0.9659258262890683122, 1.000000000000000000, 0.9659258262890683122, 1.000000000000000000, 0.9659258262890683122, 1.000000000000000000, 0.9659258262890683122, 1.000000000000000000, 0.9659258262890683122, 1.000000000000000000, 0.9659258262890683122, 1.000000000000000000, 0.9659258262890683122, 1.000000000000000000, 0.9659258262890683122, 1.000000000000000000, 0.9659258262890683122, 1.000000000000000000, 0.9659258262890683122, 1.000000000000000000, 0.9659258262890683122, 1.000000000000000000, 0.9659258262890683122, 1.000000000000000000, 0.9659258262890683122, 1.000000000000000000, 0.9659258262890683122, 1.000000000000000000, 0.9659258262890683122, 1.000000000000000000, 0.9659258262890683122, 1.000000000000000000, 0.9659258262890683122, 1.000000000000000000, 0.9659258262890683122, 1.000000000000000000, 0.9659258262890683122, 1.000000000000000000, 0.9659258262890683122, 1.000000000000000000, 0.9659258262890683122, 1.000000000000000000, 0.9659258262890683122, 1.000000000000000000, 0.9659258262890683122, 1.000000000000000000, 0.9659258262890683122, 1.000000000000000000, 0.9659258262890683122, 1.000000000000000000, 0.9659258262890683122, 1.000000000000000000, 0.9659258262890683122, 1.000000000000000000, 0.9659258262890683122, 1.000000000000000000, 0.9659258262890683122, 1.000000000000000000, 0.9659258262890683122, 1.000000000000000000, 0.9659258262890683122, 1.000000000000000000, 0.9659258262890683122, 1.000000000000000000, 0.9659258262890683122, 1.000000000000000000, 0.9659258262890683122, 1.000000000000000000, 0.9659258262890683122, 1.000000000000000000, 0.9659258262890683122, 1.000000000000000000, 0.9659258262890683122, 1.000000000000000000, 0.9659258262890683122, 1.000000000000000000, 0.9659258262890683122, 1.000000000000000000, 0.9659258262890683122, 1.000000000000000000, 0.9659258262890683122, 1.000000000000000000, 0.9659258262890683122, 1.000000000000000000, 0.9659258262890683122, 1.000000000000000000, 0.9659258262890683122, 1.000000000000000000, 0.9659258262890683122, 1.000000000000000000, 0.9659258262890683122, 1.000000000000000000, 0.9659258262890683122, 1.000000000000000000, 0.9659258262890683122, 1.000000000000000000, 0.9659258262890683122, 1.000000000000000000, 0.9659258262890683122, 1.000000000000000000, 0.9659258262890683122, 1.000000000000000000, 0.9659258262890683122, 1.000000000000000000, 0.9659258262890683122, 1.000000000000000000, 0.9659258262890683122, 1.000000000000000000, 0.9659258262890683122, 1.000000000000000000, 0.9659258262890683122, 1.000000000000000000, 0.9659258262890683122, 1.000000000000000000, 0.9659258262890683122, 1.000000000000000000, 0.9659258262890683122, 1.000000000000000000, 0.9659258262890683122, 1.000000000000000000, 0.9659258262890683122, 1.000000000000000000, 0.9659258262890683122, 1.000000000000000000, 0.9659258262890683122, 1.000000000000000000, 0.9659258262890683122, 1.000000000000000000, 0.9659258262890683122, 1.000000000000000000, 0.9659258262890683122, 1.000000000000000000, 0.9659258262890683122, 1.000000000000000000, 0.9659258262890683122, 1.000000000000000000, 0.9659258262890683122, 1.000000000000000000, 0.9659258262890683122, 1.000000000000000000, 0.9659258262890683122, 1.000000000000000000, 0.9659258262890683122, 1.000000000000000000, 0.9659258262890683122, 1.000000000000000000, 0.9659258262890683122, 1.000000000000000000, 0.9659258262890683122, 1.000000000000000000, 0.9659258262890683122, 1.000000000000000000, 0.9659258262890683122, 1.000000000000000000, 0.9659258262890683122, 1.000000000000000000, 0.9659258262890683122, 1.000000000000000000) ) ) 
 REPRESENTATION_ITEM ( '' )  SURFACE ( )  );
#39822 = CARTESIAN_POINT ( 'NONE',  ( -0.5380577427821514602, 0.05413385826771666132, 0.4176697321401328100 ) ) ;
#39823 = CARTESIAN_POINT ( 'NONE',  ( -1.541994750656167090, -0.6692913385826773087, -0.1292274648535924053 ) ) ;
#39824 = CARTESIAN_POINT ( 'NONE',  ( 0.8398950131233602345, -0.6046776061558807314, 0.2411417322834647770 ) ) ;
#39825 = CARTESIAN_POINT ( 'NONE',  ( 5.785732909357575061E-17, -0.4724409448818898682, -2.125984251968504157 ) ) ;
#39826 = CARTESIAN_POINT ( 'NONE',  ( -0.7426113562971992099, 2.401574803149605586, -0.5309055118110235227 ) ) ;
#39827 = VECTOR ( 'NONE', #75595, 39.37007874015748143 ) ;
#39828 = ORIENTED_EDGE ( 'NONE', *, *, #62908, .T. ) ;
#39829 = EDGE_LOOP ( 'NONE', ( #14790, #61786, #16447, #69659 ) ) ;
#39830 = CARTESIAN_POINT ( 'NONE',  ( -1.358267716535432434, 0.1660481256975883668, -0.3530559997133364547 ) ) ;
#39832 = CARTESIAN_POINT ( 'NONE',  ( -1.259842519685038686, -0.1870078740157480879, -0.4822834645669291653 ) ) ;
#39831 = CARTESIAN_POINT ( 'NONE',  ( -1.338582677165353729, -0.1870078740157479769, 0.3641732283464567677 ) ) ;
#39833 = CARTESIAN_POINT ( 'NONE',  ( 0.3392501089628018329, -0.1958661417322834497, -2.547224778706350445 ) ) ;
#39834 = CARTESIAN_POINT ( 'NONE',  ( 1.614173228346457378, 1.267785121476991073, -0.1372047244094476148 ) ) ;
#39835 = CARTESIAN_POINT ( 'NONE',  ( -1.502624671916009680, -0.2845877964562159024, 0.3641732283464567677 ) ) ;
#39836 = CARTESIAN_POINT ( 'NONE',  ( -1.154855643044618851, -0.6046776061558809534, -0.2411417322834644161 ) ) ;
#39837 = CARTESIAN_POINT ( 'NONE',  ( 0.4068241469816279987, -0.4281496062992127816, -0.4176697321401328100 ) ) ;
#39838 = CARTESIAN_POINT ( 'NONE',  ( -1.318897637795274802, 0.1660481256975885056, 0.3530559997133364547 ) ) ;
#39839 = CARTESIAN_POINT ( 'NONE',  ( -0.1049643490035306742, 0.3917322834645668994, -2.763760211777216202 ) ) ;
#39840 = CARTESIAN_POINT ( 'NONE',  ( 0.4724409448818904789, -0.1870078740157479769, 0.4822834645669291653 ) ) ;
#39841 = CARTESIAN_POINT ( 'NONE',  ( -0.3917322834645670104, -7.196005306013484475E-17, -1.763779527559055094 ) ) ;
#39842 = CARTESIAN_POINT ( 'NONE',  ( -0.6364829396325453192, -0.08942795157528024563, -0.3641732283464568787 ) ) ;
#39843 = VERTEX_POINT ( 'NONE', #21844 ) ;
#39844 = CARTESIAN_POINT ( 'NONE',  ( -0.1058382717557503211, 0.3949938075777409408, -2.053805774278215868 ) ) ;
#39845 = ORIENTED_EDGE ( 'NONE', *, *, #22547, .T. ) ;
#39846 = CARTESIAN_POINT ( 'NONE',  ( -1.581364829396324945, -0.2845877964562159024, 0.3641732283464567677 ) ) ;
#39847 = CARTESIAN_POINT ( 'NONE',  ( -1.056430446194224881, 0.2952755905511810774, -0.1292274648535930714 ) ) ;
#39848 = CARTESIAN_POINT ( 'NONE',  ( -1.496062992125983815, -0.1870078740157479769, 0.4822834645669291653 ) ) ;
#39849 = CARTESIAN_POINT ( 'NONE',  ( -0.1998031496062994683, 0.3460692066303958092, -0.6430446194225721834 ) ) ;
#39850 = CARTESIAN_POINT ( 'NONE',  ( -1.404199475065615932, 0.05413385826771666132, 0.4176697321401328100 ) ) ;
#39851 = CARTESIAN_POINT ( 'NONE',  ( -1.397637795275589623, 0.1660481256975885056, 0.3530559997133364547 ) ) ;
#39852 = CARTESIAN_POINT ( 'NONE',  ( -1.384514435695537005, -0.6692913385826773087, -0.1292274648535924053 ) ) ;
#39853 = CARTESIAN_POINT ( 'NONE',  ( 0.03757601356357168076, -0.4709442531824368783, -4.620136098463503353E-16 ) ) ;
#39854 = DIRECTION ( 'NONE',  ( -0.5931762764595015502, 3.423560842947300903E-15, -0.8050726085550551359 ) ) ;
#39855 = CARTESIAN_POINT ( 'NONE',  ( 8.195543980992789655E-16, -0.1870078740157480601, -0.3641732283464567677 ) ) ;
#39856 = CARTESIAN_POINT ( 'NONE',  ( 0.4668652553835576646, 1.622068519643046436, 2.152447471807370061 ) ) ;
#39857 = CARTESIAN_POINT ( 'NONE',  ( -0.2867679344610365999, 0.2867679344610364889, -0.4192913385826772532 ) ) ;
#39858 = CARTESIAN_POINT ( 'NONE',  ( -0.5052493438320203589, -0.5511811023622046335, 0.09757992244046803654 ) ) ;
#39859 = CARTESIAN_POINT ( 'NONE',  ( -0.6955380577427815458, 0.05413385826771666132, 0.4176697321401328100 ) ) ;
#39860 = CARTESIAN_POINT ( 'NONE',  ( 1.023622047244095112, -0.1870078740157480879, -0.4822834645669291653 ) ) ;
#39861 = CARTESIAN_POINT ( 'NONE',  ( -1.095800524934382292, -0.3162353388693409650, -0.4822834645669289433 ) ) ;
#39862 = ORIENTED_EDGE ( 'NONE', *, *, #54110, .F. ) ;
#39863 = VERTEX_POINT ( 'NONE', #79530 ) ;
#39864 = CARTESIAN_POINT ( 'NONE',  ( -1.102362204724408601, -0.1870078740157480879, -0.4822834645669291653 ) ) ;
#39865 = CARTESIAN_POINT ( 'NONE',  ( 0.9186351706036751663, -0.6046776061558807314, 0.2411417322834647770 ) ) ;
#39866 = CARTESIAN_POINT ( 'NONE',  ( -1.463254593175852492, -0.5511811023622048555, -0.09757992244046775898 ) ) ;
#39867 =( NAMED_UNIT ( * ) SI_UNIT ( $, .STERADIAN. ) SOLID_ANGLE_UNIT ( ) );
#39868 = CARTESIAN_POINT ( 'NONE',  ( -0.4724409448818895907, -0.1265901696524993070, -1.305774278215223072 ) ) ;
#39869 = EDGE_CURVE ( 'NONE', #62181, #64347, #66325, .T. ) ;
#39870 = CARTESIAN_POINT ( 'NONE',  ( 2.058022911372368480, 1.301102360844744510, 0.4123394245947664682 ) ) ;
#39871 = CARTESIAN_POINT ( 'NONE',  ( 0.3917322834645669549, 0.1049643490035304660, -0.2742782152230970327 ) ) ;
#39872 = CARTESIAN_POINT ( 'NONE',  ( 0.3917322834645670104, -0.1049643490035303273, -2.400918635170603110 ) ) ;
#39873 = CARTESIAN_POINT ( 'NONE',  ( -0.2887139107611542133, -0.6046776061558809534, -0.2411417322834644161 ) ) ;
#39874 = CARTESIAN_POINT ( 'NONE',  ( -1.633858267716534529, 0.07958543189024085140, 0.2665933059059887866 ) ) ;
#39875 = AXIS2_PLACEMENT_3D ( 'NONE', #15634, #30299, #55139 ) ;
#39876 = CIRCLE ( 'NONE', #51918, 0.1574803149606299746 ) ;
#39877 = CARTESIAN_POINT ( 'NONE',  ( -0.8398950131233589023, -0.6046776061558809534, -0.2411417322834644161 ) ) ;
#39878 = CARTESIAN_POINT ( 'NONE',  ( 0.1998031496062994128, -0.3460692066303957537, -0.01115485564304463835 ) ) ;
#39880 = CARTESIAN_POINT ( 'NONE',  ( -0.5314960629921372526, 2.716535433070866645, 3.224202737261813834 ) ) ;
#39879 = CARTESIAN_POINT ( 'NONE',  ( -1.292650918635170010, -0.6692913385826771977, 0.1292274648535927661 ) ) ;
#39881 = CARTESIAN_POINT ( 'NONE',  ( -1.108923884514435132, -0.3162353388693405765, 0.4822834645669290543 ) ) ;
#39882 = CARTESIAN_POINT ( 'NONE',  ( -0.2887139107611542133, 0.2306618581243848609, 0.2411417322834645549 ) ) ;
#39883 = CARTESIAN_POINT ( 'NONE',  ( -0.3420746716998660508, -0.1974969037888706924, -2.806430446194226214 ) ) ;
#39884 = CARTESIAN_POINT ( 'NONE',  ( 0.2690288713910767848, -0.5511811023622048555, -0.09757992244046775898 ) ) ;
#39885 = CARTESIAN_POINT ( 'NONE',  ( -1.112701331685803652, -5.134928753749862370E-15, -0.4281989832122463091 ) ) ;
#39886 = CARTESIAN_POINT ( 'NONE',  ( 0.1574803149606306130, -0.1870078740157480601, -0.3641732283464567677 ) ) ;
#39887 = CARTESIAN_POINT ( 'NONE',  ( 1.187664041994751285, -0.2845877964562161244, -0.3641732283464567121 ) ) ;
#39888 = CARTESIAN_POINT ( 'NONE',  ( 0.7874015748031503170, -0.1870078740157479769, 0.4822834645669291653 ) ) ;
#39889 = CARTESIAN_POINT ( 'NONE',  ( 0.3018372703412079971, -0.004921259842519870586, -0.3153832671262229437 ) ) ;
#39890 = CARTESIAN_POINT ( 'NONE',  ( -0.1049643490035307020, 0.3917322834645669549, -1.888451443569553412 ) ) ;
#39891 = CARTESIAN_POINT ( 'NONE',  ( -1.102362204724408601, -0.1870078740157480879, -0.4822834645669291653 ) ) ;
#39892 = CARTESIAN_POINT ( 'NONE',  ( -0.09186351706036689768, -0.004921259842519870586, -0.3153832671262229437 ) ) ;
#39893 = CARTESIAN_POINT ( 'NONE',  ( -0.4724409448818899238, 0.1265901696524986686, -0.1095800524934383152 ) ) ;
#39894 = CARTESIAN_POINT ( 'NONE',  ( -0.6036745406824141069, -0.5023911411419708095, -0.1820866141732282451 ) ) ;
#39895 = CARTESIAN_POINT ( 'NONE',  ( -0.4736019971540468276, 1.569430237215018176, -1.017199299814984359 ) ) ;
#39896 = CARTESIAN_POINT ( 'NONE',  ( -0.03280839895013062252, 0.2952755905511810774, -0.1292274648535930714 ) ) ;
#39897 = CARTESIAN_POINT ( 'NONE',  ( 0.3149606299212636684, 2.559055118110236560, -1.076935383196056195 ) ) ;
#39898 = CARTESIAN_POINT ( 'NONE',  ( 0.8202099737532813073, 0.1771653543307087630, 0.09757992244046791164 ) ) ;
#39899 = CARTESIAN_POINT ( 'NONE',  ( 0.1706036745406830368, -0.004921259842519576551, 0.3153832671262227771 ) ) ;
#39900 = CARTESIAN_POINT ( 'NONE',  ( -0.2165354330708654795, 0.1660481256975885056, 0.3530559997133364547 ) ) ;
#39901 = LINE ( 'NONE', #26845, #66741 ) ;
#39902 = CARTESIAN_POINT ( 'NONE',  ( -0.5643044619422565855, -0.3690944881889763329, 0.3153832671262228327 ) ) ;
#39903 = CARTESIAN_POINT ( 'NONE',  ( 0.000000000000000000, 0.000000000000000000, 0.000000000000000000 ) ) ;
#39904 = CARTESIAN_POINT ( 'NONE',  ( 0.7808398950131241190, -0.05778040916215560624, -0.4822834645669293319 ) ) ;
#39905 = CARTESIAN_POINT ( 'NONE',  ( -0.7217847769028863381, -0.4281496062992124485, 0.4176697321401328655 ) ) ;
#39906 = CARTESIAN_POINT ( 'NONE',  ( 0.2925321140481932369, 0.2925321140481932369, -1.316929133858267598 ) ) ;
#39907 = EDGE_CURVE ( 'NONE', #76998, #45287, #81579, .T. ) ;
#39908 = CARTESIAN_POINT ( 'NONE',  ( -0.3917322834645671215, 0.1049643490035301469, -2.637139107611548461 ) ) ;
#39909 = CARTESIAN_POINT ( 'NONE',  ( 0.08530183727034192087, -0.2845877964562161244, -0.3641732283464567121 ) ) ;
#39910 = CARTESIAN_POINT ( 'NONE',  ( -0.7349081364829387342, -0.6046776061558807314, 0.2411417322834647770 ) ) ;
#39911 = CARTESIAN_POINT ( 'NONE',  ( -1.043307086614172041, -0.5400638737290844871, 0.3530559997133364547 ) ) ;
#39912 = CARTESIAN_POINT ( 'NONE',  ( -1.364829396325458521, -0.5023911411419708095, 0.1820866141732285504 ) ) ;
#39913 = CARTESIAN_POINT ( 'NONE',  ( -0.9881811337016640495, 2.559055118110236560, -0.5314960629921260393 ) ) ;
#39914 = CARTESIAN_POINT ( 'NONE',  ( -1.056430446194224881, -0.5511811023622046335, 0.09757992244046803654 ) ) ;
#39915 = DIRECTION ( 'NONE',  ( -0.000000000000000000, 1.000000000000000000, -0.000000000000000000 ) ) ;
#39916 = CARTESIAN_POINT ( 'NONE',  ( 0.8989501312335963501, -0.6692913385826773087, -0.1292274648535924053 ) ) ;
#39917 = CARTESIAN_POINT ( 'NONE',  ( -0.1070741851644056997, 0.3996062992125986035, -0.1640419947506561726 ) ) ;
#39918 = CARTESIAN_POINT ( 'NONE',  ( 0.1049643490035304799, -0.3917322834645670104, -2.444245037566615597 ) ) ;
#39919 = ORIENTED_EDGE ( 'NONE', *, *, #61425, .F. ) ;
#39920 = CARTESIAN_POINT ( 'NONE',  ( 0.4470386624395689124, 1.696927142811738287, -2.611610595642054999 ) ) ;
#39921 = CARTESIAN_POINT ( 'NONE',  ( -1.706036745406823485, 0.2306618581243848609, 0.2411417322834645549 ) ) ;
#39922 = CARTESIAN_POINT ( 'NONE',  ( -1.200787401574802349, 0.1660481256975883668, -0.3530559997133364547 ) ) ;
#39923 = VECTOR ( 'NONE', #33503, 39.37007874015748854 ) ;
#39924 = CARTESIAN_POINT ( 'NONE',  ( 1.036745406824147508, -0.4281496062992127816, -0.4176697321401328100 ) ) ;
#39925 = CARTESIAN_POINT ( 'NONE',  ( -0.1958661417322834220, -0.3392501089628018884, -2.512467191601049699 ) ) ;
#39926 = CARTESIAN_POINT ( 'NONE',  ( 1.574803149606299746, -0.1870078740157480601, -0.3641732283464567677 ) ) ;
#39927 = CARTESIAN_POINT ( 'NONE',  ( 0.5249343832021005074, -0.6046776061558807314, 0.2411417322834647770 ) ) ;
#39928 = CARTESIAN_POINT ( 'NONE',  ( -0.2821522309711278487, -0.6692913385826773087, -0.1292274648535924053 ) ) ;
#39929 = CARTESIAN_POINT ( 'NONE',  ( -3.912791665790199769, 1.724409448818897905, 0.4359958488159718093 ) ) ;
#39930 = AXIS2_PLACEMENT_3D ( 'NONE', #56496, #57313, #83011 ) ;
#39932 = CARTESIAN_POINT ( 'NONE',  ( 3.884512598959606322, 2.725419031863056230, 0.5314960629921259283 ) ) ;
#39931 = AXIS2_PLACEMENT_3D ( 'NONE', #6068, #82281, #45181 ) ;
#39933 = CARTESIAN_POINT ( 'NONE',  ( 0.6430446194225728496, -0.004921259842519576551, 0.3153832671262227771 ) ) ;
#39934 = ADVANCED_FACE ( 'NONE', ( #61387 ), #37220, .F. ) ;
#39935 = CARTESIAN_POINT ( 'NONE',  ( 0.1070741851644054915, -0.3996062992125986035, -1.502624671916010346 ) ) ;
#39936 = VERTEX_POINT ( 'NONE', #60970 ) ;
#39937 = CARTESIAN_POINT ( 'NONE',  ( 0.1049643490035304799, -0.3917322834645670104, 0.07544000180346267792 ) ) ;
#39938 = ORIENTED_EDGE ( 'NONE', *, *, #80504, .T. ) ;
#39939 = CARTESIAN_POINT ( 'NONE',  ( 0.01968503937007930540, 0.1660481256975885056, 0.3530559997133364547 ) ) ;
#39940 = CARTESIAN_POINT ( 'NONE',  ( 1.312335958005249825, 0.2306618581243847221, -0.2411417322834647770 ) ) ;
#39941 = CARTESIAN_POINT ( 'NONE',  ( 0.2821522309711292364, 0.2952755905511810774, -0.1292274648535930714 ) ) ;
#39942 = CARTESIAN_POINT ( 'NONE',  ( -0.4461942257217840213, -0.5023911411419708095, -0.1820866141732282451 ) ) ;
#39943 = CARTESIAN_POINT ( 'NONE',  ( 1.272965879265092637, -0.4281496062992127816, -0.4176697321401328100 ) ) ;
#39944 = ADVANCED_FACE ( 'NONE', ( #10476 ), #61802, .T. ) ;
#39945 = CARTESIAN_POINT ( 'NONE',  ( -0.7020997375328074108, -0.05778040916215522460, 0.4822834645669289988 ) ) ;
#39946 = CARTESIAN_POINT ( 'NONE',  ( -0.1049868766404193215, 0.2306618581243847221, -0.2411417322834647770 ) ) ;
#39947 = CARTESIAN_POINT ( 'NONE',  ( 1.496062992125984703, -0.1870078740157480879, -0.4822834645669291653 ) ) ;
#39948 = CARTESIAN_POINT ( 'NONE',  ( 1.167979002624672580, 0.05413385826771626580, -0.4176697321401330321 ) ) ;
#39949 = CARTESIAN_POINT ( 'NONE',  ( 1.095800524934383846, -0.05778040916215560624, -0.4822834645669293319 ) ) ;
#39950 = CARTESIAN_POINT ( 'NONE',  ( -9.594673741351313045E-17, 0.3917322834645670104, -0.6220472440944880832 ) ) ;
#39951 = CARTESIAN_POINT ( 'NONE',  ( 0.5577427821522316087, -0.08942795157527998196, 0.3641732283464567121 ) ) ;
#39952 = ORIENTED_EDGE ( 'NONE', *, *, #7540, .T. ) ;
#39953 = CARTESIAN_POINT ( 'NONE',  ( -0.1974969037888706647, 0.3420746716998658843, -0.8005249343832020470 ) ) ;
#39954 = VERTEX_POINT ( 'NONE', #80362 ) ;
#39955 = CARTESIAN_POINT ( 'NONE',  ( -0.5971128608923877978, 0.1771653543307087630, 0.09757992244046791164 ) ) ;
#39956 = CARTESIAN_POINT ( 'NONE',  ( -0.1312335958005241554, -0.6046776061558809534, -0.2411417322834644161 ) ) ;
#39957 = CARTESIAN_POINT ( 'NONE',  ( -1.428351447576950095, 1.168345958003150331, 0.2981497428225624580 ) ) ;
#39958 = CARTESIAN_POINT ( 'NONE',  ( -0.1049868766404193215, 0.2306618581243847221, -0.2411417322834647770 ) ) ;
#39959 = CARTESIAN_POINT ( 'NONE',  ( -0.01312335958005186876, -0.4281496062992124485, 0.4176697321401328655 ) ) ;
#39960 = CARTESIAN_POINT ( 'NONE',  ( -0.7611548556430438595, -0.6046776061558809534, -0.2411417322834644161 ) ) ;
#39961 = CARTESIAN_POINT ( 'NONE',  ( -1.194225721784776262, 0.05413385826771626580, -0.4176697321401330321 ) ) ;
#39962 = CARTESIAN_POINT ( 'NONE',  ( 1.515748031496063408, 0.07958543189024085140, 0.2665933059059887866 ) ) ;
#39963 = CARTESIAN_POINT ( 'NONE',  ( -1.653543307086613234, -0.1870078740157479769, 0.4822834645669291653 ) ) ;
#39964 = CARTESIAN_POINT ( 'NONE',  ( -0.1463826306659128940, -2.624320362099288585E-15, 0.3954974714151479054 ) ) ;
#39965 = CARTESIAN_POINT ( 'NONE',  ( 1.023622047244095112, -0.1870078740157480601, -0.3641732283464567677 ) ) ;
#39966 = CARTESIAN_POINT ( 'NONE',  ( 0.4593175853018380828, 0.05413385826771626580, -0.4176697321401330321 ) ) ;
#39967 = CARTESIAN_POINT ( 'NONE',  ( 0.7939632545931766261, -0.3162353388693409650, -0.4822834645669289433 ) ) ;
#39968 = CARTESIAN_POINT ( 'NONE',  ( -0.1070741851644056997, 0.3996062992125986035, -1.108923884514435798 ) ) ;
#39969 = FACE_OUTER_BOUND ( 'NONE', #64908, .T. ) ;
#39970 = CARTESIAN_POINT ( 'NONE',  ( -0.3996062992125984925, -0.1070741851644056858, -0.5951443569553805935 ) ) ;
#39971 = CARTESIAN_POINT ( 'NONE',  ( -0.2925321140481930149, -0.2925321140481933480, -0.4507874015748031815 ) ) ;
#39972 = CARTESIAN_POINT ( 'NONE',  ( -0.5183727034120726440, -0.6692913385826773087, -0.1292274648535924053 ) ) ;
#39973 = CARTESIAN_POINT ( 'NONE',  ( -0.3458507752293909498, 0.3458507752293907833, -0.01968503937007874335 ) ) ;
#39974 = CARTESIAN_POINT ( 'NONE',  ( -0.1049643490035302024, -0.3917322834645671215, -2.204068241469816503 ) ) ;
#39975 = CARTESIAN_POINT ( 'NONE',  ( -1.220472440944881054, -0.5511811023622047445, 6.969142054262312111E-17 ) ) ;
#39976 = CARTESIAN_POINT ( 'NONE',  ( 1.076115485564305141, -0.6046776061558807314, 0.2411417322834647770 ) ) ;
#39977 = CARTESIAN_POINT ( 'NONE',  ( 1.069553805774278832, 0.2952755905511810774, -0.1292274648535930714 ) ) ;
#39978 = CARTESIAN_POINT ( 'NONE',  ( -0.2624671916010490880, -0.5023911411419708095, 0.1820866141732285504 ) ) ;
#39979 = CARTESIAN_POINT ( 'NONE',  ( 0.3018372703412079971, -0.4281496062992124485, 0.4176697321401328655 ) ) ;
#39980 = CARTESIAN_POINT ( 'NONE',  ( -0.4724409448818898682, -8.678599364036362592E-17, -2.005905511811023612 ) ) ;
#39981 = CARTESIAN_POINT ( 'NONE',  ( -0.2559055118110227234, -0.4536011799217367080, 0.2665933059059888421 ) ) ;
#39982 = CARTESIAN_POINT ( 'NONE',  ( 0.1706036745406830368, 0.05413385826771666132, 0.4176697321401328100 ) ) ;
#39983 = CARTESIAN_POINT ( 'NONE',  ( 0.2891555358219910499, 0.2891555358219910499, -1.474409448818897683 ) ) ;
#39984 = CARTESIAN_POINT ( 'NONE',  ( -1.299212598425196097, -0.6692913385826771977, 8.415575281601705876E-17 ) ) ;
#39985 = CARTESIAN_POINT ( 'NONE',  ( 0.6889763779527563470, 0.07958543189024071263, -0.2665933059059888421 ) ) ;
#39986 = CARTESIAN_POINT ( 'NONE',  ( 1.443569553805774897, -0.5023911411419708095, -0.1820866141732282451 ) ) ;
#39987 = CARTESIAN_POINT ( 'NONE',  ( -0.7742782152230965886, 0.05413385826771666132, 0.4176697321401328100 ) ) ;
#39988 = CARTESIAN_POINT ( 'NONE',  ( -0.3871391076115476282, -0.08942795157527998196, 0.3641732283464567121 ) ) ;
#39989 = LINE ( 'NONE', #31995, #49345 ) ;
#39990 = CARTESIAN_POINT ( 'NONE',  ( -0.8464566929133852113, -0.5400638737290845981, -0.3530559997133363437 ) ) ;
#39991 = CARTESIAN_POINT ( 'NONE',  ( -0.7414698162729651543, -0.6692913385826771977, 0.1292274648535927661 ) ) ;
#39992 = CARTESIAN_POINT ( 'NONE',  ( -0.07874015748031421014, -0.1870078740157479769, 0.4822834645669291653 ) ) ;
#39993 = CARTESIAN_POINT ( 'NONE',  ( 0.3460692066303959202, -0.1998031496062991630, -2.071522309711286258 ) ) ;
#39994 = CIRCLE ( 'NONE', #69275, 0.1574803149606300579 ) ;
#39996 = CARTESIAN_POINT ( 'NONE',  ( 0.1049643490035303689, 0.3917322834645668994, -2.278195907315273327 ) ) ;
#39995 =( GEOMETRIC_REPRESENTATION_CONTEXT ( 3 ) GLOBAL_UNCERTAINTY_ASSIGNED_CONTEXT ( ( #57972 ) ) GLOBAL_UNIT_ASSIGNED_CONTEXT ( ( #38360, #45496, #39191 ) ) REPRESENTATION_CONTEXT ( 'NONE', 'WORKASPACE' ) );
#39997 = FACE_OUTER_BOUND ( 'NONE', #63429, .T. ) ;
#39998 = CARTESIAN_POINT ( 'NONE',  ( 0.5708661417322842269, 0.07958543189024085140, 0.2665933059059887866 ) ) ;
#39999 = CARTESIAN_POINT ( 'NONE',  ( 1.318897637795276356, 0.1660481256975883668, -0.3530559997133364547 ) ) ;
#40000 = CARTESIAN_POINT ( 'NONE',  ( -0.6824146981627291497, -0.5023911411419708095, -0.1820866141732282451 ) ) ;
#40001 = CARTESIAN_POINT ( 'NONE',  ( -1.187664041994750175, -0.08942795157528024563, -0.3641732283464568787 ) ) ;
#40002 = CARTESIAN_POINT ( 'NONE',  ( -0.6824146981627288167, 0.2306618581243848609, 0.2411417322834645549 ) ) ;
#40003 = CARTESIAN_POINT ( 'NONE',  ( -0.3412073490813641308, -0.6046776061558807314, 0.2411417322834647770 ) ) ;
#40004 = CARTESIAN_POINT ( 'NONE',  ( 0.7152230971128616943, -0.08942795157527998196, 0.3641732283464567121 ) ) ;
#40005 = DIRECTION ( 'NONE',  ( 0.000000000000000000, 0.000000000000000000, -1.000000000000000000 ) ) ;
#40006 = CARTESIAN_POINT ( 'NONE',  ( 1.003937007874016185, 0.07958543189024071263, -0.2665933059059888421 ) ) ;
#40007 = CARTESIAN_POINT ( 'NONE',  ( 0.4593175853018380828, 0.05413385826771626580, -0.4176697321401330321 ) ) ;
#40008 = CARTESIAN_POINT ( 'NONE',  ( 0.3996062992125985480, 2.446882876249141654E-17, 0.1200787401574803098 ) ) ;
#40009 = CARTESIAN_POINT ( 'NONE',  ( -0.7939632545931754048, -0.3162353388693405765, 0.4822834645669290543 ) ) ;
#40010 = CARTESIAN_POINT ( 'NONE',  ( 0.3392501089628018884, -0.1958661417322834220, -1.606955380577427928 ) ) ;
#40011 = CARTESIAN_POINT ( 'NONE',  ( 1.574803149606299746, -0.1870078740157479769, 0.3641732283464567677 ) ) ;
#40012 = CARTESIAN_POINT ( 'NONE',  ( 0.3215223097112867578, -0.3162353388693409650, -0.4822834645669289433 ) ) ;
#40013 = CARTESIAN_POINT ( 'NONE',  ( 0.03280839895013198948, -0.6692913385826773087, -0.1292274648535924053 ) ) ;
#40014 = CARTESIAN_POINT ( 'NONE',  ( 0.09842519685039434474, 0.07958543189024085140, 0.2665933059059887866 ) ) ;
#40015 = CARTESIAN_POINT ( 'NONE',  ( 0.5636006452641431075, 3.421639014772782816E-16, 0.3464511005275203726 ) ) ;
#40016 = CARTESIAN_POINT ( 'NONE',  ( -0.1902887139107604098, 0.1771653543307087075, -0.09757992244046823083 ) ) ;
#40017 = CARTESIAN_POINT ( 'NONE',  ( 0.5839895013123367340, 0.2952755905511811885, 0.1292274648535926551 ) ) ;
#40018 = CARTESIAN_POINT ( 'NONE',  ( -0.5905511811023615998, 0.1771653543307087630, 0.000000000000000000 ) ) ;
#40019 = CARTESIAN_POINT ( 'NONE',  ( -0.8923884514435688198, -0.6046776061558807314, 0.2411417322834647770 ) ) ;
#40020 = DIRECTION ( 'NONE',  ( -0.000000000000000000, -1.000000000000000000, -0.000000000000000000 ) ) ;
#40021 = ORIENTED_EDGE ( 'NONE', *, *, #56065, .T. ) ;
#40022 = CARTESIAN_POINT ( 'NONE',  ( -1.062992125984250968, -0.6692913385826771977, 8.415575281601705876E-17 ) ) ;
#40023 = CARTESIAN_POINT ( 'NONE',  ( -0.9973753280839886548, -0.5023911411419708095, -0.1820866141732282451 ) ) ;
#40024 = CARTESIAN_POINT ( 'NONE',  ( -0.09842519685039295696, 0.1660481256975883668, -0.3530559997133364547 ) ) ;
#40025 = CARTESIAN_POINT ( 'NONE',  ( -1.692913385826770645, 0.2952755905511811885, 0.000000000000000000 ) ) ;
#40026 = CARTESIAN_POINT ( 'NONE',  ( -0.7480314960629914633, -0.6692913385826771977, 8.415575281601705876E-17 ) ) ;
#40027 = LINE ( 'NONE', #52212, #44456 ) ;
#40029 = CARTESIAN_POINT ( 'NONE',  ( 1.049868766404200127, -0.6046776061558809534, -0.2411417322834644161 ) ) ;
#40028 = CARTESIAN_POINT ( 'NONE',  ( -0.9251968503937002541, 0.1660481256975885056, 0.3530559997133364547 ) ) ;
#40030 = CARTESIAN_POINT ( 'NONE',  ( 0.9448818897637802916, -0.1870078740157480879, -0.4822834645669291653 ) ) ;
#40031 = CARTESIAN_POINT ( 'NONE',  ( 0.3392501089628018884, -0.1958661417322834220, -2.459317585301837195 ) ) ;
#40032 = CARTESIAN_POINT ( 'NONE',  ( 0.6299212598424790421, 1.724409448818897905, 3.886287458032468667 ) ) ;
#40033 = CARTESIAN_POINT ( 'NONE',  ( -1.227034120734907585, 0.2952755905511811885, 0.1292274648535926551 ) ) ;
#40034 = ADVANCED_FACE ( 'NONE', ( #66473 ), #35717, .F. ) ;
#40035 = CARTESIAN_POINT ( 'NONE',  ( -0.3996062992125987146, 0.1070741851644051862, -0.03280839895013124702 ) ) ;
#40036 = ORIENTED_EDGE ( 'NONE', *, *, #52190, .T. ) ;
#40037 = CARTESIAN_POINT ( 'NONE',  ( -0.4527559055118102749, -0.4536011799217368745, -0.2665933059059886201 ) ) ;
#40038 = CARTESIAN_POINT ( 'NONE',  ( -0.3917322834645669549, -0.1049643490035306603, -1.612860892388451539 ) ) ;
#40039 = ORIENTED_EDGE ( 'NONE', *, *, #44272, .T. ) ;
#40040 = CARTESIAN_POINT ( 'NONE',  ( 0.4068241469816279987, -0.4281496062992127816, -0.4176697321401328100 ) ) ;
#40041 = CARTESIAN_POINT ( 'NONE',  ( -0.1246719160104980823, 0.2952755905511811885, 0.1292274648535926551 ) ) ;
#40042 = CARTESIAN_POINT ( 'NONE',  ( -0.5643044619422565855, -0.4281496062992124485, 0.4176697321401328655 ) ) ;
#40043 = CARTESIAN_POINT ( 'NONE',  ( 1.640419947506562393, -0.4281496062992124485, 0.4176697321401328655 ) ) ;
#40044 = CARTESIAN_POINT ( 'NONE',  ( -0.9908136482939626788, 0.1771653543307087630, 0.09757992244046791164 ) ) ;
#40045 = DIRECTION ( 'NONE',  ( 0.000000000000000000, 0.000000000000000000, 1.000000000000000000 ) ) ;
#40046 = CARTESIAN_POINT ( 'NONE',  ( 0.7545931758530189937, 0.2952755905511810774, -0.1292274648535930714 ) ) ;
#40047 = CARTESIAN_POINT ( 'NONE',  ( 0.6036745406824153282, -0.5023911411419708095, 0.1820866141732285504 ) ) ;
#40048 = CARTESIAN_POINT ( 'NONE',  ( -0.3937007874015740483, -0.1870078740157479769, 0.4822834645669291653 ) ) ;
#40049 = CARTESIAN_POINT ( 'NONE',  ( 0.3917322834645669549, 2.398668435337827645E-17, -1.143025303640733181 ) ) ;
#40050 = CARTESIAN_POINT ( 'NONE',  ( -0.8530183727034112984, 0.05413385826771666132, 0.4176697321401328100 ) ) ;
#40051 = CARTESIAN_POINT ( 'NONE',  ( 1.614173228346456712, 0.7166040191147866611, 0.1372047244094478646 ) ) ;
#40052 = CARTESIAN_POINT ( 'NONE',  ( 1.371391076115485941, 0.2952755905511811885, 0.1292274648535926551 ) ) ;
#40053 = VERTEX_POINT ( 'NONE', #48334 ) ;
#40054 = CARTESIAN_POINT ( 'NONE',  ( 0.3917322834645670659, -0.1049643490035303273, -2.313011441766091192 ) ) ;
#40055 = CARTESIAN_POINT ( 'NONE',  ( 0.1771653543307093182, -0.5400638737290845981, -0.3530559997133363437 ) ) ;
#40056 = EDGE_LOOP ( 'NONE', ( #18322, #64888, #28041, #10874, #51178, #74516, #69344, #57604 ) ) ;
#40057 = CARTESIAN_POINT ( 'NONE',  ( -1.371391076115484831, 0.2952755905511810774, -0.1292274648535930714 ) ) ;
#40058 = CARTESIAN_POINT ( 'NONE',  ( 1.601049868766404982, 0.2306618581243848609, 0.2411417322834645549 ) ) ;
#40059 = CARTESIAN_POINT ( 'NONE',  ( 1.325459317585302665, 0.05413385826771626580, -0.4176697321401330321 ) ) ;
#40060 = CARTESIAN_POINT ( 'NONE',  ( 0.4199475065616803948, -0.6046776061558809534, -0.2411417322834644161 ) ) ;
#40061 = CARTESIAN_POINT ( 'NONE',  ( -0.2493438320209966919, -0.4281496062992124485, 0.4176697321401328655 ) ) ;
#40062 = CARTESIAN_POINT ( 'NONE',  ( 0.1958661417322834775, 0.3392501089628018884, -1.803805774278215202 ) ) ;
#40063 = CARTESIAN_POINT ( 'NONE',  ( -1.135170603674539924, -0.6692913385826771977, 0.1292274648535927661 ) ) ;
#40064 = CARTESIAN_POINT ( 'NONE',  ( -0.4790026246719152336, -0.05778040916215560624, -0.4822834645669293319 ) ) ;
#40065 = CARTESIAN_POINT ( 'NONE',  ( -0.5905511811023613777, -0.5511811023622047445, 6.969142054262312111E-17 ) ) ;
#40066 = DIRECTION ( 'NONE',  ( 1.000000000000000000, 0.000000000000000000, 0.000000000000000000 ) ) ;
#40067 = CARTESIAN_POINT ( 'NONE',  ( -0.6233595800524928121, -0.05778040916215522460, 0.4822834645669289988 ) ) ;
#40068 = CARTESIAN_POINT ( 'NONE',  ( -0.5314960629921392510, 2.753420937170568461, 3.841955293929014026 ) ) ;
#40069 = CARTESIAN_POINT ( 'NONE',  ( 0.7808398950131240079, -0.3162353388693405765, 0.4822834645669290543 ) ) ;
#40070 = CARTESIAN_POINT ( 'NONE',  ( 3.926395708098648907, 1.160952188075316860, -0.2891268611046654002 ) ) ;
#40071 = CARTESIAN_POINT ( 'NONE',  ( 0.04593175853018440641, -0.6692913385826771977, 0.1292274648535927661 ) ) ;
#40072 = CARTESIAN_POINT ( 'NONE',  ( -0.4133858267716528645, 0.07958543189024071263, -0.2665933059059888421 ) ) ;
#40074 = CARTESIAN_POINT ( 'NONE',  ( -0.8923884514435688198, 0.1539470093639521697, -0.1968503937007875793 ) ) ;
#40073 = CARTESIAN_POINT ( 'NONE',  ( 0.8661417322834653598, -0.1870078740157479769, 0.3641732283464567677 ) ) ;
#40075 = CARTESIAN_POINT ( 'NONE',  ( 5.785732909357575061E-17, -0.4724409448818898682, -0.6279527559055118058 ) ) ;
#40076 = CARTESIAN_POINT ( 'NONE',  ( 0.9842519685039378130, -0.5511811023622047445, 6.969142054262312111E-17 ) ) ;
#40077 = CARTESIAN_POINT ( 'NONE',  ( 1.213910761154856299, -0.6692913385826773087, -0.1292274648535924053 ) ) ;
#40078 = B_SPLINE_CURVE_WITH_KNOTS ( 'NONE', 3,
 ( #77748, #57939, #71427, #19652, #45731, #33124 ),
 .UNSPECIFIED., .F., .F.,
 ( 4, 2, 4 ),
 ( 0.008003512672130536076, 0.008448156958474645206, 0.008892801244818756071 ),
 .UNSPECIFIED. ) ;
#40079 = CARTESIAN_POINT ( 'NONE',  ( -0.1974969037888706924, 0.3420746716998658843, -0.08989501312335958227 ) ) ;
#40080 = CARTESIAN_POINT ( 'NONE',  ( 0.2296587926509192634, -0.05778040916215560624, -0.4822834645669293319 ) ) ;
#40081 = CARTESIAN_POINT ( 'NONE',  ( -1.502624671916009680, -0.3162353388693405765, 0.4822834645669290543 ) ) ;
#40082 = CARTESIAN_POINT ( 'NONE',  ( -1.450131233595799651, -0.6692913385826771977, 0.1292274648535927661 ) ) ;
#40083 = CARTESIAN_POINT ( 'NONE',  ( -0.06561679790026180015, -0.4281496062992127816, -0.4176697321401328100 ) ) ;
#40084 = CARTESIAN_POINT ( 'NONE',  ( 0.2891555358219910499, -0.2891555358219909944, -0.01771653543307087977 ) ) ;
#40085 = CARTESIAN_POINT ( 'NONE',  ( -1.463254593175852492, 0.1771653543307087630, 0.09757992244046791164 ) ) ;
#40086 = CARTESIAN_POINT ( 'NONE',  ( 0.4527559055118117182, -0.5400638737290844871, 0.3530559997133364547 ) ) ;
#40087 = CARTESIAN_POINT ( 'NONE',  ( 1.056430446194226658, 0.1771653543307087630, 0.09757992244046791164 ) ) ;
#40088 = CARTESIAN_POINT ( 'NONE',  ( 0.8001742991414061423, 0.004960608223778823628, 0.3437734562760190182 ) ) ;
#40089 = CARTESIAN_POINT ( 'NONE',  ( 0.2624671916010504757, 0.1283753931104748280, 0.1820866141732283561 ) ) ;
#40090 = CARTESIAN_POINT ( 'NONE',  ( -1.213910761154854745, -0.6692913385826771977, 0.1292274648535927661 ) ) ;
#40091 = CARTESIAN_POINT ( 'NONE',  ( -0.2925321140481932369, 0.2925321140481931259, -1.041338582677165281 ) ) ;
#40092 = CARTESIAN_POINT ( 'NONE',  ( 1.233595800524935227, 0.2306618581243847221, -0.2411417322834647770 ) ) ;
#40093 = CARTESIAN_POINT ( 'NONE',  ( -0.1958661417322834220, -0.3392501089628018884, -0.5301837270341206443 ) ) ;
#40094 = CARTESIAN_POINT ( 'NONE',  ( 0.5183727034120741983, -0.6692913385826771977, 0.1292274648535927661 ) ) ;
#40095 = CARTESIAN_POINT ( 'NONE',  ( -0.7988977408164217309, -3.187520833735697382E-15, -0.3791475997938244524 ) ) ;
#40096 = CARTESIAN_POINT ( 'NONE',  ( 0.5380577427821529035, -0.004921259842519870586, -0.3153832671262229437 ) ) ;
#40097 = CARTESIAN_POINT ( 'NONE',  ( 0.5511811023622055217, -0.1870078740157479769, 0.4822834645669291653 ) ) ;
#40098 = CARTESIAN_POINT ( 'NONE',  ( -0.2378425880835044470, 0.1752652180395699311, 0.1496354662858539464 ) ) ;
#40099 = CARTESIAN_POINT ( 'NONE',  ( -1.036745406824146176, -0.004921259842519870586, -0.3153832671262229437 ) ) ;
#40100 = CARTESIAN_POINT ( 'NONE',  ( -1.141732283464566011, -0.6692913385826771977, 8.415575281601705876E-17 ) ) ;
#40101 = CARTESIAN_POINT ( 'NONE',  ( -1.653543307086613234, -0.1870078740157480879, -0.4822834645669291653 ) ) ;
#40102 = CARTESIAN_POINT ( 'NONE',  ( 0.9186351706036752773, 0.2306618581243847221, -0.2411417322834647770 ) ) ;
#40103 = CARTESIAN_POINT ( 'NONE',  ( 1.601049868766404982, -0.6046776061558809534, -0.2411417322834644161 ) ) ;
#40104 = FACE_OUTER_BOUND ( 'NONE', #79621, .T. ) ;
#40105 = CARTESIAN_POINT ( 'NONE',  ( 0.6758530183727039509, 0.2952755905511810774, -0.1292274648535930714 ) ) ;
#40106 = VECTOR ( 'NONE', #42387, 39.37007874015748143 ) ;
#40107 = CARTESIAN_POINT ( 'NONE',  ( -0.1265901696524986964, -0.4724409448818899238, -2.826115485564304475 ) ) ;
#40108 = CARTESIAN_POINT ( 'NONE',  ( 0.3567026107877686592, 1.224237700298272502, 3.920828153186683096 ) ) ;
#40109 = CARTESIAN_POINT ( 'NONE',  ( 1.522309711286089939, 0.2306618581243848609, 0.2411417322834645549 ) ) ;
#40110 = CARTESIAN_POINT ( 'NONE',  ( -1.587926509186350810, -0.3690944881889763329, 0.3153832671262228327 ) ) ;
#40111 = CARTESIAN_POINT ( 'NONE',  ( 1.384514435695538559, 0.1771653543307087075, -0.09757992244046823083 ) ) ;
#40112 = CARTESIAN_POINT ( 'NONE',  ( -1.404199475065615932, -0.3690944881889765550, -0.3153832671262227771 ) ) ;
#40113 = CARTESIAN_POINT ( 'NONE',  ( -0.4199475065616791736, -0.5023911411419708095, 0.1820866141732285504 ) ) ;
#40114 = CARTESIAN_POINT ( 'NONE',  ( 1.594488188976378673, 0.1660481256975885056, 0.3530559997133364547 ) ) ;
#40115 = CARTESIAN_POINT ( 'NONE',  ( 0.3149606299212603933, -0.1870078740157479769, 0.3641732283464567677 ) ) ;
#40116 = CARTESIAN_POINT ( 'NONE',  ( 0.4593175853018380828, 0.05413385826771626580, -0.4176697321401330321 ) ) ;
#40117 = CARTESIAN_POINT ( 'NONE',  ( 0.8989501312335963501, -0.6692913385826773087, -0.1292274648535924053 ) ) ;
#40118 = CARTESIAN_POINT ( 'NONE',  ( -0.1115485564304453947, -0.6692913385826771977, 0.1292274648535927661 ) ) ;
#40119 = CARTESIAN_POINT ( 'NONE',  ( 0.2427821522309716595, -0.2845877964562161244, -0.3641732283464567121 ) ) ;
#40120 = CARTESIAN_POINT ( 'NONE',  ( 1.253280839895013710, -0.3162353388693405765, 0.4822834645669290543 ) ) ;
#40121 = ADVANCED_FACE ( 'NONE', ( #15550 ), #73626, .F. ) ;
#40122 = CARTESIAN_POINT ( 'NONE',  ( -1.601049868766403650, 0.2306618581243847221, -0.2411417322834647770 ) ) ;
#40123 = CARTESIAN_POINT ( 'NONE',  ( -0.7480314960629914633, 0.2952755905511811885, 0.000000000000000000 ) ) ;
#40124 = B_SPLINE_CURVE_WITH_KNOTS ( 'NONE', 3,
 ( #80761, #22257, #23075, #67298 ),
 .UNSPECIFIED., .F., .F.,
 ( 4, 4 ),
 ( 0.000000000000000000, 0.001493228121701169198 ),
 .UNSPECIFIED. ) ;
#40125 = CARTESIAN_POINT ( 'NONE',  ( -0.1998031496062994683, 0.3460692066303958092, -0.6430446194225721834 ) ) ;
#40126 = CARTESIAN_POINT ( 'NONE',  ( -0.2872938682423638590, 1.168647385053847909, 0.1245073136739714287 ) ) ;
#40127 = CARTESIAN_POINT ( 'NONE',  ( 0.05905511811023681640, 0.1660481256975883668, -0.3530559997133364547 ) ) ;
#40128 = CARTESIAN_POINT ( 'NONE',  ( -0.8792650918635160906, -0.4281496062992124485, 0.4176697321401328655 ) ) ;
#40129 = CARTESIAN_POINT ( 'NONE',  ( 5.463695987328526437E-16, -0.1870078740157479769, 0.4822834645669291653 ) ) ;
#40130 = CARTESIAN_POINT ( 'NONE',  ( -0.3996062992125987146, 0.1070741851644051862, -2.552493438320210029 ) ) ;
#40131 = CARTESIAN_POINT ( 'NONE',  ( -0.3949938075777409408, -0.1058382717557502933, -1.935695538057742748 ) ) ;
#40132 = CARTESIAN_POINT ( 'NONE',  ( 0.1958661417322836440, -0.3392501089628017219, -0.5564304461942257696 ) ) ;
#40133 = EDGE_CURVE ( 'NONE', #46648, #29487, #74031, .T. ) ;
#40134 = CARTESIAN_POINT ( 'NONE',  ( -0.3917322834645671215, 0.1049643490035301469, -1.127296587926509108 ) ) ;
#40135 = CARTESIAN_POINT ( 'NONE',  ( -1.010498687664041384, -0.3690944881889765550, -0.3153832671262227771 ) ) ;
#40136 = CARTESIAN_POINT ( 'NONE',  ( -0.1049643490035307020, 0.3917322834645669549, -0.9435695538057740084 ) ) ;
#40137 = CARTESIAN_POINT ( 'NONE',  ( -1.725721784776902190, -0.05778040916215522460, 0.4822834645669289988 ) ) ;
#40138 = CARTESIAN_POINT ( 'NONE',  ( 0.1958661417322834497, 0.3392501089628018329, -0.06690981807642862322 ) ) ;
#40139 = CARTESIAN_POINT ( 'NONE',  ( 0.6430446194225729606, -0.4281496062992127816, -0.4176697321401328100 ) ) ;
#40140 = CARTESIAN_POINT ( 'NONE',  ( -0.2952755905511804668, 0.07958543189024085140, 0.2665933059059887866 ) ) ;
#40141 = CARTESIAN_POINT ( 'NONE',  ( 0.7020997375328090762, -0.05778040916215560624, -0.4822834645669293319 ) ) ;
#40142 = CARTESIAN_POINT ( 'NONE',  ( 0.4265091863517067039, -0.6692913385826773087, -0.1292274648535924053 ) ) ;
#40143 = CARTESIAN_POINT ( 'NONE',  ( -0.4670044181572561293, 1.622388320715300702, -2.152632970815978375 ) ) ;
#40144 = CARTESIAN_POINT ( 'NONE',  ( -0.1070741851644051862, -0.3996062992125987146, -2.434383202099737353 ) ) ;
#40145 = CARTESIAN_POINT ( 'NONE',  ( 0.1958661417322836718, -0.3392501089628017219, -1.348444512632232861 ) ) ;
#40146 = CARTESIAN_POINT ( 'NONE',  ( 1.167979002624672580, -0.4281496062992124485, 0.4176697321401328655 ) ) ;
#40147 = CARTESIAN_POINT ( 'NONE',  ( -0.09186351706036689768, 0.05413385826771626580, -0.4176697321401330321 ) ) ;
#40148 = CARTESIAN_POINT ( 'NONE',  ( 0.3018372703412079971, -0.4281496062992124485, 0.4176697321401328655 ) ) ;
#40149 = CARTESIAN_POINT ( 'NONE',  ( -1.607611548556429737, 0.2952755905511810774, -0.1292274648535930714 ) ) ;
#40150 = CARTESIAN_POINT ( 'NONE',  ( 1.049868766404200349, 0.2306618581243848609, 0.2411417322834645549 ) ) ;
#40151 = CARTESIAN_POINT ( 'NONE',  ( 0.3392501089628018329, 0.1958661417322835607, -0.6883202099737534274 ) ) ;
#40152 = CARTESIAN_POINT ( 'NONE',  ( 0.01312335958005323398, 0.05413385826771666132, 0.4176697321401328100 ) ) ;
#40153 = CARTESIAN_POINT ( 'NONE',  ( 0.5380577427821529035, -0.4281496062992124485, 0.4176697321401328655 ) ) ;
#40154 = CARTESIAN_POINT ( 'NONE',  ( 0.09842519685039434474, 0.1660481256975885056, 0.3530559997133364547 ) ) ;
#40155 = CARTESIAN_POINT ( 'NONE',  ( 1.174540682414699111, -0.2845877964562159024, 0.3641732283464567677 ) ) ;
#40156 = CARTESIAN_POINT ( 'NONE',  ( -1.279527559055116948, -0.5400638737290844871, 0.3530559997133364547 ) ) ;
#40157 = CARTESIAN_POINT ( 'NONE',  ( -1.233595800524933894, 0.2306618581243848609, 0.2411417322834645549 ) ) ;
#40158 = CARTESIAN_POINT ( 'NONE',  ( 0.9120734908136489683, -0.6692913385826771977, 0.1292274648535927661 ) ) ;
#40159 = CARTESIAN_POINT ( 'NONE',  ( 0.2643935821223346028, -0.2898214735613004467, -1.929133858267716439 ) ) ;
#40160 = CARTESIAN_POINT ( 'NONE',  ( -0.3392501089628019995, 0.1958661417322832277, -1.908136482939632561 ) ) ;
#40161 = ORIENTED_EDGE ( 'NONE', *, *, #40891, .F. ) ;
#40162 = CARTESIAN_POINT ( 'NONE',  ( 0.1998031496062992740, 0.3460692066303959757, -0.6167979002624671692 ) ) ;
#40163 = VERTEX_POINT ( 'NONE', #42024 ) ;
#40164 = CARTESIAN_POINT ( 'NONE',  ( 1.003937007874016407, -0.5400638737290844871, 0.3530559997133364547 ) ) ;
#40165 = CARTESIAN_POINT ( 'NONE',  ( 0.9514435695538062676, -0.08942795157527998196, 0.3641732283464567121 ) ) ;
#40166 = CARTESIAN_POINT ( 'NONE',  ( 1.141392835773559211, 0.3937007874015748254, 0.9642274814428540841 ) ) ;
#40167 = CARTESIAN_POINT ( 'NONE',  ( -0.4732412630952499977, 1.503056026428865710, 2.557127100491988880 ) ) ;
#40168 = CARTESIAN_POINT ( 'NONE',  ( 0.3458507752293908943, -0.3458507752293908943, -1.200787401574802793 ) ) ;
#40169 = CARTESIAN_POINT ( 'NONE',  ( -0.3917322834645670104, -7.196005306013484475E-17, -1.226377952755905776 ) ) ;
#40170 = CARTESIAN_POINT ( 'NONE',  ( 1.404199475065617264, -0.4281496062992124485, 0.4176697321401328655 ) ) ;
#40171 = CARTESIAN_POINT ( 'NONE',  ( -3.937007874015748143, 2.165354330708661568, 0.3149606299212595606 ) ) ;
#40172 = CARTESIAN_POINT ( 'NONE',  ( -0.4002624671916004129, -0.05778040916215560624, -0.4822834645669293319 ) ) ;
#40173 = CARTESIAN_POINT ( 'NONE',  ( 1.253280839895013710, -0.3162353388693405765, 0.4822834645669290543 ) ) ;
#40174 = ORIENTED_EDGE ( 'NONE', *, *, #60737, .T. ) ;
#40175 = CARTESIAN_POINT ( 'NONE',  ( -1.456692913385826182, -0.6692913385826771977, 8.415575281601705876E-17 ) ) ;
#40176 = CARTESIAN_POINT ( 'NONE',  ( 1.614173228346456712, 1.496062992125984481, 0.1372047244094478646 ) ) ;
#40177 = DIRECTION ( 'NONE',  ( -3.491481338843133355E-15, 0.000000000000000000, 1.000000000000000000 ) ) ;
#40178 = CARTESIAN_POINT ( 'NONE',  ( -1.646051170424378096, -0.1870078740157480046, 1.254653134982923898E-17 ) ) ;
#40179 = DIRECTION ( 'NONE',  ( 0.000000000000000000, 0.000000000000000000, -1.000000000000000000 ) ) ;
#40180 = CARTESIAN_POINT ( 'NONE',  ( -0.9120734908136475250, -0.5511811023622048555, -0.09757992244046775898 ) ) ;
#40181 = CARTESIAN_POINT ( 'NONE',  ( -1.463254593175852492, 0.2952755905511811885, 0.1292274648535926551 ) ) ;
#40182 = CARTESIAN_POINT ( 'NONE',  ( 0.6758530183727039509, -0.6692913385826771977, 0.1292274648535927661 ) ) ;
#40183 = VERTEX_POINT ( 'NONE', #55059 ) ;
#40185 = CARTESIAN_POINT ( 'NONE',  ( 2.362204724409448620, 0.03937007874015751446, 8.247593713802677664E-15 ) ) ;
#40184 = CARTESIAN_POINT ( 'NONE',  ( 0.1265901696524990572, -0.4724409448818897017, -2.524278215223096478 ) ) ;
#40186 =( BOUNDED_CURVE ( )  B_SPLINE_CURVE ( 1, ( #36692, #43404 ),
 .UNSPECIFIED., .F., .F. ) 
 B_SPLINE_CURVE_WITH_KNOTS ( ( 2, 2 ),
 ( 0.000000000000000000, 0.002000000000000003511 ),
 .UNSPECIFIED. ) 
 CURVE ( )  GEOMETRIC_REPRESENTATION_ITEM ( )  RATIONAL_B_SPLINE_CURVE ( ( 0.9875488213027523443, 0.9875488213027523443 ) ) 
 REPRESENTATION_ITEM ( '' )  );
#40187 = CARTESIAN_POINT ( 'NONE',  ( 0.9580052493438327987, -0.4281496062992127816, -0.4176697321401328100 ) ) ;
#40188 = CARTESIAN_POINT ( 'NONE',  ( -1.581364829396324945, -0.3162353388693405765, 0.4822834645669290543 ) ) ;
#40189 = CARTESIAN_POINT ( 'NONE',  ( 4.797336870675655290E-17, -0.3917322834645669549, -1.103655224900575993 ) ) ;
#40190 = CARTESIAN_POINT ( 'NONE',  ( -0.6430446194225716283, -0.3690944881889763329, 0.3153832671262228327 ) ) ;
#40191 = EDGE_CURVE ( 'NONE', #64262, #12714, #20106, .T. ) ;
#40192 = CARTESIAN_POINT ( 'NONE',  ( 1.614173228346457378, -0.6692913385826771977, 8.415575281601705876E-17 ) ) ;
#40193 = LINE ( 'NONE', #14118, #6143 ) ;
#40194 = CARTESIAN_POINT ( 'NONE',  ( 0.6627296587926515548, 0.2952755905511811885, 0.1292274648535926551 ) ) ;
#40195 = CARTESIAN_POINT ( 'NONE',  ( -0.8923884514435688198, -0.5023911411419708095, 0.1820866141732285504 ) ) ;
#40196 = CARTESIAN_POINT ( 'NONE',  ( -0.4855643044619415427, -0.3690944881889763329, 0.3153832671262228327 ) ) ;
#40197 = CARTESIAN_POINT ( 'NONE',  ( -0.3346456692913377662, -0.5400638737290844871, 0.3530559997133364547 ) ) ;
#40198 = CARTESIAN_POINT ( 'NONE',  ( -1.069553805774277722, -0.5511811023622048555, -0.09757992244046775898 ) ) ;
#40199 = CARTESIAN_POINT ( 'NONE',  ( -0.1958661417322833942, -0.3392501089628018884, 0.09512504117354141087 ) ) ;
#40200 = CARTESIAN_POINT ( 'NONE',  ( 0.8136482939632553313, 0.2306618581243848609, 0.2411417322834645549 ) ) ;
#40201 = CARTESIAN_POINT ( 'NONE',  ( 0.8761506516392508770, -4.927456884911482678E-16, 0.4445507791589062840 ) ) ;
#40202 = CARTESIAN_POINT ( 'NONE',  ( 0.1265901696524990294, -0.4724409448818896462, -1.421916010498687877 ) ) ;
#40203 = CARTESIAN_POINT ( 'NONE',  ( -0.7742782152230965886, 0.05413385826771666132, 0.4176697321401328100 ) ) ;
#40204 = AXIS2_PLACEMENT_3D ( 'NONE', #13991, #13155, #70802 ) ;
#40205 = CARTESIAN_POINT ( 'NONE',  ( -0.05249343832020938322, -0.5023911411419708095, -0.1820866141732282451 ) ) ;
#40206 = CARTESIAN_POINT ( 'NONE',  ( -1.345144356955379816, -0.3162353388693405765, 0.4822834645669290543 ) ) ;
#40207 = CARTESIAN_POINT ( 'NONE',  ( 0.6758530183727039509, -0.5511811023622046335, 0.09757992244046803654 ) ) ;
#40208 = CARTESIAN_POINT ( 'NONE',  ( -0.6955380577427815458, -0.3690944881889765550, -0.3153832671262227771 ) ) ;
#40209 = CARTESIAN_POINT ( 'NONE',  ( -1.161417322834644716, -0.5400638737290845981, -0.3530559997133363437 ) ) ;
#40210 = CARTESIAN_POINT ( 'NONE',  ( -1.653543307086613234, -0.1870078740157480879, -0.4822834645669291653 ) ) ;
#40211 = CARTESIAN_POINT ( 'NONE',  ( -1.391076115485563314, -0.6046776061558809534, -0.2411417322834644161 ) ) ;
#40212 = CARTESIAN_POINT ( 'NONE',  ( 1.076115485564305141, 0.1539470093639521697, -0.1968503937007875793 ) ) ;
#40213 = CARTESIAN_POINT ( 'NONE',  ( 1.023622047244095334, -0.1870078740157479769, 0.3641732283464567677 ) ) ;
#40214 = CARTESIAN_POINT ( 'NONE',  ( 0.3937007874015754361, -0.1870078740157479769, 0.4822834645669291653 ) ) ;
#40215 = LINE ( 'NONE', #73033, #56875 ) ;
#40216 = CARTESIAN_POINT ( 'NONE',  ( 1.266404199475066328, -0.08942795157527998196, 0.3641732283464567121 ) ) ;
#40217 = ORIENTED_EDGE ( 'NONE', *, *, #43371, .T. ) ;
#40218 = CARTESIAN_POINT ( 'NONE',  ( -0.3996062992125986590, 0.1070741851644051723, -2.629265091863517423 ) ) ;
#40219 = CARTESIAN_POINT ( 'NONE',  ( -1.332020997375327642, -0.08942795157527998196, 0.3641732283464567121 ) ) ;
#40220 = CARTESIAN_POINT ( 'NONE',  ( -0.5839895013123351797, -0.6692913385826771977, 0.1292274648535927661 ) ) ;
#40221 = CARTESIAN_POINT ( 'NONE',  ( 0.8267716535433077274, 0.2952755905511811885, 0.000000000000000000 ) ) ;
#40222 = CARTESIAN_POINT ( 'NONE',  ( -1.548556430446193399, 0.1283753931104748280, 0.1820866141732283561 ) ) ;
#40223 = CARTESIAN_POINT ( 'NONE',  ( 0.2925321140481932369, -0.2925321140481931814, -1.592519685039370358 ) ) ;
#40224 = CARTESIAN_POINT ( 'NONE',  ( -1.614173228346456268, -0.6692913385826771977, 8.415575281601705876E-17 ) ) ;
#40225 = CARTESIAN_POINT ( 'NONE',  ( 0.6364829396325465405, -0.3162353388693409650, -0.4822834645669289433 ) ) ;
#40226 = CARTESIAN_POINT ( 'NONE',  ( 0.3412073490813655186, -0.6046776061558809534, -0.2411417322834644161 ) ) ;
#40227 = CARTESIAN_POINT ( 'NONE',  ( 1.030183727034121421, -0.3162353388693409650, -0.4822834645669289433 ) ) ;
#40228 = CARTESIAN_POINT ( 'NONE',  ( -0.1998031496062994405, 0.3460692066303957537, -0.8772965879265091083 ) ) ;
#40229 = CARTESIAN_POINT ( 'NONE',  ( 0.1070741851644053527, 0.3996062992125986590, -1.410761154855643129 ) ) ;
#40230 = CARTESIAN_POINT ( 'NONE',  ( -0.3949938075777409963, -7.255918531996591613E-17, -0.6692913385826770867 ) ) ;
#40231 = CARTESIAN_POINT ( 'NONE',  ( 3.937007874015748143, 2.559055118110236560, -0.5314960629921260393 ) ) ;
#40232 = CARTESIAN_POINT ( 'NONE',  ( 0.1706036745406830368, -0.004921259842519576551, 0.3153832671262227771 ) ) ;
#40233 = CARTESIAN_POINT ( 'NONE',  ( -0.4133858267716528645, 0.1660481256975883668, -0.3530559997133364547 ) ) ;
#40234 = CARTESIAN_POINT ( 'NONE',  ( 1.279527559055118724, 0.1660481256975885056, 0.3530559997133364547 ) ) ;
#40235 = CARTESIAN_POINT ( 'NONE',  ( -9.674558042662122972E-17, 0.3949938075777409963, -1.651574803149606474 ) ) ;
#40236 = CARTESIAN_POINT ( 'NONE',  ( 0.2821522309711292364, 0.1771653543307087075, -0.09757992244046823083 ) ) ;
#40237 = CARTESIAN_POINT ( 'NONE',  ( -0.7217847769028863381, -0.4281496062992124485, 0.4176697321401328655 ) ) ;
#40238 = CARTESIAN_POINT ( 'NONE',  ( -1.627296587926508442, 0.2306618581243848609, 0.2411417322834645549 ) ) ;
#40239 = CARTESIAN_POINT ( 'NONE',  ( 0.3674540682414705883, -0.6046776061558807314, 0.2411417322834647770 ) ) ;
#40240 = CARTESIAN_POINT ( 'NONE',  ( 0.4724409448818896462, 0.1265901696524990294, -2.171916010498687211 ) ) ;
#40241 = CARTESIAN_POINT ( 'NONE',  ( 1.614173228346457378, 1.330640075373405118, 0.1372047244094478369 ) ) ;
#40242 = EDGE_LOOP ( 'NONE', ( #64605, #66277, #36445, #16995 ) ) ;
#40243 = ORIENTED_EDGE ( 'NONE', *, *, #14729, .F. ) ;
#40244 = CARTESIAN_POINT ( 'NONE',  ( 1.581364829396326277, -0.08942795157527998196, 0.3641732283464567121 ) ) ;
#40246 = CARTESIAN_POINT ( 'NONE',  ( -0.9711286089238838626, 0.2306618581243847221, -0.2411417322834647770 ) ) ;
#40245 = CARTESIAN_POINT ( 'NONE',  ( -1.082677165354329896, -0.4536011799217368745, -0.2665933059059886201 ) ) ;
#40247 = CARTESIAN_POINT ( 'NONE',  ( 0.3917322834645669549, 2.398668435337827645E-17, -2.560348138286403064 ) ) ;
#40248 = LINE ( 'NONE', #65931, #51762 ) ;
#40249 = CARTESIAN_POINT ( 'NONE',  ( 1.686351706036745890, 0.2952755905511811885, 0.1292274648535926551 ) ) ;
#40250 = CARTESIAN_POINT ( 'NONE',  ( -1.377952755905511140, 0.2952755905511811885, 0.000000000000000000 ) ) ;
#40251 = CARTESIAN_POINT ( 'NONE',  ( -0.08530183727034056085, -0.05778040916215560624, -0.4822834645669293319 ) ) ;
#40252 = EDGE_CURVE ( 'NONE', #66145, #4806, #23082, .T. ) ;
#40253 = CARTESIAN_POINT ( 'NONE',  ( -1.187664041994749731, -0.3162353388693405765, 0.4822834645669290543 ) ) ;
#40254 = CARTESIAN_POINT ( 'NONE',  ( 0.3392501089628018884, -0.1958661417322834220, 0.1253280839895012100 ) ) ;
#40255 = CARTESIAN_POINT ( 'NONE',  ( 0.6430446194225728496, 0.05413385826771666132, 0.4176697321401328100 ) ) ;
#40256 = CARTESIAN_POINT ( 'NONE',  ( -0.3917322834645669549, -0.1049643490035306603, -1.927821522309711044 ) ) ;
#40257 = CARTESIAN_POINT ( 'NONE',  ( -1.246719160104985846, -0.3690944881889765550, -0.3153832671262227771 ) ) ;
#40258 = ORIENTED_EDGE ( 'NONE', *, *, #47021, .F. ) ;
#40259 = CARTESIAN_POINT ( 'NONE',  ( -0.3949938075777409963, -7.255918531996591613E-17, -2.244094488188976388 ) ) ;
#40260 = VERTEX_POINT ( 'NONE', #55468 ) ;
#40261 = CARTESIAN_POINT ( 'NONE',  ( -1.409919628453981888, 1.316123991182629460, 0.4200987300965431936 ) ) ;
#40262 = CARTESIAN_POINT ( 'NONE',  ( -0.9776902887139098386, -0.6692913385826771977, 0.1292274648535927661 ) ) ;
#40263 = CARTESIAN_POINT ( 'NONE',  ( -1.489501312335957062, -0.05778040916215522460, 0.4822834645669289988 ) ) ;
#40264 = CARTESIAN_POINT ( 'NONE',  ( -0.1998031496062991907, -0.3460692066303959757, -0.6955380577427822120 ) ) ;
#40265 = CARTESIAN_POINT ( 'NONE',  ( -1.725721784776902190, -0.05778040916215522460, 0.4822834645669289988 ) ) ;
#40266 = CARTESIAN_POINT ( 'NONE',  ( -0.7276493853111294374, 2.362204724409448620, 0.5105987775586408040 ) ) ;
#40267 = CARTESIAN_POINT ( 'NONE',  ( -1.489501312335957062, -0.05778040916215522460, 0.4822834645669289988 ) ) ;
#40268 = DIRECTION ( 'NONE',  ( 0.000000000000000000, 1.000000000000000000, -1.224646799147353207E-16 ) ) ;
#40269 = DIRECTION ( 'NONE',  ( 0.000000000000000000, 0.000000000000000000, -1.000000000000000000 ) ) ;
#40270 = CARTESIAN_POINT ( 'NONE',  ( 0.03280839895013198948, -0.5511811023622048555, -0.09757992244046775898 ) ) ;
#40271 = CARTESIAN_POINT ( 'NONE',  ( 0.2867679344610365999, 0.2867679344610365999, -0.6948818897637795144 ) ) ;
#40272 = CARTESIAN_POINT ( 'NONE',  ( -0.8333333333333323711, -0.5511811023622048555, -0.09757992244046775898 ) ) ;
#40273 = CARTESIAN_POINT ( 'NONE',  ( -1.154855643044618851, 0.2306618581243848609, 0.2411417322834645549 ) ) ;
#40274 = CARTESIAN_POINT ( 'NONE',  ( 0.9645669291338588858, 0.1660481256975885056, 0.3530559997133364547 ) ) ;
#40275 = CARTESIAN_POINT ( 'NONE',  ( -0.9842519685039360366, 0.2952755905511811885, 0.000000000000000000 ) ) ;
#40276 = CARTESIAN_POINT ( 'NONE',  ( -9.594673741351313045E-17, 0.3917322834645670104, 0.1653543307086614844 ) ) ;
#40277 = ORIENTED_EDGE ( 'NONE', *, *, #21499, .T. ) ;
#40278 = CARTESIAN_POINT ( 'NONE',  ( -0.8136482939632537770, 0.2306618581243847221, -0.2411417322834647770 ) ) ;
#40279 = CARTESIAN_POINT ( 'NONE',  ( 1.069553805774278610, -0.6692913385826771977, 0.1292274648535927661 ) ) ;
#40280 = EDGE_CURVE ( 'NONE', #33111, #40878, #39315, .T. ) ;
#40281 = CARTESIAN_POINT ( 'NONE',  ( -1.653543307086613234, -0.1870078740157480601, -0.3641732283464567677 ) ) ;
#40282 = CARTESIAN_POINT ( 'NONE',  ( -1.660104986876639543, -0.05778040916215560624, -0.4822834645669293319 ) ) ;
#40283 = CARTESIAN_POINT ( 'NONE',  ( 0.4091458600556403535, 0.2362204724409449896, -1.233595800524934338 ) ) ;
#40284 = LINE ( 'NONE', #12024, #45204 ) ;
#40285 = EDGE_CURVE ( 'NONE', #50981, #29775, #59237, .T. ) ;
#40286 = CARTESIAN_POINT ( 'NONE',  ( 0.1049643490035303689, 0.3917322834645670104, -0.4580052493438320216 ) ) ;
#40287 = CARTESIAN_POINT ( 'NONE',  ( -0.2867679344610366554, 0.2867679344610365444, -2.466535433070866201 ) ) ;
#40288 = CARTESIAN_POINT ( 'NONE',  ( -0.4921259842519677963, 0.1660481256975883668, -0.3530559997133364547 ) ) ;
#40289 = CARTESIAN_POINT ( 'NONE',  ( -1.528871391076114250, -0.5511811023622046335, 0.09757992244046803654 ) ) ;
#40290 = CARTESIAN_POINT ( 'NONE',  ( 0.1070741851644053388, 0.3996062992125986035, 0.08727034120734902811 ) ) ;
#40292 = DIRECTION ( 'NONE',  ( 0.000000000000000000, 0.000000000000000000, 1.000000000000000000 ) ) ;
#40291 = CARTESIAN_POINT ( 'NONE',  ( -1.240157480314959759, 0.1660481256975885056, 0.3530559997133364547 ) ) ;
#40293 = CARTESIAN_POINT ( 'NONE',  ( -1.456692913385826182, -0.6692913385826771977, 8.415575281601705876E-17 ) ) ;
#40294 = CARTESIAN_POINT ( 'NONE',  ( -0.5708661417322828946, 0.1660481256975883668, -0.3530559997133364547 ) ) ;
#40295 = CARTESIAN_POINT ( 'NONE',  ( -0.2891555358219911054, 0.2891555358219909388, -2.458661417322835163 ) ) ;
#40296 = CARTESIAN_POINT ( 'NONE',  ( 0.4986876640419954376, 0.1283753931104748280, 0.1820866141732283561 ) ) ;
#40297 = CARTESIAN_POINT ( 'NONE',  ( -1.113061397484513604, -4.850200619981615293E-15, -0.4118477457932993024 ) ) ;
#40298 = CARTESIAN_POINT ( 'NONE',  ( 0.2493438320209980519, -0.004921259842519576551, 0.3153832671262227771 ) ) ;
#40299 = CARTESIAN_POINT ( 'NONE',  ( 1.430446194225722500, -0.004921259842519576551, 0.3153832671262227771 ) ) ;
#40300 = CARTESIAN_POINT ( 'NONE',  ( 0.7677165354330716118, -0.5400638737290844871, 0.3530559997133364547 ) ) ;
#40301 = PRODUCT_DEFINITION_CONTEXT ( 'detailed design', #56779, 'design' ) ;
#40302 = CARTESIAN_POINT ( 'NONE',  ( -0.03280839895013062252, 0.1771653543307087075, -0.09757992244046823083 ) ) ;
#40303 = CARTESIAN_POINT ( 'NONE',  ( -0.1049643490035307020, 0.3917322834645669549, -2.045931758530183497 ) ) ;
#40304 = CARTESIAN_POINT ( 'NONE',  ( -1.161417322834644716, 0.1660481256975885056, 0.3530559997133364547 ) ) ;
#40305 = CARTESIAN_POINT ( 'NONE',  ( 5.463695987328526437E-16, -0.1870078740157479769, 0.3641732283464567677 ) ) ;
#40306 = CARTESIAN_POINT ( 'NONE',  ( -1.489501312335957062, -0.08942795157527998196, 0.3641732283464567121 ) ) ;
#40307 = CARTESIAN_POINT ( 'NONE',  ( 0.4091458600556404646, -0.2362204724409448231, -0.3392388451443569819 ) ) ;
#40308 = CARTESIAN_POINT ( 'NONE',  ( -0.3608923884514428360, 0.1771653543307087630, 0.09757992244046791164 ) ) ;
#40309 = B_SPLINE_CURVE_WITH_KNOTS ( 'NONE', 3,
 ( #42593, #68293, #60715, #67876, #80923, #9379, #42997, #61958, #4298, #41365, #29961, #4702, #75021, #48489, #16952, #73781, #10213, #54392, #55626, #16117, #47665, #67046 ),
 .UNSPECIFIED., .F., .F.,
 ( 4, 2, 2, 2, 2, 2, 2, 2, 2, 2, 4 ),
 ( 0.000000000000000000, 0.002126047124880315557, 0.003189070687320475720, 0.003720582468540548429, 0.004252094249760621572, 0.005315117812200776531, 0.005846629593420847940, 0.006378141374640921082, 0.006909653155860992491, 0.007441164937081065633, 0.008504188499521210184 ),
 .UNSPECIFIED. ) ;
#40310 = DIRECTION ( 'NONE',  ( 0.000000000000000000, 0.000000000000000000, 1.000000000000000000 ) ) ;
#40311 = CARTESIAN_POINT ( 'NONE',  ( -0.1968503937007867743, 0.2952755905511811885, 0.000000000000000000 ) ) ;
#40312 = DIRECTION ( 'NONE',  ( 0.000000000000000000, 1.000000000000000000, -1.224646799147353207E-16 ) ) ;
#40313 = CARTESIAN_POINT ( 'NONE',  ( 0.3674540682414705883, 0.1283753931104746893, -0.1820866141732285504 ) ) ;
#40314 = CARTESIAN_POINT ( 'NONE',  ( -0.2821522309711278487, 0.1771653543307087630, 0.09757992244046791164 ) ) ;
#40315 = CARTESIAN_POINT ( 'NONE',  ( -0.3674540682414689785, 0.2306618581243848609, 0.2411417322834645549 ) ) ;
#40316 = DIRECTION ( 'NONE',  ( 0.000000000000000000, 0.000000000000000000, -1.000000000000000000 ) ) ;
#40317 = CARTESIAN_POINT ( 'NONE',  ( -1.043307086614172041, -0.4536011799217367080, 0.2665933059059888421 ) ) ;
#40318 = CARTESIAN_POINT ( 'NONE',  ( -1.382164990278195615, 1.299212598425196985, 0.4102808022082835571 ) ) ;
#40319 = CARTESIAN_POINT ( 'NONE',  ( 0.7545931758530189937, 0.2952755905511810774, -0.1292274648535930714 ) ) ;
#40320 = CARTESIAN_POINT ( 'NONE',  ( -0.8792650918635160906, -0.4281496062992124485, 0.4176697321401328655 ) ) ;
#40321 = CARTESIAN_POINT ( 'NONE',  ( -0.3996062992125985480, -7.340648628747423112E-17, -1.533464566929133799 ) ) ;
#40322 =( BOUNDED_CURVE ( )  B_SPLINE_CURVE ( 2, ( #47382, #8685, #2376, #2788, #48218, #74324, #28448, #54944, #16254, #73501, #15849, #3199, #28863 ),
 .UNSPECIFIED., .F., .F. ) 
 B_SPLINE_CURVE_WITH_KNOTS ( ( 3, 2, 2, 2, 2, 2, 3 ),
 ( 0.8125000000000000000, 0.8166666666666666519, 0.8208333333333333037, 0.8249999999999999556, 0.8291666666666667185, 0.8333333333333333703, 0.8375000000000000222 ),
 .UNSPECIFIED. ) 
 CURVE ( )  GEOMETRIC_REPRESENTATION_ITEM ( )  RATIONAL_B_SPLINE_CURVE ( ( 1.000000000000000000, 0.9659258262890683122, 1.000000000000000000, 0.9659258262890683122, 1.000000000000000000, 0.9659258262890683122, 1.000000000000000000, 0.9659258262890683122, 1.000000000000000000, 0.9659258262890683122, 1.000000000000000000, 0.9659258262890683122, 1.000000000000000000 ) ) 
 REPRESENTATION_ITEM ( '' )  );
#40323 = CARTESIAN_POINT ( 'NONE',  ( -0.3392501089628017219, -0.1958661417322836718, -2.814304461942257252 ) ) ;
#40324 = CARTESIAN_POINT ( 'NONE',  ( -0.3740157480314953431, -0.4536011799217368745, -0.2665933059059886201 ) ) ;
#40325 = FACE_OUTER_BOUND ( 'NONE', #3287, .T. ) ;
#40326 = CARTESIAN_POINT ( 'NONE',  ( -1.076115485564303809, -0.5023911411419708095, -0.1820866141732282451 ) ) ;
#40327 = CARTESIAN_POINT ( 'NONE',  ( 0.5120078740157480990, 0.000000000000000000, -1.512162153811850596 ) ) ;
#40328 = CARTESIAN_POINT ( 'NONE',  ( -0.8858267716535425107, 0.07958543189024071263, -0.2665933059059888421 ) ) ;
#40329 = CARTESIAN_POINT ( 'NONE',  ( -1.091264520429692464, -2.570477104772672414E-15, 0.3954974714151479609 ) ) ;
#40330 = CARTESIAN_POINT ( 'NONE',  ( 0.9317585301837276734, -0.4281496062992124485, 0.4176697321401328655 ) ) ;
#40331 = CARTESIAN_POINT ( 'NONE',  ( 0.1998031496062994405, -0.3460692066303958092, 0.06561679790026245240 ) ) ;
#40332 = CARTESIAN_POINT ( 'NONE',  ( -0.1958661417322836995, 0.3392501089628017219, -2.687027189797587035 ) ) ;
#40333 = CARTESIAN_POINT ( 'NONE',  ( -3.826707563893392283, 2.755905511811024500, -0.5314960629921261503 ) ) ;
#40334 = CARTESIAN_POINT ( 'NONE',  ( 1.430446194225722500, -0.004921259842519576551, 0.3153832671262227771 ) ) ;
#40335 = CARTESIAN_POINT ( 'NONE',  ( -1.423884514435694859, -0.3162353388693405765, 0.4822834645669290543 ) ) ;
#40336 = EDGE_CURVE ( 'NONE', #72978, #50169, #11716, .T. ) ;
#40337 = CARTESIAN_POINT ( 'NONE',  ( 1.292650918635171564, 0.2952755905511811885, 0.1292274648535926551 ) ) ;
#40338 = CARTESIAN_POINT ( 'NONE',  ( 0.3917322834645669549, 0.1049643490035304660, -2.256561679790026531 ) ) ;
#40339 = CARTESIAN_POINT ( 'NONE',  ( 1.568241469816273659, -0.08942795157528024563, -0.3641732283464568787 ) ) ;
#40340 = CARTESIAN_POINT ( 'NONE',  ( 0.6627296587926517768, -0.6692913385826773087, -0.1292274648535924053 ) ) ;
#40341 = CARTESIAN_POINT ( 'NONE',  ( -0.4461942257217840213, -0.6046776061558809534, -0.2411417322834644161 ) ) ;
#40342 = CARTESIAN_POINT ( 'NONE',  ( 1.528871391076116026, 0.2952755905511811885, 0.1292274648535926551 ) ) ;
#40343 = CARTESIAN_POINT ( 'NONE',  ( -0.2925321140481930704, -0.2925321140481933480, -2.106299212598425008 ) ) ;
#40344 = CARTESIAN_POINT ( 'NONE',  ( 0.5643044619422579178, -0.3690944881889765550, -0.3153832671262227771 ) ) ;
#40345 = CARTESIAN_POINT ( 'NONE',  ( 0.1998031496062992740, 0.3460692066303959757, -1.876640419947506411 ) ) ;
#40346 = EDGE_LOOP ( 'NONE', ( #36735, #37259, #13156, #1948, #25514 ) ) ;
#40347 = CARTESIAN_POINT ( 'NONE',  ( -0.1049643490035307158, 0.3917322834645670104, -0.3182607855981121059 ) ) ;
#40348 = ORIENTED_EDGE ( 'NONE', *, *, #60488, .T. ) ;
#40349 = CARTESIAN_POINT ( 'NONE',  ( -0.4855643044619415427, -0.4281496062992124485, 0.4176697321401328655 ) ) ;
#40350 = CARTESIAN_POINT ( 'NONE',  ( 1.325459317585302665, 0.05413385826771626580, -0.4176697321401330321 ) ) ;
#40351 = CARTESIAN_POINT ( 'NONE',  ( 0.1771653543307093182, -0.5400638737290845981, -0.3530559997133363437 ) ) ;
#40352 = CARTESIAN_POINT ( 'NONE',  ( -0.4855643044619415427, -0.004921259842519870586, -0.3153832671262229437 ) ) ;
#40353 = CARTESIAN_POINT ( 'NONE',  ( 1.318897637795276356, -0.5400638737290844871, 0.3530559997133364547 ) ) ;
#40354 = CARTESIAN_POINT ( 'NONE',  ( -1.095800524934382292, -0.3162353388693409650, -0.4822834645669289433 ) ) ;
#40355 = CARTESIAN_POINT ( 'NONE',  ( 0.07874015748031558404, -0.1870078740157480879, -0.4822834645669291653 ) ) ;
#40356 = CARTESIAN_POINT ( 'NONE',  ( -1.469816272965878357, 0.2306618581243848609, 0.2411417322834645549 ) ) ;
#40357 = CARTESIAN_POINT ( 'NONE',  ( 0.9120734908136489683, -0.6692913385826771977, 0.1292274648535927661 ) ) ;
#40358 = CARTESIAN_POINT ( 'NONE',  ( 1.325459317585302665, -0.4281496062992124485, 0.4176697321401328655 ) ) ;
#40359 = CARTESIAN_POINT ( 'NONE',  ( -0.3917322834645669549, -0.1049643490035306603, -0.5104986876640419391 ) ) ;
#40360 = CARTESIAN_POINT ( 'NONE',  ( -0.03280839895013062252, 0.1771653543307087075, -0.09757992244046823083 ) ) ;
#40361 = EDGE_LOOP ( 'NONE', ( #14692, #36114, #51214, #33095 ) ) ;
#40362 = CARTESIAN_POINT ( 'NONE',  ( 0.3420746716998660508, -0.1974969037888703871, -1.207349081364829324 ) ) ;
#40363 = EDGE_LOOP ( 'NONE', ( #17681, #6784, #49050, #70137 ) ) ;
#40364 = CARTESIAN_POINT ( 'NONE',  ( -0.3412073490813641308, -0.5023911411419708095, 0.1820866141732285504 ) ) ;
#40365 = CARTESIAN_POINT ( 'NONE',  ( 0.08530183727034192087, -0.05778040916215522460, 0.4822834645669289988 ) ) ;
#40366 = CARTESIAN_POINT ( 'NONE',  ( 2.846947862837586829, 1.092324130688943296, 0.1650676745531752254 ) ) ;
#40367 = CARTESIAN_POINT ( 'NONE',  ( -0.1640419947506555343, -0.3162353388693405765, 0.4822834645669290543 ) ) ;
#40368 = CARTESIAN_POINT ( 'NONE',  ( -0.2952755905511804668, 0.1660481256975885056, 0.3530559997133364547 ) ) ;
#40369 = CARTESIAN_POINT ( 'NONE',  ( -1.036745406824146176, -0.4281496062992124485, 0.4176697321401328655 ) ) ;
#40370 = CARTESIAN_POINT ( 'NONE',  ( -0.9055118110236215490, 0.2952755905511811885, 0.000000000000000000 ) ) ;
#40371 = CARTESIAN_POINT ( 'NONE',  ( 1.541994750656168645, 0.1771653543307087075, -0.09757992244046823083 ) ) ;
#40372 = CARTESIAN_POINT ( 'NONE',  ( -1.627296587926508442, 0.2306618581243848609, 0.2411417322834645549 ) ) ;
#40373 = CARTESIAN_POINT ( 'NONE',  ( 0.3215223097112867578, -0.08942795157527998196, 0.3641732283464567121 ) ) ;
#40374 = CARTESIAN_POINT ( 'NONE',  ( 0.6496062992125991586, -0.5400638737290845981, -0.3530559997133363437 ) ) ;
#40375 = CARTESIAN_POINT ( 'NONE',  ( 0.5052493438320218022, -0.6692913385826773087, -0.1292274648535924053 ) ) ;
#40376 = CARTESIAN_POINT ( 'NONE',  ( -9.787531504996567848E-17, 0.3996062992125986035, -1.102362204724409489 ) ) ;
#40377 = CARTESIAN_POINT ( 'NONE',  ( -1.699475065616797398, 0.2952755905511811885, 0.1292274648535926551 ) ) ;
#40378 = CARTESIAN_POINT ( 'NONE',  ( -0.3460692066303957537, -0.1998031496062994405, -0.7591863517060367661 ) ) ;
#40379 = CARTESIAN_POINT ( 'NONE',  ( -0.3996062992125985480, -7.340648628747423112E-17, -0.5885826771653542844 ) ) ;
#40380 = CARTESIAN_POINT ( 'NONE',  ( -0.5314960629921254842, -0.5400638737290845981, -0.3530559997133363437 ) ) ;
#40381 = CARTESIAN_POINT ( 'NONE',  ( -0.2362204724409447953, -0.4091458600556404646, -0.06561679790026246628 ) ) ;
#40382 = CARTESIAN_POINT ( 'NONE',  ( -0.2867679344610365999, 0.2867679344610364889, -1.994094488188976610 ) ) ;
#40383 = CARTESIAN_POINT ( 'NONE',  ( -1.358267716535432434, -0.4536011799217367080, 0.2665933059059888421 ) ) ;
#40384 = CARTESIAN_POINT ( 'NONE',  ( 0.8333333333333340365, 0.2952755905511810774, -0.1292274648535930714 ) ) ;
#40385 = CARTESIAN_POINT ( 'NONE',  ( 0.8727034120734913358, -0.05778040916215522460, 0.4822834645669289988 ) ) ;
#40386 = CARTESIAN_POINT ( 'NONE',  ( -0.1902887139107604098, 0.1771653543307087075, -0.09757992244046823083 ) ) ;
#40387 = CARTESIAN_POINT ( 'NONE',  ( 0.6561679790026253567, 0.2306618581243848609, 0.2411417322834645549 ) ) ;
#40388 = CARTESIAN_POINT ( 'NONE',  ( -0.3458507752293906723, -0.3458507752293910609, -2.025590551181101873 ) ) ;
#40389 = CARTESIAN_POINT ( 'NONE',  ( -0.1115485564304453947, -0.5511811023622046335, 0.09757992244046803654 ) ) ;
#40390 = CARTESIAN_POINT ( 'NONE',  ( 0.1049868766404206816, -0.6046776061558809534, -0.2411417322834644161 ) ) ;
#40391 = CARTESIAN_POINT ( 'NONE',  ( 0.3420746716998660508, -0.1974969037888704149, -1.599081364829396223 ) ) ;
#40392 = EDGE_CURVE ( 'NONE', #4444, #41297, #42158, .T. ) ;
#40393 = CARTESIAN_POINT ( 'NONE',  ( -1.509186351706035767, 0.05413385826771626580, -0.4176697321401330321 ) ) ;
#40394 = CARTESIAN_POINT ( 'NONE',  ( 0.5052493438320215802, 0.1771653543307087630, 0.09757992244046791164 ) ) ;
#40395 = CARTESIAN_POINT ( 'NONE',  ( 1.640419947506562393, -0.3690944881889763329, 0.3153832671262228327 ) ) ;
#40396 = CARTESIAN_POINT ( 'NONE',  ( -0.7480314960629914633, 0.2952755905511811885, 0.000000000000000000 ) ) ;
#40397 = AXIS2_PLACEMENT_3D ( 'NONE', #72607, #2736, #14955 ) ;
#40398 = CARTESIAN_POINT ( 'NONE',  ( -0.6364829396325453192, -0.08942795157528024563, -0.3641732283464568787 ) ) ;
#40399 = DIRECTION ( 'NONE',  ( 1.000000000000000000, -0.000000000000000000, -0.000000000000000000 ) ) ;
#40400 = CARTESIAN_POINT ( 'NONE',  ( -0.8661417322834640276, -0.1870078740157480879, -0.4822834645669291653 ) ) ;
#40401 = CARTESIAN_POINT ( 'NONE',  ( -0.6955380577427815458, 0.05413385826771666132, 0.4176697321401328100 ) ) ;
#40402 = CARTESIAN_POINT ( 'NONE',  ( -0.07217847769028787330, -0.05778040916215522460, 0.4822834645669289988 ) ) ;
#40403 = CARTESIAN_POINT ( 'NONE',  ( 0.3996062992125986035, -0.1070741851644052972, -2.550524934383202158 ) ) ;
#40404 = CARTESIAN_POINT ( 'NONE',  ( 4.797336870675655290E-17, -0.3917322834645669549, -2.048537114664355396 ) ) ;
#40405 = CARTESIAN_POINT ( 'NONE',  ( -2.153082335389848279, 1.453547212638083952, -0.4672029448317642775 ) ) ;
#40406 = CARTESIAN_POINT ( 'NONE',  ( 0.6692913385826778638, -0.5511811023622047445, 6.969142054262312111E-17 ) ) ;
#40407 = CARTESIAN_POINT ( 'NONE',  ( 1.358267716535433323, -0.5400638737290845981, -0.3530559997133363437 ) ) ;
#40408 = CARTESIAN_POINT ( 'NONE',  ( -1.181102362204723644, -0.1870078740157480601, -0.3641732283464567677 ) ) ;
#40409 = ADVANCED_FACE ( 'NONE', ( #30641 ), #17210, .T. ) ;
#40410 = CARTESIAN_POINT ( 'NONE',  ( -0.9645669291338575535, -0.4536011799217367080, 0.2665933059059888421 ) ) ;
#40411 = CARTESIAN_POINT ( 'NONE',  ( -0.6167979002624665030, 0.05413385826771666132, 0.4176697321401328100 ) ) ;
#40412 = CARTESIAN_POINT ( 'NONE',  ( -0.03937007874015669567, 0.1771653543307087630, 0.000000000000000000 ) ) ;
#40413 = LINE ( 'NONE', #80803, #79739 ) ;
#40414 = CARTESIAN_POINT ( 'NONE',  ( 0.9055118110236227702, -0.5511811023622047445, 6.969142054262312111E-17 ) ) ;
#40415 = EDGE_CURVE ( 'NONE', #50299, #53271, #26462, .T. ) ;
#40416 = CARTESIAN_POINT ( 'NONE',  ( 0.3018372703412079971, 0.05413385826771626580, -0.4176697321401330321 ) ) ;
#40417 = CARTESIAN_POINT ( 'NONE',  ( 0.2925321140481932369, -0.2925321140481931814, 0.1397637795275590289 ) ) ;
#40418 = CARTESIAN_POINT ( 'NONE',  ( -0.7349081364829390672, 0.2306618581243847221, -0.2411417322834647770 ) ) ;
#40419 = CARTESIAN_POINT ( 'NONE',  ( 0.2867679344610365999, -0.2867679344610365444, -1.442913385826771755 ) ) ;
#40420 = CARTESIAN_POINT ( 'NONE',  ( 1.528871391076116026, -0.5511811023622048555, -0.09757992244046775898 ) ) ;
#40421 = CARTESIAN_POINT ( 'NONE',  ( 0.3740157480314966754, -0.5400638737290844871, 0.3530559997133364547 ) ) ;
#40422 = CARTESIAN_POINT ( 'NONE',  ( 0.006561679790026889343, -0.3162353388693409650, -0.4822834645669289433 ) ) ;
#40423 = CARTESIAN_POINT ( 'NONE',  ( 0.1509186351706045259, -0.08942795157528024563, -0.3641732283464568787 ) ) ;
#40424 = CARTESIAN_POINT ( 'NONE',  ( 1.614173228346456712, 0.9921945702958890889, 0.1372047244094478646 ) ) ;
#40425 = CARTESIAN_POINT ( 'NONE',  ( -0.2427821522309703550, -0.2845877964562159024, 0.3641732283464567677 ) ) ;
#40426 = CARTESIAN_POINT ( 'NONE',  ( 0.7217847769028878924, 0.05413385826771666132, 0.4176697321401328100 ) ) ;
#40427 = CARTESIAN_POINT ( 'NONE',  ( -0.6889763779527552368, -0.4536011799217368745, -0.2665933059059886201 ) ) ;
#40428 = CARTESIAN_POINT ( 'NONE',  ( 0.3460692066303959202, -0.1998031496062991630, -0.9691601049868766582 ) ) ;
#40429 = CARTESIAN_POINT ( 'NONE',  ( -1.102362204724408601, -0.1870078740157480879, -0.4822834645669291653 ) ) ;
#40430 = LINE ( 'NONE', #60615, #81077 ) ;
#40431 = EDGE_LOOP ( 'NONE', ( #82884, #52468, #33844, #50572 ) ) ;
#40432 = CARTESIAN_POINT ( 'NONE',  ( -1.194225721784776262, -0.4281496062992124485, 0.4176697321401328655 ) ) ;
#40433 = CARTESIAN_POINT ( 'NONE',  ( -0.9842519685039365918, -0.5511811023622047445, 6.969142054262312111E-17 ) ) ;
#40434 = CARTESIAN_POINT ( 'NONE',  ( 0.05905511811023681640, 0.1660481256975883668, -0.3530559997133364547 ) ) ;
#40435 = EDGE_CURVE ( 'NONE', #9917, #58735, #26205, .T. ) ;
#40436 = CARTESIAN_POINT ( 'NONE',  ( -1.594488188976377563, -0.5400638737290844871, 0.3530559997133364547 ) ) ;
#40437 = CARTESIAN_POINT ( 'NONE',  ( -0.8989501312335946848, -0.6692913385826771977, 0.1292274648535927661 ) ) ;
#40438 = CARTESIAN_POINT ( 'NONE',  ( -3.937007874015748143, 1.724409448818897905, 0.4359958488159719758 ) ) ;
#40440 = CARTESIAN_POINT ( 'NONE',  ( 1.076115485564305141, -0.6046776061558807314, 0.2411417322834647770 ) ) ;
#40439 = CARTESIAN_POINT ( 'NONE',  ( 1.673228346456693494, 0.1660481256975885056, 0.3530559997133364547 ) ) ;
#40441 = CARTESIAN_POINT ( 'NONE',  ( 0.8923884514435703741, 0.2306618581243848609, 0.2411417322834645549 ) ) ;
#40442 = CARTESIAN_POINT ( 'NONE',  ( 0.1958661417322836440, -0.3392501089628017219, -2.446194225721784576 ) ) ;
#40443 = CARTESIAN_POINT ( 'NONE',  ( 1.515748031496063186, -0.5400638737290845981, -0.3530559997133363437 ) ) ;
#40444 = CARTESIAN_POINT ( 'NONE',  ( -1.181102362204723644, -0.1870078740157480879, -0.4822834645669291653 ) ) ;
#40445 = CARTESIAN_POINT ( 'NONE',  ( 0.3996062992125986590, -0.1070741851644053111, -0.5839895013123358458 ) ) ;
#40447 = EDGE_CURVE ( 'NONE', #82474, #62196, #8998, .T. ) ;
#40446 = ORIENTED_EDGE ( 'NONE', *, *, #21401, .F. ) ;
#40448 = CARTESIAN_POINT ( 'NONE',  ( -0.6036745406824141069, -0.5023911411419708095, -0.1820866141732282451 ) ) ;
#40449 = CARTESIAN_POINT ( 'NONE',  ( -0.3917322834645671215, 0.1049643490035301469, -2.387139107611548905 ) ) ;
#40450 = VERTEX_POINT ( 'NONE', #10876 ) ;
#40451 = CARTESIAN_POINT ( 'NONE',  ( 0.1902887139107617975, 0.2952755905511811885, 0.1292274648535926551 ) ) ;
#40452 = CARTESIAN_POINT ( 'NONE',  ( 0.07217847769028949700, -0.05778040916215560624, -0.4822834645669293319 ) ) ;
#40453 = CARTESIAN_POINT ( 'NONE',  ( -0.8333333333333323711, 0.2952755905511811885, 0.1292274648535926551 ) ) ;
#40454 = CARTESIAN_POINT ( 'NONE',  ( 1.338582677165355062, -0.1870078740157479769, 0.4822834645669291653 ) ) ;
#40455 = CARTESIAN_POINT ( 'NONE',  ( -0.8727034120734901146, -0.2845877964562159024, 0.3641732283464567677 ) ) ;
#40456 = CARTESIAN_POINT ( 'NONE',  ( -0.7461015470515859338, 2.206450217086253218, -0.5309055118110235227 ) ) ;
#40457 = CARTESIAN_POINT ( 'NONE',  ( 0.5971128608923891301, 0.2952755905511810774, -0.1292274648535930714 ) ) ;
#40458 = CARTESIAN_POINT ( 'NONE',  ( 0.6364829396325465405, -0.08942795157527998196, 0.3641732283464567121 ) ) ;
#40459 = AXIS2_PLACEMENT_3D ( 'NONE', #12105, #30630, #56295 ) ;
#40460 = CARTESIAN_POINT ( 'NONE',  ( -0.5249343832020990641, 0.2306618581243848609, 0.2411417322834645549 ) ) ;
#40461 = CARTESIAN_POINT ( 'NONE',  ( 0.2867679344610365999, 0.2867679344610365999, -1.162710343010812108 ) ) ;
#40462 = CARTESIAN_POINT ( 'NONE',  ( -1.364829396325458521, -0.6046776061558807314, 0.2411417322834647770 ) ) ;
#40463 = CARTESIAN_POINT ( 'NONE',  ( -1.732283464566928277, -0.1870078740157479769, 0.3641732283464567677 ) ) ;
#40464 = ADVANCED_FACE ( 'NONE', ( #36537 ), #33201, .F. ) ;
#40465 = CARTESIAN_POINT ( 'NONE',  ( 1.397637795275591177, 0.1660481256975883668, -0.3530559997133364547 ) ) ;
#40466 = CARTESIAN_POINT ( 'NONE',  ( 1.522309711286089939, 0.1283753931104748280, 0.1820866141732283561 ) ) ;
#40467 = ORIENTED_EDGE ( 'NONE', *, *, #17226, .T. ) ;
#40468 = CARTESIAN_POINT ( 'NONE',  ( -0.1049643490035307158, 0.3917322834645670104, -2.522985195046931306 ) ) ;
#40469 = CARTESIAN_POINT ( 'NONE',  ( -0.1115485564304453947, -0.6692913385826771977, 0.1292274648535927661 ) ) ;
#40470 = VERTEX_POINT ( 'NONE', #30221 ) ;
#40471 = CARTESIAN_POINT ( 'NONE',  ( 1.003937007874016185, 0.07958543189024071263, -0.2665933059059888421 ) ) ;
#40472 = CARTESIAN_POINT ( 'NONE',  ( -1.220472440944881054, 0.2952755905511811885, 0.000000000000000000 ) ) ;
#40473 = CARTESIAN_POINT ( 'NONE',  ( 1.095800524934383846, -0.3162353388693405765, 0.4822834645669290543 ) ) ;
#40474 = CARTESIAN_POINT ( 'NONE',  ( 1.332020997375328974, -0.05778040916215560624, -0.4822834645669293319 ) ) ;
#40475 = CARTESIAN_POINT ( 'NONE',  ( 0.1246719160104994284, -0.6692913385826771977, 0.1292274648535927661 ) ) ;
#40476 = CARTESIAN_POINT ( 'NONE',  ( -0.1902887139107604098, 0.2952755905511810774, -0.1292274648535930714 ) ) ;
#40477 = CARTESIAN_POINT ( 'NONE',  ( 0.1958661417322836440, -0.3392501089628017219, -1.751312335958005395 ) ) ;
#40478 = CARTESIAN_POINT ( 'NONE',  ( -1.220472440944881054, 0.2952755905511811885, 0.000000000000000000 ) ) ;
#40479 = CARTESIAN_POINT ( 'NONE',  ( -0.4396325459317577122, -0.6692913385826773087, -0.1292274648535924053 ) ) ;
#40480 = CARTESIAN_POINT ( 'NONE',  ( -0.4396325459317577122, -0.5511811023622048555, -0.09757992244046775898 ) ) ;
#40481 = CARTESIAN_POINT ( 'NONE',  ( 1.436417322834645294, 2.401574803149606474, -0.3149606299212598381 ) ) ;
#40482 = AXIS2_PLACEMENT_3D ( 'NONE', #34543, #35369, #2559 ) ;
#40483 = CARTESIAN_POINT ( 'NONE',  ( -0.3346456692913377662, -0.5400638737290844871, 0.3530559997133364547 ) ) ;
#40484 = LINE ( 'NONE', #66162, #70869 ) ;
#40485 = CARTESIAN_POINT ( 'NONE',  ( 0.9120734908136489683, -0.6692913385826771977, 0.1292274648535927661 ) ) ;
#40486 = CARTESIAN_POINT ( 'NONE',  ( 0.2925321140481932369, 0.2925321140481932369, -2.027559055118109743 ) ) ;
#40487 = CARTESIAN_POINT ( 'NONE',  ( 3.913920805910253264, 1.327648775429739025, -0.4258039130830911789 ) ) ;
#40488 = CARTESIAN_POINT ( 'NONE',  ( -0.3280839895013117347, 0.05413385826771626580, -0.4176697321401330321 ) ) ;
#40490 = DIRECTION ( 'NONE',  ( 0.000000000000000000, -1.000000000000000000, 0.000000000000000000 ) ) ;
#40489 = CARTESIAN_POINT ( 'NONE',  ( 0.9711286089238851948, -0.5023911411419708095, -0.1820866141732282451 ) ) ;
#40491 = CARTESIAN_POINT ( 'NONE',  ( -0.2362204724409451284, 0.4091458600556402425, -0.7198162729658792447 ) ) ;
#40492 = CARTESIAN_POINT ( 'NONE',  ( 1.043307086614173818, 0.07958543189024085140, 0.2665933059059887866 ) ) ;
#40493 = CARTESIAN_POINT ( 'NONE',  ( 1.220472440944882386, -0.6692913385826771977, 8.415575281601705876E-17 ) ) ;
#40494 = CARTESIAN_POINT ( 'NONE',  ( -0.1058382717557503072, 0.3949938075777408852, -0.08333333333333334259 ) ) ;
#40495 = CARTESIAN_POINT ( 'NONE',  ( -0.4921259842519677963, -0.5400638737290844871, 0.3530559997133364547 ) ) ;
#40496 = DIRECTION ( 'NONE',  ( -0.000000000000000000, -1.000000000000000000, -0.000000000000000000 ) ) ;
#40497 = CARTESIAN_POINT ( 'NONE',  ( -1.456692913385826182, -0.6692913385826771977, 8.415575281601705876E-17 ) ) ;
#40498 = CARTESIAN_POINT ( 'NONE',  ( -0.1771653543307080136, -0.5400638737290844871, 0.3530559997133364547 ) ) ;
#40499 = CARTESIAN_POINT ( 'NONE',  ( 0.1058382717557500852, -0.3949938075777408852, -0.6345144356955381149 ) ) ;
#40500 = CARTESIAN_POINT ( 'NONE',  ( 1.148293963254593875, -0.6692913385826771977, 0.1292274648535927661 ) ) ;
#40501 = CARTESIAN_POINT ( 'NONE',  ( 0.5774278215223103139, -0.6046776061558809534, -0.2411417322834644161 ) ) ;
#40502 = CARTESIAN_POINT ( 'NONE',  ( 0.5577427821522316087, -0.08942795157527998196, 0.3641732283464567121 ) ) ;
#40503 = CARTESIAN_POINT ( 'NONE',  ( -0.4253597317562083369, 1.326753431064211952, -1.038326151780470497 ) ) ;
#40504 = CARTESIAN_POINT ( 'NONE',  ( 0.4921259842519691285, -0.4536011799217368745, -0.2665933059059886201 ) ) ;
#40505 = CARTESIAN_POINT ( 'NONE',  ( -1.581364829396324945, -0.05778040916215560624, -0.4822834645669293319 ) ) ;
#40506 = CARTESIAN_POINT ( 'NONE',  ( -0.1998031496062994405, 0.3460692066303957537, -1.192257217847769057 ) ) ;
#40507 = CARTESIAN_POINT ( 'NONE',  ( 0.7677165354330716118, 0.1660481256975883668, -0.3530559997133364547 ) ) ;
#40508 = CARTESIAN_POINT ( 'NONE',  ( -0.3917322834645670104, -7.196005306013484475E-17, -0.5039370078740157410 ) ) ;
#40510 = CARTESIAN_POINT ( 'NONE',  ( 0.000000000000000000, 2.677165354330708791, 0.000000000000000000 ) ) ;
#40509 = CARTESIAN_POINT ( 'NONE',  ( 0.3083989501312343062, -0.05778040916215560624, -0.4822834645669293319 ) ) ;
#40511 = CARTESIAN_POINT ( 'NONE',  ( -0.7981007675632535436, -3.187520833735697382E-15, -0.4118477457933005237 ) ) ;
#40512 = CARTESIAN_POINT ( 'NONE',  ( 0.03937007874015806264, 0.1771653543307087630, 0.000000000000000000 ) ) ;
#40513 = EDGE_CURVE ( 'NONE', #44077, #68837, #37774, .T. ) ;
#40514 = CARTESIAN_POINT ( 'NONE',  ( 0.5118110236220480003, -0.6692913385826771977, 8.415575281601705876E-17 ) ) ;
#40515 = CARTESIAN_POINT ( 'NONE',  ( 1.692913385826772421, 0.1771653543307087630, 0.000000000000000000 ) ) ;
#40516 = CARTESIAN_POINT ( 'NONE',  ( -1.095800524934382292, -0.08942795157527998196, 0.3641732283464567121 ) ) ;
#40517 = CARTESIAN_POINT ( 'NONE',  ( -1.095800524934382292, -0.05778040916215522460, 0.4822834645669289988 ) ) ;
#40518 = CARTESIAN_POINT ( 'NONE',  ( -1.587926509186350810, -0.4281496062992124485, 0.4176697321401328655 ) ) ;
#40519 = AXIS2_PLACEMENT_3D ( 'NONE', #26864, #20974, #72329 ) ;
#40520 = CARTESIAN_POINT ( 'NONE',  ( 0.3412073490813655186, -0.6046776061558809534, -0.2411417322834644161 ) ) ;
#40521 = CARTESIAN_POINT ( 'NONE',  ( 1.555118110236221041, 0.1660481256975883668, -0.3530559997133364547 ) ) ;
#40522 = CARTESIAN_POINT ( 'NONE',  ( 1.077407372805332830, 1.181077650421485936, -0.3135877947998832460 ) ) ;
#40523 = CARTESIAN_POINT ( 'NONE',  ( 0.5905511811023629321, -0.6692913385826771977, 8.415575281601705876E-17 ) ) ;
#40524 = CARTESIAN_POINT ( 'NONE',  ( -0.3996062992125985480, -7.340648628747423112E-17, 0.1988188976377952277 ) ) ;
#40525 = CARTESIAN_POINT ( 'NONE',  ( 0.4441491729173822067, 1.369957082458975739, 3.911879148534922024 ) ) ;
#40526 = CARTESIAN_POINT ( 'NONE',  ( 1.266404199475066328, -0.3162353388693409650, -0.4822834645669289433 ) ) ;
#40527 = CARTESIAN_POINT ( 'NONE',  ( -1.384514435695537005, 0.1771653543307087630, 0.09757992244046791164 ) ) ;
#40528 = CARTESIAN_POINT ( 'NONE',  ( 1.404199475065617708, -0.004921259842519870586, -0.3153832671262229437 ) ) ;
#40529 = CARTESIAN_POINT ( 'NONE',  ( -1.266404199475064773, -0.08942795157528024563, -0.3641732283464568787 ) ) ;
#40530 = CARTESIAN_POINT ( 'NONE',  ( -0.7611548556430438595, -0.5023911411419708095, -0.1820866141732282451 ) ) ;
#40531 = CARTESIAN_POINT ( 'NONE',  ( 1.541994750656168645, -0.6692913385826771977, 0.1292274648535927661 ) ) ;
#40532 = CARTESIAN_POINT ( 'NONE',  ( 0.4396325459317590445, -0.5511811023622046335, 0.09757992244046803654 ) ) ;
#40533 = CARTESIAN_POINT ( 'NONE',  ( -0.06561679790026180015, 0.05413385826771666132, 0.4176697321401328100 ) ) ;
#40534 = CARTESIAN_POINT ( 'NONE',  ( 0.9645669291338588858, 0.1660481256975885056, 0.3530559997133364547 ) ) ;
#40535 = CARTESIAN_POINT ( 'NONE',  ( 0.006561679790026889343, -0.3162353388693409650, -0.4822834645669289433 ) ) ;
#40536 = CARTESIAN_POINT ( 'NONE',  ( 0.08530183727034192087, -0.2845877964562161244, -0.3641732283464567121 ) ) ;
#40537 = CARTESIAN_POINT ( 'NONE',  ( 1.161417322834646271, 0.1660481256975883668, -0.3530559997133364547 ) ) ;
#40538 = DIRECTION ( 'NONE',  ( 0.000000000000000000, 1.000000000000000000, -0.000000000000000000 ) ) ;
#40539 = CARTESIAN_POINT ( 'NONE',  ( -0.7939632545931754048, -0.3162353388693405765, 0.4822834645669290543 ) ) ;
#40540 = CARTESIAN_POINT ( 'NONE',  ( 0.3996062992125986035, 2.446882876249141962E-17, -0.7480314960629921295 ) ) ;
#40541 = CARTESIAN_POINT ( 'NONE',  ( 0.06561679790026316017, 0.009842519685039144428, -0.3409548833797004797 ) ) ;
#40542 = CARTESIAN_POINT ( 'NONE',  ( -0.7480314960629914633, -0.6692913385826771977, 8.415575281601705876E-17 ) ) ;
#40543 = CARTESIAN_POINT ( 'NONE',  ( 0.1049868766404206816, -0.6046776061558809534, -0.2411417322834644161 ) ) ;
#40544 = CARTESIAN_POINT ( 'NONE',  ( -0.3460692066303960868, 0.1998031496062990242, -2.703412073490813583 ) ) ;
#40545 = CARTESIAN_POINT ( 'NONE',  ( -0.2891555358219911054, 0.2891555358219909388, -2.224409448818897683 ) ) ;
#40546 = CARTESIAN_POINT ( 'NONE',  ( -0.3917322834645670104, -7.196005306013484475E-17, -0.3464566929133857665 ) ) ;
#40547 = CARTESIAN_POINT ( 'NONE',  ( 3.821484228344193657, 2.755905511811024056, -0.5314960629921260393 ) ) ;
#40548 = CARTESIAN_POINT ( 'NONE',  ( -1.489501312335957062, -0.2845877964562161244, -0.3641732283464567121 ) ) ;
#40549 = CARTESIAN_POINT ( 'NONE',  ( -0.3392501089628017219, -0.1958661417322836718, -0.9895013123359579499 ) ) ;
#40550 = CARTESIAN_POINT ( 'NONE',  ( -1.522309711286088607, 0.2306618581243847221, -0.2411417322834647770 ) ) ;
#40551 = CARTESIAN_POINT ( 'NONE',  ( 0.2891555358219910499, -0.2891555358219909944, -2.852362204724409267 ) ) ;
#40552 = CARTESIAN_POINT ( 'NONE',  ( 0.3543307086614181922, -0.6692913385826771977, 8.415575281601705876E-17 ) ) ;
#40553 = CARTESIAN_POINT ( 'NONE',  ( -0.5511811023622041894, -0.1870078740157480601, -0.3641732283464567677 ) ) ;
#40554 = CARTESIAN_POINT ( 'NONE',  ( 0.8136482939632553313, 0.2306618581243848609, 0.2411417322834645549 ) ) ;
#40555 = CARTESIAN_POINT ( 'NONE',  ( 0.5446194225721792126, -0.05778040916215560624, -0.4822834645669293319 ) ) ;
#40556 = CARTESIAN_POINT ( 'NONE',  ( 0.4744094488188940750, 1.537401574803149984, 1.016821367227985329 ) ) ;
#40557 = CARTESIAN_POINT ( 'NONE',  ( -0.2925321140481930704, -0.2925321140481933480, -2.578740157480315265 ) ) ;
#40558 = CARTESIAN_POINT ( 'NONE',  ( 4.797336870675656522E-17, -0.3917322834645670659, -1.335321153052180243 ) ) ;
#40559 = CARTESIAN_POINT ( 'NONE',  ( 1.338582677165355062, -0.1870078740157479769, 0.4822834645669291653 ) ) ;
#40560 = CARTESIAN_POINT ( 'NONE',  ( -0.07217847769028813698, -0.3162353388693409650, -0.4822834645669289433 ) ) ;
#40561 = CARTESIAN_POINT ( 'NONE',  ( -1.574803149606298192, -0.1870078740157480879, -0.4822834645669291653 ) ) ;
#40562 = CARTESIAN_POINT ( 'NONE',  ( 0.9973753280839902091, -0.6046776061558807314, 0.2411417322834647770 ) ) ;
#40563 = CARTESIAN_POINT ( 'NONE',  ( -0.3917322834645669549, -0.1049643490035306603, -0.4455380577427821565 ) ) ;
#40564 = CARTESIAN_POINT ( 'NONE',  ( 0.07874015748031558404, -0.1870078740157480879, -0.4822834645669291653 ) ) ;
#40565 = CARTESIAN_POINT ( 'NONE',  ( 0.5118110236220480003, -0.6692913385826771977, 8.415575281601705876E-17 ) ) ;
#40566 = CARTESIAN_POINT ( 'NONE',  ( -0.2362204724409440182, -0.1870078740157479769, 0.4822834645669291653 ) ) ;
#40567 = CARTESIAN_POINT ( 'NONE',  ( 0.7611548556430454138, 0.1283753931104746893, -0.1820866141732285504 ) ) ;
#40568 = CARTESIAN_POINT ( 'NONE',  ( -1.148293963254592542, -0.6692913385826773087, -0.1292274648535924053 ) ) ;
#40569 = CARTESIAN_POINT ( 'NONE',  ( -1.410761154855642463, -0.05778040916215522460, 0.4822834645669289988 ) ) ;
#40570 = CARTESIAN_POINT ( 'NONE',  ( 0.8923884514435701520, -0.6046776061558809534, -0.2411417322834644161 ) ) ;
#40571 = CARTESIAN_POINT ( 'NONE',  ( -0.7535225988626923499, 2.401574803149606474, -0.4915354330708644470 ) ) ;
#40572 = CARTESIAN_POINT ( 'NONE',  ( 0.2867679344610365999, -0.2867679344610365444, -1.822834645669291653 ) ) ;
#40573 = ORIENTED_EDGE ( 'NONE', *, *, #52272, .F. ) ;
#40574 = CARTESIAN_POINT ( 'NONE',  ( -9.787531504996567848E-17, 0.3996062992125986035, -0.6299212598425196763 ) ) ;
#40575 = ORIENTED_EDGE ( 'NONE', *, *, #43383, .F. ) ;
#40576 = CARTESIAN_POINT ( 'NONE',  ( 0.9645669291338591078, -0.5400638737290845981, -0.3530559997133363437 ) ) ;
#40577 = CARTESIAN_POINT ( 'NONE',  ( 0.3608923884514443348, 0.1771653543307087075, -0.09757992244046823083 ) ) ;
#40578 = CARTESIAN_POINT ( 'NONE',  ( 3.237502119437988046, 2.729657717072965006, -0.5314960629921260393 ) ) ;
#40579 = CARTESIAN_POINT ( 'NONE',  ( 0.5314960629920921775, 2.716535433070866645, 3.224202737261820939 ) ) ;
#40580 = CARTESIAN_POINT ( 'NONE',  ( 0.3974833285012838724, 0.03087045868620753170, -1.929133858267772617 ) ) ;
#40581 = CARTESIAN_POINT ( 'NONE',  ( -0.3917322834645669549, -0.1049643490035306603, -1.075459317585301777 ) ) ;
#40582 = CARTESIAN_POINT ( 'NONE',  ( 1.476377952755906220, 0.1660481256975883668, -0.3530559997133364547 ) ) ;
#40583 = CARTESIAN_POINT ( 'NONE',  ( -1.568241469816272105, -0.3162353388693409650, -0.4822834645669289433 ) ) ;
#40584 = CARTESIAN_POINT ( 'NONE',  ( -0.2887139107611542133, 0.2306618581243848609, 0.2411417322834645549 ) ) ;
#40585 = CARTESIAN_POINT ( 'NONE',  ( 1.069553805774278610, -0.6692913385826771977, 0.1292274648535927661 ) ) ;
#40586 = VERTEX_POINT ( 'NONE', #23912 ) ;
#40587 = CARTESIAN_POINT ( 'NONE',  ( -1.725721784776902190, -0.05778040916215522460, 0.4822834645669289988 ) ) ;
#40588 = CARTESIAN_POINT ( 'NONE',  ( -1.063894186419820809, 1.223759533161110635, -0.3572641188300489934 ) ) ;
#40589 = SHAPE_DEFINITION_REPRESENTATION ( #41327, #61632 ) ;
#40590 = CARTESIAN_POINT ( 'NONE',  ( 1.673228346456693494, 0.07958543189024085140, 0.2665933059059887866 ) ) ;
#40591 = CARTESIAN_POINT ( 'NONE',  ( -0.2925321140481932369, 0.2925321140481930704, -1.986220472440944906 ) ) ;
#40592 = CARTESIAN_POINT ( 'NONE',  ( -1.496062992125983815, -0.1870078740157479769, 0.3641732283464567677 ) ) ;
#40593 = CARTESIAN_POINT ( 'NONE',  ( -1.640419947506561060, 0.05413385826771666132, 0.4176697321401328100 ) ) ;
#40594 = CARTESIAN_POINT ( 'NONE',  ( 0.7086614173228353852, -0.1870078740157479769, 0.4822834645669291653 ) ) ;
#40595 = ORIENTED_EDGE ( 'NONE', *, *, #44899, .F. ) ;
#40597 = PLANE ( 'NONE',  #23694 ) ;
#40596 = CARTESIAN_POINT ( 'NONE',  ( 1.417322834645670104, -0.1870078740157480879, -0.4822834645669291653 ) ) ;
#40598 = CARTESIAN_POINT ( 'NONE',  ( -0.5971128608923877978, 0.1771653543307087630, 0.09757992244046791164 ) ) ;
#40599 = CARTESIAN_POINT ( 'NONE',  ( 0.8464566929133866546, -0.5400638737290844871, 0.3530559997133364547 ) ) ;
#40600 = CARTESIAN_POINT ( 'NONE',  ( -1.522309711286088607, 0.2306618581243847221, -0.2411417322834647770 ) ) ;
#40601 = CARTESIAN_POINT ( 'NONE',  ( 0.3917322834645669549, 2.398668435337827645E-17, -1.143025303640733181 ) ) ;
#40602 = CARTESIAN_POINT ( 'NONE',  ( -0.9448818897637790704, -0.1870078740157479769, 0.3641732283464567677 ) ) ;
#40603 = CARTESIAN_POINT ( 'NONE',  ( -1.364829396325458521, -0.5023911411419708095, 0.1820866141732285504 ) ) ;
#40604 = CARTESIAN_POINT ( 'NONE',  ( -0.3917322834645671215, 0.1049643490035301469, -1.062335958005249381 ) ) ;
#40605 = CARTESIAN_POINT ( 'NONE',  ( 0.5774278215223103139, -0.6046776061558809534, -0.2411417322834644161 ) ) ;
#40606 = CARTESIAN_POINT ( 'NONE',  ( -1.049868766404198794, -0.5023911411419708095, 0.1820866141732285504 ) ) ;
#40607 = CARTESIAN_POINT ( 'NONE',  ( -0.1902887139107604098, -0.5511811023622046335, 0.09757992244046803654 ) ) ;
#40608 = CARTESIAN_POINT ( 'NONE',  ( -0.4658792650918627265, -0.05778040916215522460, 0.4822834645669289988 ) ) ;
#40609 = CARTESIAN_POINT ( 'NONE',  ( 1.607611548556431069, -0.6692913385826773087, -0.1292274648535924053 ) ) ;
#40610 = CARTESIAN_POINT ( 'NONE',  ( -0.2867679344610367109, 0.2867679344610365444, 0.1410567997037251442 ) ) ;
#40611 = CARTESIAN_POINT ( 'NONE',  ( 0.5971128608923890191, -0.6692913385826771977, 0.1292274648535927661 ) ) ;
#40612 = CARTESIAN_POINT ( 'NONE',  ( -1.572991167713776672, 2.401574803149606474, -0.1227090857360982196 ) ) ;
#40613 = CARTESIAN_POINT ( 'NONE',  ( 0.4091458600556403535, 0.2362204724409449896, -1.467847769028871596 ) ) ;
#40614 = CARTESIAN_POINT ( 'NONE',  ( -0.8136482939632537770, -0.6046776061558807314, 0.2411417322834647770 ) ) ;
#40615 = CARTESIAN_POINT ( 'NONE',  ( -0.3412073490813641308, -0.5023911411419708095, 0.1820866141732285504 ) ) ;
#40616 = CARTESIAN_POINT ( 'NONE',  ( -1.489501312335957062, -0.05778040916215522460, 0.4822834645669289988 ) ) ;
#40617 = CARTESIAN_POINT ( 'NONE',  ( 0.5380577427821529035, -0.3690944881889763329, 0.3153832671262228327 ) ) ;
#40618 = CARTESIAN_POINT ( 'NONE',  ( -0.8858267716535425107, 0.07958543189024071263, -0.2665933059059888421 ) ) ;
#40619 = CARTESIAN_POINT ( 'NONE',  ( -1.003937007874015297, -0.5400638737290845981, -0.3530559997133363437 ) ) ;
#40620 = CARTESIAN_POINT ( 'NONE',  ( -1.640419947506561060, -0.4281496062992127816, -0.4176697321401328100 ) ) ;
#40621 = CARTESIAN_POINT ( 'NONE',  ( -1.653543307086613234, -0.1870078740157479769, 0.4822834645669291653 ) ) ;
#40622 = DIRECTION ( 'NONE',  ( 0.000000000000000000, 0.000000000000000000, 1.000000000000000000 ) ) ;
#40623 = CARTESIAN_POINT ( 'NONE',  ( 0.7414698162729663755, 0.1771653543307087630, 0.09757992244046791164 ) ) ;
#40624 = PRODUCT_DEFINITION_SHAPE ( 'NONE', 'NONE',  #83326 ) ;
#40625 = CARTESIAN_POINT ( 'NONE',  ( 0.4330708661417329575, 0.2952755905511811885, 0.000000000000000000 ) ) ;
#40626 = CARTESIAN_POINT ( 'NONE',  ( -1.391076115485563314, -0.6046776061558809534, -0.2411417322834644161 ) ) ;
#40627 = CARTESIAN_POINT ( 'NONE',  ( 1.410761154855643795, -0.2845877964562159024, 0.3641732283464567677 ) ) ;
#40628 = VECTOR ( 'NONE', #42594, 39.37007874015748143 ) ;
#40629 = ORIENTED_EDGE ( 'NONE', *, *, #53064, .F. ) ;
#40630 = CARTESIAN_POINT ( 'NONE',  ( -0.1998031496062994405, 0.3460692066303957537, -2.767060367454068359 ) ) ;
#40631 = CARTESIAN_POINT ( 'NONE',  ( -1.351706036745406347, -0.3690944881889763329, 0.3153832671262228327 ) ) ;
#40632 = CARTESIAN_POINT ( 'NONE',  ( -0.5446194225721777693, -0.05778040916215522460, 0.4822834645669289988 ) ) ;
#40633 = CARTESIAN_POINT ( 'NONE',  ( 0.3477690288713918276, 0.2952755905511811885, 0.1292274648535926551 ) ) ;
#40634 = CARTESIAN_POINT ( 'NONE',  ( -1.450131233595799651, -0.5511811023622046335, 0.09757992244046803654 ) ) ;
#40635 = CARTESIAN_POINT ( 'NONE',  ( 0.3996062992125986035, -0.1070741851644052972, -1.605643044619422977 ) ) ;
#40636 = CARTESIAN_POINT ( 'NONE',  ( -1.450131233595799651, -0.6692913385826771977, 0.1292274648535927661 ) ) ;
#40637 = CARTESIAN_POINT ( 'NONE',  ( 0.5183727034120741983, -0.6692913385826771977, 0.1292274648535927661 ) ) ;
#40638 = CARTESIAN_POINT ( 'NONE',  ( 0.2493438320209980519, 0.05413385826771666132, 0.4176697321401328100 ) ) ;
#40639 = CARTESIAN_POINT ( 'NONE',  ( 1.253280839895013710, -0.3162353388693405765, 0.4822834645669290543 ) ) ;
#40640 = CARTESIAN_POINT ( 'NONE',  ( 0.3460692066303958092, 0.1998031496062993018, -1.152887139107611425 ) ) ;
#40641 = CARTESIAN_POINT ( 'NONE',  ( 4.893765752498283924E-17, -0.3996062992125986035, -1.496062992125984259 ) ) ;
#40642 = CARTESIAN_POINT ( 'NONE',  ( 0.3949938075777409408, 0.1058382717557500574, -0.5971128608923886860 ) ) ;
#40643 = CARTESIAN_POINT ( 'NONE',  ( 0.3392501089628018884, -0.1958661417322834220, -0.09711286089238840846 ) ) ;
#40644 = CARTESIAN_POINT ( 'NONE',  ( 0.08530183727034192087, -0.2845877964562161244, -0.3641732283464567121 ) ) ;
#40645 = CARTESIAN_POINT ( 'NONE',  ( -0.1640419947506555343, -0.3162353388693405765, 0.4822834645669290543 ) ) ;
#40646 = CARTESIAN_POINT ( 'NONE',  ( 0.8464566929133865436, 0.1660481256975883668, -0.3530559997133364547 ) ) ;
#40647 = CARTESIAN_POINT ( 'NONE',  ( 0.3420746716998660508, 0.1974969037888705814, -1.940288713910761187 ) ) ;
#40648 = CARTESIAN_POINT ( 'NONE',  ( -0.1574803149606292529, -0.1870078740157480601, -0.3641732283464567677 ) ) ;
#40649 = CARTESIAN_POINT ( 'NONE',  ( -1.246719160104985846, -0.4281496062992127816, -0.4176697321401328100 ) ) ;
#40650 = CARTESIAN_POINT ( 'NONE',  ( -1.574803149606298192, -0.1870078740157480879, -0.4822834645669291653 ) ) ;
#40651 = CARTESIAN_POINT ( 'NONE',  ( 0.1265901696524989462, 0.4724409448818897572, -2.198162729658792447 ) ) ;
#40652 = CARTESIAN_POINT ( 'NONE',  ( 0.2432155562301146490, 0.3078094465263132573, -2.755905511811025388 ) ) ;
#40653 = ORIENTED_EDGE ( 'NONE', *, *, #68271, .T. ) ;
#40654 = ORIENTED_EDGE ( 'NONE', *, *, #79843, .F. ) ;
#40655 = CARTESIAN_POINT ( 'NONE',  ( 1.312335958005249825, 0.2306618581243847221, -0.2411417322834647770 ) ) ;
#40656 = CARTESIAN_POINT ( 'NONE',  ( -1.666666666666665853, 0.05413385826771626580, -0.4176697321401330321 ) ) ;
#40658 = CARTESIAN_POINT ( 'NONE',  ( -1.364829396325458521, -0.6046776061558807314, 0.2411417322834647770 ) ) ;
#40657 = CARTESIAN_POINT ( 'NONE',  ( -1.325459317585300889, -0.004921259842519576551, 0.3153832671262227771 ) ) ;
#40659 = CARTESIAN_POINT ( 'NONE',  ( 0.1958661417322836162, -0.3392501089628018329, -2.534101419126297827 ) ) ;
#40660 = CYLINDRICAL_SURFACE ( 'NONE', #66588, 0.4822834645669291653 ) ;
#40661 = CARTESIAN_POINT ( 'NONE',  ( 1.423884514435696413, -0.3162353388693409650, -0.4822834645669289433 ) ) ;
#40662 = CARTESIAN_POINT ( 'NONE',  ( -1.719160104986876103, 0.05413385826771666132, 0.4176697321401328100 ) ) ;
#40663 = CARTESIAN_POINT ( 'NONE',  ( -0.2362204724409442680, -0.1870078740157480879, -0.4822834645669291653 ) ) ;
#40664 = CARTESIAN_POINT ( 'NONE',  ( -0.2493438320209966919, 0.05413385826771626580, -0.4176697321401330321 ) ) ;
#40665 = CARTESIAN_POINT ( 'NONE',  ( -1.181102362204723644, -0.1870078740157479769, 0.4822834645669291653 ) ) ;
#40666 = CARTESIAN_POINT ( 'NONE',  ( 4.797336870675655290E-17, -0.3917322834645669549, -2.835938689467505380 ) ) ;
#40667 = CARTESIAN_POINT ( 'NONE',  ( 0.4986876640419954376, 0.2306618581243848609, 0.2411417322834645549 ) ) ;
#40668 = CARTESIAN_POINT ( 'NONE',  ( 0.1958661417322834775, 0.3392501089628018884, -1.868766404199474929 ) ) ;
#40669 = CARTESIAN_POINT ( 'NONE',  ( -1.325459317585300889, -0.004921259842519576551, 0.3153832671262227771 ) ) ;
#40670 = ORIENTED_EDGE ( 'NONE', *, *, #58210, .F. ) ;
#40671 = CARTESIAN_POINT ( 'NONE',  ( 0.3420746716998659953, 0.1974969037888705536, -2.335958005249343827 ) ) ;
#40672 = ORIENTED_EDGE ( 'NONE', *, *, #25177, .T. ) ;
#40673 = LINE ( 'NONE', #67606, #15323 ) ;
#40674 = CARTESIAN_POINT ( 'NONE',  ( -1.194225721784776262, 0.05413385826771626580, -0.4176697321401330321 ) ) ;
#40675 = CARTESIAN_POINT ( 'NONE',  ( -1.220472440944881054, -0.6692913385826771977, 8.415575281601705876E-17 ) ) ;
#40676 = CARTESIAN_POINT ( 'NONE',  ( -0.2925321140481932924, 0.2925321140481931814, -0.8070866141732284671 ) ) ;
#40677 = CARTESIAN_POINT ( 'NONE',  ( -1.338582677165353729, -0.1870078740157480879, -0.4822834645669291653 ) ) ;
#40678 = CARTESIAN_POINT ( 'NONE',  ( -1.666666666666665853, 0.05413385826771626580, -0.4176697321401330321 ) ) ;
#40679 = FACE_BOUND ( 'NONE', #16176, .T. ) ;
#40680 = CARTESIAN_POINT ( 'NONE',  ( 0.1341536278048623410, 1.446850393700787274, 0.2827841492639507903 ) ) ;
#40681 = CARTESIAN_POINT ( 'NONE',  ( -0.3917322834645671215, 0.1049643490035301469, -0.1174540682414699083 ) ) ;
#40682 = CARTESIAN_POINT ( 'NONE',  ( 0.1049868766404206816, 0.1283753931104748280, 0.1820866141732283561 ) ) ;
#40683 = CARTESIAN_POINT ( 'NONE',  ( -0.7808398950131225646, -0.08942795157527998196, 0.3641732283464567121 ) ) ;
#40684 = CARTESIAN_POINT ( 'NONE',  ( -1.082677165354329896, -0.5400638737290845981, -0.3530559997133363437 ) ) ;
#40685 = CARTESIAN_POINT ( 'NONE',  ( 0.8398950131233602345, 0.2306618581243847221, -0.2411417322834647770 ) ) ;
#40686 = CARTESIAN_POINT ( 'NONE',  ( -0.9514435695538050464, -0.05778040916215560624, -0.4822834645669293319 ) ) ;
#40687 = CARTESIAN_POINT ( 'NONE',  ( 0.5314960629921395840, 2.716830163678111365, -3.890345922373657839 ) ) ;
#40688 = ORIENTED_EDGE ( 'NONE', *, *, #82913, .T. ) ;
#40689 = CARTESIAN_POINT ( 'NONE',  ( -1.272965879265091305, 0.05413385826771626580, -0.4176697321401330321 ) ) ;
#40690 = CARTESIAN_POINT ( 'NONE',  ( -1.482939632545930975, -0.3690944881889765550, -0.3153832671262227771 ) ) ;
#40691 = CARTESIAN_POINT ( 'NONE',  ( 0.4724409448818898682, 2.892866454678787531E-17, -1.139763779527559029 ) ) ;
#40692 = CARTESIAN_POINT ( 'NONE',  ( 0.4724409448818896462, 0.1265901696524990294, -1.227034120734908029 ) ) ;
#40693 = CARTESIAN_POINT ( 'NONE',  ( 2.169549780153825047, 1.520054044952883210, -0.4741688556381175590 ) ) ;
#40694 = EDGE_CURVE ( 'NONE', #47373, #38567, #61238, .T. ) ;
#40695 = CARTESIAN_POINT ( 'NONE',  ( 4.797336870675656522E-17, -0.3917322834645670104, -0.8582677165354329896 ) ) ;
#40696 = CARTESIAN_POINT ( 'NONE',  ( -0.1049643490035301885, -0.3917322834645671215, -2.361548556430446144 ) ) ;
#40697 = CARTESIAN_POINT ( 'NONE',  ( -0.2362204724409440182, -0.1870078740157479769, 0.4822834645669291653 ) ) ;
#40698 = CARTESIAN_POINT ( 'NONE',  ( -1.397637795275589623, -0.4536011799217368745, -0.2665933059059886201 ) ) ;
#40699 = CARTESIAN_POINT ( 'NONE',  ( -0.3996062992125985480, -7.340648628747423112E-17, 0.04133858267716532947 ) ) ;
#40701 = CARTESIAN_POINT ( 'NONE',  ( -0.3129921259842521897, 1.496062992125984259, 0.4921259842519685179 ) ) ;
#40700 = CARTESIAN_POINT ( 'NONE',  ( -1.646981627296586703, -0.3162353388693409650, -0.4822834645669289433 ) ) ;
#40702 = CARTESIAN_POINT ( 'NONE',  ( -1.371391076115484831, 0.2952755905511810774, -0.1292274648535930714 ) ) ;
#40703 = CARTESIAN_POINT ( 'NONE',  ( -0.4593175853018366950, 0.05413385826771666132, 0.4176697321401328100 ) ) ;
#40704 = CARTESIAN_POINT ( 'NONE',  ( -0.2867679344610366554, 0.2867679344610365444, 0.2152424128947000026 ) ) ;
#40705 = CARTESIAN_POINT ( 'NONE',  ( 0.3740157480314966754, 0.07958543189024071263, -0.2665933059059888421 ) ) ;
#40706 = FACE_OUTER_BOUND ( 'NONE', #1312, .T. ) ;
#40707 = CARTESIAN_POINT ( 'NONE',  ( 0.4593175853018380828, -0.004921259842519870586, -0.3153832671262229437 ) ) ;
#40708 = CARTESIAN_POINT ( 'NONE',  ( 0.8661417322834652488, -0.1870078740157480601, -0.3641732283464567677 ) ) ;
#40709 = CARTESIAN_POINT ( 'NONE',  ( 1.023622047244095112, -0.1870078740157480879, -0.4822834645669291653 ) ) ;
#40710 = CARTESIAN_POINT ( 'NONE',  ( -0.3674540682414689785, 0.1283753931104748280, 0.1820866141732283561 ) ) ;
#40711 = CARTESIAN_POINT ( 'NONE',  ( 0.3917322834645670104, -0.1049643490035303411, -1.835958005249343827 ) ) ;
#40712 = CARTESIAN_POINT ( 'NONE',  ( -1.213910761154854745, -0.6692913385826771977, 0.1292274648535927661 ) ) ;
#40713 = CARTESIAN_POINT ( 'NONE',  ( 0.09186351706036799403, -0.3690944881889765550, -0.3153832671262227771 ) ) ;
#40714 = CARTESIAN_POINT ( 'NONE',  ( -1.371391076115484609, -0.5511811023622046335, 0.09757992244046803654 ) ) ;
#40715 = CARTESIAN_POINT ( 'NONE',  ( -0.1265901696524986964, -0.4724409448818899238, -0.4639107611548556331 ) ) ;
#40716 = CARTESIAN_POINT ( 'NONE',  ( -0.9383202099737524282, -0.2845877964562161244, -0.3641732283464567121 ) ) ;
#40717 = CARTESIAN_POINT ( 'NONE',  ( 0.4436160793303255412, 1.369148167000072247, -1.503412402614913379 ) ) ;
#40718 = CARTESIAN_POINT ( 'NONE',  ( -0.05249343832020911260, 0.2306618581243848609, 0.2411417322834645549 ) ) ;
#40719 = CARTESIAN_POINT ( 'NONE',  ( 1.673228346456693494, 0.07958543189024085140, 0.2665933059059887866 ) ) ;
#40720 = CARTESIAN_POINT ( 'NONE',  ( 0.7283464566929140904, -0.4536011799217368745, -0.2665933059059886201 ) ) ;
#40721 = CARTESIAN_POINT ( 'NONE',  ( -0.2296587926509179312, -0.2845877964562161244, -0.3641732283464567121 ) ) ;
#40722 = CARTESIAN_POINT ( 'NONE',  ( -0.4986876640419939388, 0.2306618581243847221, -0.2411417322834647770 ) ) ;
#40723 = CARTESIAN_POINT ( 'NONE',  ( -1.673228346456691717, 0.1660481256975883668, -0.3530559997133364547 ) ) ;
#40724 = CARTESIAN_POINT ( 'NONE',  ( -1.049868766404198794, -0.5023911411419708095, 0.1820866141732285504 ) ) ;
#40725 = DIRECTION ( 'NONE',  ( 1.000000000000000000, 0.000000000000000000, 0.000000000000000000 ) ) ;
#40726 = AXIS2_PLACEMENT_3D ( 'NONE', #5319, #38948, #32638 ) ;
#40727 = EDGE_CURVE ( 'NONE', #45287, #66126, #46644, .T. ) ;
#40728 = CARTESIAN_POINT ( 'NONE',  ( 0.6430446194225729606, -0.4281496062992127816, -0.4176697321401328100 ) ) ;
#40729 = EDGE_LOOP ( 'NONE', ( #76506, #17506, #50885, #14926 ) ) ;
#40730 = CARTESIAN_POINT ( 'NONE',  ( 0.1998031496062992463, 0.3460692066303959202, -1.480971128608923548 ) ) ;
#40731 = DIRECTION ( 'NONE',  ( -3.096699300667737957E-16, 1.000000000000000000, -0.000000000000000000 ) ) ;
#40732 = CARTESIAN_POINT ( 'NONE',  ( -0.1902887139107604098, -0.5511811023622046335, 0.09757992244046803654 ) ) ;
#40733 = CARTESIAN_POINT ( 'NONE',  ( -1.561679790026246017, -0.4281496062992127816, -0.4176697321401328100 ) ) ;
#40734 = CARTESIAN_POINT ( 'NONE',  ( -1.489501312335957062, -0.08942795157527998196, 0.3641732283464567121 ) ) ;
#40735 = CARTESIAN_POINT ( 'NONE',  ( 1.397637795275591177, 0.1660481256975883668, -0.3530559997133364547 ) ) ;
#40736 = CARTESIAN_POINT ( 'NONE',  ( -0.5118110236220466680, -0.5511811023622047445, 6.969142054262312111E-17 ) ) ;
#40737 = CARTESIAN_POINT ( 'NONE',  ( 0.3996062992125985480, -0.1070741851644052972, -0.03083989501312337997 ) ) ;
#40738 = CARTESIAN_POINT ( 'NONE',  ( 1.062992125984252745, -0.6692913385826771977, 8.415575281601705876E-17 ) ) ;
#40739 = CARTESIAN_POINT ( 'NONE',  ( 0.3460692066303959757, -0.1998031496062991907, -0.2624671916010498651 ) ) ;
#40740 = VECTOR ( 'NONE', #8859, 39.37007874015748143 ) ;
#40741 = CARTESIAN_POINT ( 'NONE',  ( -0.3917322834645670104, -0.1049643490035307020, -2.719835588747718802 ) ) ;
#40742 = DIRECTION ( 'NONE',  ( 0.000000000000000000, 0.000000000000000000, -1.000000000000000000 ) ) ;
#40743 = CARTESIAN_POINT ( 'NONE',  ( 1.423884514435696191, -0.08942795157527998196, 0.3641732283464567121 ) ) ;
#40744 = CARTESIAN_POINT ( 'NONE',  ( -1.115485564304461219, -0.4281496062992124485, 0.4176697321401328655 ) ) ;
#40745 = CARTESIAN_POINT ( 'NONE',  ( 1.299212598425197429, 0.2952755905511811885, 0.000000000000000000 ) ) ;
#40746 = CARTESIAN_POINT ( 'NONE',  ( -0.3392501089628019995, 0.1958661417322832277, -2.473097112860892288 ) ) ;
#40747 = CARTESIAN_POINT ( 'NONE',  ( 1.167979002624672580, -0.3690944881889763329, 0.3153832671262228327 ) ) ;
#40748 = ADVANCED_FACE ( 'NONE', ( #41477 ), #54087, .F. ) ;
#40749 = CARTESIAN_POINT ( 'NONE',  ( 0.2755905511811031494, 0.2952755905511811885, 0.000000000000000000 ) ) ;
#40750 = CARTESIAN_POINT ( 'NONE',  ( -0.3149606299212590610, -0.1870078740157480879, -0.4822834645669291653 ) ) ;
#40751 = CARTESIAN_POINT ( 'NONE',  ( -0.3996062992122574320, -0.1070741851649966020, -1.935695538057784493 ) ) ;
#40752 = CARTESIAN_POINT ( 'NONE',  ( 0.2887139107611556010, -0.5023911411419708095, 0.1820866141732285504 ) ) ;
#40753 = ORIENTED_EDGE ( 'NONE', *, *, #63106, .T. ) ;
#40754 = CARTESIAN_POINT ( 'NONE',  ( -0.1049643490035307158, 0.3917322834645670104, -0.4757411005587420805 ) ) ;
#40755 = ORIENTED_EDGE ( 'NONE', *, *, #72350, .T. ) ;
#40756 = CARTESIAN_POINT ( 'NONE',  ( -0.4199475065616791736, 0.2306618581243847221, -0.2411417322834647770 ) ) ;
#40757 = CARTESIAN_POINT ( 'NONE',  ( 1.364829396325459854, -0.6046776061558809534, -0.2411417322834644161 ) ) ;
#40758 = CARTESIAN_POINT ( 'NONE',  ( 0.06561679790026316017, -0.4281496062992124485, 0.4176697321401328655 ) ) ;
#40759 = CARTESIAN_POINT ( 'NONE',  ( -0.2755905511811015396, -0.5511811023622047445, 6.969142054262312111E-17 ) ) ;
#40760 = CARTESIAN_POINT ( 'NONE',  ( 1.108923884514436686, -0.3162353388693409650, -0.4822834645669289433 ) ) ;
#40761 = CARTESIAN_POINT ( 'NONE',  ( -1.023622047244093558, -0.1870078740157479769, 0.4822834645669291653 ) ) ;
#40762 = CARTESIAN_POINT ( 'NONE',  ( -0.1181102362204717315, 0.2952755905511811885, 0.000000000000000000 ) ) ;
#40763 = CARTESIAN_POINT ( 'NONE',  ( -0.7480314960629914633, 0.2952755905511811885, 0.000000000000000000 ) ) ;
#40764 = CARTESIAN_POINT ( 'NONE',  ( 1.233595800524935227, -0.6046776061558807314, 0.2411417322834647770 ) ) ;
#40765 = CARTESIAN_POINT ( 'NONE',  ( 0.7939632545931766261, -0.05778040916215522460, 0.4822834645669289988 ) ) ;
#40766 = CARTESIAN_POINT ( 'NONE',  ( 1.023622047244095334, -0.1870078740157479769, 0.4822834645669291653 ) ) ;
#40767 = CARTESIAN_POINT ( 'NONE',  ( -0.3917322834645671215, 0.1049643490035301469, -0.8123359580052491591 ) ) ;
#40768 = CARTESIAN_POINT ( 'NONE',  ( 0.1443569553805781891, -0.004921259842519870586, -0.3153832671262229437 ) ) ;
#40769 = ORIENTED_EDGE ( 'NONE', *, *, #66014, .F. ) ;
#40770 = CARTESIAN_POINT ( 'NONE',  ( -9.674558042662121740E-17, 0.3949938075777409963, -0.9448818897637795144 ) ) ;
#40771 = EDGE_LOOP ( 'NONE', ( #14565, #71518 ) ) ;
#40772 = CARTESIAN_POINT ( 'NONE',  ( -0.9842519685039365918, -0.5511811023622047445, 6.969142054262312111E-17 ) ) ;
#40773 = CARTESIAN_POINT ( 'NONE',  ( 0.1509186351706045259, -0.05778040916215560624, -0.4822834645669293319 ) ) ;
#40774 = CARTESIAN_POINT ( 'NONE',  ( -1.441491218394533647, 1.158252404499417576, 0.2851933289425553353 ) ) ;
#40775 = CARTESIAN_POINT ( 'NONE',  ( -0.1181102362204717315, 0.2952755905511811885, 0.000000000000000000 ) ) ;
#40776 = CARTESIAN_POINT ( 'NONE',  ( -0.3477690288713905509, -0.6692913385826771977, 0.1292274648535927661 ) ) ;
#40777 = CARTESIAN_POINT ( 'NONE',  ( -0.8595800524934373854, -0.05778040916215522460, 0.4822834645669289988 ) ) ;
#40778 = CARTESIAN_POINT ( 'NONE',  ( -1.246719160104986512, 0.05413385826771666132, 0.4176697321401328100 ) ) ;
#40779 = CARTESIAN_POINT ( 'NONE',  ( 1.338582677165355062, -0.1870078740157479769, 0.3641732283464567677 ) ) ;
#40780 = DIRECTION ( 'NONE',  ( 0.000000000000000000, 0.000000000000000000, -1.000000000000000000 ) ) ;
#40781 = CARTESIAN_POINT ( 'NONE',  ( 0.2917632292039851194, 0.04688088360317046316, 5.530710407408372831 ) ) ;
#40782 = CARTESIAN_POINT ( 'NONE',  ( 0.3018372703412079971, -0.3690944881889763329, 0.3153832671262228327 ) ) ;
#40783 = VECTOR ( 'NONE', #59663, 39.37007874015748143 ) ;
#40784 = CARTESIAN_POINT ( 'NONE',  ( -0.006561679790025524116, -0.05778040916215560624, -0.4822834645669293319 ) ) ;
#40785 = CARTESIAN_POINT ( 'NONE',  ( 0.4658792650918641698, -0.05778040916215560624, -0.4822834645669293319 ) ) ;
#40786 = ORIENTED_EDGE ( 'NONE', *, *, #32000, .F. ) ;
#40787 = CARTESIAN_POINT ( 'NONE',  ( 0.3460692066303959757, -0.1998031496062991907, -1.837270341207349000 ) ) ;
#40788 = CARTESIAN_POINT ( 'NONE',  ( -0.6036745406824141069, 0.1539470093639523085, 0.1968503937007873850 ) ) ;
#40789 = CARTESIAN_POINT ( 'NONE',  ( 0.3996062992125985480, 2.446882876249141654E-17, -0.9822834645669291653 ) ) ;
#40790 = CARTESIAN_POINT ( 'NONE',  ( -9.787531504996566615E-17, 0.3996062992125985480, -0.5492125984251968740 ) ) ;
#40791 = CARTESIAN_POINT ( 'NONE',  ( -0.5380577427821514602, -0.4281496062992127816, -0.4176697321401328100 ) ) ;
#40792 = CARTESIAN_POINT ( 'NONE',  ( 0.2362204724409449064, 0.4091458600556404646, -0.1443569553805774397 ) ) ;
#40793 = CARTESIAN_POINT ( 'NONE',  ( -0.3392501089628019995, 0.1958661417322832277, -2.315616797900262647 ) ) ;
#40794 = CARTESIAN_POINT ( 'NONE',  ( -1.548556430446193399, -0.5023911411419708095, -0.1820866141732282451 ) ) ;
#40795 = CARTESIAN_POINT ( 'NONE',  ( 0.7020997375328090762, -0.05778040916215560624, -0.4822834645669293319 ) ) ;
#40796 = CARTESIAN_POINT ( 'NONE',  ( 0.8923884514435703741, 0.2306618581243848609, 0.2411417322834645549 ) ) ;
#40797 = CARTESIAN_POINT ( 'NONE',  ( -0.2690288713910754526, -0.5511811023622046335, 0.09757992244046803654 ) ) ;
#40798 = CARTESIAN_POINT ( 'NONE',  ( 0.2165354330708668673, 0.1660481256975883668, -0.3530559997133364547 ) ) ;
#40799 = CARTESIAN_POINT ( 'NONE',  ( 0.1265901696524989462, 0.4724409448818897572, -2.117454068241469756 ) ) ;
#40800 = CARTESIAN_POINT ( 'NONE',  ( -0.02624671916010428221, 0.1283753931104746893, -0.1820866141732285504 ) ) ;
#40801 = CARTESIAN_POINT ( 'NONE',  ( -0.3608923884514428360, -0.6692913385826773087, -0.1292274648535924053 ) ) ;
#40802 = VECTOR ( 'NONE', #67704, 39.37007874015748143 ) ;
#40803 = CARTESIAN_POINT ( 'NONE',  ( -0.3949938075777409963, -7.255918531996591613E-17, -2.005905511811023612 ) ) ;
#40804 = CARTESIAN_POINT ( 'NONE',  ( -1.515748031496062076, 0.1660481256975883668, -0.3530559997133364547 ) ) ;
#40805 = CARTESIAN_POINT ( 'NONE',  ( 0.05905511811023681640, 0.07958543189024071263, -0.2665933059059888421 ) ) ;
#40806 = CARTESIAN_POINT ( 'NONE',  ( 1.384514435695538559, 0.1771653543307087075, -0.09757992244046823083 ) ) ;
#40807 = CARTESIAN_POINT ( 'NONE',  ( -0.9645669291338575535, -0.5400638737290844871, 0.3530559997133364547 ) ) ;
#40808 = CARTESIAN_POINT ( 'NONE',  ( -0.6299212598425188991, -0.1870078740157480601, -0.3641732283464567677 ) ) ;
#40809 = FACE_OUTER_BOUND ( 'NONE', #24903, .T. ) ;
#40810 = CARTESIAN_POINT ( 'NONE',  ( -0.6561679790026240244, -0.6046776061558807314, 0.2411417322834647770 ) ) ;
#40811 = CARTESIAN_POINT ( 'NONE',  ( -0.7742782152230962556, -0.4281496062992127816, -0.4176697321401328100 ) ) ;
#40812 = CARTESIAN_POINT ( 'NONE',  ( 0.1574803149606306130, -0.1870078740157480879, -0.4822834645669291653 ) ) ;
#40813 = CARTESIAN_POINT ( 'NONE',  ( 0.1070741851644053388, 0.3996062992125986035, -2.432414698162729039 ) ) ;
#40814 =( BOUNDED_CURVE ( )  B_SPLINE_CURVE ( 1, ( #4997, #50417 ),
 .UNSPECIFIED., .F., .F. ) 
 B_SPLINE_CURVE_WITH_KNOTS ( ( 2, 2 ),
 ( 3.469446951953614189E-18, 0.002000000000000005246 ),
 .UNSPECIFIED. ) 
 CURVE ( )  GEOMETRIC_REPRESENTATION_ITEM ( )  RATIONAL_B_SPLINE_CURVE ( ( 0.9875488213027527884, 0.9875488213027527884 ) ) 
 REPRESENTATION_ITEM ( '' )  );
#40815 = CARTESIAN_POINT ( 'NONE',  ( -0.1049643490035301746, -0.3917322834645670659, -2.041975434874328865 ) ) ;
#40816 = CARTESIAN_POINT ( 'NONE',  ( -0.5314960629921124946, 2.740199102106095186, -3.870235431238102208 ) ) ;
#40817 = CARTESIAN_POINT ( 'NONE',  ( 0.3346456692913393205, -0.4536011799217368745, -0.2665933059059886201 ) ) ;
#40818 = CARTESIAN_POINT ( 'NONE',  ( 1.095800524934383846, -0.3162353388693405765, 0.4822834645669290543 ) ) ;
#40819 = CARTESIAN_POINT ( 'NONE',  ( -1.108923884514435132, -0.2845877964562159024, 0.3641732283464567677 ) ) ;
#40820 = CARTESIAN_POINT ( 'NONE',  ( 1.141732283464567788, -0.6692913385826771977, 8.415575281601705876E-17 ) ) ;
#40821 = CARTESIAN_POINT ( 'NONE',  ( -1.213910761154854745, 0.1771653543307087075, -0.09757992244046823083 ) ) ;
#40822 = CARTESIAN_POINT ( 'NONE',  ( -0.4133858267716528645, 0.1660481256975883668, -0.3530559997133364547 ) ) ;
#40823 = CARTESIAN_POINT ( 'NONE',  ( 0.2427821522309719648, -0.08942795157527998196, 0.3641732283464567121 ) ) ;
#40824 = CARTESIAN_POINT ( 'NONE',  ( 0.4724409448818898682, 2.892866454678787531E-17, -0.9055118110236221041 ) ) ;
#40825 = CARTESIAN_POINT ( 'NONE',  ( 0.7086614173228352742, -0.1870078740157480601, -0.3641732283464567677 ) ) ;
#40826 = EDGE_CURVE ( 'NONE', #79281, #28871, #47971, .T. ) ;
#40827 = CARTESIAN_POINT ( 'NONE',  ( 0.1574803149606306130, -0.1870078740157480879, -0.4822834645669291653 ) ) ;
#40828 = CARTESIAN_POINT ( 'NONE',  ( 0.3460692066303958092, 0.1998031496062993018, -0.2080052493438320216 ) ) ;
#40829 = EDGE_CURVE ( 'NONE', #21005, #36505, #52287, .T. ) ;
#40830 = CARTESIAN_POINT ( 'NONE',  ( -0.8333333333333323711, -0.6692913385826773087, -0.1292274648535924053 ) ) ;
#40831 = CARTESIAN_POINT ( 'NONE',  ( 0.3917322834645670104, 2.398668435337828261E-17, -1.462598425196850460 ) ) ;
#40832 = CARTESIAN_POINT ( 'NONE',  ( 1.076115485564305141, -0.5023911411419708095, 0.1820866141732285504 ) ) ;
#40833 = CARTESIAN_POINT ( 'NONE',  ( 0.5708661417322842269, 0.1660481256975885056, 0.3530559997133364547 ) ) ;
#40834 = CARTESIAN_POINT ( 'NONE',  ( -0.2755905511811015396, -0.6692913385826771977, 8.415575281601705876E-17 ) ) ;
#40835 = CARTESIAN_POINT ( 'NONE',  ( -0.2559055118110227234, -0.4536011799217367080, 0.2665933059059888421 ) ) ;
#40836 = LINE ( 'NONE', #21069, #48084 ) ;
#40837 = CARTESIAN_POINT ( 'NONE',  ( 0.1574803149606306130, -0.1870078740157480601, -0.3641732283464567677 ) ) ;
#40838 = CARTESIAN_POINT ( 'NONE',  ( 0.2493438320209980519, 0.05413385826771666132, 0.4176697321401328100 ) ) ;
#40839 = CARTESIAN_POINT ( 'NONE',  ( -0.5511811023622041894, -0.1870078740157480601, -0.3641732283464567677 ) ) ;
#40840 = CARTESIAN_POINT ( 'NONE',  ( 0.2925321140481932369, 0.2925321140481932369, -1.159448818897637734 ) ) ;
#40841 = CARTESIAN_POINT ( 'NONE',  ( -1.227034120734907141, -0.6692913385826773087, -0.1292274648535924053 ) ) ;
#40842 = CARTESIAN_POINT ( 'NONE',  ( 0.8546455861312993729, 1.722984403643211298E-16, -0.3791483426435174331 ) ) ;
#40843 = ORIENTED_EDGE ( 'NONE', *, *, #15427, .F. ) ;
#40844 = CARTESIAN_POINT ( 'NONE',  ( -1.246719160104986512, -0.004921259842519576551, 0.3153832671262227771 ) ) ;
#40845 = CARTESIAN_POINT ( 'NONE',  ( -0.2296587926509179312, -0.3162353388693409650, -0.4822834645669289433 ) ) ;
#40846 = CARTESIAN_POINT ( 'NONE',  ( 0.3972027188793966213, 0.005815251566292155977, -1.220472440942466319 ) ) ;
#40847 = CARTESIAN_POINT ( 'NONE',  ( -0.9711286089238838626, 0.2306618581243847221, -0.2411417322834647770 ) ) ;
#40848 = DIRECTION ( 'NONE',  ( 1.000000000000000000, -0.000000000000000000, -0.000000000000000000 ) ) ;
#40849 = EDGE_CURVE ( 'NONE', #25966, #5694, #9491, .T. ) ;
#40850 = CARTESIAN_POINT ( 'NONE',  ( -0.9186351706036736120, 0.2306618581243848609, 0.2411417322834645549 ) ) ;
#40851 = CARTESIAN_POINT ( 'NONE',  ( 0.8464566929133866546, -0.5400638737290844871, 0.3530559997133364547 ) ) ;
#40852 = DIRECTION ( 'NONE',  ( 0.000000000000000000, 0.000000000000000000, 1.000000000000000000 ) ) ;
#40853 = CARTESIAN_POINT ( 'NONE',  ( 1.528871391076116026, -0.6692913385826773087, -0.1292274648535924053 ) ) ;
#40854 = CARTESIAN_POINT ( 'NONE',  ( 0.2524317427257167790, -0.1533591454305971991, 5.791393970467345831 ) ) ;
#40855 = EDGE_CURVE ( 'NONE', #37713, #72462, #74255, .T. ) ;
#40856 = CARTESIAN_POINT ( 'NONE',  ( -1.266404199475064773, -0.3162353388693405765, 0.4822834645669290543 ) ) ;
#40857 = CARTESIAN_POINT ( 'NONE',  ( -9.787531504996567848E-17, 0.3996062992125986035, -0.4724409448818898127 ) ) ;
#40858 = ORIENTED_EDGE ( 'NONE', *, *, #44641, .F. ) ;
#40859 = CARTESIAN_POINT ( 'NONE',  ( -0.5118110236220466680, 0.1771653543307087630, 0.000000000000000000 ) ) ;
#40861 = CARTESIAN_POINT ( 'NONE',  ( 0.1958661417322834775, 0.3392501089628018884, -2.341207349081364963 ) ) ;
#40860 = CIRCLE ( 'NONE', #51577, 2.637795275590551380 ) ;
#40862 = ORIENTED_EDGE ( 'NONE', *, *, #64032, .T. ) ;
#40863 = CARTESIAN_POINT ( 'NONE',  ( 0.8136482939632553313, 0.2306618581243848609, 0.2411417322834645549 ) ) ;
#40865 = CARTESIAN_POINT ( 'NONE',  ( -0.04593175853018302557, -0.6692913385826773087, -0.1292274648535924053 ) ) ;
#40864 = PRODUCT_DEFINITION ( 'UNKNOWN', '', #77247, #40301 ) ;
#40866 = CARTESIAN_POINT ( 'NONE',  ( -0.8727034120734901146, -0.3162353388693405765, 0.4822834645669290543 ) ) ;
#40867 = CARTESIAN_POINT ( 'NONE',  ( 1.555118110236221041, 0.1660481256975883668, -0.3530559997133364547 ) ) ;
#40868 = CARTESIAN_POINT ( 'NONE',  ( -0.8530183727034112984, -0.004921259842519576551, 0.3153832671262227771 ) ) ;
#40869 = CARTESIAN_POINT ( 'NONE',  ( 0.1265901696524990572, -0.4724409448818897017, -2.051837270341206665 ) ) ;
#40870 = CARTESIAN_POINT ( 'NONE',  ( 0.5314960629921267055, -0.5400638737290844871, 0.3530559997133364547 ) ) ;
#40871 = CARTESIAN_POINT ( 'NONE',  ( 0.5577427821522314977, -0.2845877964562161244, -0.3641732283464567121 ) ) ;
#40872 = CARTESIAN_POINT ( 'NONE',  ( -1.023622047244093558, -0.1870078740157479769, 0.4822834645669291653 ) ) ;
#40873 = CARTESIAN_POINT ( 'NONE',  ( -0.3917322834645670659, 0.1049643490035301607, -1.372684096291651556 ) ) ;
#40874 = CARTESIAN_POINT ( 'NONE',  ( -1.443569553805773564, 0.2306618581243847221, -0.2411417322834647770 ) ) ;
#40875 = CARTESIAN_POINT ( 'NONE',  ( -1.699475065616797398, 0.1771653543307087630, 0.09757992244046791164 ) ) ;
#40876 = CARTESIAN_POINT ( 'NONE',  ( 0.8661417322834653598, -0.1870078740157479769, 0.4822834645669291653 ) ) ;
#40877 = CARTESIAN_POINT ( 'NONE',  ( 1.325459317585302665, -0.3690944881889763329, 0.3153832671262228327 ) ) ;
#40878 = VERTEX_POINT ( 'NONE', #81451 ) ;
#40879 = CARTESIAN_POINT ( 'NONE',  ( -0.3917322834645670659, -7.196005306013484475E-17, -2.870754223918321912 ) ) ;
#40880 = CARTESIAN_POINT ( 'NONE',  ( -0.3346456692913377662, 0.1660481256975883668, -0.3530559997133364547 ) ) ;
#40881 = VERTEX_POINT ( 'NONE', #73051 ) ;
#40882 = CARTESIAN_POINT ( 'NONE',  ( 0.4330708661417329575, -0.5511811023622047445, 6.969142054262312111E-17 ) ) ;
#40883 = CARTESIAN_POINT ( 'NONE',  ( -1.358267716535432434, 0.1660481256975883668, -0.3530559997133364547 ) ) ;
#40884 = CARTESIAN_POINT ( 'NONE',  ( 0.8530183727034126306, 0.05413385826771626580, -0.4176697321401330321 ) ) ;
#40885 = CARTESIAN_POINT ( 'NONE',  ( 1.023622047244095112, -0.1870078740157480879, -0.4822834645669291653 ) ) ;
#40886 = CARTESIAN_POINT ( 'NONE',  ( 0.09842519685039434474, -0.5400638737290845981, -0.3530559997133363437 ) ) ;
#40887 = CARTESIAN_POINT ( 'NONE',  ( -0.3608923884514428360, 0.2952755905511811885, 0.1292274648535926551 ) ) ;
#40888 = CARTESIAN_POINT ( 'NONE',  ( 0.3392501089628018884, -0.1958661417322834220, -2.236876640419947826 ) ) ;
#40889 = CARTESIAN_POINT ( 'NONE',  ( -1.482939632545930975, -0.4281496062992127816, -0.4176697321401328100 ) ) ;
#40890 = CARTESIAN_POINT ( 'NONE',  ( -0.8005249343832011588, 0.05413385826771626580, -0.4176697321401330321 ) ) ;
#40891 = EDGE_CURVE ( 'NONE', #18593, #18898, #10129, .T. ) ;
#40892 = CARTESIAN_POINT ( 'NONE',  ( -0.3543307086614165824, 0.1771653543307087630, 0.000000000000000000 ) ) ;
#40893 = CARTESIAN_POINT ( 'NONE',  ( 1.161417322834646493, -0.5400638737290844871, 0.3530559997133364547 ) ) ;
#40894 = CARTESIAN_POINT ( 'NONE',  ( 1.456692913385827515, -0.6692913385826771977, 8.415575281601705876E-17 ) ) ;
#40895 = CARTESIAN_POINT ( 'NONE',  ( -0.5708661417322828946, 0.1660481256975883668, -0.3530559997133364547 ) ) ;
#40896 = CARTESIAN_POINT ( 'NONE',  ( -0.1070741851644056997, 0.3996062992125984925, 0.07414698162729659037 ) ) ;
#40897 = CARTESIAN_POINT ( 'NONE',  ( 0.6561679790026253567, 0.2306618581243848609, 0.2411417322834645549 ) ) ;
#40898 = CARTESIAN_POINT ( 'NONE',  ( 0.2925321140481932369, 0.2925321140481932369, -1.712598425196850460 ) ) ;
#40899 = CARTESIAN_POINT ( 'NONE',  ( 1.595398199321655275, 1.034147571970761126, 0.1559797534342493575 ) ) ;
#40900 = CARTESIAN_POINT ( 'NONE',  ( -0.05249343832020911260, 0.2306618581243848609, 0.2411417322834645549 ) ) ;
#40901 = CARTESIAN_POINT ( 'NONE',  ( -1.115485564304461219, -0.004921259842519870586, -0.3153832671262229437 ) ) ;
#40903 = CARTESIAN_POINT ( 'NONE',  ( -0.5314960629921323676, 2.755905511811024056, 1.813482582612291560 ) ) ;
#40902 = CARTESIAN_POINT ( 'NONE',  ( 1.135170603674541256, -0.5511811023622048555, -0.09757992244046775898 ) ) ;
#40904 = CARTESIAN_POINT ( 'NONE',  ( 0.4724409448818898682, 2.892866454678787531E-17, -0.8248031496062991907 ) ) ;
#40905 = CARTESIAN_POINT ( 'NONE',  ( 1.220472440944882608, 0.1771653543307087630, 0.000000000000000000 ) ) ;
#40906 = CARTESIAN_POINT ( 'NONE',  ( 1.266404199475066328, -0.05778040916215522460, 0.4822834645669289988 ) ) ;
#40907 = CARTESIAN_POINT ( 'NONE',  ( -0.3420746716998660508, -0.1974969037888706924, -0.2867454068241469534 ) ) ;
#40908 = CARTESIAN_POINT ( 'NONE',  ( -0.2034120734908131112, -0.6692913385826773087, -0.1292274648535924053 ) ) ;
#40909 = DIRECTION ( 'NONE',  ( -0.8660254037844433705, 0.000000000000000000, 0.4999999999999920064 ) ) ;
#40910 = CONICAL_SURFACE ( 'NONE', #27496, 0.1771653543307086798, 0.7853981633974482790 ) ;
#40911 = CARTESIAN_POINT ( 'NONE',  ( 1.227034120734908917, -0.5511811023622046335, 0.09757992244046803654 ) ) ;
#40912 = CARTESIAN_POINT ( 'NONE',  ( -0.1968503937007867743, -0.6692913385826771977, 8.415575281601705876E-17 ) ) ;
#40913 = CARTESIAN_POINT ( 'NONE',  ( 4.837279021331061486E-17, -0.3949938075777409963, -0.3129921259842520231 ) ) ;
#40914 = CARTESIAN_POINT ( 'NONE',  ( 1.082677165354331228, 0.1660481256975883668, -0.3530559997133364547 ) ) ;
#40915 = CARTESIAN_POINT ( 'NONE',  ( 0.3740157480314966754, 0.1660481256975883668, -0.3530559997133364547 ) ) ;
#40916 = CARTESIAN_POINT ( 'NONE',  ( 0.5774278215223104249, 0.1283753931104748280, 0.1820866141732283561 ) ) ;
#40917 = DIRECTION ( 'NONE',  ( 0.000000000000000000, 1.000000000000000000, -0.000000000000000000 ) ) ;
#40918 = CARTESIAN_POINT ( 'NONE',  ( 0.6167979002624679463, -0.004921259842519870586, -0.3153832671262229437 ) ) ;
#40919 = CARTESIAN_POINT ( 'NONE',  ( -2.795275590551183242, 1.574803149606300412, -1.327125379919507468E-16 ) ) ;
#40920 = EDGE_CURVE ( 'NONE', #11040, #36023, #15401, .T. ) ;
#40921 = CARTESIAN_POINT ( 'NONE',  ( -0.3996062992125985480, -7.340648628747423112E-17, -1.218503937007874072 ) ) ;
#40922 = CARTESIAN_POINT ( 'NONE',  ( 0.6102362204724416372, 0.1660481256975883668, -0.3530559997133364547 ) ) ;
#40923 = CARTESIAN_POINT ( 'NONE',  ( -0.2867679344610365999, 0.2867679344610364889, -0.9566929133858265155 ) ) ;
#40924 = CARTESIAN_POINT ( 'NONE',  ( 0.4606732211678791766, 2.793565526369266028, 0.5309055118110233007 ) ) ;
#40925 = CARTESIAN_POINT ( 'NONE',  ( -0.4724409448818898682, -8.678599364036362592E-17, -0.4311023622047244208 ) ) ;
#40926 = CARTESIAN_POINT ( 'NONE',  ( 0.07874015748031558404, -0.1870078740157480601, -0.3641732283464567677 ) ) ;
#40927 = AXIS2_PLACEMENT_3D ( 'NONE', #79749, #9440, #80990 ) ;
#40928 = CARTESIAN_POINT ( 'NONE',  ( -0.04593175853018302557, 0.2952755905511811885, 0.1292274648535926551 ) ) ;
#40929 = CARTESIAN_POINT ( 'NONE',  ( 1.318897637795276356, -0.4536011799217367080, 0.2665933059059888421 ) ) ;
#40930 = CARTESIAN_POINT ( 'NONE',  ( -1.496062992125983815, -0.1870078740157480601, -0.3641732283464567677 ) ) ;
#40931 = CARTESIAN_POINT ( 'NONE',  ( -1.148293963254592542, -0.6692913385826773087, -0.1292274648535924053 ) ) ;
#40932 = CARTESIAN_POINT ( 'NONE',  ( 0.6167979002624679463, 0.05413385826771626580, -0.4176697321401330321 ) ) ;
#40933 = CARTESIAN_POINT ( 'NONE',  ( 1.627296587926509996, -0.6046776061558807314, 0.2411417322834647770 ) ) ;
#40934 = ADVANCED_FACE ( 'NONE', ( #23352 ), #62074, .F. ) ;
#40935 = CARTESIAN_POINT ( 'NONE',  ( -0.03443470937343537375, 1.064243487142137568, -1.440673310089392478 ) ) ;
#40936 = CARTESIAN_POINT ( 'NONE',  ( 0.4593175853018379162, -0.4281496062992124485, 0.4176697321401328655 ) ) ;
#40937 = CARTESIAN_POINT ( 'NONE',  ( -0.3460692066303960313, 0.1998031496062989965, 0.2119422572178477349 ) ) ;
#40938 = CARTESIAN_POINT ( 'NONE',  ( 1.587926509186352586, -0.4281496062992127816, -0.4176697321401328100 ) ) ;
#40939 = CARTESIAN_POINT ( 'NONE',  ( 0.9842519685039378130, -0.6692913385826771977, 8.415575281601705876E-17 ) ) ;
#40940 = CARTESIAN_POINT ( 'NONE',  ( -1.391076115485563758, 0.1283753931104748280, 0.1820866141732283561 ) ) ;
#40941 = CARTESIAN_POINT ( 'NONE',  ( 1.259842519685040019, -0.1870078740157480601, -0.3641732283464567677 ) ) ;
#40942 = CARTESIAN_POINT ( 'NONE',  ( -1.614173228346455824, 0.1771653543307087630, 0.000000000000000000 ) ) ;
#40943 = CARTESIAN_POINT ( 'NONE',  ( -0.7480314960629914633, -0.5511811023622047445, 6.969142054262312111E-17 ) ) ;
#40944 = CARTESIAN_POINT ( 'NONE',  ( 1.509186351706037543, -0.4281496062992127816, -0.4176697321401328100 ) ) ;
#40945 = CARTESIAN_POINT ( 'NONE',  ( 0.6496062992125991586, 0.07958543189024085140, 0.2665933059059887866 ) ) ;
#40946 = CARTESIAN_POINT ( 'NONE',  ( 0.3215223097112867578, -0.3162353388693409650, -0.4822834645669289433 ) ) ;
#40947 = CARTESIAN_POINT ( 'NONE',  ( 1.082677165354331228, -0.5400638737290844871, 0.3530559997133364547 ) ) ;
#40948 = CARTESIAN_POINT ( 'NONE',  ( -0.4330708661417315697, -0.6692913385826771977, 8.415575281601705876E-17 ) ) ;
#40949 = CARTESIAN_POINT ( 'NONE',  ( 0.3412073490813655186, 0.1283753931104748280, 0.1820866141732283561 ) ) ;
#40950 = CARTESIAN_POINT ( 'NONE',  ( 1.036745406824147508, -0.4281496062992127816, -0.4176697321401328100 ) ) ;
#40951 = CARTESIAN_POINT ( 'NONE',  ( -1.561679790026246017, -0.4281496062992127816, -0.4176697321401328100 ) ) ;
#40952 = CARTESIAN_POINT ( 'NONE',  ( -1.030183727034119867, -0.05778040916215560624, -0.4822834645669293319 ) ) ;
#40954 = CARTESIAN_POINT ( 'NONE',  ( -0.1998031496062991907, -0.3460692066303959757, -0.8530183727034120755 ) ) ;
#40953 = CARTESIAN_POINT ( 'NONE',  ( -1.391076115485563758, 0.1283753931104748280, 0.1820866141732283561 ) ) ;
#40955 = CARTESIAN_POINT ( 'NONE',  ( -1.207349081364828880, 0.1539470093639521697, -0.1968503937007875793 ) ) ;
#40956 = CARTESIAN_POINT ( 'NONE',  ( -0.6758530183727028406, 0.2952755905511811885, 0.1292274648535926551 ) ) ;
#40957 = CARTESIAN_POINT ( 'NONE',  ( 0.05905511811023681640, 0.1660481256975883668, -0.3530559997133364547 ) ) ;
#40958 = CARTESIAN_POINT ( 'NONE',  ( -0.3996062992125986035, -7.340648628747425578E-17, -2.874015748031495843 ) ) ;
#40959 = CARTESIAN_POINT ( 'NONE',  ( 0.3420746716998659953, 0.1974969037888705536, -2.335958005249343827 ) ) ;
#40960 = EDGE_LOOP ( 'NONE', ( #49542, #79185, #24729, #79531 ) ) ;
#40961 = B_SPLINE_CURVE_WITH_KNOTS ( 'NONE', 3,
 ( #5679, #44374, #69669, #30118, #74758, #82709, #5276, #56200, #30939, #12421, #56606, #37666, #57013, #11190, #17515, #63753, #57429, #17106, #43147, #68437, #55780, #10777, #62110, #81901, #81488, #24212, #75583, #17922 ),
 .UNSPECIFIED., .F., .F.,
 ( 4, 2, 2, 2, 2, 2, 2, 2, 2, 2, 2, 2, 2, 4 ),
 ( 0.01911876323414707021, 0.02031104709728144900, 0.02150333096041582431, 0.02269561482355020310, 0.02388789868668458188, 0.02508018254981896067, 0.02627246641295333945, 0.02746475027608771824, 0.02865703413922209702, 0.02984931800235647581, 0.03104160186549084766, 0.03342616959175960523, 0.03581073731802836280, 0.03819530504429712037 ),
 .UNSPECIFIED. ) ;
#40962 = CARTESIAN_POINT ( 'NONE',  ( -0.2867679344610364334, -0.2867679344610367109, -1.153543307086613900 ) ) ;
#40963 = CARTESIAN_POINT ( 'NONE',  ( 1.135170603674541256, 0.2952755905511811885, 0.1292274648535926551 ) ) ;
#40964 = PRODUCT_DEFINITION_FORMATION_WITH_SPECIFIED_SOURCE ( 'ANY', '', #70817, .NOT_KNOWN. ) ;
#40965 = CARTESIAN_POINT ( 'NONE',  ( -0.2465595919006988435, -1.283732188437465593E-15, -0.4281993546915532911 ) ) ;
#40966 = CARTESIAN_POINT ( 'NONE',  ( -1.187664041994750175, -0.08942795157528024563, -0.3641732283464568787 ) ) ;
#40967 = CARTESIAN_POINT ( 'NONE',  ( 1.423884514435696413, -0.3162353388693409650, -0.4822834645669289433 ) ) ;
#40968 = CARTESIAN_POINT ( 'NONE',  ( -1.469816272965878357, -0.6046776061558809534, -0.2411417322834644161 ) ) ;
#40969 = CARTESIAN_POINT ( 'NONE',  ( 0.3917322834645669549, 2.398668435337827645E-17, -0.1981434138769535558 ) ) ;
#40970 = CARTESIAN_POINT ( 'NONE',  ( 0.1115485564304470323, 0.2952755905511811885, 0.1292274648535926551 ) ) ;
#40971 = CARTESIAN_POINT ( 'NONE',  ( -0.4265091863517051496, 0.1771653543307087075, -0.09757992244046823083 ) ) ;
#40972 = CARTESIAN_POINT ( 'NONE',  ( 0.6627296587926515548, 0.2952755905511811885, 0.1292274648535926551 ) ) ;
#40973 = CARTESIAN_POINT ( 'NONE',  ( 0.5577427821522314977, -0.3162353388693409650, -0.4822834645669289433 ) ) ;
#40974 = CARTESIAN_POINT ( 'NONE',  ( 0.2389359915688108460, 1.126391250279107137, 1.096629699561409987 ) ) ;
#40975 = CARTESIAN_POINT ( 'NONE',  ( 4.893765752498283924E-17, -0.3996062992125986035, -2.913385826771653697 ) ) ;
#40976 = CARTESIAN_POINT ( 'NONE',  ( 0.2867679344610366554, -0.2867679344610365999, -1.827447137304149205 ) ) ;
#40977 = CARTESIAN_POINT ( 'NONE',  ( 0.8398950131233602345, -0.6046776061558807314, 0.2411417322834647770 ) ) ;
#40978 = CARTESIAN_POINT ( 'NONE',  ( -0.05249343832020938322, -0.6046776061558809534, -0.2411417322834644161 ) ) ;
#40979 = CARTESIAN_POINT ( 'NONE',  ( -0.9842519685039360366, 0.2952755905511811885, 0.000000000000000000 ) ) ;
#40980 = EDGE_CURVE ( 'NONE', #64172, #70570, #65283, .T. ) ;
#40982 = CARTESIAN_POINT ( 'NONE',  ( -1.640419947506561060, 0.05413385826771666132, 0.4176697321401328100 ) ) ;
#40981 = AXIS2_PLACEMENT_3D ( 'NONE', #75582, #37265, #70065 ) ;
#40983 = CARTESIAN_POINT ( 'NONE',  ( 0.6889763779527566800, -0.5400638737290844871, 0.3530559997133364547 ) ) ;
#40984 = CARTESIAN_POINT ( 'NONE',  ( -0.1958661417322836718, 0.3392501089628017219, -0.4127296587926510552 ) ) ;
#40985 = CARTESIAN_POINT ( 'NONE',  ( -0.1509186351706028884, -0.05778040916215522460, 0.4822834645669289988 ) ) ;
#40986 = CARTESIAN_POINT ( 'NONE',  ( 0.4724409448818904789, -0.1870078740157480879, -0.4822834645669291653 ) ) ;
#40987 = CARTESIAN_POINT ( 'NONE',  ( 0.1640419947506569498, -0.3162353388693409650, -0.4822834645669289433 ) ) ;
#40988 = EDGE_CURVE ( 'NONE', #62471, #71224, #1727, .T. ) ;
#40989 = CARTESIAN_POINT ( 'NONE',  ( 0.7939632545931766261, -0.2845877964562161244, -0.3641732283464567121 ) ) ;
#40990 = CARTESIAN_POINT ( 'NONE',  ( -1.541994750656167090, 0.2952755905511811885, 0.1292274648535926551 ) ) ;
#40991 = CARTESIAN_POINT ( 'NONE',  ( -1.581364829396324945, -0.3162353388693405765, 0.4822834645669290543 ) ) ;
#40992 = CARTESIAN_POINT ( 'NONE',  ( 0.5577427821522314977, -0.3162353388693409650, -0.4822834645669289433 ) ) ;
#40993 = DIRECTION ( 'NONE',  ( -0.000000000000000000, -1.000000000000000000, -0.000000000000000000 ) ) ;
#40994 = CARTESIAN_POINT ( 'NONE',  ( 0.1958661417322836440, -0.3392501089628017219, -2.288713910761154935 ) ) ;
#40995 = EDGE_LOOP ( 'NONE', ( #39952, #69524, #27836, #42826 ) ) ;
#40996 = CARTESIAN_POINT ( 'NONE',  ( -0.3996062992125987146, 0.1070741851644051862, -0.5052493438320209140 ) ) ;
#40997 = EDGE_LOOP ( 'NONE', ( #31525, #77543, #4951, #15718, #14364 ) ) ;
#40998 = CARTESIAN_POINT ( 'NONE',  ( 1.227034120734908917, 0.2952755905511810774, -0.1292274648535930714 ) ) ;
#40999 = CARTESIAN_POINT ( 'NONE',  ( 0.4461942257217855201, -0.5023911411419708095, 0.1820866141732285504 ) ) ;
#41000 = CARTESIAN_POINT ( 'NONE',  ( 0.6102362204724416372, 0.1660481256975883391, -0.3530559997133364547 ) ) ;
#41001 = DIRECTION ( 'NONE',  ( 0.000000000000000000, 1.000000000000000000, 0.000000000000000000 ) ) ;
#41002 = CARTESIAN_POINT ( 'NONE',  ( -0.1049643490035307020, 0.3917322834645669549, -1.351049868766404538 ) ) ;
#41003 = CARTESIAN_POINT ( 'NONE',  ( 0.3460692066303958092, 0.1998031496062993018, -1.940288713910761187 ) ) ;
#41004 = CARTESIAN_POINT ( 'NONE',  ( -1.601049868766403650, 0.2306618581243847221, -0.2411417322834647770 ) ) ;
#41005 = CARTESIAN_POINT ( 'NONE',  ( -0.3805774278215216522, -0.4281496062992127816, -0.4176697321401328100 ) ) ;
#41006 = CARTESIAN_POINT ( 'NONE',  ( 1.102362204724410155, -0.1870078740157479769, 0.4822834645669291653 ) ) ;
#41007 = VERTEX_POINT ( 'NONE', #28842 ) ;
#41008 = CARTESIAN_POINT ( 'NONE',  ( 1.607611548556431069, -0.5511811023622048555, -0.09757992244046775898 ) ) ;
#41009 = SHAPE_DEFINITION_REPRESENTATION ( #58020, #33107 ) ;
#41010 = CARTESIAN_POINT ( 'NONE',  ( 1.620734908136483465, -0.5511811023622046335, 0.09757992244046803654 ) ) ;
#41011 = DIRECTION ( 'NONE',  ( 0.000000000000000000, 8.326672684688674053E-16, 1.000000000000000000 ) ) ;
#41012 = CARTESIAN_POINT ( 'NONE',  ( -1.135170603674539924, 0.1771653543307087075, -0.09757992244046823083 ) ) ;
#41013 = CARTESIAN_POINT ( 'NONE',  ( 0.3917322834645670104, 2.398668435337828261E-17, 0.04724409448818902429 ) ) ;
#41014 = CARTESIAN_POINT ( 'NONE',  ( 0.05249343832021075018, -0.6046776061558807314, 0.2411417322834647770 ) ) ;
#41016 = CARTESIAN_POINT ( 'NONE',  ( -0.5314960629921122726, 2.559055118110236560, -3.937007874015763687 ) ) ;
#41015 = CARTESIAN_POINT ( 'NONE',  ( 1.489501312335958172, -0.3162353388693405765, 0.4822834645669290543 ) ) ;
#41017 = CARTESIAN_POINT ( 'NONE',  ( -0.7611548556430438595, 0.1283753931104748280, 0.1820866141732283561 ) ) ;
#41018 = CARTESIAN_POINT ( 'NONE',  ( 0.6561679790026253567, -0.6046776061558809534, -0.2411417322834644161 ) ) ;
#41019 = CARTESIAN_POINT ( 'NONE',  ( 1.482939632545932307, -0.004921259842519870586, -0.3153832671262229437 ) ) ;
#41020 = CARTESIAN_POINT ( 'NONE',  ( 0.2867679344610365999, 0.2867679344610365999, -1.320190657971441528 ) ) ;
#41021 = CARTESIAN_POINT ( 'NONE',  ( -0.8858267716535425107, 0.07958543189024071263, -0.2665933059059888421 ) ) ;
#41022 = CARTESIAN_POINT ( 'NONE',  ( -1.574803149606298192, -0.1870078740157480601, -0.3641732283464567677 ) ) ;
#41023 = FACE_OUTER_BOUND ( 'NONE', #3319, .T. ) ;
#41024 = CARTESIAN_POINT ( 'NONE',  ( 0.4133858267716541968, -0.5400638737290845981, -0.3530559997133363437 ) ) ;
#41025 = CARTESIAN_POINT ( 'NONE',  ( -1.089238845144356427, -0.3690944881889765550, -0.3153832671262227771 ) ) ;
#41026 = CARTESIAN_POINT ( 'NONE',  ( -0.4265091863517051496, 0.1771653543307087075, -0.09757992244046823083 ) ) ;
#41027 = CARTESIAN_POINT ( 'NONE',  ( -0.5052493438320203589, -0.6692913385826771977, 0.1292274648535927661 ) ) ;
#41028 = CARTESIAN_POINT ( 'NONE',  ( 1.660104986876641320, -0.05778040916215522460, 0.4822834645669289988 ) ) ;
#41029 = CARTESIAN_POINT ( 'NONE',  ( -0.3917322834645670659, -7.196005306013484475E-17, -0.03610855462698352170 ) ) ;
#41030 = CARTESIAN_POINT ( 'NONE',  ( 0.7480314960629927956, -0.6692913385826771977, 8.415575281601705876E-17 ) ) ;
#41031 = FACE_OUTER_BOUND ( 'NONE', #36921, .T. ) ;
#41032 = CARTESIAN_POINT ( 'NONE',  ( -1.157146581871515012E-16, 0.4724409448818898682, -1.651574803149606474 ) ) ;
#41033 = CARTESIAN_POINT ( 'NONE',  ( -0.5905511811023615998, 0.2952755905511811885, 0.000000000000000000 ) ) ;
#41034 = CARTESIAN_POINT ( 'NONE',  ( -0.2887139107611542133, 0.1283753931104748280, 0.1820866141732283561 ) ) ;
#41035 = CARTESIAN_POINT ( 'NONE',  ( -1.325459317585300889, 0.05413385826771666132, 0.4176697321401328100 ) ) ;
#41036 = CARTESIAN_POINT ( 'NONE',  ( 0.4527559055118117182, 0.07958543189024071263, -0.2665933059059888421 ) ) ;
#41037 = VECTOR ( 'NONE', #23372, 39.37007874015748143 ) ;
#41038 = CARTESIAN_POINT ( 'NONE',  ( -0.5249343832020990641, -0.5023911411419708095, -0.1820866141732282451 ) ) ;
#41039 = CARTESIAN_POINT ( 'NONE',  ( -0.9908136482939626788, -0.6692913385826773087, -0.1292274648535924053 ) ) ;
#41040 = CARTESIAN_POINT ( 'NONE',  ( -1.377952755905511140, 0.2952755905511811885, 0.000000000000000000 ) ) ;
#41041 = CARTESIAN_POINT ( 'NONE',  ( 1.391076115485564868, 0.2306618581243847221, -0.2411417322834647770 ) ) ;
#41042 = DIRECTION ( 'NONE',  ( -3.491481338843133355E-15, -0.000000000000000000, 1.000000000000000000 ) ) ;
#41043 = CARTESIAN_POINT ( 'NONE',  ( 1.036745406824147731, -0.004921259842519576551, 0.3153832671262227771 ) ) ;
#41044 = CARTESIAN_POINT ( 'NONE',  ( 0.4461942257217856311, 0.2306618581243847221, -0.2411417322834647770 ) ) ;
#41045 = CARTESIAN_POINT ( 'NONE',  ( -1.813482582612293559, 2.755905511811024056, 0.5314960629921260393 ) ) ;
#41046 = CARTESIAN_POINT ( 'NONE',  ( 1.345144356955381593, -0.2845877964562161244, -0.3641732283464567121 ) ) ;
#41047 = ORIENTED_EDGE ( 'NONE', *, *, #3407, .T. ) ;
#41048 = CARTESIAN_POINT ( 'NONE',  ( -0.3420746716998660508, -0.1974969037888706924, 0.1856955380577428039 ) ) ;
#41049 = CARTESIAN_POINT ( 'NONE',  ( -1.148293963254592542, 0.1771653543307087630, 0.09757992244046791164 ) ) ;
#41050 = CARTESIAN_POINT ( 'NONE',  ( -0.4265091863517051496, -0.6692913385826771977, 0.1292274648535927661 ) ) ;
#41051 = CARTESIAN_POINT ( 'NONE',  ( 0.3740157480314966754, 0.1660481256975883668, -0.3530559997133364547 ) ) ;
#41052 = CARTESIAN_POINT ( 'NONE',  ( -1.653543307086613234, -0.1870078740157480601, -0.3641732283464567677 ) ) ;
#41053 = CARTESIAN_POINT ( 'NONE',  ( 0.2925321140481932369, -0.2925321140481931814, -2.222440944881889813 ) ) ;
#41054 = CARTESIAN_POINT ( 'NONE',  ( -1.410761154855642463, -0.05778040916215522460, 0.4822834645669289988 ) ) ;
#41055 = CARTESIAN_POINT ( 'NONE',  ( 0.4002624671916016896, -0.05778040916215522460, 0.4822834645669289988 ) ) ;
#41056 = CARTESIAN_POINT ( 'NONE',  ( 0.03280839895013198948, -0.6692913385826773087, -0.1292274648535924053 ) ) ;
#41057 = CARTESIAN_POINT ( 'NONE',  ( 1.246719160104987623, -0.4281496062992124485, 0.4176697321401328655 ) ) ;
#41058 = CARTESIAN_POINT ( 'NONE',  ( -0.3996062992125985480, -7.340648628747423112E-17, -1.061023622047243986 ) ) ;
#41059 = CARTESIAN_POINT ( 'NONE',  ( -0.1070741851644051862, -0.3996062992125987146, -1.332020997375328086 ) ) ;
#41060 = CARTESIAN_POINT ( 'NONE',  ( -9.674558042662121740E-17, 0.3949938075777409963, -1.102362204724409711 ) ) ;
#41061 = CARTESIAN_POINT ( 'NONE',  ( 0.1998031496062992740, 0.3460692066303959757, -2.506561679790026087 ) ) ;
#41062 = DIRECTION ( 'NONE',  ( 3.114085624724525612E-16, -1.000000000000000000, -5.270319453084425600E-32 ) ) ;
#41063 = CARTESIAN_POINT ( 'NONE',  ( -0.1958661417322836718, 0.3392501089628017219, -0.3202099737532808077 ) ) ;
#41064 = CARTESIAN_POINT ( 'NONE',  ( -0.1181102362204717315, 0.1771653543307087630, 0.000000000000000000 ) ) ;
#41065 = CARTESIAN_POINT ( 'NONE',  ( -0.3805774278215216522, -0.4281496062992127816, -0.4176697321401328100 ) ) ;
#41066 = CARTESIAN_POINT ( 'NONE',  ( 0.9055118110236227702, -0.6692913385826771977, 8.415575281601705876E-17 ) ) ;
#41067 = CARTESIAN_POINT ( 'NONE',  ( 0.3949938075777409963, 2.418639510665530743E-17, -1.769685039370078927 ) ) ;
#41068 = CARTESIAN_POINT ( 'NONE',  ( -0.1640419947506553400, -0.08942795157528024563, -0.3641732283464568787 ) ) ;
#41069 = CARTESIAN_POINT ( 'NONE',  ( -1.174540682414697335, -0.05778040916215522460, 0.4822834645669289988 ) ) ;
#41070 = CARTESIAN_POINT ( 'NONE',  ( 1.515748031496063186, -0.5400638737290845981, -0.3530559997133363437 ) ) ;
#41071 = CARTESIAN_POINT ( 'NONE',  ( 0.4724409448818896462, 0.1265901696524990294, -2.014435695538057569 ) ) ;
#41072 = CARTESIAN_POINT ( 'NONE',  ( 0.3503937007874015075, 0.000000000000000000, -0.3051181102362204856 ) ) ;
#41073 = ORIENTED_EDGE ( 'NONE', *, *, #71071, .T. ) ;
#41074 = EDGE_CURVE ( 'NONE', #24808, #24707, #68354, .T. ) ;
#41075 = ORIENTED_EDGE ( 'NONE', *, *, #60880, .T. ) ;
#41076 = CARTESIAN_POINT ( 'NONE',  ( 1.010498687664042716, 0.05413385826771626580, -0.4176697321401330321 ) ) ;
#41077 = CARTESIAN_POINT ( 'NONE',  ( 1.509186351706037543, -0.3690944881889765550, -0.3153832671262227771 ) ) ;
#41079 = CARTESIAN_POINT ( 'NONE',  ( -1.003937007874014853, 0.1660481256975885056, 0.3530559997133364547 ) ) ;
#41078 = CARTESIAN_POINT ( 'NONE',  ( -1.003937007874014853, 0.07958543189024085140, 0.2665933059059887866 ) ) ;
#41080 = CARTESIAN_POINT ( 'NONE',  ( 4.797336870675655290E-17, -0.3917322834645669549, -2.520978059546244765 ) ) ;
#41081 = DIRECTION ( 'NONE',  ( -8.673617379884021667E-16, 1.000000000000000000, -3.028377322213054317E-30 ) ) ;
#41082 = CARTESIAN_POINT ( 'NONE',  ( 1.391076115485564868, 0.2306618581243847221, -0.2411417322834647770 ) ) ;
#41083 = CARTESIAN_POINT ( 'NONE',  ( -1.548556430446193399, 0.2306618581243848609, 0.2411417322834645549 ) ) ;
#41084 = CARTESIAN_POINT ( 'NONE',  ( -0.2755905511811018171, 0.2952755905511811885, 0.000000000000000000 ) ) ;
#41085 = CARTESIAN_POINT ( 'NONE',  ( -0.01968503937007793844, -0.5400638737290844871, 0.3530559997133364547 ) ) ;
#41086 = CARTESIAN_POINT ( 'NONE',  ( -1.056430446194224881, -0.6692913385826771977, 0.1292274648535927661 ) ) ;
#41087 = CARTESIAN_POINT ( 'NONE',  ( 0.3917322834645669549, 2.398668435337827645E-17, -2.875308768207662347 ) ) ;
#41088 = CARTESIAN_POINT ( 'NONE',  ( -0.006561679790025524116, -0.3162353388693405765, 0.4822834645669290543 ) ) ;
#41089 = CARTESIAN_POINT ( 'NONE',  ( 0.1049643490035303689, 0.3917322834645670104, -1.717847769028871596 ) ) ;
#41090 = CARTESIAN_POINT ( 'NONE',  ( -1.299212598425196097, 0.1771653543307087630, 0.000000000000000000 ) ) ;
#41091 = ORIENTED_EDGE ( 'NONE', *, *, #10113, .T. ) ;
#41092 = CARTESIAN_POINT ( 'NONE',  ( 0.3949938075777411073, -0.1058382717557499464, -2.158792650918635481 ) ) ;
#41093 = EDGE_LOOP ( 'NONE', ( #16851, #28043, #62836, #56246, #67271, #4634, #79602, #5836, #368, #16264, #80765, #21230, #52133, #61457 ) ) ;
#41094 = DIRECTION ( 'NONE',  ( -0.7071067811865472397, -0.000000000000000000, -0.7071067811865476838 ) ) ;
#41095 = VECTOR ( 'NONE', #13876, 39.37007874015748854 ) ;
#41096 = CARTESIAN_POINT ( 'NONE',  ( -1.443569553805773564, -0.6046776061558807314, 0.2411417322834647770 ) ) ;
#41097 = CARTESIAN_POINT ( 'NONE',  ( 1.391076115485564868, -0.6046776061558807314, 0.2411417322834647770 ) ) ;
#41098 = CARTESIAN_POINT ( 'NONE',  ( 0.1070741851644053527, 0.3996062992125986590, -0.6233595800524933672 ) ) ;
#41099 = CARTESIAN_POINT ( 'NONE',  ( -1.535433070866141225, 0.2952755905511811885, 0.000000000000000000 ) ) ;
#41100 = CARTESIAN_POINT ( 'NONE',  ( 1.840814904541342001, 2.729664745829105232, -0.5314960629921260393 ) ) ;
#41101 = CARTESIAN_POINT ( 'NONE',  ( 2.795275590551181466, 2.362204724409448620, 0.000000000000000000 ) ) ;
#41102 = CARTESIAN_POINT ( 'NONE',  ( 0.05060072268092381115, -0.3900885325447104868, -2.755905511811024056 ) ) ;
#41103 = CARTESIAN_POINT ( 'NONE',  ( 4.797336870675656522E-17, -0.3917322834645670104, -0.1633858267716536417 ) ) ;
#41104 = CARTESIAN_POINT ( 'NONE',  ( -0.2952755905511803003, -0.4536011799217368745, -0.2665933059059886201 ) ) ;
#41105 = CARTESIAN_POINT ( 'NONE',  ( -0.9711286089238838626, -0.5023911411419708095, 0.1820866141732285504 ) ) ;
#41106 = CARTESIAN_POINT ( 'NONE',  ( -1.102362204724408601, -0.1870078740157480879, -0.4822834645669291653 ) ) ;
#41107 = CARTESIAN_POINT ( 'NONE',  ( 1.036745406824147508, -0.4281496062992127816, -0.4176697321401328100 ) ) ;
#41108 = CARTESIAN_POINT ( 'NONE',  ( -1.030183727034119867, -0.3162353388693405765, 0.4822834645669290543 ) ) ;
#41109 = CARTESIAN_POINT ( 'NONE',  ( 0.1958661417322836440, -0.3392501089628017219, 0.07349081364829400387 ) ) ;
#41110 = ORIENTED_EDGE ( 'NONE', *, *, #61921, .T. ) ;
#41111 = CARTESIAN_POINT ( 'NONE',  ( -1.404199475065615932, -0.4281496062992127816, -0.4176697321401328100 ) ) ;
#41112 = CARTESIAN_POINT ( 'NONE',  ( -1.606188285223383527, 0.2952475903453252171, -0.04693825581093245825 ) ) ;
#41113 = CARTESIAN_POINT ( 'NONE',  ( -0.4091458600556405756, 0.2362204724409446288, -1.443569553805774230 ) ) ;
#41114 = CARTESIAN_POINT ( 'NONE',  ( 1.851423525050895247, 1.064103292658514777, -0.03357545743408756056 ) ) ;
#41115 = CARTESIAN_POINT ( 'NONE',  ( -0.1958661417322834220, -0.3392501089628018884, -0.6876640419947506189 ) ) ;
#41116 = CARTESIAN_POINT ( 'NONE',  ( -0.2867679344610364334, -0.2867679344610367109, -2.505905511811023612 ) ) ;
#41117 = CARTESIAN_POINT ( 'NONE',  ( -0.3608923884514428360, 0.2952755905511811885, 0.1292274648535926551 ) ) ;
#41118 = CARTESIAN_POINT ( 'NONE',  ( 1.594488188976378673, -0.5400638737290845981, -0.3530559997133363437 ) ) ;
#41119 = CARTESIAN_POINT ( 'NONE',  ( -0.3996062992125984925, -0.1070741851644056858, 0.03477690288713908284 ) ) ;
#41121 = DIRECTION ( 'NONE',  ( -0.000000000000000000, 1.000000000000000000, -0.000000000000000000 ) ) ;
#41120 = CYLINDRICAL_SURFACE ( 'NONE', #19382, 1.181102362204724310 ) ;
#41122 = CARTESIAN_POINT ( 'NONE',  ( -1.279527559055116948, -0.5400638737290844871, 0.3530559997133364547 ) ) ;
#41123 = CARTESIAN_POINT ( 'NONE',  ( -0.8661417322834640276, -0.1870078740157480879, -0.4822834645669291653 ) ) ;
#41124 = CARTESIAN_POINT ( 'NONE',  ( 0.1049643490035303689, 0.3917322834645668994, -0.07347149786645487679 ) ) ;
#41125 = CARTESIAN_POINT ( 'NONE',  ( 0.4330708661417329575, -0.5511811023622047445, 6.969142054262312111E-17 ) ) ;
#41126 = CARTESIAN_POINT ( 'NONE',  ( 0.1958661417322834775, 0.3392501089628018884, -0.07152230971128617498 ) ) ;
#41127 = CARTESIAN_POINT ( 'NONE',  ( 0.2034120734908144990, -0.5511811023622046335, 0.09757992244046803654 ) ) ;
#41128 = CARTESIAN_POINT ( 'NONE',  ( 0.8858267716535438430, -0.4536011799217368745, -0.2665933059059886201 ) ) ;
#41129 = CARTESIAN_POINT ( 'NONE',  ( 0.9776902887139113929, 0.2952755905511811885, 0.1292274648535926551 ) ) ;
#41130 = CARTESIAN_POINT ( 'NONE',  ( -0.2099737532808391705, 0.1283753931104748280, 0.1820866141732283561 ) ) ;
#41131 = CARTESIAN_POINT ( 'NONE',  ( 0.1049643490035304938, -0.3917322834645669549, -2.124671916010498762 ) ) ;
#41132 = CARTESIAN_POINT ( 'NONE',  ( -1.391076115485563314, -0.6046776061558809534, -0.2411417322834644161 ) ) ;
#41133 = CARTESIAN_POINT ( 'NONE',  ( -0.03937007874015669567, -0.5511811023622047445, 6.969142054262312111E-17 ) ) ;
#41134 = CARTESIAN_POINT ( 'NONE',  ( -1.213910761154854745, -0.5511811023622046335, 0.09757992244046803654 ) ) ;
#41135 = VECTOR ( 'NONE', #54958, 39.37007874015748143 ) ;
#41136 = CARTESIAN_POINT ( 'NONE',  ( 0.2362204724409451007, -0.4091458600556402980, -0.4835958005249343938 ) ) ;
#41137 = CARTESIAN_POINT ( 'NONE',  ( -0.9251968503937002541, -0.4536011799217368745, -0.2665933059059886201 ) ) ;
#41138 = CARTESIAN_POINT ( 'NONE',  ( -0.04593175853018302557, 0.2952755905511811885, 0.1292274648535926551 ) ) ;
#41139 = CARTESIAN_POINT ( 'NONE',  ( 0.2017716535433070613, -0.2017716535433070890, -0.3937007874015748254 ) ) ;
#41140 = CARTESIAN_POINT ( 'NONE',  ( 0.3346456692913390985, 0.07958543189024085140, 0.2665933059059887866 ) ) ;
#41141 = CARTESIAN_POINT ( 'NONE',  ( -0.3412073490813641308, -0.5023911411419708095, 0.1820866141732285504 ) ) ;
#41142 = CARTESIAN_POINT ( 'NONE',  ( -0.8595800524934373854, -0.05778040916215522460, 0.4822834645669289988 ) ) ;
#41143 = CARTESIAN_POINT ( 'NONE',  ( -1.699475065616797398, 0.2952755905511811885, 0.1292274648535926551 ) ) ;
#41144 = CARTESIAN_POINT ( 'NONE',  ( -1.233595800524933894, -0.5023911411419708095, -0.1820866141732282451 ) ) ;
#41145 = LINE ( 'NONE', #3676, #77065 ) ;
#41146 = CARTESIAN_POINT ( 'NONE',  ( 0.6364829396325465405, -0.3162353388693409650, -0.4822834645669289433 ) ) ;
#41147 = CARTESIAN_POINT ( 'NONE',  ( -0.1998031496062991630, -0.3460692066303959202, -1.717191601049868677 ) ) ;
#41148 = CARTESIAN_POINT ( 'NONE',  ( 1.476377952755906220, 0.1660481256975883668, -0.3530559997133364547 ) ) ;
#41149 = CARTESIAN_POINT ( 'NONE',  ( -0.3871391076115479057, -0.2845877964562161244, -0.3641732283464567121 ) ) ;
#41150 = CIRCLE ( 'NONE', #54537, 0.09842519685039351207 ) ;
#41151 = CARTESIAN_POINT ( 'NONE',  ( -0.1443569553805768291, 0.05413385826771666132, 0.4176697321401328100 ) ) ;
#41152 = CARTESIAN_POINT ( 'NONE',  ( -1.482939632545930975, 0.05413385826771666132, 0.4176697321401328100 ) ) ;
#41153 = CARTESIAN_POINT ( 'NONE',  ( -1.640419947506561060, -0.004921259842519576551, 0.3153832671262227771 ) ) ;
#41154 = CARTESIAN_POINT ( 'NONE',  ( 1.181102362204725198, -0.1870078740157479769, 0.4822834645669291653 ) ) ;
#41155 = CARTESIAN_POINT ( 'NONE',  ( -0.4790026246719154557, -0.2845877964562159024, 0.3641732283464567677 ) ) ;
#41156 = CARTESIAN_POINT ( 'NONE',  ( 0.3149606299212185379, 2.559055118110236560, 3.924389226575471845 ) ) ;
#41157 = CARTESIAN_POINT ( 'NONE',  ( 0.1998031496062994405, -0.3460692066303958092, -0.2493438320209973857 ) ) ;
#41158 = CARTESIAN_POINT ( 'NONE',  ( -0.1058382717557503211, 0.3949938075777409408, -0.006561679790026304741 ) ) ;
#41159 = CARTESIAN_POINT ( 'NONE',  ( -0.09156050430092219083, -0.3808816823641230087, -1.492482962822815952E-17 ) ) ;
#41160 = CARTESIAN_POINT ( 'NONE',  ( 1.332020997375328974, -0.08942795157528024563, -0.3641732283464568787 ) ) ;
#41161 = CARTESIAN_POINT ( 'NONE',  ( -1.581364829396324945, -0.3162353388693405765, 0.4822834645669290543 ) ) ;
#41162 = CARTESIAN_POINT ( 'NONE',  ( 0.6889763779527563470, 0.1660481256975883668, -0.3530559997133364547 ) ) ;
#41163 = CARTESIAN_POINT ( 'NONE',  ( 0.3917322834645670104, 2.398668435337828261E-17, -2.250000000000000000 ) ) ;
#41164 = CARTESIAN_POINT ( 'NONE',  ( 1.213910761154856299, 0.1771653543307087630, 0.09757992244046791164 ) ) ;
#41165 = EDGE_CURVE ( 'NONE', #11079, #2570, #62432, .T. ) ;
#41166 = CARTESIAN_POINT ( 'NONE',  ( 0.03937007874015833325, -0.6692913385826771977, 8.415575281601705876E-17 ) ) ;
#41167 = CARTESIAN_POINT ( 'NONE',  ( -0.3543307086614165824, 0.2952755905511811885, 0.000000000000000000 ) ) ;
#41168 = DIRECTION ( 'NONE',  ( -0.000000000000000000, -1.000000000000000000, -0.000000000000000000 ) ) ;
#41169 = CARTESIAN_POINT ( 'NONE',  ( 0.4724409448818898682, 2.892866454678787531E-17, -0.9055118110236221041 ) ) ;
#41170 = CARTESIAN_POINT ( 'NONE',  ( 3.821484228344193657, 2.755905511811024056, 0.5314960629921260393 ) ) ;
#41171 = CARTESIAN_POINT ( 'NONE',  ( 0.1640419947506569498, -0.08942795157527998196, 0.3641732283464567121 ) ) ;
#41172 = ORIENTED_EDGE ( 'NONE', *, *, #14046, .T. ) ;
#41173 = CARTESIAN_POINT ( 'NONE',  ( -0.2867679344610367109, 0.2867679344610365444, -0.3313841451781647240 ) ) ;
#41174 = ORIENTED_EDGE ( 'NONE', *, *, #19278, .F. ) ;
#41175 = EDGE_CURVE ( 'NONE', #9799, #16468, #3653, .T. ) ;
#41176 = CARTESIAN_POINT ( 'NONE',  ( -0.6167979002624665030, 0.05413385826771666132, 0.4176697321401328100 ) ) ;
#41177 = CARTESIAN_POINT ( 'NONE',  ( 1.167979002624672580, 0.05413385826771626580, -0.4176697321401330321 ) ) ;
#41178 = CARTESIAN_POINT ( 'NONE',  ( 0.3543307086614181922, -0.6692913385826771977, 8.415575281601705876E-17 ) ) ;
#41179 = CARTESIAN_POINT ( 'NONE',  ( -0.4527559055118102749, -0.4536011799217368745, -0.2665933059059886201 ) ) ;
#41180 = CARTESIAN_POINT ( 'NONE',  ( 0.9842519685039378130, -0.6692913385826771977, 8.415575281601705876E-17 ) ) ;
#41181 = CARTESIAN_POINT ( 'NONE',  ( -1.062992125984250968, -0.6692913385826771977, 8.415575281601705876E-17 ) ) ;
#41182 = CARTESIAN_POINT ( 'NONE',  ( -0.2165354330708654795, -0.5400638737290845981, -0.3530559997133363437 ) ) ;
#41183 = CARTESIAN_POINT ( 'NONE',  ( -0.9317585301837263412, 0.05413385826771666132, 0.4176697321401328100 ) ) ;
#41184 = CARTESIAN_POINT ( 'NONE',  ( 1.318897637795276356, 0.1660481256975883668, -0.3530559997133364547 ) ) ;
#41185 = CARTESIAN_POINT ( 'NONE',  ( 0.7742782152230978099, -0.4281496062992124485, 0.4176697321401328655 ) ) ;
#41186 = CARTESIAN_POINT ( 'NONE',  ( 0.7545931758530189937, 0.2952755905511810774, -0.1292274648535930714 ) ) ;
#41187 = CARTESIAN_POINT ( 'NONE',  ( 0.1049643490035304938, -0.3917322834645669549, -0.7073490813648293241 ) ) ;
#41188 = CARTESIAN_POINT ( 'NONE',  ( -0.1181102362204717315, -0.5511811023622047445, 6.969142054262312111E-17 ) ) ;
#41189 = ORIENTED_EDGE ( 'NONE', *, *, #22645, .F. ) ;
#41190 = CARTESIAN_POINT ( 'NONE',  ( 0.3420746716998659953, 0.1974969037888705536, -1.233595800524934338 ) ) ;
#41191 = EDGE_LOOP ( 'NONE', ( #52870, #17795, #27130, #70073 ) ) ;
#41192 = CARTESIAN_POINT ( 'NONE',  ( -0.8005249343832013809, -0.3690944881889763329, 0.3153832671262228327 ) ) ;
#41193 = VECTOR ( 'NONE', #31401, 39.37007874015748143 ) ;
#41194 = CIRCLE ( 'NONE', #57323, 0.1181102362204723977 ) ;
#41195 = CARTESIAN_POINT ( 'NONE',  ( 0.06561679790026316017, -0.4281496062992124485, 0.4176697321401328655 ) ) ;
#41196 = DIRECTION ( 'NONE',  ( 0.8660254037844361541, 0.000000000000000000, 0.5000000000000043299 ) ) ;
#41197 = CARTESIAN_POINT ( 'NONE',  ( -0.3805774278215216522, -0.4281496062992127816, -0.4176697321401328100 ) ) ;
#41198 = CARTESIAN_POINT ( 'NONE',  ( -0.3740157480314953431, -0.5400638737290845981, -0.3530559997133363437 ) ) ;
#41199 = CARTESIAN_POINT ( 'NONE',  ( -1.259842519685038686, -0.1870078740157480879, -0.4822834645669291653 ) ) ;
#41200 = CARTESIAN_POINT ( 'NONE',  ( -1.515748031496062076, 0.1660481256975883668, -0.3530559997133364547 ) ) ;
#41201 = CARTESIAN_POINT ( 'NONE',  ( 1.555118110236221041, 0.07958543189024071263, -0.2665933059059888421 ) ) ;
#41202 = CARTESIAN_POINT ( 'NONE',  ( -3.924389226575468737, 2.559055118110236560, 0.3149606299212596716 ) ) ;
#41203 = CARTESIAN_POINT ( 'NONE',  ( 0.2371198560983137360, 0.1759840215932894636, 5.725591907046406526 ) ) ;
#41204 = CARTESIAN_POINT ( 'NONE',  ( 0.6824146981627303710, 0.1283753931104746893, -0.1820866141732285504 ) ) ;
#41205 = CARTESIAN_POINT ( 'NONE',  ( -0.1181102362204717315, -0.6692913385826771977, 8.415575281601705876E-17 ) ) ;
#41206 = CARTESIAN_POINT ( 'NONE',  ( 0.5249343832021005074, -0.6046776061558807314, 0.2411417322834647770 ) ) ;
#41207 = ORIENTED_EDGE ( 'NONE', *, *, #6822, .F. ) ;
#41208 = CARTESIAN_POINT ( 'NONE',  ( 0.1998031496062994405, -0.3460692066303958092, -1.509186351706036655 ) ) ;
#41209 = CARTESIAN_POINT ( 'NONE',  ( -0.5120078740157480990, 0.000000000000000000, 0.000000000000000000 ) ) ;
#41210 = VERTEX_POINT ( 'NONE', #83084 ) ;
#41211 = CARTESIAN_POINT ( 'NONE',  ( 0.3460692066303958092, 0.1998031496062993018, -1.310367454068241511 ) ) ;
#41212 = CARTESIAN_POINT ( 'NONE',  ( 0.3460692066303959202, -0.1998031496062991630, -0.4967191601049869010 ) ) ;
#41213 = CARTESIAN_POINT ( 'NONE',  ( -0.5905511811023615998, 0.2952755905511811885, 0.000000000000000000 ) ) ;
#41214 = CARTESIAN_POINT ( 'NONE',  ( 5.785732909357575061E-17, -0.4724409448818898682, -0.07874015748031495954 ) ) ;
#41215 = CARTESIAN_POINT ( 'NONE',  ( -0.1958661417322836718, 0.3392501089628017219, -2.617454068241469756 ) ) ;
#41216 = CARTESIAN_POINT ( 'NONE',  ( -1.653543307086613234, -0.1870078740157479769, 0.3641732283464567677 ) ) ;
#41217 = CARTESIAN_POINT ( 'NONE',  ( 0.7611548556430451917, -0.6046776061558807314, 0.2411417322834647770 ) ) ;
#41218 = AXIS2_PLACEMENT_3D ( 'NONE', #79226, #68952, #11723 ) ;
#41219 = CARTESIAN_POINT ( 'NONE',  ( 0.9711286089238851948, -0.6046776061558809534, -0.2411417322834644161 ) ) ;
#41220 = CARTESIAN_POINT ( 'NONE',  ( -0.4068241469816264999, -0.3690944881889763329, 0.3153832671262228327 ) ) ;
#41221 = CARTESIAN_POINT ( 'NONE',  ( -0.1312335958005241554, 0.2306618581243848609, 0.2411417322834645549 ) ) ;
#41222 = CARTESIAN_POINT ( 'NONE',  ( -0.2362204724409447953, -0.4091458600556404646, -2.032152230971128848 ) ) ;
#41223 = CARTESIAN_POINT ( 'NONE',  ( 0.1181102362204730916, 0.1771653543307087630, 0.000000000000000000 ) ) ;
#41224 = CARTESIAN_POINT ( 'NONE',  ( -0.5839895013123351797, 0.2952755905511810774, -0.1292274648535930714 ) ) ;
#41225 = CARTESIAN_POINT ( 'NONE',  ( 0.2891555358219910499, -0.2891555358219909944, -1.750000000000000000 ) ) ;
#41226 = CARTESIAN_POINT ( 'NONE',  ( -1.633858267716534529, -0.5400638737290845981, -0.3530559997133363437 ) ) ;
#41227 = CARTESIAN_POINT ( 'NONE',  ( -0.01312335958005186876, -0.3690944881889763329, 0.3153832671262228327 ) ) ;
#41228 = CARTESIAN_POINT ( 'NONE',  ( 1.515748031496063408, 0.07958543189024085140, 0.2665933059059887866 ) ) ;
#41229 = CARTESIAN_POINT ( 'NONE',  ( -1.076115485564303809, 0.2306618581243848609, 0.2411417322834645549 ) ) ;
#41230 = CARTESIAN_POINT ( 'NONE',  ( -0.5446194225721777693, -0.08942795157527998196, 0.3641732283464567121 ) ) ;
#41231 = CARTESIAN_POINT ( 'NONE',  ( -1.586052503253848389, 0.7480314960629931287, -0.1653254495020559933 ) ) ;
#41232 = CARTESIAN_POINT ( 'NONE',  ( -1.364829396325458521, 0.2306618581243847221, -0.2411417322834647770 ) ) ;
#41233 = CARTESIAN_POINT ( 'NONE',  ( 0.1509186351706045259, -0.05778040916215560624, -0.4822834645669293319 ) ) ;
#41234 = CARTESIAN_POINT ( 'NONE',  ( -0.1998031496062994405, 0.3460692066303957537, -2.609580052493438274 ) ) ;
#41235 = CARTESIAN_POINT ( 'NONE',  ( 0.2867679344610365999, -0.2867679344610365999, -2.540663098916323914 ) ) ;
#41236 = CARTESIAN_POINT ( 'NONE',  ( -2.020039340939639771, 1.253873987468399509, -0.3814095263789812895 ) ) ;
#41237 = CARTESIAN_POINT ( 'NONE',  ( 0.2887139107611556010, 0.1283753931104746893, -0.1820866141732285504 ) ) ;
#41238 = CARTESIAN_POINT ( 'NONE',  ( 0.8792650918635177559, -0.4281496062992127816, -0.4176697321401328100 ) ) ;
#41239 = CARTESIAN_POINT ( 'NONE',  ( -1.056430446194224881, 0.1771653543307087075, -0.09757992244046823083 ) ) ;
#41240 = CARTESIAN_POINT ( 'NONE',  ( 1.292650918635171564, -0.6692913385826773087, -0.1292274648535924053 ) ) ;
#41241 = CARTESIAN_POINT ( 'NONE',  ( -1.371391076115484831, 0.1771653543307087075, -0.09757992244046823083 ) ) ;
#41242 = EDGE_CURVE ( 'NONE', #34982, #44828, #17884, .T. ) ;
#41243 = CARTESIAN_POINT ( 'NONE',  ( -0.5249343832020990641, -0.6046776061558809534, -0.2411417322834644161 ) ) ;
#41244 = CARTESIAN_POINT ( 'NONE',  ( 0.05249343832021075018, -0.5023911411419708095, 0.1820866141732285504 ) ) ;
#41245 = CARTESIAN_POINT ( 'NONE',  ( 1.608925997164302624, 0.2886606758775757675, -0.09234068394397736135 ) ) ;
#41246 = CARTESIAN_POINT ( 'NONE',  ( 0.7874015748031503170, -0.1870078740157479769, 0.3641732283464567677 ) ) ;
#41247 = CARTESIAN_POINT ( 'NONE',  ( 0.03937007874015833325, -0.6692913385826771977, 8.415575281601705876E-17 ) ) ;
#41248 = CARTESIAN_POINT ( 'NONE',  ( -0.3460692066303957537, -0.1998031496062994405, -0.2867454068241469534 ) ) ;
#41249 = CARTESIAN_POINT ( 'NONE',  ( -0.7152230971128602510, -0.05778040916215560624, -0.4822834645669293319 ) ) ;
#41250 = VECTOR ( 'NONE', #44491, 39.37007874015748854 ) ;
#41251 = CARTESIAN_POINT ( 'NONE',  ( -0.2867679344610365999, 0.2867679344610364889, -1.679133858267716661 ) ) ;
#41252 = CARTESIAN_POINT ( 'NONE',  ( 0.9383202099737536495, -0.2845877964562159024, 0.3641732283464567677 ) ) ;
#41253 = CARTESIAN_POINT ( 'NONE',  ( 0.1902887139107617975, -0.6692913385826773087, -0.1292274648535924053 ) ) ;
#41254 = CONICAL_SURFACE ( 'NONE', #43931, 2.362204724409449508, 0.8582239808723030050 ) ;
#41255 = CARTESIAN_POINT ( 'NONE',  ( -0.3937007874015740483, -0.1870078740157479769, 0.4822834645669291653 ) ) ;
#41256 = CARTESIAN_POINT ( 'NONE',  ( -0.2952755905511803003, -0.4536011799217368745, -0.2665933059059886201 ) ) ;
#41257 = CARTESIAN_POINT ( 'NONE',  ( 3.937007874015748143, 2.165354330708662012, 0.6299212598425202314 ) ) ;
#41258 = CARTESIAN_POINT ( 'NONE',  ( -0.6299212598425188991, -0.1870078740157480601, -0.3641732283464567677 ) ) ;
#41259 = CARTESIAN_POINT ( 'NONE',  ( 0.5577427821522316087, -0.05778040916215522460, 0.4822834645669289988 ) ) ;
#41260 = CARTESIAN_POINT ( 'NONE',  ( -0.8858267716535425107, 0.07958543189024071263, -0.2665933059059888421 ) ) ;
#41261 = CARTESIAN_POINT ( 'NONE',  ( -0.1998031496062994405, 0.3460692066303957537, -0.8772965879265091083 ) ) ;
#41262 = CARTESIAN_POINT ( 'NONE',  ( -1.305774278215222184, 0.2952755905511811885, 0.1292274648535926551 ) ) ;
#41263 = CARTESIAN_POINT ( 'NONE',  ( -0.8554425558739509050, -4.966502543501560364E-15, 0.4118484887281982920 ) ) ;
#41264 = VERTEX_POINT ( 'NONE', #63307 ) ;
#41265 = CARTESIAN_POINT ( 'NONE',  ( -0.9776902887139098386, -0.5511811023622046335, 0.09757992244046803654 ) ) ;
#41266 = CARTESIAN_POINT ( 'NONE',  ( -0.2821522309711278487, 0.2952755905511811885, 0.1292274648535926551 ) ) ;
#41267 = CARTESIAN_POINT ( 'NONE',  ( -1.706036745406823485, 0.2306618581243848609, 0.2411417322834645549 ) ) ;
#41268 = CARTESIAN_POINT ( 'NONE',  ( -1.181102362204723644, -0.1870078740157479769, 0.4822834645669291653 ) ) ;
#41269 = CARTESIAN_POINT ( 'NONE',  ( 1.614173228346456712, 2.401574803149606474, 0.1372047244094478646 ) ) ;
#41270 = CARTESIAN_POINT ( 'NONE',  ( 1.456692913385827515, -0.6692913385826771977, 8.415575281601705876E-17 ) ) ;
#41271 = CARTESIAN_POINT ( 'NONE',  ( 0.9973753280839902091, -0.6046776061558807314, 0.2411417322834647770 ) ) ;
#41272 = FACE_OUTER_BOUND ( 'NONE', #16266, .T. ) ;
#41273 = CARTESIAN_POINT ( 'NONE',  ( -1.436417322834643739, 0.4405861044731112508, -0.3149606299212598381 ) ) ;
#41274 = CARTESIAN_POINT ( 'NONE',  ( 1.489501312335958172, -0.08942795157528024563, -0.3641732283464568787 ) ) ;
#41275 = CARTESIAN_POINT ( 'NONE',  ( -0.3996062992125986035, -7.340648628747425578E-17, -0.6692913385826770867 ) ) ;
#41276 = VERTEX_POINT ( 'NONE', #50665 ) ;
#41277 = CARTESIAN_POINT ( 'NONE',  ( -0.4330708661417315697, -0.5511811023622047445, 6.969142054262312111E-17 ) ) ;
#41278 = CARTESIAN_POINT ( 'NONE',  ( -0.3917322834645669549, -0.1049643490035306603, -2.400262467191600635 ) ) ;
#41279 = ORIENTED_EDGE ( 'NONE', *, *, #21598, .F. ) ;
#41280 = CARTESIAN_POINT ( 'NONE',  ( 0.9776902887139113929, 0.2952755905511811885, 0.1292274648535926551 ) ) ;
#41281 = CARTESIAN_POINT ( 'NONE',  ( 0.01312335958005323398, 0.05413385826771666132, 0.4176697321401328100 ) ) ;
#41282 = CARTESIAN_POINT ( 'NONE',  ( -0.6496062992125976043, 0.1660481256975883668, -0.3530559997133364547 ) ) ;
#41283 = CARTESIAN_POINT ( 'NONE',  ( 1.397637795275591177, 0.1660481256975883668, -0.3530559997133364547 ) ) ;
#41284 = CARTESIAN_POINT ( 'NONE',  ( -1.305774278215222184, 0.1771653543307087630, 0.09757992244046791164 ) ) ;
#41285 = CARTESIAN_POINT ( 'NONE',  ( 0.05803841145411302999, 1.066555667699313759, -1.527167351498692538 ) ) ;
#41286 = CARTESIAN_POINT ( 'NONE',  ( 0.5118110236220480003, -0.6692913385826771977, 8.415575281601705876E-17 ) ) ;
#41287 = CARTESIAN_POINT ( 'NONE',  ( 0.7086614173228352742, -0.1870078740157480601, -0.3641732283464567677 ) ) ;
#41288 = CARTESIAN_POINT ( 'NONE',  ( -0.7086614173228339419, -0.1870078740157479769, 0.4822834645669291653 ) ) ;
#41289 = CARTESIAN_POINT ( 'NONE',  ( 0.3392501089628018329, -0.1958661417322834497, -1.444862573981940512 ) ) ;
#41290 = CARTESIAN_POINT ( 'NONE',  ( -1.338582677165353729, -0.1870078740157479769, 0.4822834645669291653 ) ) ;
#41291 = CARTESIAN_POINT ( 'NONE',  ( -1.559171609364246924, 1.299212598425196985, 0.5949441279213820710 ) ) ;
#41292 = CARTESIAN_POINT ( 'NONE',  ( 1.017060367454068803, -0.3162353388693405765, 0.4822834645669290543 ) ) ;
#41293 = CARTESIAN_POINT ( 'NONE',  ( 1.213910761154856299, 0.1771653543307087630, 0.09757992244046791164 ) ) ;
#41294 = VERTEX_POINT ( 'NONE', #19099 ) ;
#41295 = CARTESIAN_POINT ( 'NONE',  ( -0.1974969037888703871, -0.3420746716998661063, 0.09186351706036739728 ) ) ;
#41296 = CARTESIAN_POINT ( 'NONE',  ( -0.2624671916010490880, -0.6046776061558807314, 0.2411417322834647770 ) ) ;
#41297 = VERTEX_POINT ( 'NONE', #56976 ) ;
#41298 = CARTESIAN_POINT ( 'NONE',  ( 0.2690288713910767848, -0.5511811023622048555, -0.09757992244046775898 ) ) ;
#41299 = CARTESIAN_POINT ( 'NONE',  ( -1.181102362204723644, -0.1870078740157480879, -0.4822834645669291653 ) ) ;
#41300 = CARTESIAN_POINT ( 'NONE',  ( 0.8923884514435701520, -0.6046776061558809534, -0.2411417322834644161 ) ) ;
#41301 = CARTESIAN_POINT ( 'NONE',  ( 0.9776902887139113929, 0.2952755905511811885, 0.1292274648535926551 ) ) ;
#41302 = CARTESIAN_POINT ( 'NONE',  ( -0.1902887139107604098, -0.6692913385826771977, 0.1292274648535927661 ) ) ;
#41303 = CARTESIAN_POINT ( 'NONE',  ( -0.8858267716535425107, -0.5400638737290844871, 0.3530559997133364547 ) ) ;
#41304 = CARTESIAN_POINT ( 'NONE',  ( -0.1049643490035307020, 0.3917322834645669549, -2.138451443569553412 ) ) ;
#41305 = CARTESIAN_POINT ( 'NONE',  ( -1.555118110236219930, 0.1660481256975885056, 0.3530559997133364547 ) ) ;
#41306 = CARTESIAN_POINT ( 'NONE',  ( -0.6167979002624665030, -0.4281496062992127816, -0.4176697321401328100 ) ) ;
#41307 = CARTESIAN_POINT ( 'NONE',  ( -0.4002624671916004129, -0.2845877964562159024, 0.3641732283464567677 ) ) ;
#41308 = CARTESIAN_POINT ( 'NONE',  ( 1.450131233595801428, -0.6692913385826773087, -0.1292274648535924053 ) ) ;
#41309 = CARTESIAN_POINT ( 'NONE',  ( 1.443569553805774897, -0.6046776061558809534, -0.2411417322834644161 ) ) ;
#41310 = EDGE_CURVE ( 'NONE', #21631, #28101, #58238, .T. ) ;
#41311 = CARTESIAN_POINT ( 'NONE',  ( -0.9186351706036736120, 0.2306618581243848609, 0.2411417322834645549 ) ) ;
#41312 = DIRECTION ( 'NONE',  ( 1.000000000000000000, 3.096699300667737957E-16, -1.692413147294446216E-16 ) ) ;
#41313 = VECTOR ( 'NONE', #1334, 39.37007874015748854 ) ;
#41314 = EDGE_CURVE ( 'NONE', #21419, #24203, #73338, .T. ) ;
#41315 = CARTESIAN_POINT ( 'NONE',  ( 0.5052493438320215802, 0.2952755905511811885, 0.1292274648535926551 ) ) ;
#41316 = CARTESIAN_POINT ( 'NONE',  ( 0.3996062992125986035, 0.1070741851644054776, -1.856955380577427928 ) ) ;
#41317 = CARTESIAN_POINT ( 'NONE',  ( 3.933488357682179970, 1.093105643167624930, 0.1670540113780165925 ) ) ;
#41318 = ADVANCED_FACE ( 'NONE', ( #43519 ), #41254, .F. ) ;
#41319 = CARTESIAN_POINT ( 'NONE',  ( -0.03280839895013062252, 0.2952755905511810774, -0.1292274648535930714 ) ) ;
#41320 = AXIS2_PLACEMENT_3D ( 'NONE', #41559, #54173, #21379 ) ;
#41321 = CARTESIAN_POINT ( 'NONE',  ( -1.062992125984250968, -0.5511811023622047445, 6.969142054262312111E-17 ) ) ;
#41322 = CARTESIAN_POINT ( 'NONE',  ( 1.036745406824147731, -0.004921259842519576551, 0.3153832671262227771 ) ) ;
#41323 = CARTESIAN_POINT ( 'NONE',  ( -0.4724409448818899238, 0.1265901696524986686, -0.5820209973753280863 ) ) ;
#41324 = CARTESIAN_POINT ( 'NONE',  ( 1.233595800524935227, 0.1283753931104746893, -0.1820866141732285504 ) ) ;
#41325 = CARTESIAN_POINT ( 'NONE',  ( 0.7545931758530188826, -0.6692913385826771977, 0.1292274648535927661 ) ) ;
#41326 = CARTESIAN_POINT ( 'NONE',  ( -0.3420746716998662729, 0.1974969037888702206, -0.4179790026246719137 ) ) ;
#41327 = PRODUCT_DEFINITION_SHAPE ( 'NONE', 'NONE',  #37243 ) ;
#41328 = CARTESIAN_POINT ( 'NONE',  ( -0.5052493438320203589, -0.6692913385826771977, 0.1292274648535927661 ) ) ;
#41329 = PLANE ( 'NONE',  #31079 ) ;
#41330 = CARTESIAN_POINT ( 'NONE',  ( 1.377952755905512472, -0.5511811023622047445, 6.969142054262312111E-17 ) ) ;
#41331 = CARTESIAN_POINT ( 'NONE',  ( -0.4265091863517051496, 0.2952755905511810774, -0.1292274648535930714 ) ) ;
#41332 = CARTESIAN_POINT ( 'NONE',  ( 0.3420746716998660508, 0.1974969037888705814, -0.3654855643044619407 ) ) ;
#41333 = CARTESIAN_POINT ( 'NONE',  ( 1.456692913385827515, -0.6692913385826771977, 8.415575281601705876E-17 ) ) ;
#41334 = CARTESIAN_POINT ( 'NONE',  ( 0.1312335958005255154, -0.6046776061558807314, 0.2411417322834647770 ) ) ;
#41335 = CARTESIAN_POINT ( 'NONE',  ( 0.6496062992125991586, -0.4536011799217368745, -0.2665933059059886201 ) ) ;
#41336 = CARTESIAN_POINT ( 'NONE',  ( -0.06298769380853883049, 1.066927083894429140, -1.120388281904474814 ) ) ;
#41337 = CARTESIAN_POINT ( 'NONE',  ( 0.5905511811023629321, 0.1771653543307087630, 0.000000000000000000 ) ) ;
#41338 = CARTESIAN_POINT ( 'NONE',  ( -1.653543307086613234, -0.1870078740157479769, 0.4822834645669291653 ) ) ;
#41339 = CARTESIAN_POINT ( 'NONE',  ( -0.1998031496062991630, -0.3460692066303959202, -1.402230971128609172 ) ) ;
#41340 = CARTESIAN_POINT ( 'NONE',  ( 0.6692913385826778638, -0.6692913385826771977, 8.415575281601705876E-17 ) ) ;
#41341 = ADVANCED_FACE ( 'NONE', ( #11567 ), #5238, .F. ) ;
#41342 = CARTESIAN_POINT ( 'NONE',  ( -9.594673741351313045E-17, 0.3917322834645670104, -1.094488188976378007 ) ) ;
#41343 = CARTESIAN_POINT ( 'NONE',  ( 1.581364829396326277, -0.2845877964562161244, -0.3641732283464567121 ) ) ;
#41344 = CARTESIAN_POINT ( 'NONE',  ( -0.1574803149606292529, -0.1870078740157479769, 0.3641732283464567677 ) ) ;
#41345 = CARTESIAN_POINT ( 'NONE',  ( 0.1181102362204730916, 0.2952755905511811885, 0.000000000000000000 ) ) ;
#41346 = CARTESIAN_POINT ( 'NONE',  ( 1.410761154855643795, -0.08942795157528024563, -0.3641732283464568787 ) ) ;
#41347 = CARTESIAN_POINT ( 'NONE',  ( -1.541994750656167090, 0.1771653543307087630, 0.09757992244046791164 ) ) ;
#41348 = CARTESIAN_POINT ( 'NONE',  ( -1.312335958005248715, -0.6046776061558809534, -0.2411417322834644161 ) ) ;
#41349 = CARTESIAN_POINT ( 'NONE',  ( 0.6889763779527566800, -0.5400638737290844871, 0.3530559997133364547 ) ) ;
#41350 = CARTESIAN_POINT ( 'NONE',  ( 1.633858267716535639, -0.5400638737290844871, 0.3530559997133364547 ) ) ;
#41351 = CARTESIAN_POINT ( 'NONE',  ( 0.2017716535433070613, -0.2017716535433070890, 0.000000000000000000 ) ) ;
#41352 = CARTESIAN_POINT ( 'NONE',  ( 0.6299212598425204535, -0.1870078740157479769, 0.4822834645669291653 ) ) ;
#41353 = CARTESIAN_POINT ( 'NONE',  ( 1.437007874015748810, -0.5400638737290845981, -0.3530559997133363437 ) ) ;
#41354 = CARTESIAN_POINT ( 'NONE',  ( 0.9120734908136490793, 0.2952755905511810774, -0.1292274648535930714 ) ) ;
#41355 = CARTESIAN_POINT ( 'NONE',  ( -1.692913385826770645, 0.1771653543307087630, 0.000000000000000000 ) ) ;
#41356 = CARTESIAN_POINT ( 'NONE',  ( 0.9317585301837276734, -0.004921259842519870586, -0.3153832671262229437 ) ) ;
#41357 = CARTESIAN_POINT ( 'NONE',  ( 1.679790026246720025, 0.2306618581243848609, 0.2411417322834645549 ) ) ;
#41358 = CARTESIAN_POINT ( 'NONE',  ( -0.9055118110236215490, -0.5511811023622047445, 6.969142054262312111E-17 ) ) ;
#41359 = CARTESIAN_POINT ( 'NONE',  ( 0.6692913385826777528, 0.1771653543307087630, 0.000000000000000000 ) ) ;
#41360 = CARTESIAN_POINT ( 'NONE',  ( 0.2559055118110243332, 0.1660481256975885056, 0.3530559997133364547 ) ) ;
#41361 = CARTESIAN_POINT ( 'NONE',  ( 0.7480314960629927956, -0.6692913385826771977, 8.415575281601705876E-17 ) ) ;
#41362 = CARTESIAN_POINT ( 'NONE',  ( -0.1837270341207340729, 0.2306618581243847221, -0.2411417322834647770 ) ) ;
#41363 = CARTESIAN_POINT ( 'NONE',  ( 0.1115485564304467270, -0.5511811023622048555, -0.09757992244046775898 ) ) ;
#41364 = CARTESIAN_POINT ( 'NONE',  ( 1.207349081364829990, -0.6046776061558809534, -0.2411417322834644161 ) ) ;
#41365 = CARTESIAN_POINT ( 'NONE',  ( -1.690245196119324333, 1.168079626289185269, 0.2980098697639514405 ) ) ;
#41366 = CARTESIAN_POINT ( 'NONE',  ( -1.043307086614172707, 0.1660481256975883668, -0.3530559997133364547 ) ) ;
#41368 = CARTESIAN_POINT ( 'NONE',  ( 0.3460692066303959757, -0.1998031496062991907, -0.8923884514435694859 ) ) ;
#41367 = CARTESIAN_POINT ( 'NONE',  ( -0.5314960629921349211, 2.742779892193532909, 2.570293763077048155 ) ) ;
#41369 = AXIS2_PLACEMENT_3D ( 'NONE', #14768, #71579, #13930 ) ;
#41370 = CARTESIAN_POINT ( 'NONE',  ( -0.6824146981627288167, 0.2306618581243848609, 0.2411417322834645549 ) ) ;
#41371 = CARTESIAN_POINT ( 'NONE',  ( -0.5971128608923877978, 0.2952755905511811885, 0.1292274648535926551 ) ) ;
#41372 = CARTESIAN_POINT ( 'NONE',  ( -0.2925321140481932924, 0.2925321140481931814, -2.854330708661417138 ) ) ;
#41373 = CARTESIAN_POINT ( 'NONE',  ( 0.1974969037888706369, -0.3420746716998659953, -2.454068241469816503 ) ) ;
#41374 = ORIENTED_EDGE ( 'NONE', *, *, #5920, .F. ) ;
#41375 = CARTESIAN_POINT ( 'NONE',  ( 0.7611548556430454138, 0.1283753931104746893, -0.1820866141732285504 ) ) ;
#41376 = CARTESIAN_POINT ( 'NONE',  ( -0.2867679344610365999, 0.2867679344610364889, -1.114173228346456712 ) ) ;
#41377 = CARTESIAN_POINT ( 'NONE',  ( 1.122047244094488860, 0.1660481256975885056, 0.3530559997133364547 ) ) ;
#41378 = CARTESIAN_POINT ( 'NONE',  ( -1.646051170424378096, 0.8346805926620876059, -0.3149606299212598381 ) ) ;
#41379 = CARTESIAN_POINT ( 'NONE',  ( -1.332020997375327642, -0.2845877964562161244, -0.3641732283464567121 ) ) ;
#41380 = CARTESIAN_POINT ( 'NONE',  ( -0.1243525380209066500, 1.078522938818520238, 1.115555442254801077 ) ) ;
#41381 = CARTESIAN_POINT ( 'NONE',  ( 1.607611548556431069, 0.1771653543307087630, 0.09757992244046791164 ) ) ;
#41382 = CARTESIAN_POINT ( 'NONE',  ( 0.3917322834645669549, 2.398668435337827645E-17, -0.5131040437982135050 ) ) ;
#41383 = EDGE_CURVE ( 'NONE', #72444, #6265, #30492, .T. ) ;
#41384 = CARTESIAN_POINT ( 'NONE',  ( -0.05249343832020911260, 0.2306618581243848609, 0.2411417322834645549 ) ) ;
#41385 = CARTESIAN_POINT ( 'NONE',  ( -0.3412073490813641308, -0.5023911411419708095, 0.1820866141732285504 ) ) ;
#41386 = CARTESIAN_POINT ( 'NONE',  ( 0.7742782152230978099, -0.4281496062992124485, 0.4176697321401328655 ) ) ;
#41387 = CARTESIAN_POINT ( 'NONE',  ( 0.02624671916010564918, 0.2306618581243848609, 0.2411417322834645549 ) ) ;
#41388 = CARTESIAN_POINT ( 'NONE',  ( -0.2362204724409451284, 0.4091458600556402425, -0.01312335958005249326 ) ) ;
#41389 = CARTESIAN_POINT ( 'NONE',  ( -0.01149616601327268020, 1.490381362800744269E-15, -0.3791475997938222320 ) ) ;
#41390 = CARTESIAN_POINT ( 'NONE',  ( -0.1958661417322836995, 0.3392501089628017219, -1.584664985073177546 ) ) ;
#41391 = CARTESIAN_POINT ( 'NONE',  ( 0.8595800524934390507, -0.3162353388693405765, 0.4822834645669290543 ) ) ;
#41392 = CARTESIAN_POINT ( 'NONE',  ( 0.1837270341207354329, 0.2306618581243848609, 0.2411417322834645549 ) ) ;
#41393 = CARTESIAN_POINT ( 'NONE',  ( -1.167979002624671470, 0.05413385826771666132, 0.4176697321401328100 ) ) ;
#41394 = CARTESIAN_POINT ( 'NONE',  ( 0.9186351706036751663, -0.6046776061558807314, 0.2411417322834647770 ) ) ;
#41395 = CARTESIAN_POINT ( 'NONE',  ( 0.9186351706036752773, 0.2306618581243847221, -0.2411417322834647770 ) ) ;
#41396 = CARTESIAN_POINT ( 'NONE',  ( -0.1049643490035307020, 0.3917322834645669549, -0.8786089238845143923 ) ) ;
#41397 = CARTESIAN_POINT ( 'NONE',  ( -0.2493438320209966919, 0.05413385826771626580, -0.4176697321401330321 ) ) ;
#41398 = CARTESIAN_POINT ( 'NONE',  ( 0.7808398950131241190, -0.05778040916215560624, -0.4822834645669293319 ) ) ;
#41399 = CARTESIAN_POINT ( 'NONE',  ( -0.04593175853018302557, 0.2952755905511811885, 0.1292274648535926551 ) ) ;
#41400 = CARTESIAN_POINT ( 'NONE',  ( 0.6824146981627303710, -0.5023911411419708095, 0.1820866141732285504 ) ) ;
#41401 = CARTESIAN_POINT ( 'NONE',  ( -1.364829396325458521, 0.2306618581243847221, -0.2411417322834647770 ) ) ;
#41402 = CARTESIAN_POINT ( 'NONE',  ( -1.679790026246718693, 0.2306618581243847221, -0.2411417322834647770 ) ) ;
#41403 = CARTESIAN_POINT ( 'NONE',  ( 0.1377952755905518800, -0.5400638737290844871, 0.3530559997133364547 ) ) ;
#41404 = CARTESIAN_POINT ( 'NONE',  ( 0.000000000000000000, 1.724409448818897461, 0.000000000000000000 ) ) ;
#41405 = CARTESIAN_POINT ( 'NONE',  ( -0.3917322834645671215, 0.1049643490035301469, -2.387139107611548905 ) ) ;
#41406 = ORIENTED_EDGE ( 'NONE', *, *, #49802, .F. ) ;
#41407 = ORIENTED_EDGE ( 'NONE', *, *, #20457, .T. ) ;
#41408 = CARTESIAN_POINT ( 'NONE',  ( 0.9711286089238851948, -0.6046776061558809534, -0.2411417322834644161 ) ) ;
#41409 = CARTESIAN_POINT ( 'NONE',  ( 0.5971128608923890191, -0.5511811023622046335, 0.09757992244046803654 ) ) ;
#41411 = LINE ( 'NONE', #78484, #779 ) ;
#41410 = CYLINDRICAL_SURFACE ( 'NONE', #49811, 0.4744094488188972947 ) ;
#41412 = CARTESIAN_POINT ( 'NONE',  ( 2.795275590551181466, 2.204724409448820310, 0.000000000000000000 ) ) ;
#41413 = CYLINDRICAL_SURFACE ( 'NONE', #17692, 0.09842519685039351207 ) ;
#41414 = CARTESIAN_POINT ( 'NONE',  ( 0.3917322834645670104, -0.1049643490035303411, -1.141076115485564202 ) ) ;
#41415 = CARTESIAN_POINT ( 'NONE',  ( 0.1070741851644053388, 0.3996062992125986035, -2.274934383202099397 ) ) ;
#41416 = CARTESIAN_POINT ( 'NONE',  ( -0.7939632545931750718, -0.05778040916215560624, -0.4822834645669293319 ) ) ;
#41417 = CARTESIAN_POINT ( 'NONE',  ( -0.7808398950131225646, -0.05778040916215522460, 0.4822834645669289988 ) ) ;
#41418 = CARTESIAN_POINT ( 'NONE',  ( 1.089238845144357537, -0.4281496062992124485, 0.4176697321401328655 ) ) ;
#41419 = ORIENTED_EDGE ( 'NONE', *, *, #9160, .F. ) ;
#41420 = CARTESIAN_POINT ( 'NONE',  ( 1.161417322834646271, 0.1660481256975883668, -0.3530559997133364547 ) ) ;
#41421 = ITEM_DEFINED_TRANSFORMATION ( 'NONE', 'NONE', #54405,  #22098 ) ;
#41422 = CARTESIAN_POINT ( 'NONE',  ( 1.666666666666667185, -0.004921259842519576551, 0.3153832671262227771 ) ) ;
#41423 = DIRECTION ( 'NONE',  ( -0.000000000000000000, -1.000000000000000000, -0.000000000000000000 ) ) ;
#41424 = CARTESIAN_POINT ( 'NONE',  ( -1.351706036745406347, -0.3690944881889763329, 0.3153832671262228327 ) ) ;
#41425 = FACE_OUTER_BOUND ( 'NONE', #63094, .T. ) ;
#41426 = CARTESIAN_POINT ( 'NONE',  ( 0.09186351706036827158, 0.05413385826771666132, 0.4176697321401328100 ) ) ;
#41427 = AXIS2_PLACEMENT_3D ( 'NONE', #38846, #6863, #58196 ) ;
#41429 = CARTESIAN_POINT ( 'NONE',  ( -1.646051170424378096, 0.8346805926620876059, 0.3149606299212598381 ) ) ;
#41428 = DIRECTION ( 'NONE',  ( 0.000000000000000000, 1.000000000000000000, -0.000000000000000000 ) ) ;
#41430 = CARTESIAN_POINT ( 'NONE',  ( -0.9645669291338575535, -0.4536011799217367080, 0.2665933059059888421 ) ) ;
#41431 = CARTESIAN_POINT ( 'NONE',  ( 0.7480314960629927956, 0.2952755905511811885, 0.000000000000000000 ) ) ;
#41432 = CARTESIAN_POINT ( 'NONE',  ( 1.279527559055118724, 0.07958543189024085140, 0.2665933059059887866 ) ) ;
#41433 = CARTESIAN_POINT ( 'NONE',  ( 0.3392501089628018329, 0.1958661417322835052, -1.156148663220785799 ) ) ;
#41434 = CARTESIAN_POINT ( 'NONE',  ( -0.9186351706036736120, 0.1283753931104748280, 0.1820866141732283561 ) ) ;
#41435 = CARTESIAN_POINT ( 'NONE',  ( 1.574803149606299746, -0.1870078740157480879, -0.4822834645669291653 ) ) ;
#41436 = CARTESIAN_POINT ( 'NONE',  ( 0.1509182436465724975, 1.937587712771704940, 0.2746401537082780453 ) ) ;
#41437 = CARTESIAN_POINT ( 'NONE',  ( -0.2690288713910754526, 0.2952755905511810774, -0.1292274648535930714 ) ) ;
#41438 = CARTESIAN_POINT ( 'NONE',  ( -1.397637795275589623, -0.4536011799217368745, -0.2665933059059886201 ) ) ;
#41439 = CARTESIAN_POINT ( 'NONE',  ( -0.2690288713910754526, 0.1771653543307087075, -0.09757992244046823083 ) ) ;
#41440 = CARTESIAN_POINT ( 'NONE',  ( -0.4724409448818890911, -0.1870078740157479769, 0.4822834645669291653 ) ) ;
#41441 = CARTESIAN_POINT ( 'NONE',  ( -1.581364829396324945, -0.08942795157528024563, -0.3641732283464568787 ) ) ;
#41442 = CARTESIAN_POINT ( 'NONE',  ( 0.1958661417322834775, 0.3392501089628018884, -0.2985757462280333452 ) ) ;
#41443 = CARTESIAN_POINT ( 'NONE',  ( 0.3149606299212603933, -0.1870078740157479769, 0.4822834645669291653 ) ) ;
#41444 = PLANE ( 'NONE',  #59310 ) ;
#41445 = CARTESIAN_POINT ( 'NONE',  ( 0.4724409448818897572, -0.1265901696524988906, -1.763123359580051952 ) ) ;
#41446 = CARTESIAN_POINT ( 'NONE',  ( -0.5971128608923877978, 0.2952755905511811885, 0.1292274648535926551 ) ) ;
#41447 = CARTESIAN_POINT ( 'NONE',  ( -0.2493438320209966919, -0.004921259842519870586, -0.3153832671262229437 ) ) ;
#41448 = EDGE_CURVE ( 'NONE', #4880, #38353, #31729, .T. ) ;
#41449 = CARTESIAN_POINT ( 'NONE',  ( -1.279527559055116948, 0.1660481256975883668, -0.3530559997133364547 ) ) ;
#41450 = CARTESIAN_POINT ( 'NONE',  ( -0.1574803149606292529, -0.1870078740157480879, -0.4822834645669291653 ) ) ;
#41451 = CARTESIAN_POINT ( 'NONE',  ( 0.4724409448818904789, -0.1870078740157480601, -0.3641732283464567677 ) ) ;
#41452 = CARTESIAN_POINT ( 'NONE',  ( -0.8464566929133852113, -0.4536011799217368745, -0.2665933059059886201 ) ) ;
#41453 = CARTESIAN_POINT ( 'NONE',  ( -0.9120734908136475250, 0.2952755905511811885, 0.1292274648535926551 ) ) ;
#41454 = CARTESIAN_POINT ( 'NONE',  ( -1.706036745406823485, 0.2306618581243848609, 0.2411417322834645549 ) ) ;
#41455 = CARTESIAN_POINT ( 'NONE',  ( 1.496062992125985147, -0.1870078740157479769, 0.4822834645669291653 ) ) ;
#41456 = CARTESIAN_POINT ( 'NONE',  ( 0.4606976121171817429, 1.423084236280321324, 2.139116380834042541 ) ) ;
#41457 = CARTESIAN_POINT ( 'NONE',  ( 0.7152230971128616943, -0.08942795157527998196, 0.3641732283464567121 ) ) ;
#41458 = CARTESIAN_POINT ( 'NONE',  ( 0.6889763779527566800, -0.5400638737290844871, 0.3530559997133364547 ) ) ;
#41459 = EDGE_CURVE ( 'NONE', #51397, #30609, #72198, .T. ) ;
#41460 = CARTESIAN_POINT ( 'NONE',  ( 1.200787401574803681, -0.4536011799217368745, -0.2665933059059886201 ) ) ;
#41461 = VERTEX_POINT ( 'NONE', #75133 ) ;
#41462 = CARTESIAN_POINT ( 'NONE',  ( -0.7545931758530176614, -0.6692913385826773087, -0.1292274648535924053 ) ) ;
#41463 = CARTESIAN_POINT ( 'NONE',  ( 0.3996062992125984925, 0.1070741851644054637, -2.721128608923884418 ) ) ;
#41464 = CARTESIAN_POINT ( 'NONE',  ( -1.377952755905511140, -0.5511811023622047445, 6.969142054262312111E-17 ) ) ;
#41465 = CARTESIAN_POINT ( 'NONE',  ( -0.9908136482939626788, 0.2952755905511811885, 0.1292274648535926551 ) ) ;
#41466 = CARTESIAN_POINT ( 'NONE',  ( 0.1574803149606306130, -0.1870078740157479769, 0.4822834645669291653 ) ) ;
#41467 = CARTESIAN_POINT ( 'NONE',  ( -1.345144356955379816, -0.08942795157528024563, -0.3641732283464568787 ) ) ;
#41468 = CARTESIAN_POINT ( 'NONE',  ( -0.3996062992125985480, -7.340648628747423112E-17, -2.320866141732283783 ) ) ;
#41469 = CARTESIAN_POINT ( 'NONE',  ( -1.397637795275589623, 0.1660481256975885056, 0.3530559997133364547 ) ) ;
#41470 = CARTESIAN_POINT ( 'NONE',  ( 0.5052493438320218022, -0.6692913385826773087, -0.1292274648535924053 ) ) ;
#41471 = CARTESIAN_POINT ( 'NONE',  ( 0.2755905511811031494, 0.2952755905511811885, 0.000000000000000000 ) ) ;
#41472 = CARTESIAN_POINT ( 'NONE',  ( 1.305774278215223960, 0.2952755905511810774, -0.1292274648535930714 ) ) ;
#41473 = CARTESIAN_POINT ( 'NONE',  ( 0.4531182788721078158, 1.535433070866141447, 0.5309055118110234117 ) ) ;
#41474 = CARTESIAN_POINT ( 'NONE',  ( -0.3460692066303958092, -0.1998031496062994683, -1.627296587926509330 ) ) ;
#41475 = CARTESIAN_POINT ( 'NONE',  ( 0.3949938075777409963, 2.418639510665530435E-17, -1.220472440944881942 ) ) ;
#41476 = CARTESIAN_POINT ( 'NONE',  ( -0.1070741851644056997, 0.3996062992125986035, -2.368766404199475151 ) ) ;
#41477 = FACE_OUTER_BOUND ( 'NONE', #32174, .T. ) ;
#41478 = CARTESIAN_POINT ( 'NONE',  ( -0.3917322834645670104, -7.196005306013484475E-17, -0.1889763779527558474 ) ) ;
#41479 = CARTESIAN_POINT ( 'NONE',  ( -0.2099737532808391705, -0.5023911411419708095, -0.1820866141732282451 ) ) ;
#41480 = CARTESIAN_POINT ( 'NONE',  ( -0.2690288713910754526, 0.2952755905511810774, -0.1292274648535930714 ) ) ;
#41481 = CARTESIAN_POINT ( 'NONE',  ( 0.7086614173228352742, -0.1870078740157480879, -0.4822834645669291653 ) ) ;
#41482 = CARTESIAN_POINT ( 'NONE',  ( 0.1058382717557500852, -0.3949938075777408852, -2.209317585301837639 ) ) ;
#41483 = CARTESIAN_POINT ( 'NONE',  ( -0.06561679790026180015, -0.004921259842519576551, 0.3153832671262227771 ) ) ;
#41484 = CARTESIAN_POINT ( 'NONE',  ( -1.023622047244093558, -0.1870078740157479769, 0.4822834645669291653 ) ) ;
#41485 = CARTESIAN_POINT ( 'NONE',  ( 1.240157480314961314, -0.5400638737290844871, 0.3530559997133364547 ) ) ;
#41486 = CARTESIAN_POINT ( 'NONE',  ( 0.1265901696524990294, -0.4724409448818896462, -2.604986876640420057 ) ) ;
#41487 = CYLINDRICAL_SURFACE ( 'NONE', #45183, 0.3937007874015748254 ) ;
#41488 = ORIENTED_EDGE ( 'NONE', *, *, #6986, .F. ) ;
#41489 = ORIENTED_EDGE ( 'NONE', *, *, #43698, .F. ) ;
#41490 = CARTESIAN_POINT ( 'NONE',  ( 0.9776902887139113929, 0.2952755905511811885, 0.1292274648535926551 ) ) ;
#41491 = EDGE_CURVE ( 'NONE', #74617, #60812, #12050, .T. ) ;
#41492 = CARTESIAN_POINT ( 'NONE',  ( -1.561679790026246017, 0.05413385826771666132, 0.4176697321401328100 ) ) ;
#41494 = CARTESIAN_POINT ( 'NONE',  ( -1.049868766404198794, -0.6046776061558807314, 0.2411417322834647770 ) ) ;
#41493 = CARTESIAN_POINT ( 'NONE',  ( -1.181102362204723644, -0.1870078740157479769, 0.3641732283464567677 ) ) ;
#41495 = CARTESIAN_POINT ( 'NONE',  ( -0.2867679344610364334, -0.2867679344610367109, 0.1712598425196849850 ) ) ;
#41496 = DIRECTION ( 'NONE',  ( 0.000000000000000000, 0.000000000000000000, -1.000000000000000000 ) ) ;
#41497 = CARTESIAN_POINT ( 'NONE',  ( 1.154855643044620184, -0.6046776061558807314, 0.2411417322834647770 ) ) ;
#41498 = CARTESIAN_POINT ( 'NONE',  ( 1.220472440944881054, 0.4405861044731111953, -0.5309055118110239668 ) ) ;
#41499 = CARTESIAN_POINT ( 'NONE',  ( -0.2821522309711278487, 0.2952755905511811885, 0.1292274648535926551 ) ) ;
#41500 = CARTESIAN_POINT ( 'NONE',  ( -0.4921259842519677963, -0.5400638737290844871, 0.3530559997133364547 ) ) ;
#41501 = CARTESIAN_POINT ( 'NONE',  ( -1.115485564304461219, 0.05413385826771626580, -0.4176697321401330321 ) ) ;
#41502 = CARTESIAN_POINT ( 'NONE',  ( 4.797336870675656522E-17, -0.3917322834645670104, -0.005905511811023714773 ) ) ;
#41503 = CARTESIAN_POINT ( 'NONE',  ( 0.1377952755905518800, -0.5400638737290844871, 0.3530559997133364547 ) ) ;
#41504 = CARTESIAN_POINT ( 'NONE',  ( -0.2867679344610365999, 0.2867679344610364889, -2.374015748031496287 ) ) ;
#41505 = CARTESIAN_POINT ( 'NONE',  ( -1.404199475065615932, -0.3690944881889765550, -0.3153832671262227771 ) ) ;
#41506 = ORIENTED_EDGE ( 'NONE', *, *, #32892, .T. ) ;
#41507 = CARTESIAN_POINT ( 'NONE',  ( -0.3420746716998659953, -0.1974969037888706647, -2.257217847769029007 ) ) ;
#41508 = ORIENTED_EDGE ( 'NONE', *, *, #2607, .F. ) ;
#41509 = CARTESIAN_POINT ( 'NONE',  ( -1.382164990278195615, 1.299212598425196985, 0.4102808022082835571 ) ) ;
#41510 = CARTESIAN_POINT ( 'NONE',  ( 1.594488188976378673, 0.07958543189024085140, 0.2665933059059887866 ) ) ;
#41511 = CARTESIAN_POINT ( 'NONE',  ( -0.3996062992125987146, 0.1070741851644051862, -0.9776902887139107268 ) ) ;
#41512 = CARTESIAN_POINT ( 'NONE',  ( -1.686351706036744558, 0.2952755905511810774, -0.1292274648535930714 ) ) ;
#41513 = DIRECTION ( 'NONE',  ( 0.000000000000000000, 8.881784197001252323E-16, -1.000000000000000000 ) ) ;
#41514 = CARTESIAN_POINT ( 'NONE',  ( -0.9842519685039360366, 0.2952755905511811885, 0.000000000000000000 ) ) ;
#41515 = CARTESIAN_POINT ( 'NONE',  ( 2.795275590551181910, 1.771653543307087242, 0.000000000000000000 ) ) ;
#41516 = CARTESIAN_POINT ( 'NONE',  ( -9.594673741351313045E-17, 0.3917322834645670104, -0.08464566929133868212 ) ) ;
#41517 = CARTESIAN_POINT ( 'NONE',  ( -0.3346456692913377662, 0.07958543189024071263, -0.2665933059059888421 ) ) ;
#41518 = CARTESIAN_POINT ( 'NONE',  ( -0.7545931758530177724, 0.1771653543307087630, 0.09757992244046791164 ) ) ;
#41519 = CARTESIAN_POINT ( 'NONE',  ( -1.017060367454067249, -0.05778040916215522460, 0.4822834645669289988 ) ) ;
#41520 = CARTESIAN_POINT ( 'NONE',  ( 0.4002624671916016896, -0.3162353388693409650, -0.4822834645669289433 ) ) ;
#41521 = CARTESIAN_POINT ( 'NONE',  ( -0.8136482939632537770, 0.2306618581243847221, -0.2411417322834647770 ) ) ;
#41522 = FACE_OUTER_BOUND ( 'NONE', #2148, .T. ) ;
#41523 = ORIENTED_EDGE ( 'NONE', *, *, #51624, .T. ) ;
#41524 = CARTESIAN_POINT ( 'NONE',  ( -1.187664041994749731, -0.3162353388693405765, 0.4822834645669290543 ) ) ;
#41525 = DIRECTION ( 'NONE',  ( 1.000000000000000000, -0.000000000000000000, -0.000000000000000000 ) ) ;
#41526 = CARTESIAN_POINT ( 'NONE',  ( -0.3458507752293906723, -0.3458507752293910609, -1.476377952755905554 ) ) ;
#41527 = DIRECTION ( 'NONE',  ( 1.000000000000000000, 3.469446951953613203E-16, 0.000000000000000000 ) ) ;
#41528 = CARTESIAN_POINT ( 'NONE',  ( -0.3917322834645669549, -0.1049643490035306603, -0.6679790026246719137 ) ) ;
#41529 = CARTESIAN_POINT ( 'NONE',  ( -0.2867679344610366554, 0.2867679344610365444, -2.309055118110236116 ) ) ;
#41530 = CARTESIAN_POINT ( 'NONE',  ( -0.6955380577427815458, 0.05413385826771666132, 0.4176697321401328100 ) ) ;
#41531 = CARTESIAN_POINT ( 'NONE',  ( 1.417322834645670104, -0.1870078740157480879, -0.4822834645669291653 ) ) ;
#41532 = CARTESIAN_POINT ( 'NONE',  ( 0.3996062992125986035, -0.1070741851644052972, -0.5032808398950130435 ) ) ;
#41534 = CARTESIAN_POINT ( 'NONE',  ( -0.6423408027444563739, -2.609869883881465018E-15, -0.3464511005275220379 ) ) ;
#41533 = CARTESIAN_POINT ( 'NONE',  ( -0.6399301791983041943, -2.567464376874931580E-15, -0.4445507791589072832 ) ) ;
#41535 = CARTESIAN_POINT ( 'NONE',  ( -1.469816272965878357, -0.6046776061558809534, -0.2411417322834644161 ) ) ;
#41536 = CARTESIAN_POINT ( 'NONE',  ( -0.7480314960629914633, 0.2952755905511811885, 0.000000000000000000 ) ) ;
#41537 = CARTESIAN_POINT ( 'NONE',  ( 0.3392501089628018329, 0.1958661417322835052, -0.05378645849637612303 ) ) ;
#41538 = CARTESIAN_POINT ( 'NONE',  ( 0.5971128608923890191, -0.5511811023622046335, 0.09757992244046803654 ) ) ;
#41539 = CARTESIAN_POINT ( 'NONE',  ( 0.1049643490035303689, 0.3917322834645670104, -0.2355643044619423199 ) ) ;
#41540 = CARTESIAN_POINT ( 'NONE',  ( 0.3543307086614181922, -0.5511811023622047445, 6.969142054262312111E-17 ) ) ;
#41541 = CARTESIAN_POINT ( 'NONE',  ( 1.141732283464567566, 0.1771653543307087630, 0.000000000000000000 ) ) ;
#41542 = CARTESIAN_POINT ( 'NONE',  ( 1.167979002624672580, 0.05413385826771626580, -0.4176697321401330321 ) ) ;
#41543 = CARTESIAN_POINT ( 'NONE',  ( -0.1115485564304453947, -0.5511811023622046335, 0.09757992244046803654 ) ) ;
#41544 = CARTESIAN_POINT ( 'NONE',  ( -0.1049643490035302024, -0.3917322834645671215, -2.269028871391075786 ) ) ;
#41545 = CARTESIAN_POINT ( 'NONE',  ( -1.601049868766403650, 0.2306618581243847221, -0.2411417322834647770 ) ) ;
#41546 = CARTESIAN_POINT ( 'NONE',  ( -1.089238845144356427, -0.3690944881889765550, -0.3153832671262227771 ) ) ;
#41547 = CARTESIAN_POINT ( 'NONE',  ( -0.3458507752293909498, 0.3458507752293907833, -0.5688976377952755792 ) ) ;
#41548 = CARTESIAN_POINT ( 'NONE',  ( -1.030183727034119867, -0.2845877964562159024, 0.3641732283464567677 ) ) ;
#41549 = ADVANCED_FACE ( 'NONE', ( #36809 ), #24176, .F. ) ;
#41550 = CARTESIAN_POINT ( 'NONE',  ( -0.02624671916010428221, 0.2306618581243847221, -0.2411417322834647770 ) ) ;
#41551 = DIRECTION ( 'NONE',  ( 0.000000000000000000, 1.000000000000000000, 0.000000000000000000 ) ) ;
#41552 = CARTESIAN_POINT ( 'NONE',  ( 0.7217847769028878924, -0.3690944881889765550, -0.3153832671262227771 ) ) ;
#41553 = CARTESIAN_POINT ( 'NONE',  ( -0.1246719160104980823, 0.1771653543307087630, 0.09757992244046791164 ) ) ;
#41554 = CARTESIAN_POINT ( 'NONE',  ( -0.9120734908136475250, -0.6692913385826773087, -0.1292274648535924053 ) ) ;
#41555 = CARTESIAN_POINT ( 'NONE',  ( -2.795275590551185907, 0.5118110236220471121, -3.981376139758521912E-16 ) ) ;
#41556 = DIRECTION ( 'NONE',  ( 0.000000000000000000, 0.000000000000000000, -1.000000000000000000 ) ) ;
#41557 = CARTESIAN_POINT ( 'NONE',  ( 0.2887139107611556010, 0.2306618581243847221, -0.2411417322834647770 ) ) ;
#41558 = CARTESIAN_POINT ( 'NONE',  ( -0.3460692066303957537, -0.1998031496062994405, -1.546587926509186639 ) ) ;
#41559 = CARTESIAN_POINT ( 'NONE',  ( 1.220472440944882386, -0.1870078740157480046, 1.254653134982923898E-17 ) ) ;
#41560 = CARTESIAN_POINT ( 'NONE',  ( -0.3543307086614165824, -0.5511811023622047445, 6.969142054262312111E-17 ) ) ;
#41561 = CARTESIAN_POINT ( 'NONE',  ( -0.2427821522309703550, -0.05778040916215560624, -0.4822834645669293319 ) ) ;
#41562 = CARTESIAN_POINT ( 'NONE',  ( -1.627296587926508442, 0.2306618581243848609, 0.2411417322834645549 ) ) ;
#41563 = CARTESIAN_POINT ( 'NONE',  ( 1.502624671916010790, -0.05778040916215522460, 0.4822834645669289988 ) ) ;
#41564 = CARTESIAN_POINT ( 'NONE',  ( 1.122047244094488860, -0.5400638737290845981, -0.3530559997133363437 ) ) ;
#41565 = CARTESIAN_POINT ( 'NONE',  ( -0.5708661417322828946, 0.07958543189024071263, -0.2665933059059888421 ) ) ;
#41566 = CARTESIAN_POINT ( 'NONE',  ( 0.3460692066303958092, 0.1998031496062993018, -0.3654855643044619407 ) ) ;
#41567 = CARTESIAN_POINT ( 'NONE',  ( -0.3996062992125986035, -0.1070741851644056997, -0.5183727034120735322 ) ) ;
#41568 = CARTESIAN_POINT ( 'NONE',  ( -0.2867679344610365444, -0.2867679344610367664, -2.732958948327771420 ) ) ;
#41569 = CARTESIAN_POINT ( 'NONE',  ( 1.614173228346457156, 1.496062992125984037, 0.5309055118110233007 ) ) ;
#41570 = CARTESIAN_POINT ( 'NONE',  ( 1.174540682414699111, -0.08942795157528024563, -0.3641732283464568787 ) ) ;
#41571 = CARTESIAN_POINT ( 'NONE',  ( -1.522309711286088607, 0.2306618581243847221, -0.2411417322834647770 ) ) ;
#41572 = CARTESIAN_POINT ( 'NONE',  ( 0.9120734908136489683, -0.6692913385826771977, 0.1292274648535927661 ) ) ;
#41573 = CARTESIAN_POINT ( 'NONE',  ( -0.3420746716998662729, 0.1974969037888702206, -0.7329396325459319739 ) ) ;
#41574 = CARTESIAN_POINT ( 'NONE',  ( 1.115485564304462551, -0.3690944881889765550, -0.3153832671262227771 ) ) ;
#41575 = CARTESIAN_POINT ( 'NONE',  ( -0.09186351706036663400, -0.4281496062992124485, 0.4176697321401328655 ) ) ;
#41576 = CARTESIAN_POINT ( 'NONE',  ( -0.5183727034120726440, 0.2952755905511811885, 0.1292274648535926551 ) ) ;
#41577 = DIRECTION ( 'NONE',  ( 0.000000000000000000, 0.000000000000000000, 1.000000000000000000 ) ) ;
#41578 = CARTESIAN_POINT ( 'NONE',  ( 0.2362204724409451007, -0.4091458600556402980, -0.8792650918635170898 ) ) ;
#41579 = CARTESIAN_POINT ( 'NONE',  ( -0.1998031496062994683, 0.3460692066303958092, -2.375328083989501238 ) ) ;
#41580 = CARTESIAN_POINT ( 'NONE',  ( 0.4396325459317590445, -0.5511811023622046335, 0.09757992244046803654 ) ) ;
#41581 = ORIENTED_EDGE ( 'NONE', *, *, #56862, .F. ) ;
#41582 = CARTESIAN_POINT ( 'NONE',  ( 4.797336870675656522E-17, -0.3917322834645670659, -0.3904392632884007841 ) ) ;
#41583 = ORIENTED_EDGE ( 'NONE', *, *, #46355, .F. ) ;
#41584 = CARTESIAN_POINT ( 'NONE',  ( -0.5446194225721777693, -0.3162353388693409650, -0.4822834645669289433 ) ) ;
#41585 = CARTESIAN_POINT ( 'NONE',  ( 1.049868766404200127, -0.6046776061558809534, -0.2411417322834644161 ) ) ;
#41586 = CARTESIAN_POINT ( 'NONE',  ( 0.09186351706036827158, 0.05413385826771666132, 0.4176697321401328100 ) ) ;
#41587 = CARTESIAN_POINT ( 'NONE',  ( -0.4396325459317577122, -0.5511811023622048555, -0.09757992244046775898 ) ) ;
#41588 = CARTESIAN_POINT ( 'NONE',  ( 0.7349081364829403995, 0.2306618581243848609, 0.2411417322834645549 ) ) ;
#41589 = CARTESIAN_POINT ( 'NONE',  ( -0.9383202099737524282, -0.3162353388693409650, -0.4822834645669289433 ) ) ;
#41590 = CARTESIAN_POINT ( 'NONE',  ( -0.4461942257217840213, 0.2306618581243848609, 0.2411417322834645549 ) ) ;
#41591 = CARTESIAN_POINT ( 'NONE',  ( 1.076115485564305141, -0.6046776061558807314, 0.2411417322834647770 ) ) ;
#41592 = CARTESIAN_POINT ( 'NONE',  ( 0.9908136482939640111, 0.2952755905511810774, -0.1292274648535930714 ) ) ;
#41593 = CARTESIAN_POINT ( 'NONE',  ( 0.9645669291338591078, -0.5400638737290845981, -0.3530559997133363437 ) ) ;
#41594 = CARTESIAN_POINT ( 'NONE',  ( 0.2867679344610365999, -0.2867679344610365444, -0.5629921259842519676 ) ) ;
#41595 = CARTESIAN_POINT ( 'NONE',  ( 0.03937007874015833325, -0.5511811023622047445, 6.969142054262312111E-17 ) ) ;
#41596 = ORIENTED_EDGE ( 'NONE', *, *, #74789, .T. ) ;
#41597 = CARTESIAN_POINT ( 'NONE',  ( -0.2891555358219911054, 0.2891555358219909388, -0.9645669291338583307 ) ) ;
#41598 = ORIENTED_EDGE ( 'NONE', *, *, #54320, .T. ) ;
#41599 = CARTESIAN_POINT ( 'NONE',  ( -0.8727034120734901146, -0.08942795157528024563, -0.3641732283464568787 ) ) ;
#41600 = CARTESIAN_POINT ( 'NONE',  ( -0.5577427821522301654, -0.3162353388693405765, 0.4822834645669290543 ) ) ;
#41601 = DIRECTION ( 'NONE',  ( 0.000000000000000000, 0.000000000000000000, -1.000000000000000000 ) ) ;
#41602 = CARTESIAN_POINT ( 'NONE',  ( -0.3674540682414692561, -0.6046776061558809534, -0.2411417322834644161 ) ) ;
#41603 = CARTESIAN_POINT ( 'NONE',  ( -0.4724409448818890911, -0.1870078740157479769, 0.4822834645669291653 ) ) ;
#41605 = CARTESIAN_POINT ( 'NONE',  ( -1.482939632545930975, 0.05413385826771666132, 0.4176697321401328100 ) ) ;
#41604 = B_SPLINE_CURVE_WITH_KNOTS ( 'NONE', 3,
 ( #66884, #71944, #14296, #60548, #27313, #8795, #66459, #34049, #78686, #40774, #73613, #39957, #52972, #21009, #72363, #59712, #29387, #68522, #24303, #74018 ),
 .UNSPECIFIED., .F., .F.,
 ( 4, 2, 2, 2, 2, 2, 2, 2, 2, 4 ),
 ( 0.008504188499521210184, 0.009565469904607836610, 0.01009611060715114028, 0.01062675130969444395, 0.01168803271478104956, 0.01221867341732434456, 0.01274931411986764129, 0.01381059552495423129, 0.01487187693004082129, 0.01699443974021398046 ),
 .UNSPECIFIED. ) ;
#41606 = CARTESIAN_POINT ( 'NONE',  ( -1.456692913385826182, -0.6692913385826771977, 8.415575281601705876E-17 ) ) ;
#41607 = CARTESIAN_POINT ( 'NONE',  ( 0.9580052493438327987, -0.3690944881889765550, -0.3153832671262227771 ) ) ;
#41608 = CARTESIAN_POINT ( 'NONE',  ( -0.4724409448818898682, -8.678599364036362592E-17, -0.9842519685039369248 ) ) ;
#41609 = CARTESIAN_POINT ( 'NONE',  ( 0.2380158072512373602, 0.1747520019874606312, 5.672240063627637774 ) ) ;
#41610 = CARTESIAN_POINT ( 'NONE',  ( 0.4265091863517067039, -0.5511811023622048555, -0.09757992244046775898 ) ) ;
#41611 = CARTESIAN_POINT ( 'NONE',  ( 0.05905511811023709395, -0.5400638737290844871, 0.3530559997133364547 ) ) ;
#41612 = CARTESIAN_POINT ( 'NONE',  ( 0.2230971128608932319, -0.4281496062992124485, 0.4176697321401328655 ) ) ;
#41613 = ORIENTED_EDGE ( 'NONE', *, *, #38580, .T. ) ;
#41614 = CARTESIAN_POINT ( 'NONE',  ( 0.2925321140481932369, 0.2925321140481932369, -1.712598425196850460 ) ) ;
#41615 = CARTESIAN_POINT ( 'NONE',  ( -1.586052503253848167, 1.023622047244095556, 0.1653254495020564929 ) ) ;
#41616 = VERTEX_POINT ( 'NONE', #46008 ) ;
#41617 = CARTESIAN_POINT ( 'NONE',  ( -0.3996062992125986590, 0.1070741851644051723, -1.369422572178477404 ) ) ;
#41618 = CARTESIAN_POINT ( 'NONE',  ( 0.1070741851644053388, 0.3996062992125986035, -0.7001312335958002064 ) ) ;
#41619 = CARTESIAN_POINT ( 'NONE',  ( -0.5708661417322828946, 0.07958543189024071263, -0.2665933059059888421 ) ) ;
#41620 = CARTESIAN_POINT ( 'NONE',  ( -0.8792650918635160906, 0.05413385826771626580, -0.4176697321401330321 ) ) ;
#41621 = CARTESIAN_POINT ( 'NONE',  ( -0.4724409448818899238, 0.1265901696524986686, 0.1246719160104986929 ) ) ;
#41622 = CARTESIAN_POINT ( 'NONE',  ( -0.2867679344610364334, -0.2867679344610367109, -2.348425196850393970 ) ) ;
#41623 = CARTESIAN_POINT ( 'NONE',  ( 1.627296587926509996, -0.6046776061558807314, 0.2411417322834647770 ) ) ;
#41624 = CARTESIAN_POINT ( 'NONE',  ( 1.023622047244095112, -0.1870078740157480879, -0.4822834645669291653 ) ) ;
#41625 = CARTESIAN_POINT ( 'NONE',  ( 0.3280839895013130669, -0.4281496062992127816, -0.4176697321401328100 ) ) ;
#41626 = CARTESIAN_POINT ( 'NONE',  ( -0.5249343832020990641, 0.1283753931104748280, 0.1820866141732283561 ) ) ;
#41627 = CARTESIAN_POINT ( 'NONE',  ( 0.1706036745406830368, 0.05413385826771666132, 0.4176697321401328100 ) ) ;
#41628 = CARTESIAN_POINT ( 'NONE',  ( -0.4091458600556402980, -0.2362204724409451284, -1.861548556430446144 ) ) ;
#41629 = CARTESIAN_POINT ( 'NONE',  ( -0.2034120734908128059, 0.1771653543307087630, 0.09757992244046791164 ) ) ;
#41630 = CARTESIAN_POINT ( 'NONE',  ( -0.6036745406824141069, 0.2306618581243848609, 0.2411417322834645549 ) ) ;
#41631 = CARTESIAN_POINT ( 'NONE',  ( 0.2891555358219910499, -0.2891555358219909944, -1.907480314960629419 ) ) ;
#41632 = CARTESIAN_POINT ( 'NONE',  ( -1.496062992125983815, -0.1870078740157480879, -0.4822834645669291653 ) ) ;
#41633 = CARTESIAN_POINT ( 'NONE',  ( 0.2099737532808405305, 0.1283753931104746893, -0.1820866141732285504 ) ) ;
#41634 = DIRECTION ( 'NONE',  ( -0.000000000000000000, -0.000000000000000000, 1.000000000000000000 ) ) ;
#41635 = CARTESIAN_POINT ( 'NONE',  ( -0.9908136482939626788, -0.6692913385826773087, -0.1292274648535924053 ) ) ;
#41636 = CARTESIAN_POINT ( 'NONE',  ( -0.6824146981627288167, 0.1283753931104748280, 0.1820866141732283561 ) ) ;
#41637 = CARTESIAN_POINT ( 'NONE',  ( 0.4091458600556403535, 0.2362204724409449896, -2.255249343832020692 ) ) ;
#41638 = CARTESIAN_POINT ( 'NONE',  ( -1.023622047244094002, -0.1870078740157480879, -0.4822834645669291653 ) ) ;
#41639 = CARTESIAN_POINT ( 'NONE',  ( 0.1640419947506569498, -0.3162353388693409650, -0.4822834645669289433 ) ) ;
#41640 = CARTESIAN_POINT ( 'NONE',  ( 0.1070741851644054776, -0.3996062992125984925, -2.681758530183727895 ) ) ;
#41641 = EDGE_CURVE ( 'NONE', #12714, #22431, #15737, .T. ) ;
#41642 = CARTESIAN_POINT ( 'NONE',  ( -0.2867679344610366554, 0.2867679344610365444, -2.619403256396638735 ) ) ;
#41643 = CARTESIAN_POINT ( 'NONE',  ( -2.139011644334197104, 1.422882880004775918, -0.4606469518571241206 ) ) ;
#41644 = CARTESIAN_POINT ( 'NONE',  ( 0.2296587926509192634, -0.2845877964562159024, 0.3641732283464567677 ) ) ;
#41645 = CARTESIAN_POINT ( 'NONE',  ( 1.167979002624672580, 0.05413385826771626580, -0.4176697321401330321 ) ) ;
#41646 = CARTESIAN_POINT ( 'NONE',  ( -1.391076115485563758, 0.1283753931104748280, 0.1820866141732283561 ) ) ;
#41647 = CARTESIAN_POINT ( 'NONE',  ( 1.167979002624672580, -0.4281496062992124485, 0.4176697321401328655 ) ) ;
#41648 = CARTESIAN_POINT ( 'NONE',  ( -1.660104986876639543, -0.08942795157528024563, -0.3641732283464568787 ) ) ;
#41649 = CARTESIAN_POINT ( 'NONE',  ( -0.4855643044619415427, -0.4281496062992124485, 0.4176697321401328655 ) ) ;
#41650 = CARTESIAN_POINT ( 'NONE',  ( 0.01312335958005323398, -0.3690944881889765550, -0.3153832671262227771 ) ) ;
#41651 = CARTESIAN_POINT ( 'NONE',  ( 1.306827173596999403, 0.000000000000000000, -0.4445507791589060620 ) ) ;
#41652 = CARTESIAN_POINT ( 'NONE',  ( 0.5905511811023629321, -0.5511811023622047445, 6.969142054262312111E-17 ) ) ;
#41653 = CARTESIAN_POINT ( 'NONE',  ( -0.07874015748031421014, -0.1870078740157479769, 0.4822834645669291653 ) ) ;
#41654 = CARTESIAN_POINT ( 'NONE',  ( 0.3460692066303959202, -0.1998031496062991630, -0.1817585301837270351 ) ) ;
#41655 = CARTESIAN_POINT ( 'NONE',  ( -1.272965879265091305, -0.4281496062992124485, 0.4176697321401328655 ) ) ;
#41656 = CARTESIAN_POINT ( 'NONE',  ( -0.3392501089628019995, 0.1958661417322832277, -1.843175853018372834 ) ) ;
#41657 = CARTESIAN_POINT ( 'NONE',  ( 1.082677165354331228, -0.4536011799217367080, 0.2665933059059888421 ) ) ;
#41658 = CARTESIAN_POINT ( 'NONE',  ( 0.2165354330708668673, -0.5400638737290844871, 0.3530559997133364547 ) ) ;
#41659 = CARTESIAN_POINT ( 'NONE',  ( -0.3346456692913377662, 0.1660481256975883668, -0.3530559997133364547 ) ) ;
#41660 = CARTESIAN_POINT ( 'NONE',  ( -0.2165354330708654795, 0.07958543189024085140, 0.2665933059059887866 ) ) ;
#41661 = DIRECTION ( 'NONE',  ( 1.000000000000000000, 8.805702923740138355E-17, -0.000000000000000000 ) ) ;
#41662 = CARTESIAN_POINT ( 'NONE',  ( -0.4068241469816264999, -0.3690944881889763329, 0.3153832671262228327 ) ) ;
#41663 = CARTESIAN_POINT ( 'NONE',  ( 0.3346456692913393205, -0.5400638737290845981, -0.3530559997133363437 ) ) ;
#41664 = CARTESIAN_POINT ( 'NONE',  ( -1.220472440944881054, 0.1771653543307087630, 0.000000000000000000 ) ) ;
#41665 = CARTESIAN_POINT ( 'NONE',  ( -0.2925321140481932369, 0.2925321140481931259, -1.041338582677165281 ) ) ;
#41666 = CARTESIAN_POINT ( 'NONE',  ( -0.9842519685039360366, 0.2952755905511811885, 0.000000000000000000 ) ) ;
#41667 = CARTESIAN_POINT ( 'NONE',  ( 0.4606732211678803424, 1.778019097314518016, -0.5309055118110237448 ) ) ;
#41668 = VERTEX_POINT ( 'NONE', #66539 ) ;
#41669 = CARTESIAN_POINT ( 'NONE',  ( -1.706036745406823485, 0.1283753931104748280, 0.1820866141732283561 ) ) ;
#41670 = CARTESIAN_POINT ( 'NONE',  ( -0.5511811023622041894, -0.1870078740157480879, -0.4822834645669291653 ) ) ;
#41671 = CARTESIAN_POINT ( 'NONE',  ( 0.2510736293007090891, 1.134572453438782214, 2.808463035490861071 ) ) ;
#41672 = CARTESIAN_POINT ( 'NONE',  ( -1.233595800524933894, -0.6046776061558809534, -0.2411417322834644161 ) ) ;
#41673 = CARTESIAN_POINT ( 'NONE',  ( 0.3726288332213487653, 0.1208384647389236927, -1.220472440944882164 ) ) ;
#41674 = CARTESIAN_POINT ( 'NONE',  ( 1.377952755905512472, 0.2952755905511811885, 0.000000000000000000 ) ) ;
#41675 = CARTESIAN_POINT ( 'NONE',  ( 0.7283464566929143125, 0.1660481256975885056, 0.3530559997133364547 ) ) ;
#41676 = CARTESIAN_POINT ( 'NONE',  ( 0.2814773692359251456, -0.08976595949324575607, 5.548806511850565393 ) ) ;
#41677 = CARTESIAN_POINT ( 'NONE',  ( 1.548556430446194954, -0.5023911411419708095, 0.1820866141732285504 ) ) ;
#41678 = CARTESIAN_POINT ( 'NONE',  ( -0.2925321140481932924, 0.2925321140481931814, -0.4921259842519684624 ) ) ;
#41679 = ORIENTED_EDGE ( 'NONE', *, *, #35281, .F. ) ;
#41680 = CARTESIAN_POINT ( 'NONE',  ( -0.4199475065616791736, -0.5023911411419708095, 0.1820866141732285504 ) ) ;
#41681 = CARTESIAN_POINT ( 'NONE',  ( -0.2867679344610365999, 0.2867679344610364889, -2.374015748031496287 ) ) ;
#41682 = ORIENTED_EDGE ( 'NONE', *, *, #4697, .F. ) ;
#41683 = CARTESIAN_POINT ( 'NONE',  ( 0.7283464566929140904, -0.5400638737290845981, -0.3530559997133363437 ) ) ;
#41684 = CARTESIAN_POINT ( 'NONE',  ( -0.1968503937007867743, -0.6692913385826771977, 8.415575281601705876E-17 ) ) ;
#41685 = CARTESIAN_POINT ( 'NONE',  ( -0.9251968503937002541, -0.5400638737290845981, -0.3530559997133363437 ) ) ;
#41686 = CARTESIAN_POINT ( 'NONE',  ( 1.312335958005250269, -0.6046776061558807314, 0.2411417322834647770 ) ) ;
#41687 = CARTESIAN_POINT ( 'NONE',  ( -1.325459317585300889, -0.004921259842519576551, 0.3153832671262227771 ) ) ;
#41688 = CARTESIAN_POINT ( 'NONE',  ( -0.4732141852945584981, 1.572163861244849636, -2.557193068050839013 ) ) ;
#41689 = CARTESIAN_POINT ( 'NONE',  ( 0.3215223097112867578, -0.3162353388693409650, -0.4822834645669289433 ) ) ;
#41690 = CARTESIAN_POINT ( 'NONE',  ( -0.8989501312335946848, -0.6692913385826771977, 0.1292274648535927661 ) ) ;
#41691 = CARTESIAN_POINT ( 'NONE',  ( -9.594673741351310580E-17, 0.3917322834645669549, -1.497356012302150763 ) ) ;
#41692 = CARTESIAN_POINT ( 'NONE',  ( -1.279527559055116948, 0.1660481256975883668, -0.3530559997133364547 ) ) ;
#41693 = DIRECTION ( 'NONE',  ( -1.000000000000000000, 0.000000000000000000, 1.692413147294446216E-16 ) ) ;
#41694 = CARTESIAN_POINT ( 'NONE',  ( 0.8136482939632553313, -0.6046776061558809534, -0.2411417322834644161 ) ) ;
#41695 = CARTESIAN_POINT ( 'NONE',  ( 1.482939632545932307, -0.3690944881889763329, 0.3153832671262228327 ) ) ;
#41696 = ORIENTED_EDGE ( 'NONE', *, *, #55977, .T. ) ;
#41697 = CARTESIAN_POINT ( 'NONE',  ( 0.3917322834645670659, -0.1049643490035303273, -2.942932701608610646 ) ) ;
#41698 = CARTESIAN_POINT ( 'NONE',  ( -0.2887139107611542133, -0.6046776061558809534, -0.2411417322834644161 ) ) ;
#41699 = EDGE_LOOP ( 'NONE', ( #58884, #61041 ) ) ;
#41700 = CARTESIAN_POINT ( 'NONE',  ( 0.3608923884514443348, 0.1771653543307087075, -0.09757992244046823083 ) ) ;
#41701 = CARTESIAN_POINT ( 'NONE',  ( -1.207349081364828880, 0.2306618581243847221, -0.2411417322834647770 ) ) ;
#41702 = CARTESIAN_POINT ( 'NONE',  ( 1.010498687664042716, 0.05413385826771626580, -0.4176697321401330321 ) ) ;
#41703 = CARTESIAN_POINT ( 'NONE',  ( 1.003937007874016185, 0.1660481256975883668, -0.3530559997133364547 ) ) ;
#41704 = CARTESIAN_POINT ( 'NONE',  ( -0.3215223097112853146, -0.3162353388693405765, 0.4822834645669290543 ) ) ;
#41705 = AXIS2_PLACEMENT_3D ( 'NONE', #78064, #20394, #19135 ) ;
#41706 = CARTESIAN_POINT ( 'NONE',  ( -0.2867679344610365444, -0.2867679344610367664, -1.315636113682101982 ) ) ;
#41707 = CARTESIAN_POINT ( 'NONE',  ( -0.7414698162729651543, -0.6692913385826771977, 0.1292274648535927661 ) ) ;
#41708 = CARTESIAN_POINT ( 'NONE',  ( -0.1049643490035302024, -0.3917322834645671215, -2.204068241469816503 ) ) ;
#41709 = CARTESIAN_POINT ( 'NONE',  ( -1.417322834645668772, -0.1870078740157479769, 0.4822834645669291653 ) ) ;
#41710 = CARTESIAN_POINT ( 'NONE',  ( -0.5052493438320203589, 0.2952755905511810774, -0.1292274648535930714 ) ) ;
#41711 = CARTESIAN_POINT ( 'NONE',  ( 1.240157480314961314, 0.1660481256975883668, -0.3530559997133364547 ) ) ;
#41712 = CARTESIAN_POINT ( 'NONE',  ( 1.417322834645670104, -0.1870078740157480879, -0.4822834645669291653 ) ) ;
#41713 = CARTESIAN_POINT ( 'NONE',  ( -0.9645669291338575535, -0.5400638737290844871, 0.3530559997133364547 ) ) ;
#41714 = CARTESIAN_POINT ( 'NONE',  ( -0.2925321140481930149, -0.2925321140481933480, 0.02165354330708659653 ) ) ;
#41715 = CARTESIAN_POINT ( 'NONE',  ( 0.8661417322834652488, -0.1870078740157480879, -0.4822834645669291653 ) ) ;
#41716 = CARTESIAN_POINT ( 'NONE',  ( -0.3996062992125987146, 0.1070741851644051862, -1.765091863517059823 ) ) ;
#41717 = CARTESIAN_POINT ( 'NONE',  ( -0.6627296587926501115, 0.2952755905511810774, -0.1292274648535930714 ) ) ;
#41718 = CARTESIAN_POINT ( 'NONE',  ( -1.089238845144356427, -0.3690944881889765550, -0.3153832671262227771 ) ) ;
#41719 = CARTESIAN_POINT ( 'NONE',  ( 0.8070866141732289112, -0.4536011799217368745, -0.2665933059059886201 ) ) ;
#41720 = CARTESIAN_POINT ( 'NONE',  ( 0.3458507752293908943, 0.3458507752293908943, -0.6870078740157479213 ) ) ;
#41721 = CARTESIAN_POINT ( 'NONE',  ( 1.062992125984252745, 0.1771653543307087630, 0.000000000000000000 ) ) ;
#41722 = CARTESIAN_POINT ( 'NONE',  ( 0.9514435695538062676, -0.05778040916215522460, 0.4822834645669289988 ) ) ;
#41723 = CARTESIAN_POINT ( 'NONE',  ( 0.2891555358219910499, -0.2891555358219909944, -0.4901574803149606474 ) ) ;
#41724 = CARTESIAN_POINT ( 'NONE',  ( -0.4330708661417315697, 0.2952755905511811885, 0.000000000000000000 ) ) ;
#41725 = LINE ( 'NONE', #61915, #75446 ) ;
#41726 = CARTESIAN_POINT ( 'NONE',  ( 1.541994750656168645, -0.5511811023622046335, 0.09757992244046803654 ) ) ;
#41727 = CARTESIAN_POINT ( 'NONE',  ( -0.4002624671916004129, -0.05778040916215560624, -0.4822834645669293319 ) ) ;
#41728 = CARTESIAN_POINT ( 'NONE',  ( 0.1058382717557500852, -0.3949938075777408852, -0.3195538057742782212 ) ) ;
#41729 = CARTESIAN_POINT ( 'NONE',  ( 1.404199475065617708, 0.05413385826771626580, -0.4176697321401330321 ) ) ;
#41730 = CARTESIAN_POINT ( 'NONE',  ( -0.05249343832020938322, -0.6046776061558809534, -0.2411417322834644161 ) ) ;
#41731 = CARTESIAN_POINT ( 'NONE',  ( 0.3871391076115493490, -0.2845877964562159024, 0.3641732283464567677 ) ) ;
#41732 = CARTESIAN_POINT ( 'NONE',  ( 0.4724409448818898127, -0.1265901696524988629, -0.1883202099737532331 ) ) ;
#41733 = CARTESIAN_POINT ( 'NONE',  ( -0.006561679790025524116, -0.08942795157528024563, -0.3641732283464568787 ) ) ;
#41734 = CARTESIAN_POINT ( 'NONE',  ( 1.220472440944882164, 0.000000000000000000, 0.3464511005275205946 ) ) ;
#41735 = CARTESIAN_POINT ( 'NONE',  ( -0.2925321140481932369, 0.2925321140481931259, -1.356299212598425452 ) ) ;
#41736 = CARTESIAN_POINT ( 'NONE',  ( 0.5577427821522316087, -0.05778040916215522460, 0.4822834645669289988 ) ) ;
#41737 = CARTESIAN_POINT ( 'NONE',  ( 0.2867679344610365999, -0.2867679344610365444, -1.035433070866141447 ) ) ;
#41738 = CARTESIAN_POINT ( 'NONE',  ( 1.509186351706037543, -0.004921259842519576551, 0.3153832671262227771 ) ) ;
#41739 = CARTESIAN_POINT ( 'NONE',  ( 0.09186351706036827158, 0.05413385826771666132, 0.4176697321401328100 ) ) ;
#41740 = CARTESIAN_POINT ( 'NONE',  ( -0.06561679790026180015, -0.3690944881889765550, -0.3153832671262227771 ) ) ;
#41741 = CARTESIAN_POINT ( 'NONE',  ( 0.2099737532808405305, -0.6046776061558807314, 0.2411417322834647770 ) ) ;
#41742 = CARTESIAN_POINT ( 'NONE',  ( 1.587926509186352586, -0.3690944881889765550, -0.3153832671262227771 ) ) ;
#41743 = CARTESIAN_POINT ( 'NONE',  ( -1.561679790026246017, -0.004921259842519576551, 0.3153832671262227771 ) ) ;
#41744 = CARTESIAN_POINT ( 'NONE',  ( -1.410761154855642463, -0.05778040916215522460, 0.4822834645669289988 ) ) ;
#41745 = CARTESIAN_POINT ( 'NONE',  ( 0.5839895013123367340, 0.2952755905511811885, 0.1292274648535926551 ) ) ;
#41746 = CARTESIAN_POINT ( 'NONE',  ( 1.325459317585302665, -0.4281496062992124485, 0.4176697321401328655 ) ) ;
#41747 = CARTESIAN_POINT ( 'NONE',  ( 6.372542394380578105E-15, 1.062992125984252523, -1.629220936382730134 ) ) ;
#41748 = CARTESIAN_POINT ( 'NONE',  ( -0.01968503937007793844, -0.5400638737290844871, 0.3530559997133364547 ) ) ;
#41749 = CARTESIAN_POINT ( 'NONE',  ( 1.213910761154856299, 0.2952755905511811885, 0.1292274648535926551 ) ) ;
#41750 = CARTESIAN_POINT ( 'NONE',  ( 0.9973753280839902091, -0.6046776061558807314, 0.2411417322834647770 ) ) ;
#41751 = CYLINDRICAL_SURFACE ( 'NONE', #1064, 0.4724409448818898682 ) ;
#41752 = CARTESIAN_POINT ( 'NONE',  ( 0.9842519685039378130, -0.5511811023622047445, 6.969142054262312111E-17 ) ) ;
#41753 = CARTESIAN_POINT ( 'NONE',  ( 1.601049868766404982, -0.6046776061558809534, -0.2411417322834644161 ) ) ;
#41754 = CARTESIAN_POINT ( 'NONE',  ( -0.6627296587926501115, 0.1771653543307087075, -0.09757992244046823083 ) ) ;
#41755 = CARTESIAN_POINT ( 'NONE',  ( 0.4593175853018379162, -0.3690944881889763329, 0.3153832671262228327 ) ) ;
#41756 = CARTESIAN_POINT ( 'NONE',  ( 0.07217847769028949700, -0.3162353388693405765, 0.4822834645669290543 ) ) ;
#41757 = CARTESIAN_POINT ( 'NONE',  ( 0.5905511811023629321, -0.6692913385826771977, 8.415575281601705876E-17 ) ) ;
#41758 = CARTESIAN_POINT ( 'NONE',  ( -0.5183727034120726440, 0.2952755905511811885, 0.1292274648535926551 ) ) ;
#41759 = EDGE_CURVE ( 'NONE', #41668, #51820, #36201, .T. ) ;
#41760 = CARTESIAN_POINT ( 'NONE',  ( 0.06561679790026316017, -0.004921259842519870586, -0.3153832671262229437 ) ) ;
#41761 = VECTOR ( 'NONE', #74024, 39.37007874015748143 ) ;
#41762 = CARTESIAN_POINT ( 'NONE',  ( 0.7939632545931766261, -0.05778040916215522460, 0.4822834645669289988 ) ) ;
#41763 = FACE_OUTER_BOUND ( 'NONE', #54617, .T. ) ;
#41764 = CARTESIAN_POINT ( 'NONE',  ( -0.9776902887139098386, -0.6692913385826771977, 0.1292274648535927661 ) ) ;
#41766 = CARTESIAN_POINT ( 'NONE',  ( 0.3460692066303959757, -0.1998031496062991907, -1.207349081364829324 ) ) ;
#41765 = LINE ( 'NONE', #16537, #40628 ) ;
#41767 = CARTESIAN_POINT ( 'NONE',  ( -0.2700868329615992991, 1.134086821910841758, 0.1585113167840819515 ) ) ;
#41768 = CARTESIAN_POINT ( 'NONE',  ( -0.6692913385826764205, 0.2952755905511811885, 0.000000000000000000 ) ) ;
#41769 = CARTESIAN_POINT ( 'NONE',  ( -0.6036745406824141069, 0.2306618581243848609, 0.2411417322834645549 ) ) ;
#41770 = CARTESIAN_POINT ( 'NONE',  ( -0.4724409448818898682, -8.678599364036362592E-17, -0.03937007874015747977 ) ) ;
#41771 = CARTESIAN_POINT ( 'NONE',  ( 0.1974969037888704704, 0.3420746716998660508, -2.506561679790026087 ) ) ;
#41772 = VERTEX_POINT ( 'NONE', #41273 ) ;
#41773 = CARTESIAN_POINT ( 'NONE',  ( 0.7874015748031503170, -0.1870078740157480601, -0.3641732283464567677 ) ) ;
#41774 = CARTESIAN_POINT ( 'NONE',  ( -0.1958661417322834220, -0.3392501089628018884, -1.002624671916010568 ) ) ;
#41775 = CARTESIAN_POINT ( 'NONE',  ( 1.174540682414699111, -0.05778040916215560624, -0.4822834645669293319 ) ) ;
#41776 = CARTESIAN_POINT ( 'NONE',  ( -0.1698998578625667832, -2.609869883881465018E-15, -0.3464511005275220379 ) ) ;
#41778 = AXIS2_PLACEMENT_3D ( 'NONE', #71592, #46740, #33300 ) ;
#41777 = CARTESIAN_POINT ( 'NONE',  ( -1.279527559055116948, -0.4536011799217367080, 0.2665933059059888421 ) ) ;
#41779 = CARTESIAN_POINT ( 'NONE',  ( 1.397637795275591177, 0.1660481256975883668, -0.3530559997133364547 ) ) ;
#41780 = CARTESIAN_POINT ( 'NONE',  ( -1.509186351706035767, 0.05413385826771626580, -0.4176697321401330321 ) ) ;
#41781 = CARTESIAN_POINT ( 'NONE',  ( 0.4855643044619430415, -0.4281496062992127816, -0.4176697321401328100 ) ) ;
#41782 = CARTESIAN_POINT ( 'NONE',  ( 4.797336870675655290E-17, -0.3917322834645669549, -0.3162536500974260090 ) ) ;
#41783 = CARTESIAN_POINT ( 'NONE',  ( 0.006561679790026889343, -0.3162353388693409650, -0.4822834645669289433 ) ) ;
#41784 = CARTESIAN_POINT ( 'NONE',  ( -0.9055118110236215490, 0.1771653543307087630, 0.000000000000000000 ) ) ;
#41785 = EDGE_CURVE ( 'NONE', #30946, #21487, #7679, .T. ) ;
#41786 = CARTESIAN_POINT ( 'NONE',  ( 1.023622047244095112, -0.1870078740157480879, -0.4822834645669291653 ) ) ;
#41787 = CARTESIAN_POINT ( 'NONE',  ( -0.1115485564304456306, 0.2952755905511810774, -0.1292274648535930714 ) ) ;
#41788 =( BOUNDED_SURFACE ( )  B_SPLINE_SURFACE ( 1, 2, ( 
 ( #36533, #54344, #18022, #48032, #11291, #36950, #56302, #57532, #82808, #310, #70168, #37770, #51211, #50392, #82405, #25964, #12521, #52047, #37368, #63857, #56706, #63039, #6194, #51622, #63445, #76089, #38599, #39010, #77327, #76907, #25544, #5377, #83223, #44477, #25132, #38182, #19656, #31872, #19237, #44888, #69358, #64694, #24724, #11712, #70587, #50802, #7033, #18433, #31038, #57943, #32283, #44075, #76503, #45318, #12941, #26389, #71013, #69768, #58369, #12112, #731, #32703, #64277, #5781, #31451, #77752, #57114, #43656, #18832, #6612, #13357, #33128, #45735, #65957, #33546, #7458, #15029, #34379, #71854, #66371, #34801, #1569, #8293, #27641, #53715, #60461, #8708, #15448, #41107, #59208, #39860, #33961, #59623, #13778, #2811, #28058, #66795, #46158, #78596, #40274, #14204, #9130, #28470, #72681, #21742, #65551, #47407, #1978, #21335, #58798, #7882, #53303, #46987, #1156, #54131, #26807, #65123, #79016, #40685, #46575, #71431, #20504, #52465, #27223, #60044, #52884, #2400, #20920, #39435, #79422, #73096, #20085, #78173, #72272, #14620, #36033, #43151, #68848, #36855, #9948, #67205, #4047, #60870, #62115, #35621, #54966, #22579, #11196, #42333, #62529, #9538, #36442, #55787, #81493, #4867, #68442, #75175, #48240, #80263, #61284, #30540, #4458, #47822, #17519, #67618, #30123, #3223, #29712, #55375, #23809, #35208, #79846, #49482, #81081, #74349, #22163, #3636, #28888, #73936, #54548, #73523, #23398, #15872, #49065, #42747, #41520, #16279, #29304, #41925, #74763, #80673, #22986, #17112, #48652, #16693, #68031, #10376, #61707, #10782, #11612, #43977, #63758, #69265, #6931, #70916, #57434, #51112, #76809, #82714, #82311, #38915, #18337, #49888, #64595, #44379, #83127, #69674, #45215, #24631, #50297, #70071, #56204, #13265, #37272, #38502, #18737, #19140, #25447, #62947, #75995, #12017, #44790, #37672, #70486, #6099, #12426, #56611, #38084, #81905, #63349, #32188, #5684, #24217, #77227, #17928, #31773, #211, #5282, #75589, #31353, #25034, #30944, #12843, #64184, #6518, #57844, #57019, #50707, #76406, #25864, #51524, #19556, #43564, #27119, #58265, #27953, #71329, #629, #14519, #71746, #53612, #13677, #26285, #46883, #21228, #51946, #39751, #72577, #59107, #15343, #34276, #33018, #47300, #77651, #72990, #79320, #72164, #39329, #78069, #14924, #40584, #21640, #19984, #20400, #7779, #45634, #65015, #78492, #46052, #7350, #27537, #66266, #1053, #78907, #41005, #14099, #20815, #40172, #8605, #66688, #59937, #32602, #58688, #65447, #52363, #46470, #65856, #26707, #33447, #2293, #1463, #52783, #8189, #33856, #59520, #1877, #53194, #61607, #10686, #3119, #36341, #22885, #10270, #47718, #28785, #48549, #35938, #73416, #81391, #15765, #54028, #16590, #42235, #35519, #60359, #9432, #22056, #54447, #74247, #35101, #74665, #80159, #2706, #67929, #3950, #60768, #55271, #29611, #67101, #80982, #48137, #48965, #61182, #22476, #23295, #41417, #73834, #17009, #3536, #17421, #28366, #29203, #16174, #79740, #54869, #42649, #41820, #67511, #68346, #4352, #62015, #30020, #55684, #9848, #23707, #80575, #49378, #75074, #43052, #9023, #34696, #37166, #31672, #111, #50198, #56923, #76310, #19044, #25766, #57333, #64082, #6419, #82213, #5182, #31255, #82617, #62424, #51427, #76711, #32088, #11510, #43875, #5588, #62846, #57749, #77130, #37987, #70388, #30846, #12743, #24933, #69975, #24118, #56511, #50603, #12329, #49787, #19463, #75488, #30437, #18641, #44285, #11921, #36748, #69159, #81806, #24532, #63663, #75895, #51012, #18235, #4761, #6003, #83027, #69573, #25350, #44691, #43462, #38402, #37576, #68748, #63249, #11091, #56102, #17828, #536, #1783, #14004, #53526, #38818, #65351, #58167, #64496, #7689, #27443, #64919, #51850, #40082, #40497, #53104, #78395, #27026, #6834, #1374, #45955, #963, #39661, #78813, #33356, #52687, #59019, #70820, #66177, #26189, #13168, #20727, #26617, #8515, #77557, #32504, #59428, #33766, #19890, #52270, #21142, #71652, #27866, #46797, #45538, #59846, #71236, #2198, #34182, #46378, #13580, #7257, #72488, #14837, #79234, #39234, #32929 ),
 ( #14430, #8101, #45113, #58594, #77975, #20305, #72071, #65769, #8927, #42142, #80885, #41726, #55584, #47627, #67010, #22791, #60269, #9343, #29104, #34604, #21549, #36247, #48451, #16498, #67837, #48044, #73322, #4258, #35014, #15251, #29921, #9753, #74151, #60678, #10590, #15668, #41330, #35425, #47210, #61916, #2619, #3855, #67420, #10176, #35841, #28275, #3027, #28693, #61509, #54355, #29515, #54775, #61090, #21966, #3441, #72900, #80066, #23198, #22384, #40911, #42552, #66592, #80478, #48869, #53937, #79649, #73745, #16081, #55176, #74569, #16914, #68255, #63154, #81712, #82116, #50916, #11828, #69060, #42956, #75383, #68650, #44594, #70289, #38302, #11410, #10988, #5494, #62324, #63566, #37065, #56417, #24022, #12641, #43772, #63977, #36649, #37890, #57229, #82930, #6313, #69880, #76616, #49690, #17731, #62750, #31990, #5900, #49279, #18946, #5086, #31573, #4662, #31156, #56822, #25252, #30335, #81296, #43359, #30754, #23610, #74982, #17327, #56001, #24431, #50099, #75795, #82520, #24837, #18138, #69475, #37481, #50505, #76209, #18546, #44190, #12233, #45013, #58065, #6732, #59328, #33256, #39985, #26926, #20626, #78714, #70712, #64813, #65675, #1277, #77031, #13064, #78294, #33666, #77872, #8412, #432, #19784, #58918, #38718, #45437, #65247, #64396, #57651, #72391, #52585, #46277, #71973, #857, #26087, #40394, #71132, #51327, #66076, #45852, #14327, #13475, #46698, #51747, #77450, #71551, #13, #14741, #32402, #8002, #20202, #1684, #27343, #39132, #7154, #32825, #53001, #58493, #21039, #7584, #13900, #26514, #39558, #25666, #52168, #19363, #34501, #74467, #55076, #79135, #9657, #61404, #66489, #42450, #53834, #2931, #8824, #73644, #15986, #80380, #41633, #60166, #34918, #3753, #47941, #21861, #21452, #28177, #47109, #80784, #23100, #16814, #47526, #72799, #67323, #15148, #16397, #73217, #9246, #2519, #48768, #79968, #68150, #40805, #74049, #10072, #35736, #34080, #22693, #29417, #79548, #35327, #15567, #42043, #41227, #60580, #66914, #59743, #22281, #2097, #28595, #67739, #27762, #53427, #54252, #48352, #60990, #3339, #29003, #54669, #25156, #50414, #61820, #31476, #81616, #44098, #17231, #18045, #43678, #69791, #81198, #5805, #76114, #11735, #4993, #63471, #23930, #23513, #10895, #42861, #12137, #69381, #18455, #63062, #56730, #57137, #49182, #17634, #37793, #37390, #29825, #74885, #31062, #82834, #30661, #44501, #36555, #55904, #5399, #68554, #49597, #82427, #62231, #10494, #50824, #24747, #76526, #18854, #36972, #4570, #36148, #75291, #4160, #55487, #82023, #30241, #43266, #68963, #11313, #62652, #24336, #56324, #50006, #75703, #53626, #33870, #34290, #14939, #76932, #12964, #32305, #59952, #38621, #40598, #21243, #27551, #70609, #53210, #70191, #25987, #47314, #64299, #28379, #9036, #31893, #46898, #15356, #19259, #79753, #6633, #39033, #44912, #78921, #72592, #2307, #66280, #57966, #71036, #41017, #1891, #333, #57554, #51646, #83245, #34710, #60371, #54040, #77350, #25568, #6217, #8620, #13380, #19682, #65870, #27968, #8205, #79334, #59534, #12545, #66703, #51233, #38204, #21654, #45340, #2719, #73004, #63878, #22070, #36353, #41430, #54882, #62029, #74260, #30450, #49392, #48152, #62437, #67113, #4774, #11105, #3961, #54460, #9861, #30033, #55696, #36761, #9444, #35531, #22894, #60781, #73428, #10283, #61193, #35115, #42661, #4365, #16187, #10698, #56114, #29215, #35949, #55284, #81404, #81820, #23721, #43064, #68761, #3549, #67524, #61619, #29624, #3133, #47730, #75086, #15778, #73847, #48562, #67941, #41834, #28797, #80174, #17022, #17433, #80587, #22488, #80994, #48977, #16601, #42246, #23307, #74676, #68359, #13183, #62858, #69171, #31686, #57345, #50617, #75501, #24546, #37179, #43889, #63674, #50210, #6433, #18247, #17840, #83041, #25364, #75908, #70402, #44706, #82226, #37998, #63260, #64097, #76322, #69586, #51027, #30859, #5194, #32104, #18652, #32519, #43475, #44296, #56524, #11522, #69987, #57763, #11932, #37587, #19058, #19477, #125, #76726, #6015, #5601, #31268, #56934, #70835, #38833, #64512, #82630, #24944, #12758, #12342 ) ),
 .UNSPECIFIED., .F., .F., .F. ) 
 B_SPLINE_SURFACE_WITH_KNOTS ( ( 2, 2 ),
 ( 3, 2, 2, 2, 2, 2, 2, 2, 2, 2, 2, 2, 2, 2, 2, 2, 2, 2, 2, 2, 2, 2, 2, 2, 2, 2, 2, 2, 2, 2, 2, 2, 2, 2, 2, 2, 2, 2, 2, 2, 2, 2, 2, 2, 2, 2, 2, 2, 2, 2, 2, 2, 2, 2, 2, 2, 2, 2, 2, 2, 2, 2, 2, 2, 2, 2, 2, 2, 2, 2, 2, 2, 2, 2, 2, 2, 2, 2, 2, 2, 2, 2, 2, 2, 2, 2, 2, 2, 2, 2, 2, 2, 2, 2, 2, 2, 2, 2, 2, 2, 2, 2, 2, 2, 2, 2, 2, 2, 2, 2, 2, 2, 2, 2, 2, 2, 2, 2, 2, 2, 2, 2, 2, 2, 2, 2, 2, 2, 2, 2, 2, 2, 2, 2, 2, 2, 2, 2, 2, 2, 2, 2, 2, 2, 2, 2, 2, 2, 2, 2, 2, 2, 2, 2, 2, 2, 2, 2, 2, 2, 2, 2, 2, 2, 2, 2, 2, 2, 2, 2, 2, 2, 2, 2, 2, 2, 2, 2, 2, 2, 2, 2, 2, 2, 2, 2, 2, 2, 2, 2, 2, 2, 2, 2, 2, 2, 2, 2, 2, 2, 2, 2, 2, 2, 2, 2, 2, 2, 2, 2, 2, 2, 2, 2, 2, 2, 2, 2, 2, 2, 2, 2, 2, 2, 2, 2, 2, 2, 2, 2, 2, 2, 2, 2, 2, 2, 2, 2, 2, 2, 2, 2, 2, 2, 2, 2, 2, 2, 2, 2, 2, 2, 2, 2, 2, 3 ),
 ( 0.000000000000000000, 1.000000000000000000 ),
 ( 0.000000000000000000, 0.003787878787878787984, 0.007575757575757575968, 0.01136363636363636395, 0.01515151515151515194, 0.01893939393939393992, 0.02272727272727272790, 0.02651515151515151589, 0.03030303030303030387, 0.03409090909090908839, 0.03787878787878787984, 0.04166666666666666435, 0.04545454545454545581, 0.04924242424242424032, 0.05303030303030303177, 0.05681818181818181629, 0.06060606060606060774, 0.06439393939393939226, 0.06818181818181817677, 0.07196969696969697516, 0.07575757575757575968, 0.07954545454545454419, 0.08333333333333332871, 0.08712121212121212710, 0.09090909090909091161, 0.09469696969696969613, 0.09848484848484848064, 0.1022727272727272790, 0.1060606060606060635, 0.1098484848484848481, 0.1136363636363636326, 0.1174242424242424310, 0.1212121212121212155, 0.1250000000000000000, 0.1287878787878787845, 0.1325757575757575690, 0.1363636363636363535, 0.1401515151515151381, 0.1439393939393939503, 0.1477272727272727348, 0.1515151515151515194, 0.1553030303030303039, 0.1590909090909090884, 0.1628787878787878729, 0.1666666666666666574, 0.1704545454545454419, 0.1742424242424242542, 0.1780303030303030387, 0.1818181818181818232, 0.1856060606060606077, 0.1893939393939393923, 0.1931818181818181768, 0.1969696969696969613, 0.2007575757575757458, 0.2045454545454545581, 0.2083333333333333426, 0.2121212121212121271, 0.2159090909090909116, 0.2196969696969696961, 0.2234848484848484806, 0.2272727272727272652, 0.2310606060606060497, 0.2348484848484848619, 0.2386363636363636465, 0.2424242424242424310, 0.2462121212121212155, 0.2500000000000000000, 0.2537878787878787845, 0.2575757575757575690, 0.2613636363636363535, 0.2651515151515151381, 0.2689393939393939226, 0.2727272727272727071, 0.2765151515151514916, 0.2803030303030302761, 0.2840909090909091161, 0.2878787878787879007, 0.2916666666666666852, 0.2954545454545454697, 0.2992424242424242542, 0.3030303030303030387, 0.3068181818181818232, 0.3106060606060606077, 0.3143939393939393923, 0.3181818181818181768, 0.3219696969696969613, 0.3257575757575757458, 0.3295454545454545303, 0.3333333333333333148, 0.3371212121212120993, 0.3409090909090908839, 0.3446969696969697239, 0.3484848484848485084, 0.3522727272727272929, 0.3560606060606060774, 0.3598484848484848619, 0.3636363636363636465, 0.3674242424242424310, 0.3712121212121212155, 0.3750000000000000000, 0.3787878787878787845, 0.3825757575757575690, 0.3863636363636363535, 0.3901515151515151381, 0.3939393939393939226, 0.3977272727272727071, 0.4015151515151514916, 0.4053030303030302761, 0.4090909090909091161, 0.4128787878787879007, 0.4166666666666666852, 0.4204545454545454697, 0.4242424242424242542, 0.4280303030303030387, 0.4318181818181818232, 0.4356060606060606077, 0.4393939393939393923, 0.4431818181818181768, 0.4469696969696969613, 0.4507575757575757458, 0.4545454545454545303, 0.4583333333333333148, 0.4621212121212120993, 0.4659090909090908839, 0.4696969696969697239, 0.4734848484848485084, 0.4772727272727272929, 0.4810606060606060774, 0.4848484848484848619, 0.4886363636363636465, 0.4924242424242424310, 0.4962121212121212155, 0.5000000000000000000, 0.5037878787878787845, 0.5075757575757575690, 0.5113636363636363535, 0.5151515151515151381, 0.5189393939393939226, 0.5227272727272727071, 0.5265151515151514916, 0.5303030303030302761, 0.5340909090909090606, 0.5378787878787878451, 0.5416666666666666297, 0.5454545454545454142, 0.5492424242424241987, 0.5530303030303029832, 0.5568181818181817677, 0.5606060606060605522, 0.5643939393939394478, 0.5681818181818182323, 0.5719696969696970168, 0.5757575757575758013, 0.5795454545454545858, 0.5833333333333333703, 0.5871212121212121549, 0.5909090909090909394, 0.5946969696969697239, 0.5984848484848485084, 0.6022727272727272929, 0.6060606060606060774, 0.6098484848484848619, 0.6136363636363636465, 0.6174242424242424310, 0.6212121212121212155, 0.6250000000000000000, 0.6287878787878787845, 0.6325757575757575690, 0.6363636363636363535, 0.6401515151515151381, 0.6439393939393939226, 0.6477272727272727071, 0.6515151515151514916, 0.6553030303030302761, 0.6590909090909090606, 0.6628787878787878451, 0.6666666666666666297, 0.6704545454545454142, 0.6742424242424241987, 0.6780303030303029832, 0.6818181818181817677, 0.6856060606060605522, 0.6893939393939394478, 0.6931818181818182323, 0.6969696969696970168, 0.7007575757575758013, 0.7045454545454545858, 0.7083333333333333703, 0.7121212121212121549, 0.7159090909090909394, 0.7196969696969697239, 0.7234848484848485084, 0.7272727272727272929, 0.7310606060606060774, 0.7348484848484848619, 0.7386363636363636465, 0.7424242424242424310, 0.7462121212121212155, 0.7500000000000000000, 0.7537878787878787845, 0.7575757575757575690, 0.7613636363636363535, 0.7651515151515151381, 0.7689393939393939226, 0.7727272727272727071, 0.7765151515151514916, 0.7803030303030302761, 0.7840909090909090606, 0.7878787878787878451, 0.7916666666666666297, 0.7954545454545454142, 0.7992424242424241987, 0.8030303030303029832, 0.8068181818181817677, 0.8106060606060605522, 0.8143939393939394478, 0.8181818181818182323, 0.8219696969696970168, 0.8257575757575758013, 0.8295454545454545858, 0.8333333333333333703, 0.8371212121212121549, 0.8409090909090909394, 0.8446969696969697239, 0.8484848484848485084, 0.8522727272727272929, 0.8560606060606060774, 0.8598484848484848619, 0.8636363636363636465, 0.8674242424242424310, 0.8712121212121212155, 0.8750000000000000000, 0.8787878787878787845, 0.8825757575757575690, 0.8863636363636363535, 0.8901515151515151381, 0.8939393939393939226, 0.8977272727272727071, 0.9015151515151514916, 0.9053030303030302761, 0.9090909090909090606, 0.9128787878787878451, 0.9166666666666666297, 0.9204545454545454142, 0.9242424242424241987, 0.9280303030303029832, 0.9318181818181817677, 0.9356060606060605522, 0.9393939393939394478, 0.9431818181818182323, 0.9469696969696970168, 0.9507575757575758013, 0.9545454545454545858, 0.9583333333333333703, 0.9621212121212121549, 0.9659090909090909394 ),
 .UNSPECIFIED. ) 
 GEOMETRIC_REPRESENTATION_ITEM ( )  RATIONAL_B_SPLINE_SURFACE ( (
 ( 1.000000000000000000, 0.9659258262890683122, 1.000000000000000000, 0.9659258262890683122, 1.000000000000000000, 0.9659258262890683122, 1.000000000000000000, 0.9659258262890683122, 1.000000000000000000, 0.9659258262890683122, 1.000000000000000000, 0.9659258262890683122, 1.000000000000000000, 0.9659258262890683122, 1.000000000000000000, 0.9659258262890683122, 1.000000000000000000, 0.9659258262890683122, 1.000000000000000000, 0.9659258262890683122, 1.000000000000000000, 0.9659258262890683122, 1.000000000000000000, 0.9659258262890683122, 1.000000000000000000, 0.9659258262890683122, 1.000000000000000000, 0.9659258262890683122, 1.000000000000000000, 0.9659258262890683122, 1.000000000000000000, 0.9659258262890683122, 1.000000000000000000, 0.9659258262890683122, 1.000000000000000000, 0.9659258262890683122, 1.000000000000000000, 0.9659258262890683122, 1.000000000000000000, 0.9659258262890683122, 1.000000000000000000, 0.9659258262890683122, 1.000000000000000000, 0.9659258262890683122, 1.000000000000000000, 0.9659258262890683122, 1.000000000000000000, 0.9659258262890683122, 1.000000000000000000, 0.9659258262890683122, 1.000000000000000000, 0.9659258262890683122, 1.000000000000000000, 0.9659258262890683122, 1.000000000000000000, 0.9659258262890683122, 1.000000000000000000, 0.9659258262890683122, 1.000000000000000000, 0.9659258262890683122, 1.000000000000000000, 0.9659258262890683122, 1.000000000000000000, 0.9659258262890683122, 1.000000000000000000, 0.9659258262890683122, 1.000000000000000000, 0.9659258262890683122, 1.000000000000000000, 0.9659258262890683122, 1.000000000000000000, 0.9659258262890683122, 1.000000000000000000, 0.9659258262890683122, 1.000000000000000000, 0.9659258262890683122, 1.000000000000000000, 0.9659258262890683122, 1.000000000000000000, 0.9659258262890683122, 1.000000000000000000, 0.9659258262890683122, 1.000000000000000000, 0.9659258262890683122, 1.000000000000000000, 0.9659258262890683122, 1.000000000000000000, 0.9659258262890683122, 1.000000000000000000, 0.9659258262890683122, 1.000000000000000000, 0.9659258262890683122, 1.000000000000000000, 0.9659258262890683122, 1.000000000000000000, 0.9659258262890683122, 1.000000000000000000, 0.9659258262890683122, 1.000000000000000000, 0.9659258262890683122, 1.000000000000000000, 0.9659258262890683122, 1.000000000000000000, 0.9659258262890683122, 1.000000000000000000, 0.9659258262890683122, 1.000000000000000000, 0.9659258262890683122, 1.000000000000000000, 0.9659258262890683122, 1.000000000000000000, 0.9659258262890683122, 1.000000000000000000, 0.9659258262890683122, 1.000000000000000000, 0.9659258262890683122, 1.000000000000000000, 0.9659258262890683122, 1.000000000000000000, 0.9659258262890683122, 1.000000000000000000, 0.9659258262890683122, 1.000000000000000000, 0.9659258262890683122, 1.000000000000000000, 0.9659258262890683122, 1.000000000000000000, 0.9659258262890683122, 1.000000000000000000, 0.9659258262890683122, 1.000000000000000000, 0.9659258262890683122, 1.000000000000000000, 0.9659258262890683122, 1.000000000000000000, 0.9659258262890683122, 1.000000000000000000, 0.9659258262890683122, 1.000000000000000000, 0.9659258262890683122, 1.000000000000000000, 0.9659258262890683122, 1.000000000000000000, 0.9659258262890683122, 1.000000000000000000, 0.9659258262890683122, 1.000000000000000000, 0.9659258262890683122, 1.000000000000000000, 0.9659258262890683122, 1.000000000000000000, 0.9659258262890683122, 1.000000000000000000, 0.9659258262890683122, 1.000000000000000000, 0.9659258262890683122, 1.000000000000000000, 0.9659258262890683122, 1.000000000000000000, 0.9659258262890683122, 1.000000000000000000, 0.9659258262890683122, 1.000000000000000000, 0.9659258262890683122, 1.000000000000000000, 0.9659258262890683122, 1.000000000000000000, 0.9659258262890683122, 1.000000000000000000, 0.9659258262890683122, 1.000000000000000000, 0.9659258262890683122, 1.000000000000000000, 0.9659258262890683122, 1.000000000000000000, 0.9659258262890683122, 1.000000000000000000, 0.9659258262890683122, 1.000000000000000000, 0.9659258262890683122, 1.000000000000000000, 0.9659258262890683122, 1.000000000000000000, 0.9659258262890683122, 1.000000000000000000, 0.9659258262890683122, 1.000000000000000000, 0.9659258262890683122, 1.000000000000000000, 0.9659258262890683122, 1.000000000000000000, 0.9659258262890683122, 1.000000000000000000, 0.9659258262890683122, 1.000000000000000000, 0.9659258262890683122, 1.000000000000000000, 0.9659258262890683122, 1.000000000000000000, 0.9659258262890683122, 1.000000000000000000, 0.9659258262890683122, 1.000000000000000000, 0.9659258262890683122, 1.000000000000000000, 0.9659258262890683122, 1.000000000000000000, 0.9659258262890683122, 1.000000000000000000, 0.9659258262890683122, 1.000000000000000000, 0.9659258262890683122, 1.000000000000000000, 0.9659258262890683122, 1.000000000000000000, 0.9659258262890683122, 1.000000000000000000, 0.9659258262890683122, 1.000000000000000000, 0.9659258262890683122, 1.000000000000000000, 0.9659258262890683122, 1.000000000000000000, 0.9659258262890683122, 1.000000000000000000, 0.9659258262890683122, 1.000000000000000000, 0.9659258262890683122, 1.000000000000000000, 0.9659258262890683122, 1.000000000000000000, 0.9659258262890683122, 1.000000000000000000, 0.9659258262890683122, 1.000000000000000000, 0.9659258262890683122, 1.000000000000000000, 0.9659258262890683122, 1.000000000000000000, 0.9659258262890683122, 1.000000000000000000, 0.9659258262890683122, 1.000000000000000000, 0.9659258262890683122, 1.000000000000000000, 0.9659258262890683122, 1.000000000000000000, 0.9659258262890683122, 1.000000000000000000, 0.9659258262890683122, 1.000000000000000000, 0.9659258262890683122, 1.000000000000000000, 0.9659258262890683122, 1.000000000000000000, 0.9659258262890683122, 1.000000000000000000, 0.9659258262890683122, 1.000000000000000000, 0.9659258262890683122, 1.000000000000000000, 0.9659258262890683122, 1.000000000000000000, 0.9659258262890683122, 1.000000000000000000, 0.9659258262890683122, 1.000000000000000000, 0.9659258262890683122, 1.000000000000000000, 0.9659258262890683122, 1.000000000000000000, 0.9659258262890683122, 1.000000000000000000, 0.9659258262890683122, 1.000000000000000000, 0.9659258262890683122, 1.000000000000000000, 0.9659258262890683122, 1.000000000000000000, 0.9659258262890683122, 1.000000000000000000, 0.9659258262890683122, 1.000000000000000000, 0.9659258262890683122, 1.000000000000000000, 0.9659258262890683122, 1.000000000000000000, 0.9659258262890683122, 1.000000000000000000, 0.9659258262890683122, 1.000000000000000000, 0.9659258262890683122, 1.000000000000000000, 0.9659258262890683122, 1.000000000000000000, 0.9659258262890683122, 1.000000000000000000, 0.9659258262890683122, 1.000000000000000000, 0.9659258262890683122, 1.000000000000000000, 0.9659258262890683122, 1.000000000000000000, 0.9659258262890683122, 1.000000000000000000, 0.9659258262890683122, 1.000000000000000000, 0.9659258262890683122, 1.000000000000000000, 0.9659258262890683122, 1.000000000000000000, 0.9659258262890683122, 1.000000000000000000, 0.9659258262890683122, 1.000000000000000000, 0.9659258262890683122, 1.000000000000000000, 0.9659258262890683122, 1.000000000000000000, 0.9659258262890683122, 1.000000000000000000, 0.9659258262890683122, 1.000000000000000000, 0.9659258262890683122, 1.000000000000000000, 0.9659258262890683122, 1.000000000000000000, 0.9659258262890683122, 1.000000000000000000, 0.9659258262890683122, 1.000000000000000000, 0.9659258262890683122, 1.000000000000000000, 0.9659258262890683122, 1.000000000000000000, 0.9659258262890683122, 1.000000000000000000, 0.9659258262890683122, 1.000000000000000000, 0.9659258262890683122, 1.000000000000000000, 0.9659258262890683122, 1.000000000000000000, 0.9659258262890683122, 1.000000000000000000, 0.9659258262890683122, 1.000000000000000000, 0.9659258262890683122, 1.000000000000000000, 0.9659258262890683122, 1.000000000000000000, 0.9659258262890683122, 1.000000000000000000, 0.9659258262890683122, 1.000000000000000000, 0.9659258262890683122, 1.000000000000000000, 0.9659258262890683122, 1.000000000000000000, 0.9659258262890683122, 1.000000000000000000, 0.9659258262890683122, 1.000000000000000000, 0.9659258262890683122, 1.000000000000000000, 0.9659258262890683122, 1.000000000000000000, 0.9659258262890683122, 1.000000000000000000, 0.9659258262890683122, 1.000000000000000000, 0.9659258262890683122, 1.000000000000000000, 0.9659258262890683122, 1.000000000000000000, 0.9659258262890683122, 1.000000000000000000, 0.9659258262890683122, 1.000000000000000000, 0.9659258262890683122, 1.000000000000000000, 0.9659258262890683122, 1.000000000000000000, 0.9659258262890683122, 1.000000000000000000, 0.9659258262890683122, 1.000000000000000000, 0.9659258262890683122, 1.000000000000000000, 0.9659258262890683122, 1.000000000000000000, 0.9659258262890683122, 1.000000000000000000, 0.9659258262890683122, 1.000000000000000000, 0.9659258262890683122, 1.000000000000000000, 0.9659258262890683122, 1.000000000000000000, 0.9659258262890683122, 1.000000000000000000, 0.9659258262890683122, 1.000000000000000000, 0.9659258262890683122, 1.000000000000000000, 0.9659258262890683122, 1.000000000000000000, 0.9659258262890683122, 1.000000000000000000, 0.9659258262890683122, 1.000000000000000000, 0.9659258262890683122, 1.000000000000000000, 0.9659258262890683122, 1.000000000000000000, 0.9659258262890683122, 1.000000000000000000, 0.9659258262890683122, 1.000000000000000000, 0.9659258262890683122, 1.000000000000000000, 0.9659258262890683122, 1.000000000000000000, 0.9659258262890683122, 1.000000000000000000, 0.9659258262890683122, 1.000000000000000000, 0.9659258262890683122, 1.000000000000000000, 0.9659258262890683122, 1.000000000000000000, 0.9659258262890683122, 1.000000000000000000, 0.9659258262890683122, 1.000000000000000000, 0.9659258262890683122, 1.000000000000000000, 0.9659258262890683122, 1.000000000000000000, 0.9659258262890683122, 1.000000000000000000, 0.9659258262890683122, 1.000000000000000000, 0.9659258262890683122, 1.000000000000000000, 0.9659258262890683122, 1.000000000000000000, 0.9659258262890683122, 1.000000000000000000, 0.9659258262890683122, 1.000000000000000000, 0.9659258262890683122, 1.000000000000000000, 0.9659258262890683122, 1.000000000000000000, 0.9659258262890683122, 1.000000000000000000, 0.9659258262890683122, 1.000000000000000000, 0.9659258262890683122, 1.000000000000000000, 0.9659258262890683122, 1.000000000000000000, 0.9659258262890683122, 1.000000000000000000, 0.9659258262890683122, 1.000000000000000000, 0.9659258262890683122, 1.000000000000000000, 0.9659258262890683122, 1.000000000000000000, 0.9659258262890683122, 1.000000000000000000, 0.9659258262890683122, 1.000000000000000000, 0.9659258262890683122, 1.000000000000000000, 0.9659258262890683122, 1.000000000000000000, 0.9659258262890683122, 1.000000000000000000, 0.9659258262890683122, 1.000000000000000000, 0.9659258262890683122, 1.000000000000000000, 0.9659258262890683122, 1.000000000000000000, 0.9659258262890683122, 1.000000000000000000, 0.9659258262890683122, 1.000000000000000000, 0.9659258262890683122, 1.000000000000000000, 0.9659258262890683122, 1.000000000000000000, 0.9659258262890683122, 1.000000000000000000, 0.9659258262890683122, 1.000000000000000000, 0.9659258262890683122, 1.000000000000000000, 0.9659258262890683122, 1.000000000000000000, 0.9659258262890683122, 1.000000000000000000, 0.9659258262890683122, 1.000000000000000000, 0.9659258262890683122, 1.000000000000000000, 0.9659258262890683122, 1.000000000000000000),
 ( 1.000000000000000000, 0.9659258262890683122, 1.000000000000000000, 0.9659258262890683122, 1.000000000000000000, 0.9659258262890683122, 1.000000000000000000, 0.9659258262890683122, 1.000000000000000000, 0.9659258262890683122, 1.000000000000000000, 0.9659258262890683122, 1.000000000000000000, 0.9659258262890683122, 1.000000000000000000, 0.9659258262890683122, 1.000000000000000000, 0.9659258262890683122, 1.000000000000000000, 0.9659258262890683122, 1.000000000000000000, 0.9659258262890683122, 1.000000000000000000, 0.9659258262890683122, 1.000000000000000000, 0.9659258262890683122, 1.000000000000000000, 0.9659258262890683122, 1.000000000000000000, 0.9659258262890683122, 1.000000000000000000, 0.9659258262890683122, 1.000000000000000000, 0.9659258262890683122, 1.000000000000000000, 0.9659258262890683122, 1.000000000000000000, 0.9659258262890683122, 1.000000000000000000, 0.9659258262890683122, 1.000000000000000000, 0.9659258262890683122, 1.000000000000000000, 0.9659258262890683122, 1.000000000000000000, 0.9659258262890683122, 1.000000000000000000, 0.9659258262890683122, 1.000000000000000000, 0.9659258262890683122, 1.000000000000000000, 0.9659258262890683122, 1.000000000000000000, 0.9659258262890683122, 1.000000000000000000, 0.9659258262890683122, 1.000000000000000000, 0.9659258262890683122, 1.000000000000000000, 0.9659258262890683122, 1.000000000000000000, 0.9659258262890683122, 1.000000000000000000, 0.9659258262890683122, 1.000000000000000000, 0.9659258262890683122, 1.000000000000000000, 0.9659258262890683122, 1.000000000000000000, 0.9659258262890683122, 1.000000000000000000, 0.9659258262890683122, 1.000000000000000000, 0.9659258262890683122, 1.000000000000000000, 0.9659258262890683122, 1.000000000000000000, 0.9659258262890683122, 1.000000000000000000, 0.9659258262890683122, 1.000000000000000000, 0.9659258262890683122, 1.000000000000000000, 0.9659258262890683122, 1.000000000000000000, 0.9659258262890683122, 1.000000000000000000, 0.9659258262890683122, 1.000000000000000000, 0.9659258262890683122, 1.000000000000000000, 0.9659258262890683122, 1.000000000000000000, 0.9659258262890683122, 1.000000000000000000, 0.9659258262890683122, 1.000000000000000000, 0.9659258262890683122, 1.000000000000000000, 0.9659258262890683122, 1.000000000000000000, 0.9659258262890683122, 1.000000000000000000, 0.9659258262890683122, 1.000000000000000000, 0.9659258262890683122, 1.000000000000000000, 0.9659258262890683122, 1.000000000000000000, 0.9659258262890683122, 1.000000000000000000, 0.9659258262890683122, 1.000000000000000000, 0.9659258262890683122, 1.000000000000000000, 0.9659258262890683122, 1.000000000000000000, 0.9659258262890683122, 1.000000000000000000, 0.9659258262890683122, 1.000000000000000000, 0.9659258262890683122, 1.000000000000000000, 0.9659258262890683122, 1.000000000000000000, 0.9659258262890683122, 1.000000000000000000, 0.9659258262890683122, 1.000000000000000000, 0.9659258262890683122, 1.000000000000000000, 0.9659258262890683122, 1.000000000000000000, 0.9659258262890683122, 1.000000000000000000, 0.9659258262890683122, 1.000000000000000000, 0.9659258262890683122, 1.000000000000000000, 0.9659258262890683122, 1.000000000000000000, 0.9659258262890683122, 1.000000000000000000, 0.9659258262890683122, 1.000000000000000000, 0.9659258262890683122, 1.000000000000000000, 0.9659258262890683122, 1.000000000000000000, 0.9659258262890683122, 1.000000000000000000, 0.9659258262890683122, 1.000000000000000000, 0.9659258262890683122, 1.000000000000000000, 0.9659258262890683122, 1.000000000000000000, 0.9659258262890683122, 1.000000000000000000, 0.9659258262890683122, 1.000000000000000000, 0.9659258262890683122, 1.000000000000000000, 0.9659258262890683122, 1.000000000000000000, 0.9659258262890683122, 1.000000000000000000, 0.9659258262890683122, 1.000000000000000000, 0.9659258262890683122, 1.000000000000000000, 0.9659258262890683122, 1.000000000000000000, 0.9659258262890683122, 1.000000000000000000, 0.9659258262890683122, 1.000000000000000000, 0.9659258262890683122, 1.000000000000000000, 0.9659258262890683122, 1.000000000000000000, 0.9659258262890683122, 1.000000000000000000, 0.9659258262890683122, 1.000000000000000000, 0.9659258262890683122, 1.000000000000000000, 0.9659258262890683122, 1.000000000000000000, 0.9659258262890683122, 1.000000000000000000, 0.9659258262890683122, 1.000000000000000000, 0.9659258262890683122, 1.000000000000000000, 0.9659258262890683122, 1.000000000000000000, 0.9659258262890683122, 1.000000000000000000, 0.9659258262890683122, 1.000000000000000000, 0.9659258262890683122, 1.000000000000000000, 0.9659258262890683122, 1.000000000000000000, 0.9659258262890683122, 1.000000000000000000, 0.9659258262890683122, 1.000000000000000000, 0.9659258262890683122, 1.000000000000000000, 0.9659258262890683122, 1.000000000000000000, 0.9659258262890683122, 1.000000000000000000, 0.9659258262890683122, 1.000000000000000000, 0.9659258262890683122, 1.000000000000000000, 0.9659258262890683122, 1.000000000000000000, 0.9659258262890683122, 1.000000000000000000, 0.9659258262890683122, 1.000000000000000000, 0.9659258262890683122, 1.000000000000000000, 0.9659258262890683122, 1.000000000000000000, 0.9659258262890683122, 1.000000000000000000, 0.9659258262890683122, 1.000000000000000000, 0.9659258262890683122, 1.000000000000000000, 0.9659258262890683122, 1.000000000000000000, 0.9659258262890683122, 1.000000000000000000, 0.9659258262890683122, 1.000000000000000000, 0.9659258262890683122, 1.000000000000000000, 0.9659258262890683122, 1.000000000000000000, 0.9659258262890683122, 1.000000000000000000, 0.9659258262890683122, 1.000000000000000000, 0.9659258262890683122, 1.000000000000000000, 0.9659258262890683122, 1.000000000000000000, 0.9659258262890683122, 1.000000000000000000, 0.9659258262890683122, 1.000000000000000000, 0.9659258262890683122, 1.000000000000000000, 0.9659258262890683122, 1.000000000000000000, 0.9659258262890683122, 1.000000000000000000, 0.9659258262890683122, 1.000000000000000000, 0.9659258262890683122, 1.000000000000000000, 0.9659258262890683122, 1.000000000000000000, 0.9659258262890683122, 1.000000000000000000, 0.9659258262890683122, 1.000000000000000000, 0.9659258262890683122, 1.000000000000000000, 0.9659258262890683122, 1.000000000000000000, 0.9659258262890683122, 1.000000000000000000, 0.9659258262890683122, 1.000000000000000000, 0.9659258262890683122, 1.000000000000000000, 0.9659258262890683122, 1.000000000000000000, 0.9659258262890683122, 1.000000000000000000, 0.9659258262890683122, 1.000000000000000000, 0.9659258262890683122, 1.000000000000000000, 0.9659258262890683122, 1.000000000000000000, 0.9659258262890683122, 1.000000000000000000, 0.9659258262890683122, 1.000000000000000000, 0.9659258262890683122, 1.000000000000000000, 0.9659258262890683122, 1.000000000000000000, 0.9659258262890683122, 1.000000000000000000, 0.9659258262890683122, 1.000000000000000000, 0.9659258262890683122, 1.000000000000000000, 0.9659258262890683122, 1.000000000000000000, 0.9659258262890683122, 1.000000000000000000, 0.9659258262890683122, 1.000000000000000000, 0.9659258262890683122, 1.000000000000000000, 0.9659258262890683122, 1.000000000000000000, 0.9659258262890683122, 1.000000000000000000, 0.9659258262890683122, 1.000000000000000000, 0.9659258262890683122, 1.000000000000000000, 0.9659258262890683122, 1.000000000000000000, 0.9659258262890683122, 1.000000000000000000, 0.9659258262890683122, 1.000000000000000000, 0.9659258262890683122, 1.000000000000000000, 0.9659258262890683122, 1.000000000000000000, 0.9659258262890683122, 1.000000000000000000, 0.9659258262890683122, 1.000000000000000000, 0.9659258262890683122, 1.000000000000000000, 0.9659258262890683122, 1.000000000000000000, 0.9659258262890683122, 1.000000000000000000, 0.9659258262890683122, 1.000000000000000000, 0.9659258262890683122, 1.000000000000000000, 0.9659258262890683122, 1.000000000000000000, 0.9659258262890683122, 1.000000000000000000, 0.9659258262890683122, 1.000000000000000000, 0.9659258262890683122, 1.000000000000000000, 0.9659258262890683122, 1.000000000000000000, 0.9659258262890683122, 1.000000000000000000, 0.9659258262890683122, 1.000000000000000000, 0.9659258262890683122, 1.000000000000000000, 0.9659258262890683122, 1.000000000000000000, 0.9659258262890683122, 1.000000000000000000, 0.9659258262890683122, 1.000000000000000000, 0.9659258262890683122, 1.000000000000000000, 0.9659258262890683122, 1.000000000000000000, 0.9659258262890683122, 1.000000000000000000, 0.9659258262890683122, 1.000000000000000000, 0.9659258262890683122, 1.000000000000000000, 0.9659258262890683122, 1.000000000000000000, 0.9659258262890683122, 1.000000000000000000, 0.9659258262890683122, 1.000000000000000000, 0.9659258262890683122, 1.000000000000000000, 0.9659258262890683122, 1.000000000000000000, 0.9659258262890683122, 1.000000000000000000, 0.9659258262890683122, 1.000000000000000000, 0.9659258262890683122, 1.000000000000000000, 0.9659258262890683122, 1.000000000000000000, 0.9659258262890683122, 1.000000000000000000, 0.9659258262890683122, 1.000000000000000000, 0.9659258262890683122, 1.000000000000000000, 0.9659258262890683122, 1.000000000000000000, 0.9659258262890683122, 1.000000000000000000, 0.9659258262890683122, 1.000000000000000000, 0.9659258262890683122, 1.000000000000000000, 0.9659258262890683122, 1.000000000000000000, 0.9659258262890683122, 1.000000000000000000, 0.9659258262890683122, 1.000000000000000000, 0.9659258262890683122, 1.000000000000000000, 0.9659258262890683122, 1.000000000000000000, 0.9659258262890683122, 1.000000000000000000, 0.9659258262890683122, 1.000000000000000000, 0.9659258262890683122, 1.000000000000000000, 0.9659258262890683122, 1.000000000000000000, 0.9659258262890683122, 1.000000000000000000, 0.9659258262890683122, 1.000000000000000000, 0.9659258262890683122, 1.000000000000000000, 0.9659258262890683122, 1.000000000000000000, 0.9659258262890683122, 1.000000000000000000, 0.9659258262890683122, 1.000000000000000000, 0.9659258262890683122, 1.000000000000000000, 0.9659258262890683122, 1.000000000000000000, 0.9659258262890683122, 1.000000000000000000, 0.9659258262890683122, 1.000000000000000000, 0.9659258262890683122, 1.000000000000000000, 0.9659258262890683122, 1.000000000000000000, 0.9659258262890683122, 1.000000000000000000, 0.9659258262890683122, 1.000000000000000000, 0.9659258262890683122, 1.000000000000000000, 0.9659258262890683122, 1.000000000000000000, 0.9659258262890683122, 1.000000000000000000, 0.9659258262890683122, 1.000000000000000000, 0.9659258262890683122, 1.000000000000000000, 0.9659258262890683122, 1.000000000000000000, 0.9659258262890683122, 1.000000000000000000, 0.9659258262890683122, 1.000000000000000000, 0.9659258262890683122, 1.000000000000000000, 0.9659258262890683122, 1.000000000000000000, 0.9659258262890683122, 1.000000000000000000, 0.9659258262890683122, 1.000000000000000000, 0.9659258262890683122, 1.000000000000000000, 0.9659258262890683122, 1.000000000000000000, 0.9659258262890683122, 1.000000000000000000, 0.9659258262890683122, 1.000000000000000000, 0.9659258262890683122, 1.000000000000000000, 0.9659258262890683122, 1.000000000000000000, 0.9659258262890683122, 1.000000000000000000, 0.9659258262890683122, 1.000000000000000000, 0.9659258262890683122, 1.000000000000000000, 0.9659258262890683122, 1.000000000000000000, 0.9659258262890683122, 1.000000000000000000, 0.9659258262890683122, 1.000000000000000000, 0.9659258262890683122, 1.000000000000000000, 0.9659258262890683122, 1.000000000000000000, 0.9659258262890683122, 1.000000000000000000) ) ) 
 REPRESENTATION_ITEM ( '' )  SURFACE ( )  );
